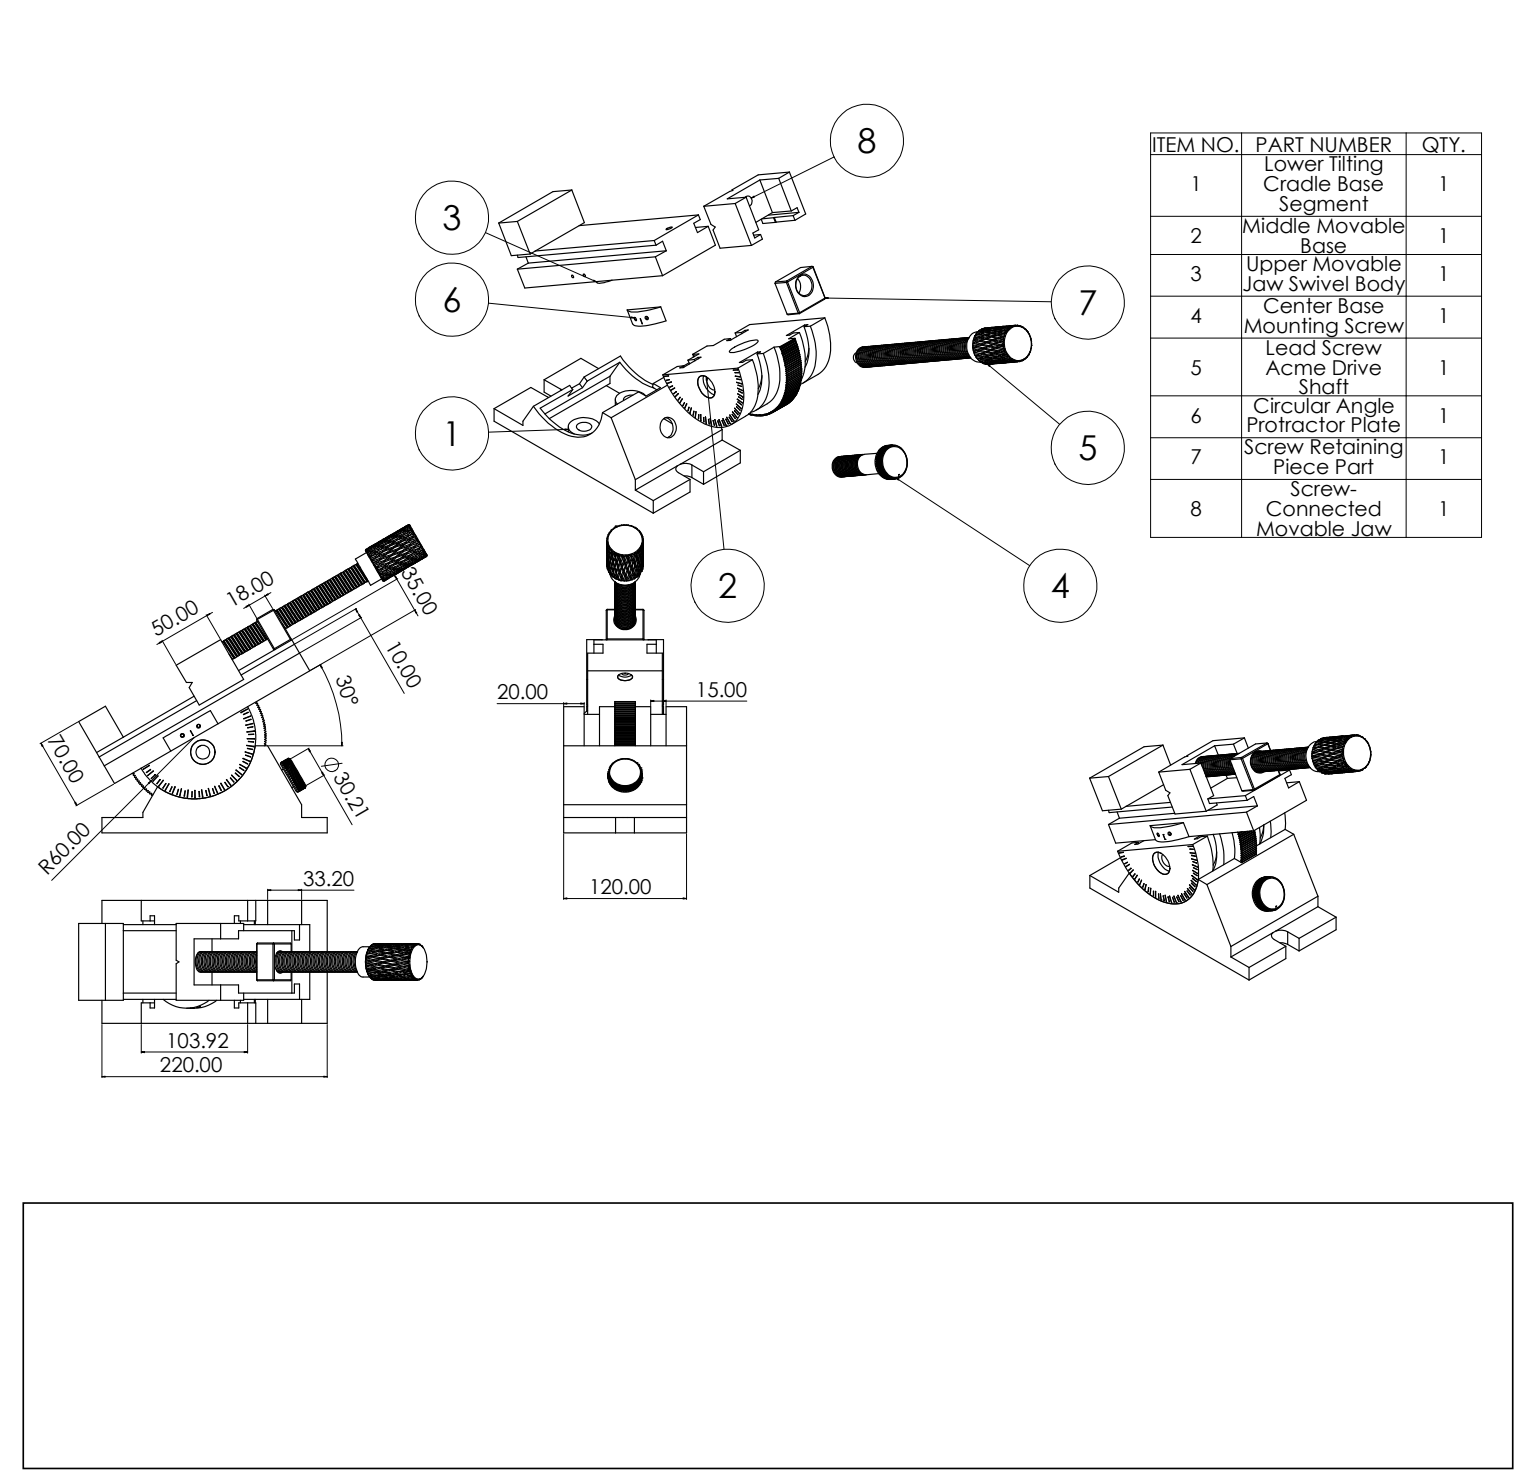
ISO-10303-21;
HEADER;
FILE_DESCRIPTION (('STEP AP214'),
    '1' );
FILE_NAME ('MAS-322',
    '2026-10-24T22:31:37',
    ( '' ),
    ( '' ),
    'SwSTEP 2.0',
    'SolidWorks 2025',
    '' );
FILE_SCHEMA (( 'AUTOMOTIVE_DESIGN' ));
ENDSEC;

DATA;
#1 = CARTESIAN_POINT ( 'NONE',  ( 23.65144817020273749, 15.78380873178787347, -6.180339887498949025 ) ) ;
#2 = EDGE_CURVE ( 'NONE', #71353, #27127, #17244, .T. ) ;
#3 = DIRECTION ( 'NONE',  ( 0.6270036013472524150, 0.3336146661356817478, 0.7039657224870777830 ) ) ;
#4 =( GEOMETRIC_REPRESENTATION_CONTEXT ( 3 ) GLOBAL_UNCERTAINTY_ASSIGNED_CONTEXT ( ( #48363 ) ) GLOBAL_UNIT_ASSIGNED_CONTEXT ( ( #53726, #45627, #22843 ) ) REPRESENTATION_CONTEXT ( 'NONE', 'WORKASPACE' ) );
#5 = CARTESIAN_POINT ( 'NONE',  ( 165.5065167046122099, 285.3186853228385758, 0.5240180121679646197 ) ) ;
#6 = CARTESIAN_POINT ( 'NONE',  ( 181.3318829485781976, 258.8378521386378566, -10.46588027007283017 ) ) ;
#7 = DIRECTION ( 'NONE',  ( -0.5866775868892348811, -0.8098206029990989707, 0.000000000000000000 ) ) ;
#8 = ORIENTED_EDGE ( 'NONE', *, *, #76052, .F. ) ;
#9 = CARTESIAN_POINT ( 'NONE',  ( 192.4853974341616549, 296.6629111496555424, 11.26379224701618398 ) ) ;
#10 = CARTESIAN_POINT ( 'NONE',  ( 33.33147356615550194, 41.01751292744059896, 6.180339887498949913 ) ) ;
#11 = CARTESIAN_POINT ( 'NONE',  ( 35.05240415091495976, 28.43677371833803846, -10.00000000000000355 ) ) ;
#12 = CARTESIAN_POINT ( 'NONE',  ( 201.3053499423511425, 281.9759013948520874, -16.75960365258566398 ) ) ;
#13 = CARTESIAN_POINT ( 'NONE',  ( 72.98662891910291250, 70.81012252529507123, 7.400885746516181030 ) ) ;
#14 = CARTESIAN_POINT ( 'NONE',  ( 67.19710446998851694, 67.37600790391256567, -7.293204404656055573 ) ) ;
#15 = CARTESIAN_POINT ( 'NONE',  ( 199.8044370756099966, 266.7412756917946695, 4.662294411209313871 ) ) ;
#16 = CARTESIAN_POINT ( 'NONE',  ( 202.7688273210276293, 274.1343011241658587, 13.26872680179261366 ) ) ;
#17 = CARTESIAN_POINT ( 'NONE',  ( 41.47569090598248920, 209.1868197944957899, -17.47570218321533631 ) ) ;
#18 = CARTESIAN_POINT ( 'NONE',  ( 80.56168512721397690, 49.66943426028002762, 14.25699872614796249 ) ) ;
#19 = CARTESIAN_POINT ( 'NONE',  ( 199.0151342380902406, 265.3454304162409585, 1.621217956766562551 ) ) ;
#20 = CARTESIAN_POINT ( 'NONE',  ( 154.6973317394036940, 271.0068791071395253, 14.01324914462427174 ) ) ;
#21 = VERTEX_POINT ( 'NONE', #91655 ) ;
#22 = CARTESIAN_POINT ( 'NONE',  ( 146.8195026170398023, 276.3481572557323034, 4.765869558735466249 ) ) ;
#23 = CARTESIAN_POINT ( 'NONE',  ( 202.2773826701151165, 280.2922913237452462, 16.62862787739668846 ) ) ;
#24 = CARTESIAN_POINT ( 'NONE',  ( 164.2578067403839555, 246.1441285162624126, -2.322300236470859591 ) ) ;
#27 = DIRECTION ( 'NONE',  ( 0.06115825522547173321, -0.9981280818701455670, 0.000000000000000000 ) ) ;
#26 = B_SPLINE_CURVE_WITH_KNOTS ( 'NONE', 3,
 ( #42002, #50106, #43488, #81061 ),
 .UNSPECIFIED., .F., .F.,
 ( 4, 4 ),
 ( 0.04462388129695979422, 0.04887120950165262795 ),
 .UNSPECIFIED. ) ;
#25 = CARTESIAN_POINT ( 'NONE',  ( 78.90549422596571105, 46.47045305960070039, 12.99985401326298984 ) ) ;
#28 = CARTESIAN_POINT ( 'NONE',  ( 21.21387930172907588, 35.18080186712593616, 3.090169943749475401 ) ) ;
#29 = CARTESIAN_POINT ( 'NONE',  ( 171.0277932295235814, 274.5471866711665712, 17.25980421070102366 ) ) ;
#30 = CARTESIAN_POINT ( 'NONE',  ( 30.34687108590969373, 93.06504152958497400, 45.00000000000000711 ) ) ;
#31 = CARTESIAN_POINT ( 'NONE',  ( -19.65312891409030271, 93.06504152958497400, -10.00000000000000888 ) ) ;
#32 = CARTESIAN_POINT ( 'NONE',  ( -22.42236680055709641, 157.8615022471902591, 0.000000000000000000 ) ) ;
#33 = CARTESIAN_POINT ( 'NONE',  ( 149.7543087857887656, 247.2677522451417929, -5.000000000000041744 ) ) ;
#34 = CARTESIAN_POINT ( 'NONE',  ( 82.20432729060253507, 208.2677522451417929, -5.000000000000041744 ) ) ;
#35 = VERTEX_POINT ( 'NONE', #22220 ) ;
#36 = VECTOR ( 'NONE', #79966, 1000.000000000000000 ) ;
#37 = CARTESIAN_POINT ( 'NONE',  ( 67.11298872355467893, 67.73948000908561085, -6.511686963657441929 ) ) ;
#38 = CARTESIAN_POINT ( 'NONE',  ( 73.03670947328784280, 70.42367050102286896, -8.076464510798354368 ) ) ;
#39 = DIRECTION ( 'NONE',  ( 0.000000000000000000, 0.000000000000000000, 1.000000000000000000 ) ) ;
#40 = CARTESIAN_POINT ( 'NONE',  ( 81.58428055322238492, 41.63658381244528073, 5.723166745212680873 ) ) ;
#41 = CARTESIAN_POINT ( 'NONE',  ( 20.25662117580333899, 176.3768266524159856, -9.188101187500093303 ) ) ;
#42 = FACE_OUTER_BOUND ( 'NONE', #88886, .T. ) ;
#43 = ADVANCED_FACE ( 'NONE', ( #53119 ), #78501, .F. ) ;
#44 = CARTESIAN_POINT ( 'NONE',  ( 181.8933809143826466, 275.6627081342313090, -16.43118812148207653 ) ) ;
#45 = CARTESIAN_POINT ( 'NONE',  ( 25.22600817569196963, 38.65659080271452552, -1.878358725466461243E-16 ) ) ;
#46 = CARTESIAN_POINT ( 'NONE',  ( 119.5854454918513170, 251.3967562850347122, -4.648177544792955347E-16 ) ) ;
#47 = CARTESIAN_POINT ( 'NONE',  ( 87.34642337659644795, 43.20430561321286689, -4.696387144280492735E-07 ) ) ;
#48 = DIRECTION ( 'NONE',  ( -0.8660254037844387076, -0.4999999999999998890, -0.000000000000000000 ) ) ;
#49 = CARTESIAN_POINT ( 'NONE',  ( 176.0471099249906217, 252.5555583919553726, -3.347364798285545895 ) ) ;
#50 = CARTESIAN_POINT ( 'NONE',  ( 190.7726985512088049, 261.9670508072832718, -0.9699378005772294475 ) ) ;
#51 = CARTESIAN_POINT ( 'NONE',  ( 182.4467602783141729, 295.3384606270356585, 1.016252470355397008 ) ) ;
#52 = CARTESIAN_POINT ( 'NONE',  ( 71.10837680816226225, 221.8615022471903160, 5.000000000000046185 ) ) ;
#53 = CARTESIAN_POINT ( 'NONE',  ( 45.00959873851216031, 26.39040679176986970, 1.333680081654574804E-15 ) ) ;
#54 = CARTESIAN_POINT ( 'NONE',  ( 82.57385212973971989, 41.04541115053230982, -1.138833187496899768 ) ) ;
#55 = CARTESIAN_POINT ( 'NONE',  ( 36.00728465925030974, 191.5958772461660544, -9.188101187500095079 ) ) ;
#56 = CARTESIAN_POINT ( 'NONE',  ( 66.42592059512334401, 67.89756533557547868, 6.603446877074300225 ) ) ;
#57 = ADVANCED_FACE ( 'NONE', ( #26227 ), #57103, .T. ) ;
#58 = DIRECTION ( 'NONE',  ( -0.5866775868892348811, -0.8098206029990989707, 0.000000000000000000 ) ) ;
#59 = CARTESIAN_POINT ( 'NONE',  ( 72.04657099559547362, 205.7365022471902023, -10.00000000000009237 ) ) ;
#60 = CARTESIAN_POINT ( 'NONE',  ( 198.6894790592683080, 286.5067226703918095, -17.06774375037124614 ) ) ;
#61 = CARTESIAN_POINT ( 'NONE',  ( 164.2600772519394923, 246.1401958748887182, -2.110785484364219311 ) ) ;
#62 = DIRECTION ( 'NONE',  ( 0.000000000000000000, -1.000000000000000000, 1.090355031989287297E-16 ) ) ;
#63 = CARTESIAN_POINT ( 'NONE',  ( 159.8708946529933996, 278.4983629143405324, -9.843749539283454197 ) ) ;
#64 = CARTESIAN_POINT ( 'NONE',  ( 160.1967185059513383, 280.0836358635930310, 9.265555704265979742 ) ) ;
#65 = CARTESIAN_POINT ( 'NONE',  ( 15.07770630580378501, 30.74646525600389424, 2.839279412974139660 ) ) ;
#66 = FACE_OUTER_BOUND ( 'NONE', #40596, .T. ) ;
#67 = CARTESIAN_POINT ( 'NONE',  ( 71.88182444303143370, 59.07920979518379312, 15.37605134340125090 ) ) ;
#68 = CARTESIAN_POINT ( 'NONE',  ( 188.9056787950111413, 270.0514309397178181, -14.11362088196558773 ) ) ;
#69 = EDGE_LOOP ( 'NONE', ( #91985, #84994, #72800, #59520 ) ) ;
#70 = CARTESIAN_POINT ( 'NONE',  ( 4.275827057391709651, 20.65586893147753500, -7.433330006724137462 ) ) ;
#71 = CARTESIAN_POINT ( 'NONE',  ( 75.23698744953621542, 53.54332355648684683, -16.05067780448434078 ) ) ;
#72 = CARTESIAN_POINT ( 'NONE',  ( 87.14941533941508567, 43.54552546780055877, 0.3078308432578384934 ) ) ;
#73 = CARTESIAN_POINT ( 'NONE',  ( -4.101579717973121930, 179.9860189848785694, -2.679491924311240503 ) ) ;
#74 = LINE ( 'NONE', #15241, #89935 ) ;
#75 = EDGE_LOOP ( 'NONE', ( #46929, #82112, #52955, #6832 ) ) ;
#76 = CARTESIAN_POINT ( 'NONE',  ( 47.43014843991451102, 113.9519901285712251, 10.00000000000000000 ) ) ;
#77 = CARTESIAN_POINT ( 'NONE',  ( 71.49780929996677514, 71.35361720523084728, -4.112299254006656746 ) ) ;
#78 = CARTESIAN_POINT ( 'NONE',  ( 76.99791550217098290, 63.80129665876799550, 14.94914524525639266 ) ) ;
#79 = CARTESIAN_POINT ( 'NONE',  ( 180.4501283053277803, 256.5846271277198412, -7.835696842545695873 ) ) ;
#80 = ORIENTED_EDGE ( 'NONE', *, *, #23057, .F. ) ;
#81 = ORIENTED_EDGE ( 'NONE', *, *, #67086, .T. ) ;
#82 = LINE ( 'NONE', #92802, #76218 ) ;
#83 = ORIENTED_EDGE ( 'NONE', *, *, #17750, .F. ) ;
#84 = CARTESIAN_POINT ( 'NONE',  ( 190.9907605556751093, 299.8412942717858414, 8.799173206188184437 ) ) ;
#85 = DIRECTION ( 'NONE',  ( 0.4999999999999992784, -0.8660254037844390407, 0.000000000000000000 ) ) ;
#86 = CARTESIAN_POINT ( 'NONE',  ( 80.05322980421331636, 57.68292478952277946, 16.60179730502024853 ) ) ;
#87 = CARTESIAN_POINT ( 'NONE',  ( 66.50947442187053582, 69.16636744153423422, -3.269992574601006119 ) ) ;
#88 = ORIENTED_EDGE ( 'NONE', *, *, #97854, .T. ) ;
#89 = CARTESIAN_POINT ( 'NONE',  ( 148.3280470635002928, 273.7352816289870248, 9.058704604771318003 ) ) ;
#90 = CARTESIAN_POINT ( 'NONE',  ( 196.4783028304046013, 290.3365922432724346, -16.37291435488387492 ) ) ;
#91 = CARTESIAN_POINT ( 'NONE',  ( 173.2337249902883798, 270.7486416191997023, 17.82094672905207133 ) ) ;
#92 = ORIENTED_EDGE ( 'NONE', *, *, #79784, .F. ) ;
#93 = LINE ( 'NONE', #62359, #20761 ) ;
#94 = CARTESIAN_POINT ( 'NONE',  ( 159.3297396961336290, 265.7340194281295567, 16.79158499271843041 ) ) ;
#95 = ORIENTED_EDGE ( 'NONE', *, *, #9124, .F. ) ;
#96 = ADVANCED_FACE ( 'NONE', ( #87601 ), #64731, .F. ) ;
#97 = CARTESIAN_POINT ( 'NONE',  ( 149.4491471355718772, 271.7934793437897270, 11.43912701239353780 ) ) ;
#98 = CARTESIAN_POINT ( 'NONE',  ( 78.41477381124543911, 47.32040575020751305, -14.22103711521623559 ) ) ;
#99 = ORIENTED_EDGE ( 'NONE', *, *, #21399, .F. ) ;
#100 = CARTESIAN_POINT ( 'NONE',  ( -11.19568923542803773, 72.02527638617826256, 14.65695210810445737 ) ) ;
#101 = CARTESIAN_POINT ( 'NONE',  ( 159.7595800023532320, 255.3516961917271999, 16.21405881663931936 ) ) ;
#102 = FACE_OUTER_BOUND ( 'NONE', #93953, .T. ) ;
#103 = CARTESIAN_POINT ( 'NONE',  ( 83.68415435101742617, 52.28560849428279766, 14.71934805883068975 ) ) ;
#104 = VERTEX_POINT ( 'NONE', #18635 ) ;
#105 = ORIENTED_EDGE ( 'NONE', *, *, #46073, .T. ) ;
#106 = CARTESIAN_POINT ( 'NONE',  ( 190.9402756120810523, 299.5005484933402613, 5.898581097966179243 ) ) ;
#107 = CARTESIAN_POINT ( 'NONE',  ( -32.94356256989595977, 94.88921800892812541, 10.61543114587583503 ) ) ;
#108 = CARTESIAN_POINT ( 'NONE',  ( 189.8480911035503880, 301.8204558191226283, -0.8992086515915015399 ) ) ;
#109 = CARTESIAN_POINT ( 'NONE',  ( 190.2389970918280540, 301.1433867864428748, 4.601241515604689525 ) ) ;
#110 = CARTESIAN_POINT ( 'NONE',  ( 173.6269293304046357, 276.7763204810394200, -15.65584202761720611 ) ) ;
#111 = CARTESIAN_POINT ( 'NONE',  ( 146.5086121934486982, 276.8866352649785654, -0.04230388357226919777 ) ) ;
#112 = EDGE_CURVE ( 'NONE', #27867, #86369, #27228, .T. ) ;
#113 = CARTESIAN_POINT ( 'NONE',  ( 192.8011239859581849, 296.7056528303708660, -11.79847971295421694 ) ) ;
#114 = CARTESIAN_POINT ( 'NONE',  ( 161.7445750920071816, 256.8061939151814386, 15.71254058960433397 ) ) ;
#115 = CARTESIAN_POINT ( 'NONE',  ( 70.01037705890988150, 67.69997893903554598, 9.246301564518420335 ) ) ;
#116 = DIRECTION ( 'NONE',  ( -0.8660254037844387076, -0.4999999999999998890, -0.000000000000000000 ) ) ;
#117 = LINE ( 'NONE', #62385, #16927 ) ;
#118 = CARTESIAN_POINT ( 'NONE',  ( 22.66956910419568061, 38.88013629349138256, -10.00000000000000000 ) ) ;
#119 = CARTESIAN_POINT ( 'NONE',  ( 78.58712697892576671, 47.46528512289431490, 14.24466080792137923 ) ) ;
#120 = CARTESIAN_POINT ( 'NONE',  ( 105.9391831106087380, 219.7202760586659736, -5.415160957724236172E-17 ) ) ;
#121 = VERTEX_POINT ( 'NONE', #65704 ) ;
#122 = CARTESIAN_POINT ( 'NONE',  ( 149.0943192338760070, 272.4080592974699471, -12.87526400066115606 ) ) ;
#123 = CARTESIAN_POINT ( 'NONE',  ( 70.63585127456710211, 66.25873673130102759, 11.15280021666221266 ) ) ;
#124 = CARTESIAN_POINT ( 'NONE',  ( 87.74659634842467426, 45.27479573043824246, -7.097702524348068920 ) ) ;
#125 = CARTESIAN_POINT ( 'NONE',  ( 79.09597600355056102, 46.01113921700726195, 13.22013416637107674 ) ) ;
#126 = CARTESIAN_POINT ( 'NONE',  ( 180.5399386764078997, 283.1336537301233420, -15.18944844307240238 ) ) ;
#127 = CARTESIAN_POINT ( 'NONE',  ( 80.54938030787035075, 54.28115242235315208, -16.20956398890630368 ) ) ;
#128 = AXIS2_PLACEMENT_3D ( 'NONE', #29113, #74733, #4299 ) ;
#129 = CARTESIAN_POINT ( 'NONE',  ( 69.87848390701969947, 64.97149032717396722, -11.85179110244203926 ) ) ;
#130 = VERTEX_POINT ( 'NONE', #94659 ) ;
#131 = CARTESIAN_POINT ( 'NONE',  ( 163.0056347026689707, 248.3129541054019569, -11.27842346302751508 ) ) ;
#132 = CARTESIAN_POINT ( 'NONE',  ( 72.22030775602182473, 71.51030902015637025, 5.034539909834746751 ) ) ;
#133 = CARTESIAN_POINT ( 'NONE',  ( 45.39824762976388683, 187.0177522451417929, 5.000000000000051514 ) ) ;
#134 = CARTESIAN_POINT ( 'NONE',  ( 124.5040820605901217, 248.8149278399160949, -9.188101187500095079 ) ) ;
#135 = CARTESIAN_POINT ( 'NONE',  ( 180.7770252323854834, 294.0936096853982349, -2.952313513407788026 ) ) ;
#136 = CARTESIAN_POINT ( 'NONE',  ( 67.15772368909350121, 67.74692886573922124, -6.548511843863573212 ) ) ;
#137 = CARTESIAN_POINT ( 'NONE',  ( 157.6673516573649181, 257.5591315650518141, 16.79781451397666103 ) ) ;
#138 = CARTESIAN_POINT ( 'NONE',  ( 175.3042518086594441, 253.4457403629180021, -3.880823026268251930 ) ) ;
#139 = CARTESIAN_POINT ( 'NONE',  ( 46.23738328933649200, 191.3768266524159856, -9.188101187500091527 ) ) ;
#140 = CARTESIAN_POINT ( 'NONE',  ( 85.75095722755503402, 48.73152497522561788, -11.95392408748539381 ) ) ;
#141 = ORIENTED_EDGE ( 'NONE', *, *, #32045, .F. ) ;
#142 = CARTESIAN_POINT ( 'NONE',  ( 70.62071346605948463, 62.04983420565448426, 13.98037766351442457 ) ) ;
#143 = CARTESIAN_POINT ( 'NONE',  ( -37.33262083840156009, 163.6868197944959888, -1.732050807568741524 ) ) ;
#144 = DIRECTION ( 'NONE',  ( 1.000000000000000000, 0.000000000000000000, 0.000000000000000000 ) ) ;
#145 = CARTESIAN_POINT ( 'NONE',  ( 146.8358616138309571, 276.3198226421291679, 4.054088818585255716 ) ) ;
#146 = CARTESIAN_POINT ( 'NONE',  ( 82.03168081927420019, 41.83908362533459524, -5.586039627916139949 ) ) ;
#147 = DIRECTION ( 'NONE',  ( -0.9979398670145497308, -0.06415622980648832963, 0.000000000000000000 ) ) ;
#148 = CARTESIAN_POINT ( 'NONE',  ( 17.25242200676963833, 170.7677522451417929, -5.000000000000041744 ) ) ;
#149 = CARTESIAN_POINT ( 'NONE',  ( 102.9889369814289921, 240.2677522451419065, -5.000000000000047962 ) ) ;
#150 = ORIENTED_EDGE ( 'NONE', *, *, #60128, .F. ) ;
#151 = CARTESIAN_POINT ( 'NONE',  ( 163.3854574543125580, 247.6550818016845597, 10.82482370245618775 ) ) ;
#152 = CARTESIAN_POINT ( 'NONE',  ( 163.3939361803663246, 247.6403962173759226, -10.78041711314006790 ) ) ;
#153 = EDGE_CURVE ( 'NONE', #73023, #47320, #41466, .T. ) ;
#154 = CARTESIAN_POINT ( 'NONE',  ( 29.56604717072103483, 194.0024278399160949, 9.188101187500095079 ) ) ;
#155 = CARTESIAN_POINT ( 'NONE',  ( 17.22757050757671493, 15.11029122506293554, -8.090169943749478065 ) ) ;
#156 = CARTESIAN_POINT ( 'NONE',  ( 195.4765535648738535, 273.5335777180424657, 14.55181105716135903 ) ) ;
#157 = DIRECTION ( 'NONE',  ( -1.000000000000000000, 0.000000000000000000, 0.000000000000000000 ) ) ;
#158 = DIRECTION ( 'NONE',  ( -0.4755282581475737680, 0.8236391035463299648, -0.3090169943749573878 ) ) ;
#160 = CARTESIAN_POINT ( 'NONE',  ( 69.07880331415105957, 204.5643266524160140, 9.188101187500095079 ) ) ;
#159 = CARTESIAN_POINT ( 'NONE',  ( 194.7274671941087831, 275.0520795863097305, -15.83285290351333785 ) ) ;
#161 = EDGE_CURVE ( 'NONE', #56410, #9864, #92298, .T. ) ;
#162 = CARTESIAN_POINT ( 'NONE',  ( 161.4396252346964218, 251.0253620690641299, 14.51972485405798885 ) ) ;
#163 = CARTESIAN_POINT ( 'NONE',  ( 72.59198933040177337, 57.21847231819964463, 16.35083922987430327 ) ) ;
#164 = CARTESIAN_POINT ( 'NONE',  ( -31.31952861460583648, 96.88699691338099740, 44.45098699770857564 ) ) ;
#165 = CARTESIAN_POINT ( 'NONE',  ( 66.48182541455327055, 68.83268692814938561, -4.376997617227660342 ) ) ;
#166 = VERTEX_POINT ( 'NONE', #35811 ) ;
#167 =( BOUNDED_CURVE ( )  B_SPLINE_CURVE ( 2, ( #94120, #92619, #24674, #32772, #7471, #38365, #3886, #40856, #18091 ),
 .UNSPECIFIED., .F., .T. ) 
 B_SPLINE_CURVE_WITH_KNOTS ( ( 3, 2, 2, 2, 3 ),
 ( 0.1330645161290322509, 0.1344086021505376261, 0.1370967741935483764, 0.1397849462365591267, 0.1411290322580645296 ),
 .UNSPECIFIED. ) 
 CURVE ( )  GEOMETRIC_REPRESENTATION_ITEM ( )  RATIONAL_B_SPLINE_CURVE ( ( 0.9330127018922194093, 0.9330127018922194093, 1.000000000000000000, 0.8660254037844387076, 1.000000000000000000, 0.8660254037844387076, 1.000000000000000000, 0.9330127018922187432, 0.9330127018922194093 ) ) 
 REPRESENTATION_ITEM ( '' )  );
#168 = CARTESIAN_POINT ( 'NONE',  ( 165.4887069070615269, 269.3414653546907402, 17.07898631664743405 ) ) ;
#169 = CARTESIAN_POINT ( 'NONE',  ( 29.10614472461701752, 187.6115022471902591, 10.00000000000009592 ) ) ;
#170 = CARTESIAN_POINT ( 'NONE',  ( 208.2175703429120688, 270.0035844679667889, 2.257951022351344150 ) ) ;
#171 = CARTESIAN_POINT ( 'NONE',  ( -1.394013918807642360, 163.8768266524159856, 9.188101187500098632 ) ) ;
#172 = CARTESIAN_POINT ( 'NONE',  ( 30.35763184873497877, 26.03085787977764198, 9.188101187500006262 ) ) ;
#174 = EDGE_CURVE ( 'NONE', #25263, #42575, #10857, .T. ) ;
#173 = CARTESIAN_POINT ( 'NONE',  ( 167.7163553651179768, 262.5077956943969753, -16.64284935447819791 ) ) ;
#175 = CARTESIAN_POINT ( 'NONE',  ( 185.3704253846254346, 260.3657602090070782, 6.355839938251095944 ) ) ;
#176 = CARTESIAN_POINT ( 'NONE',  ( 206.0627831668701901, 273.7357853363691902, 10.14454147593459687 ) ) ;
#177 = CARTESIAN_POINT ( 'NONE',  ( 68.73278530260755304, 67.96956153877513884, 8.699763636338595063 ) ) ;
#178 = CARTESIAN_POINT ( 'NONE',  ( 66.40112479374357690, 68.71345452083818373, 2.354737509933789941 ) ) ;
#179 = VERTEX_POINT ( 'NONE', #22103 ) ;
#180 = CARTESIAN_POINT ( 'NONE',  ( 43.35468487962021555, 120.5828561944265687, -10.00000000000000000 ) ) ;
#181 = CARTESIAN_POINT ( 'NONE',  ( 208.2813134324037492, 269.8931781983357041, -0.4511785827856357178 ) ) ;
#182 = DIRECTION ( 'NONE',  ( -0.8770933717188628131, -0.4803199113995136327, 0.000000000000000000 ) ) ;
#183 = CARTESIAN_POINT ( 'NONE',  ( 16.06339478488542127, 14.98920272979925272, 7.433330006724137462 ) ) ;
#184 = VERTEX_POINT ( 'NONE', #13527 ) ;
#185 = CARTESIAN_POINT ( 'NONE',  ( -77.58047734835668052, 56.02942318228900120, 10.00000000000000000 ) ) ;
#186 = EDGE_CURVE ( 'NONE', #58877, #48375, #99124, .T. ) ;
#187 = CARTESIAN_POINT ( 'NONE',  ( -37.40701240123932791, 25.35389310390295847, 177.5919119679930134 ) ) ;
#188 = CARTESIAN_POINT ( 'NONE',  ( 84.96478326871331888, 219.8615022471902591, -10.00000000000009592 ) ) ;
#189 = CARTESIAN_POINT ( 'NONE',  ( 173.0837253472800796, 264.8280141993791972, 17.07053884509587860 ) ) ;
#190 = CARTESIAN_POINT ( 'NONE',  ( 162.6541320028305506, 248.9217746405196294, -10.16950121496441817 ) ) ;
#191 = VECTOR ( 'NONE', #26487, 1000.000000000000000 ) ;
#192 = DIRECTION ( 'NONE',  ( -0.2575544297740129385, 0.9662637919863205083, 0.000000000000000000 ) ) ;
#193 = ORIENTED_EDGE ( 'NONE', *, *, #79471, .F. ) ;
#194 = ORIENTED_EDGE ( 'NONE', *, *, #7075, .T. ) ;
#195 = LINE ( 'NONE', #21507, #68091 ) ;
#196 = CARTESIAN_POINT ( 'NONE',  ( 72.70339454587075068, 70.80219159916109106, 7.145408444353458677 ) ) ;
#197 = ORIENTED_EDGE ( 'NONE', *, *, #54268, .F. ) ;
#198 = LINE ( 'NONE', #694, #6256 ) ;
#199 = DIRECTION ( 'NONE',  ( -0.1269555777209495084, -0.9919084036772447543, 0.000000000000000000 ) ) ;
#200 = ORIENTED_EDGE ( 'NONE', *, *, #33555, .T. ) ;
#201 = DIRECTION ( 'NONE',  ( -0.9956898167541090583, 0.09274582908232942291, 0.000000000000000000 ) ) ;
#202 = CARTESIAN_POINT ( 'NONE',  ( 171.2743479101317234, 254.4242377521371736, -11.94796457435898951 ) ) ;
#203 = CARTESIAN_POINT ( 'NONE',  ( 164.2712161151136172, 246.1209027979328710, 7.276091357954241445 ) ) ;
#204 = CARTESIAN_POINT ( 'NONE',  ( 69.57540738265171854, 62.56329180587877659, 13.35759117457639533 ) ) ;
#205 = ORIENTED_EDGE ( 'NONE', *, *, #96749, .F. ) ;
#206 = CARTESIAN_POINT ( 'NONE',  ( 155.6989589471585020, 260.9684877483775267, 17.28906573347438425 ) ) ;
#207 = CARTESIAN_POINT ( 'NONE',  ( 151.2455280670316711, 268.6820563007532314, 14.35914944935941229 ) ) ;
#208 = CARTESIAN_POINT ( 'NONE',  ( 81.41173721124711449, 42.57291668893481784, -7.675381966840256531 ) ) ;
#209 = ORIENTED_EDGE ( 'NONE', *, *, #18748, .T. ) ;
#210 = ADVANCED_FACE ( 'NONE', ( #82475 ), #75330, .F. ) ;
#211 = EDGE_CURVE ( 'NONE', #97533, #84233, #8682, .T. ) ;
#212 = ORIENTED_EDGE ( 'NONE', *, *, #13551, .F. ) ;
#213 = VERTEX_POINT ( 'NONE', #51000 ) ;
#214 = CARTESIAN_POINT ( 'NONE',  ( 159.9635946688021022, 268.7707599091479551, -17.14635356962945778 ) ) ;
#215 = ORIENTED_EDGE ( 'NONE', *, *, #48377, .F. ) ;
#216 = CARTESIAN_POINT ( 'NONE',  ( -34.42581292930597670, 25.91608375674935161, -10.00000000000000000 ) ) ;
#217 = ORIENTED_EDGE ( 'NONE', *, *, #97229, .F. ) ;
#218 = EDGE_CURVE ( 'NONE', #7931, #29087, #34574, .T. ) ;
#219 = CARTESIAN_POINT ( 'NONE',  ( 207.5792673731680793, 271.1091576421853233, 2.359198794924813214 ) ) ;
#220 = CARTESIAN_POINT ( 'NONE',  ( 90.04477061917849312, 44.76220097505219542, 0.000000000000000000 ) ) ;
#221 = CARTESIAN_POINT ( 'NONE',  ( 167.3703162778506055, 281.6204983129350694, 11.41617640160279024 ) ) ;
#222 = CARTESIAN_POINT ( 'NONE',  ( 194.9220242159064185, 293.0321458743159724, -14.92681063007793263 ) ) ;
#223 = EDGE_CURVE ( 'NONE', #61495, #4321, #98638, .T. ) ;
#224 = CARTESIAN_POINT ( 'NONE',  ( 82.66575685400569284, 54.08976349579732812, -15.88644314918171929 ) ) ;
#225 = ADVANCED_FACE ( 'NONE', ( #75832 ), #98127, .T. ) ;
#226 = CARTESIAN_POINT ( 'NONE',  ( -38.08094845355783065, 65.40755614729289391, -10.00000000000000000 ) ) ;
#227 = CARTESIAN_POINT ( 'NONE',  ( 11.61360469066603507, 28.74646525600389069, 2.839279412974139660 ) ) ;
#228 = CARTESIAN_POINT ( 'NONE',  ( 198.4408884114532725, 277.4403926908931908, -15.34803116808097023 ) ) ;
#229 = CARTESIAN_POINT ( 'NONE',  ( 85.68485941944550177, 48.66523437743575187, 11.91861461389294163 ) ) ;
#231 = EDGE_LOOP ( 'NONE', ( #23374, #30336, #91707, #91795 ) ) ;
#230 = LINE ( 'NONE', #68626, #5643 ) ;
#232 = EDGE_CURVE ( 'NONE', #38319, #90439, #71654, .T. ) ;
#233 = CARTESIAN_POINT ( 'NONE',  ( 147.2256490141643042, 275.6446910606013603, -4.110658582098289493 ) ) ;
#234 = CARTESIAN_POINT ( 'NONE',  ( 32.49301573174289359, 102.6727471919249552, 59.99999999999999289 ) ) ;
#235 = EDGE_CURVE ( 'NONE', #80145, #45676, #581, .T. ) ;
#236 = CARTESIAN_POINT ( 'NONE',  ( 206.3018347371251195, 273.3217358710584790, -9.309724106897926177 ) ) ;
#237 = PLANE ( 'NONE',  #70015 ) ;
#238 = CARTESIAN_POINT ( 'NONE',  ( 80.58987807051757102, 46.20205379198799989, -12.14270396900382742 ) ) ;
#239 = CARTESIAN_POINT ( 'NONE',  ( 171.8224262749942852, 254.8926688302297521, 11.02064826558146748 ) ) ;
#240 = CARTESIAN_POINT ( 'NONE',  ( 157.5687383428415274, 281.7222027203141579, 1.387399794590924440 ) ) ;
#241 = ORIENTED_EDGE ( 'NONE', *, *, #65257, .F. ) ;
#242 = CARTESIAN_POINT ( 'NONE',  ( 194.3044832453722677, 294.1017582110366106, -14.10778293554018603 ) ) ;
#243 = CARTESIAN_POINT ( 'NONE',  ( -5.171971415982786979, 24.31384663199769491, -10.00000000000000000 ) ) ;
#244 = CARTESIAN_POINT ( 'NONE',  ( 141.2767884429413243, 240.8262482093457777, 3.021315404115420679E-15 ) ) ;
#245 = CARTESIAN_POINT ( 'NONE',  ( -0.9341114727036189391, 170.2677522451418781, 10.00000000000009592 ) ) ;
#246 = CARTESIAN_POINT ( 'NONE',  ( 94.73480590126506229, 219.3768266524160140, 9.188101187500096856 ) ) ;
#247 = CARTESIAN_POINT ( 'NONE',  ( 195.8651621160345542, 269.3302623707359658, -10.80388373675355851 ) ) ;
#248 = B_SPLINE_CURVE_WITH_KNOTS ( 'NONE', 3,
 ( #65678, #27199, #81432, #4384, #59558, #20106, #51479, #97613, #89544, #13499, #59053, #74319, #21105, #43869, #50975, #81927, #67174, #28181, #12503, #36275, #83920, #90535, #6867, #75301, #21584, #82446, #82923, #43372, #90024, #4902, #51985, #5389, #13010, #98098, #74811, #52469, #20596, #35785, #67678, #29191, #68662, #60058, #44369, #28675, #66678, #13984 ),
 .UNSPECIFIED., .F., .F.,
 ( 4, 1, 1, 1, 2, 2, 1, 1, 1, 2, 2, 1, 1, 2, 2, 1, 1, 2, 2, 1, 1, 2, 2, 1, 2, 2, 1, 2, 2, 4 ),
 ( 0.000000000000000000, 0.06249999999999578115, 0.09374999999999281131, 0.1093749999999927697, 0.1171874999999917982, 0.1249999999999908268, 0.1874999999999810985, 0.2187499999999757694, 0.2343749999999731048, 0.2421874999999721889, 0.2499999999999712730, 0.3124999999999665823, 0.3437499999999636957, 0.3593749999999625855, 0.3749999999999614753, 0.4374999999999584777, 0.4687499999999559241, 0.4843749999999560907, 0.4999999999999562572, 0.5624999999999540368, 0.5937499999999539257, 0.6093749999999549249, 0.6249999999999558131, 0.6874999999999583666, 0.7187499999999606981, 0.7499999999999630296, 0.8124999999999696909, 0.8437499999999743538, 0.8749999999999790168, 1.000000000000000000 ),
 .UNSPECIFIED. ) ;
#249 = CARTESIAN_POINT ( 'NONE',  ( 19.31801425620939483, 115.5650415295850451, 45.00000000000000711 ) ) ;
#250 = CARTESIAN_POINT ( 'NONE',  ( 170.2105851965358738, 280.7371124046519526, -14.06690082814746390 ) ) ;
#251 = DIRECTION ( 'NONE',  ( -0.7299047266382377996, 0.6835488936653758563, 0.000000000000000000 ) ) ;
#253 = LINE ( 'NONE', #93489, #65775 ) ;
#252 = CARTESIAN_POINT ( 'NONE',  ( 17.27983239817682559, 168.5327760586659736, 1.948934522072303157E-15 ) ) ;
#254 = CARTESIAN_POINT ( 'NONE',  ( 200.4592688079413847, 283.4413569069752725, 18.39277739746426832 ) ) ;
#255 = ORIENTED_EDGE ( 'NONE', *, *, #28716, .T. ) ;
#256 = ORIENTED_EDGE ( 'NONE', *, *, #59561, .F. ) ;
#257 = CARTESIAN_POINT ( 'NONE',  ( 167.4700212936181458, 285.1112495945437786, 9.221858443278774686 ) ) ;
#258 = CARTESIAN_POINT ( 'NONE',  ( 84.80990162342361316, 46.15601649245774496, -9.987538208358218483 ) ) ;
#259 = CARTESIAN_POINT ( 'NONE',  ( 157.8159121039657293, 257.3018173235443555, -17.05074702406642118 ) ) ;
#260 = VECTOR ( 'NONE', #98642, 1000.000000000000000 ) ;
#261 = CARTESIAN_POINT ( 'NONE',  ( 201.9437967514558920, 280.8700790835527528, -16.67046097481324196 ) ) ;
#262 = CARTESIAN_POINT ( 'NONE',  ( 113.9506338607584723, 225.0494855054051868, -2.679491924311248496 ) ) ;
#263 = CARTESIAN_POINT ( 'NONE',  ( 74.05204724713870235, 68.33764315531155376, -11.67956189741113349 ) ) ;
#264 = CARTESIAN_POINT ( 'NONE',  ( 23.34166312890287998, 184.2833772461660544, -9.188101187500095079 ) ) ;
#265 = CARTESIAN_POINT ( 'NONE',  ( 130.0524911732904343, 236.7048013555409796, 4.594050593750051981 ) ) ;
#266 = CARTESIAN_POINT ( 'NONE',  ( 183.1279196651564973, 257.7771318069471249, -2.489900343309737529 ) ) ;
#267 = ORIENTED_EDGE ( 'NONE', *, *, #37270, .F. ) ;
#268 = CARTESIAN_POINT ( 'NONE',  ( 179.8888715531147682, 274.4711782159853328, -17.82026667163308531 ) ) ;
#269 = CARTESIAN_POINT ( 'NONE',  ( -8.863483026448420787, 159.5643266524160140, 9.188101187500095079 ) ) ;
#270 = DIRECTION ( 'NONE',  ( 0.000000000000000000, 0.000000000000000000, 1.000000000000000000 ) ) ;
#271 = CARTESIAN_POINT ( 'NONE',  ( 194.5047661587782386, 293.7548580291293092, 14.86680123054176583 ) ) ;
#272 = CARTESIAN_POINT ( 'NONE',  ( 177.2183068813167495, 256.3290312667157309, -10.31296860541032423 ) ) ;
#273 = CARTESIAN_POINT ( 'NONE',  ( 190.1462790299653420, 284.8797699240140560, 17.00550891877788473 ) ) ;
#274 = CARTESIAN_POINT ( 'NONE',  ( 147.6508870500795467, 274.9081571770856272, -8.950912509993816712 ) ) ;
#275 = CARTESIAN_POINT ( 'NONE',  ( 189.2224370172964143, 262.6230431603515854, 8.075317388220659254 ) ) ;
#276 = CARTESIAN_POINT ( 'NONE',  ( 167.7174649547847309, 278.2620246372183601, 14.62053864993239216 ) ) ;
#277 = DIRECTION ( 'NONE',  ( -0.8660254037844377084, -0.5000000000000015543, -0.000000000000000000 ) ) ;
#278 = CARTESIAN_POINT ( 'NONE',  ( 69.28790557221618940, 69.26308972205728764, 6.048929301421852145 ) ) ;
#279 = CARTESIAN_POINT ( 'NONE',  ( 148.3707431749605234, 273.6613297946520902, 8.912574527564540716 ) ) ;
#280 = FACE_OUTER_BOUND ( 'NONE', #77196, .T. ) ;
#281 = ORIENTED_EDGE ( 'NONE', *, *, #67790, .T. ) ;
#282 = CARTESIAN_POINT ( 'NONE',  ( 45.86253193465722688, 68.41350641406140198, -10.00000000000000000 ) ) ;
#283 = CARTESIAN_POINT ( 'NONE',  ( 184.9437015084479299, 269.6468049839930927, 15.52015019358652204 ) ) ;
#284 = CARTESIAN_POINT ( 'NONE',  ( 109.0781781035623226, 233.7833772461660544, -9.188101187500095079 ) ) ;
#285 = CARTESIAN_POINT ( 'NONE',  ( 17.19404571121151548, 18.43085787977762280, -9.188101187500008038 ) ) ;
#287 = EDGE_CURVE ( 'NONE', #95521, #97948, #4932, .T. ) ;
#286 = CARTESIAN_POINT ( 'NONE',  ( 190.9907605556751093, 299.8412942717858414, 8.799173206188184437 ) ) ;
#288 = CYLINDRICAL_SURFACE ( 'NONE', #48455, 17.82106496071139645 ) ;
#290 = CARTESIAN_POINT ( 'NONE',  ( 195.5685147139090816, 278.4936960503050045, 16.53693894814080423 ) ) ;
#289 = CARTESIAN_POINT ( 'NONE',  ( 48.58805178314242568, 84.67719436603331928, -10.00000000000000000 ) ) ;
#291 = CARTESIAN_POINT ( 'NONE',  ( 201.3138726815416817, 270.7303338844035352, -9.934698065831957692 ) ) ;
#292 = CARTESIAN_POINT ( 'NONE',  ( 163.2031704490160848, 279.2514240946757695, 12.88724473550253258 ) ) ;
#293 = CARTESIAN_POINT ( 'NONE',  ( 137.7719789713245291, 261.8967562850346553, -4.648177544792955347E-16 ) ) ;
#294 = CARTESIAN_POINT ( 'NONE',  ( 43.17480782474465428, 33.43085787977766898, -9.188101187500008038 ) ) ;
#295 = DIRECTION ( 'NONE',  ( -0.000000000000000000, 0.000000000000000000, -1.000000000000000000 ) ) ;
#296 = CARTESIAN_POINT ( 'NONE',  ( 81.30975366074838462, 56.24313983998633404, -16.44754541364716971 ) ) ;
#297 = ORIENTED_EDGE ( 'NONE', *, *, #4120, .T. ) ;
#298 = CARTESIAN_POINT ( 'NONE',  ( 163.8995163580303256, 256.4334289116373498, -14.90821826893867730 ) ) ;
#299 = CARTESIAN_POINT ( 'NONE',  ( 33.38390286057418166, 24.98920272979928470, 7.433330006724137462 ) ) ;
#300 = DIRECTION ( 'NONE',  ( 0.4145187862775202015, -0.7179675985244525771, -0.5591929034707450175 ) ) ;
#301 = CARTESIAN_POINT ( 'NONE',  ( 81.38004395914478550, 48.63429429711172247, 14.01118663915790030 ) ) ;
#302 = CARTESIAN_POINT ( 'NONE',  ( 149.5390997184345281, 271.6376768999995761, -11.52989534384373016 ) ) ;
#304 = ORIENTED_EDGE ( 'NONE', *, *, #16098, .T. ) ;
#303 = EDGE_CURVE ( 'NONE', #60481, #57725, #20128, .T. ) ;
#305 = B_SPLINE_SURFACE_WITH_KNOTS ( 'NONE', 3, 1, ( 
 ( #12840, #43700 ),
 ( #74643, #5218 ),
 ( #82762, #13328 ),
 ( #36596, #67500 ),
 ( #98432, #29023 ),
 ( #59894, #44684 ),
 ( #39075, #60879 ),
 ( #91339, #6708 ),
 ( #61389, #92343 ),
 ( #76606, #22402 ),
 ( #37586, #53297 ),
 ( #7698, #46696 ),
 ( #602, #22892 ),
 ( #14308, #91841 ),
 ( #8206, #99420 ),
 ( #45194, #69988 ),
 ( #69496, #23889 ),
 ( #99915, #7192 ),
 ( #68496, #84250 ),
 ( #92834, #15789 ),
 ( #38077, #54790 ),
 ( #14798, #21899 ),
 ( #68004, #53777 ),
 ( #38590, #77621 ),
 ( #31486, #84740 ),
 ( #76133, #45680 ),
 ( #62378, #29997 ),
 ( #68990, #93335 ),
 ( #109, #85769 ),
 ( #30501, #15281 ),
 ( #46176, #77096 ),
 ( #83745, #30994 ),
 ( #61879, #16297 ),
 ( #23385, #54275 ) ),
 .UNSPECIFIED., .T., .F., .F.,
 ( 4, 2, 2, 2, 2, 2, 2, 2, 2, 2, 2, 2, 2, 2, 2, 2, 4 ),
 ( 2, 2 ),
 ( 0.000000000000000000, 0.06250000000000000000, 0.1250000000000000000, 0.1875000000000000000, 0.2500000000000000000, 0.3125000000000000000, 0.3750000000000000000, 0.4375000000000000000, 0.5000000000000000000, 0.5625000000000000000, 0.6250000000000000000, 0.6875000000000000000, 0.7500000000000000000, 0.8125000000000000000, 0.8750000000000000000, 0.9375000000000000000, 1.000000000000000000 ),
 ( 0.000000000000000000, 1.000000000000000000 ),
 .UNSPECIFIED. ) ;
#306 = EDGE_CURVE ( 'NONE', #13446, #76018, #73820, .T. ) ;
#307 = CARTESIAN_POINT ( 'NONE',  ( 84.83590989842353736, 50.19589791021755332, -13.76099895038702847 ) ) ;
#308 = CARTESIAN_POINT ( 'NONE',  ( 75.63268008801900066, 65.14737934564519151, -14.41129995628930516 ) ) ;
#309 = CARTESIAN_POINT ( 'NONE',  ( 183.6798712561491982, 264.4388490002158960, -13.51192819117503596 ) ) ;
#310 = CARTESIAN_POINT ( 'NONE',  ( 73.99515186948657686, 54.97541550358009488, -16.60506967685200408 ) ) ;
#311 = CARTESIAN_POINT ( 'NONE',  ( 152.6845319923753834, 266.1896283897672220, 17.20844521882669653 ) ) ;
#312 = VERTEX_POINT ( 'NONE', #28205 ) ;
#313 = CARTESIAN_POINT ( 'NONE',  ( 73.43248428410468875, 69.89844921070914552, 9.717079046730820124 ) ) ;
#314 = CARTESIAN_POINT ( 'NONE',  ( 38.69312636016019269, 30.84335787977765619, 9.188101187500006262 ) ) ;
#315 = VERTEX_POINT ( 'NONE', #76800 ) ;
#316 = CARTESIAN_POINT ( 'NONE',  ( 167.5102911960937320, 249.8330499937025309, 6.951336391313942542 ) ) ;
#317 = CARTESIAN_POINT ( 'NONE',  ( -19.77952770554638207, 93.00072136042149396, 59.99999999999999289 ) ) ;
#318 = B_SPLINE_CURVE_WITH_KNOTS ( 'NONE', 3,
 ( #32597, #24493, #55372, #7801 ),
 .UNSPECIFIED., .F., .F.,
 ( 4, 4 ),
 ( 0.02854077651451781411, 0.03771323773808555463 ),
 .UNSPECIFIED. ) ;
#319 = ORIENTED_EDGE ( 'NONE', *, *, #9183, .T. ) ;
#320 = CARTESIAN_POINT ( 'NONE',  ( 86.52915347386752387, 47.38364953835303339, -10.30352551399626648 ) ) ;
#321 = CARTESIAN_POINT ( 'NONE',  ( 158.9773147466768819, 255.2902089383236159, 17.46634807813732237 ) ) ;
#322 = CARTESIAN_POINT ( 'NONE',  ( 192.9115332263593814, 296.5144184163711429, -13.56440505672942898 ) ) ;
#323 = CARTESIAN_POINT ( 'NONE',  ( 163.1062016187225936, 254.8584145212696228, 15.52417137768656019 ) ) ;
#324 = CARTESIAN_POINT ( 'NONE',  ( 41.44395331530407844, 35.87878583063845639, -9.188101187500006262 ) ) ;
#325 = CARTESIAN_POINT ( 'NONE',  ( 80.05943320740847469, 44.70013682444275815, 11.13689609985222617 ) ) ;
#326 = DIRECTION ( 'NONE',  ( 0.2091919045418403900, 0.9778746070300412541, 0.000000000000000000 ) ) ;
#327 = ORIENTED_EDGE ( 'NONE', *, *, #3828, .T. ) ;
#328 = CARTESIAN_POINT ( 'NONE',  ( 195.4130005142917241, 291.0508895501969846, 16.15472393341080348 ) ) ;
#329 = VERTEX_POINT ( 'NONE', #37789 ) ;
#330 = CARTESIAN_POINT ( 'NONE',  ( 81.35074466249913883, 55.80872010294902452, 16.38725056492407361 ) ) ;
#331 = ORIENTED_EDGE ( 'NONE', *, *, #16780, .F. ) ;
#332 = CARTESIAN_POINT ( 'NONE',  ( 171.7871149756895761, 270.4574563033415870, 16.48193621075655102 ) ) ;
#333 = ORIENTED_EDGE ( 'NONE', *, *, #33379, .F. ) ;
#334 = EDGE_CURVE ( 'NONE', #85237, #99635, #55991, .T. ) ;
#335 = DIRECTION ( 'NONE',  ( -0.5000000000000015543, 0.8660254037844378194, 0.000000000000000000 ) ) ;
#336 = CARTESIAN_POINT ( 'NONE',  ( 35.42939366167109938, 22.58380873178788306, 6.180339887498953466 ) ) ;
#337 = CARTESIAN_POINT ( 'NONE',  ( 48.83428215874786815, 87.09189275153327969, -10.00000000000000000 ) ) ;
#338 = CARTESIAN_POINT ( 'NONE',  ( 196.1025787785897307, 284.4507243824010629, -17.50425523595241017 ) ) ;
#339 = CARTESIAN_POINT ( 'NONE',  ( 82.56576626489119519, 41.03778865018932720, 1.100605105531167416 ) ) ;
#340 = CARTESIAN_POINT ( 'NONE',  ( 167.6634616256541790, 249.2278186638985744, -5.457181400944699057 ) ) ;
#341 = DIRECTION ( 'NONE',  ( -0.8660254037844387076, -0.4999999999999998890, -0.000000000000000000 ) ) ;
#342 = EDGE_CURVE ( 'NONE', #62365, #23265, #62078, .T. ) ;
#343 = CARTESIAN_POINT ( 'NONE',  ( 186.8073520874924611, 287.1005927419247996, -15.84640929283254174 ) ) ;
#344 = ADVANCED_FACE ( 'NONE', ( #31678 ), #99228, .T. ) ;
#345 = CARTESIAN_POINT ( 'NONE',  ( 119.1457234225564008, 239.5958772461660544, -9.188101187500095079 ) ) ;
#346 = VERTEX_POINT ( 'NONE', #7914 ) ;
#347 = CARTESIAN_POINT ( 'NONE',  ( 70.49910835669693654, 60.86989013130169468, -15.00567599565220434 ) ) ;
#348 = CARTESIAN_POINT ( 'NONE',  ( 41.71939737199939202, 29.80170272979930246, 7.433330006724137462 ) ) ;
#349 = CARTESIAN_POINT ( 'NONE',  ( 189.4928799553373437, 274.7536700704093846, 17.18705487055967396 ) ) ;
#350 = ORIENTED_EDGE ( 'NONE', *, *, #95990, .T. ) ;
#351 = EDGE_CURVE ( 'NONE', #45858, #78719, #48667, .T. ) ;
#352 = ORIENTED_EDGE ( 'NONE', *, *, #17619, .T. ) ;
#353 = DIRECTION ( 'NONE',  ( -0.000000000000000000, -0.000000000000000000, 1.000000000000000000 ) ) ;
#354 = CARTESIAN_POINT ( 'NONE',  ( -19.56589364647650697, 93.17686168307763239, 59.99999999999999289 ) ) ;
#355 = EDGE_CURVE ( 'NONE', #21265, #77716, #63095, .T. ) ;
#356 = CARTESIAN_POINT ( 'NONE',  ( 171.0928659016861673, 287.7346803495887002, -4.756451642342891972 ) ) ;
#357 = CARTESIAN_POINT ( 'NONE',  ( -54.25007008209492199, 32.21233689110872689, 10.00000000000000000 ) ) ;
#358 = CARTESIAN_POINT ( 'NONE',  ( 72.39980299547302423, 63.20348272691148139, 13.94953712136970836 ) ) ;
#359 = CARTESIAN_POINT ( 'NONE',  ( 153.1961624462112752, 265.3034584490234806, -16.19494717845262954 ) ) ;
#360 = CARTESIAN_POINT ( 'NONE',  ( 177.2362443690770135, 288.8424983797139021, -9.276591687040479428 ) ) ;
#361 = ORIENTED_EDGE ( 'NONE', *, *, #84758, .T. ) ;
#362 = LINE ( 'NONE', #55534, #72254 ) ;
#363 = CARTESIAN_POINT ( 'NONE',  ( 164.5340810747928515, 246.5053760637088658, 4.244836759601243514 ) ) ;
#364 = ORIENTED_EDGE ( 'NONE', *, *, #82612, .F. ) ;
#365 = CARTESIAN_POINT ( 'NONE',  ( 147.9791529310278122, 274.3395839928920168, -7.789432462804474433 ) ) ;
#366 = LINE ( 'NONE', #79411, #99707 ) ;
#367 = ORIENTED_EDGE ( 'NONE', *, *, #49379, .F. ) ;
#368 = CARTESIAN_POINT ( 'NONE',  ( 188.2054311839045226, 266.2807901288332459, -11.82779421608511150 ) ) ;
#369 = CARTESIAN_POINT ( 'NONE',  ( 156.9836120038223726, 276.6206255467238293, 10.24398227673275841 ) ) ;
#370 = CARTESIAN_POINT ( 'NONE',  ( 195.6984238921373560, 265.3498530178097212, 4.338345965406653626 ) ) ;
#371 = CARTESIAN_POINT ( 'NONE',  ( 179.8888715531147682, 274.4711782159853328, -17.82026667163308531 ) ) ;
#372 = PLANE ( 'NONE',  #40302 ) ;
#374 = CARTESIAN_POINT ( 'NONE',  ( 70.01283242295177445, 62.80173547756309915, -13.36538303052352816 ) ) ;
#373 = CARTESIAN_POINT ( 'NONE',  ( 153.4529711877194131, 270.0553744293359841, 14.23171068006870854 ) ) ;
#375 = CARTESIAN_POINT ( 'NONE',  ( 200.7484899876179441, 282.9404111291507888, -16.88964748465601673 ) ) ;
#376 = ORIENTED_EDGE ( 'NONE', *, *, #23774, .F. ) ;
#377 = CARTESIAN_POINT ( 'NONE',  ( 147.4963928429778264, 275.1757489932608109, 4.929816573182678852 ) ) ;
#378 = CARTESIAN_POINT ( 'NONE',  ( 72.32867159652951727, 65.47220889536410482, 12.56686077310279082 ) ) ;
#379 = CARTESIAN_POINT ( 'NONE',  ( 187.3693387071396046, 263.1408467955632204, -9.037621127357647666 ) ) ;
#380 = DIRECTION ( 'NONE',  ( 0.000000000000000000, 1.000000000000000000, 0.000000000000000000 ) ) ;
#381 = CARTESIAN_POINT ( 'NONE',  ( 173.8665542827094725, 250.6399523573830095, -0.9454928766311748722 ) ) ;
#382 = B_SPLINE_CURVE_WITH_KNOTS ( 'NONE', 3,
 ( #16996, #47885, #78827, #78323 ),
 .UNSPECIFIED., .F., .F.,
 ( 4, 4 ),
 ( 0.003697259335896347244, 0.01166702794401381499 ),
 .UNSPECIFIED. ) ;
#383 = CARTESIAN_POINT ( 'NONE',  ( 184.7157775894015117, 297.3647472220100099, -4.497232409310948142 ) ) ;
#384 = CARTESIAN_POINT ( 'NONE',  ( 45.79324619304848909, 117.8999360398438512, 177.5919119679930134 ) ) ;
#385 = CARTESIAN_POINT ( 'NONE',  ( 23.13271821863878230, 13.75978393459164195, -1.583844403245362020 ) ) ;
#386 = CARTESIAN_POINT ( 'NONE',  ( 155.2419697281468416, 261.7600162942170527, 18.58580762350309357 ) ) ;
#387 = CARTESIAN_POINT ( 'NONE',  ( 191.1424450985878138, 283.3691956586972083, -16.58317466969614173 ) ) ;
#388 = CARTESIAN_POINT ( 'NONE',  ( 82.68215287466908592, 53.55713939286302150, -15.73562046651999502 ) ) ;
#389 = CARTESIAN_POINT ( 'NONE',  ( 84.82981389336303835, 207.5327760586659167, 1.948934522072303157E-15 ) ) ;
#390 = CARTESIAN_POINT ( 'NONE',  ( -59.85755863633952600, 35.44530052843370527, 10.00000000000000000 ) ) ;
#391 = DIRECTION ( 'NONE',  ( 0.000000000000000000, 0.000000000000000000, 1.000000000000000000 ) ) ;
#392 = DIRECTION ( 'NONE',  ( -1.000000000000000000, 0.000000000000000000, 0.000000000000000000 ) ) ;
#393 = EDGE_CURVE ( 'NONE', #90851, #29361, #37739, .T. ) ;
#394 = CARTESIAN_POINT ( 'NONE',  ( 202.8535267948003593, 279.2943804273081696, -15.36804658072946062 ) ) ;
#395 = DIRECTION ( 'NONE',  ( 0.4999999999999992784, -0.8660254037844390407, 0.000000000000000000 ) ) ;
#396 = CARTESIAN_POINT ( 'NONE',  ( 84.87359499838788679, 50.02211777990267194, -13.22747082306951327 ) ) ;
#397 = CARTESIAN_POINT ( 'NONE',  ( 48.76667776935668996, 187.4155109091896065, 2.679491924311254714 ) ) ;
#399 = CARTESIAN_POINT ( 'NONE',  ( 75.97293632993350343, 51.42040260576536781, 16.16535879681820731 ) ) ;
#398 = CARTESIAN_POINT ( 'NONE',  ( 73.56775416758397057, 69.23451306489744184, -10.00871374113025070 ) ) ;
#400 = FACE_OUTER_BOUND ( 'NONE', #98699, .T. ) ;
#401 = CARTESIAN_POINT ( 'NONE',  ( 166.1592670111344887, 249.7066296865716311, -9.087955240109561572 ) ) ;
#402 = CARTESIAN_POINT ( 'NONE',  ( 205.5338712131946863, 274.6518877128656868, -12.59077173197751343 ) ) ;
#403 = CARTESIAN_POINT ( 'NONE',  ( 195.8248271798537417, 291.4684452715354155, 17.35175160929494709 ) ) ;
#404 = CARTESIAN_POINT ( 'NONE',  ( 167.9211111253673323, 249.4040118433879627, 8.061254949035708606 ) ) ;
#405 = CARTESIAN_POINT ( 'NONE',  ( 207.5785076975260779, 271.1104734389944042, -6.824813054587777650 ) ) ;
#406 = CARTESIAN_POINT ( 'NONE',  ( 43.09804120061789945, 189.5643266524160140, 9.188101187500095079 ) ) ;
#407 = CARTESIAN_POINT ( 'NONE',  ( 56.16917826928300883, 212.4244531367911577, -4.594050593750046652 ) ) ;
#408 = CARTESIAN_POINT ( 'NONE',  ( 185.8626946602280441, 259.3471889805154547, 7.308832903665572367 ) ) ;
#410 = EDGE_CURVE ( 'NONE', #10093, #75363, #77822, .T. ) ;
#409 = CARTESIAN_POINT ( 'NONE',  ( 75.75493378409400691, 65.86437009324525604, -14.07593894684414693 ) ) ;
#411 = CARTESIAN_POINT ( 'NONE',  ( 163.8983913010820572, 258.1275895590765685, 15.54516205773220250 ) ) ;
#412 = CARTESIAN_POINT ( 'NONE',  ( -3.441976700948088386, 155.4865022471901455, 1.119607411625061291E-15 ) ) ;
#413 = CARTESIAN_POINT ( 'NONE',  ( 66.36268096397610350, 69.44190093015801324, 9.875986171954755521E-07 ) ) ;
#414 = DIRECTION ( 'NONE',  ( -0.2270762630343793331, 0.9738769792773321887, 0.000000000000000000 ) ) ;
#415 = CARTESIAN_POINT ( 'NONE',  ( 27.04628097738780212, 27.56628583063842086, 9.188101187500006262 ) ) ;
#416 = CARTESIAN_POINT ( 'NONE',  ( 132.8668134119921547, 247.5177522451418497, -10.00000000000009592 ) ) ;
#417 = CARTESIAN_POINT ( 'NONE',  ( 81.38192374540615504, 47.39962897157295885, -12.69884445555879360 ) ) ;
#418 = CARTESIAN_POINT ( 'NONE',  ( 11.61057445305848823, 22.10171378149917842, 9.188101187500008038 ) ) ;
#419 = CARTESIAN_POINT ( 'NONE',  ( 70.29673831216418023, 202.2048013555409796, 4.594050593750051981 ) ) ;
#420 = CARTESIAN_POINT ( 'NONE',  ( 77.30463285345523161, 63.36080703450485174, 15.53535672671000079 ) ) ;
#421 = CARTESIAN_POINT ( 'NONE',  ( 155.2193237801463113, 261.7992402267395846, -18.58295809893692407 ) ) ;
#422 = CARTESIAN_POINT ( 'NONE',  ( 159.6978881494930249, 254.0421391940632532, 15.34888828951022610 ) ) ;
#423 = CARTESIAN_POINT ( 'NONE',  ( 67.41248320326423027, 66.37693208286884783, -8.946798147498746800 ) ) ;
#424 = CARTESIAN_POINT ( 'NONE',  ( 153.3576077035983758, 276.7962943880863804, 7.310696788985877603 ) ) ;
#425 = EDGE_CURVE ( 'NONE', #74638, #6038, #70695, .T. ) ;
#426 = B_SPLINE_CURVE_WITH_KNOTS ( 'NONE', 3,
 ( #1225, #30627, #55888, #713 ),
 .UNSPECIFIED., .F., .F.,
 ( 4, 4 ),
 ( 0.04422796245080886507, 0.04887120950165270428 ),
 .UNSPECIFIED. ) ;
#427 = EDGE_CURVE ( 'NONE', #15755, #20151, #43801, .T. ) ;
#428 = CARTESIAN_POINT ( 'NONE',  ( 80.28226457095783530, 55.01127608260450330, -15.95866588083628557 ) ) ;
#429 = CARTESIAN_POINT ( 'NONE',  ( 113.4714528099510744, 242.9865022471902876, -10.00000000000009415 ) ) ;
#430 = CARTESIAN_POINT ( 'NONE',  ( 200.8828793852583203, 282.7076418644388696, 17.90302398138411633 ) ) ;
#431 = CARTESIAN_POINT ( 'NONE',  ( 164.4440639631384045, 245.8215215431751233, -2.910115319305802029 ) ) ;
#432 = ORIENTED_EDGE ( 'NONE', *, *, #46720, .F. ) ;
#433 = CARTESIAN_POINT ( 'NONE',  ( 32.24342178309110096, 47.97677246190463052, 10.00000000000000000 ) ) ;
#434 = CARTESIAN_POINT ( 'NONE',  ( 82.50452235219570696, 53.86480448276186905, 15.85105177732747173 ) ) ;
#435 = ORIENTED_EDGE ( 'NONE', *, *, #30362, .T. ) ;
#436 = CARTESIAN_POINT ( 'NONE',  ( 206.1405152101578437, 273.6011494880188479, -9.618815605734603480 ) ) ;
#437 = CARTESIAN_POINT ( 'NONE',  ( 190.3113039736807934, 278.6935773923744364, -16.50932879894303085 ) ) ;
#438 = CARTESIAN_POINT ( 'NONE',  ( -47.78078991586326651, 28.96484896693080913, -10.00000000000000000 ) ) ;
#439 = EDGE_LOOP ( 'NONE', ( #58462, #85908, #2245, #41062 ) ) ;
#440 = CARTESIAN_POINT ( 'NONE',  ( 173.3330552357551824, 251.5762317818503959, 0.1350323028907620126 ) ) ;
#441 = VERTEX_POINT ( 'NONE', #51248 ) ;
#442 = LINE ( 'NONE', #39415, #16658 ) ;
#443 = CARTESIAN_POINT ( 'NONE',  ( 147.8308140999695866, 274.5965143850199865, -7.866624397492971710 ) ) ;
#444 = CARTESIAN_POINT ( 'NONE',  ( 82.09009853944208146, 44.85671956714123354, 10.87987463625776741 ) ) ;
#446 = ORIENTED_EDGE ( 'NONE', *, *, #42908, .T. ) ;
#445 = VECTOR ( 'NONE', #6291, 1000.000000000000000 ) ;
#447 = CARTESIAN_POINT ( 'NONE',  ( 23.73796034364816521, 35.74646525600390845, 2.839279412974139660 ) ) ;
#448 = CARTESIAN_POINT ( 'NONE',  ( 79.97518497192163522, 44.56399469350409959, 11.74208085782137267 ) ) ;
#449 = DIRECTION ( 'NONE',  ( 0.8660254037844391517, 0.4999999999999990008, 0.000000000000000000 ) ) ;
#450 = CARTESIAN_POINT ( 'NONE',  ( 75.08013308270209052, 67.09339902234967212, -13.09435070823463043 ) ) ;
#451 = AXIS2_PLACEMENT_3D ( 'NONE', #67847, #36429, #6548 ) ;
#452 = ORIENTED_EDGE ( 'NONE', *, *, #76491, .T. ) ;
#453 = CARTESIAN_POINT ( 'NONE',  ( -13.11024591527723437, 27.99999999999999645, -17.00000000000016698 ) ) ;
#454 = CARTESIAN_POINT ( 'NONE',  ( 206.7680519836501958, 272.5142239127119979, -10.57935479673322021 ) ) ;
#455 = ORIENTED_EDGE ( 'NONE', *, *, #60528, .T. ) ;
#456 = CARTESIAN_POINT ( 'NONE',  ( 174.8047606067528363, 286.1344884131184472, 10.79450168243746688 ) ) ;
#457 = EDGE_CURVE ( 'NONE', #20349, #15680, #60827, .T. ) ;
#459 = FACE_OUTER_BOUND ( 'NONE', #67397, .T. ) ;
#458 = CARTESIAN_POINT ( 'NONE',  ( 162.5887743522035294, 284.9919049736276975, -2.844505511527740005 ) ) ;
#460 = CARTESIAN_POINT ( 'NONE',  ( 163.4218292706009095, 247.5920839679097014, -10.44611490715852042 ) ) ;
#461 = CARTESIAN_POINT ( 'NONE',  ( 204.9103773355753617, 275.7318107871104189, 13.62808820451859937 ) ) ;
#462 = CARTESIAN_POINT ( 'NONE',  ( 185.4002507578896086, 292.6011188852542091, -10.72436994641770269 ) ) ;
#463 = CARTESIAN_POINT ( 'NONE',  ( 164.3112807403088595, 265.7596940169248683, -17.57772941833111346 ) ) ;
#464 = CARTESIAN_POINT ( 'NONE',  ( 141.8249372320439647, 246.5643266524160140, 9.188101187500095079 ) ) ;
#465 = CARTESIAN_POINT ( 'NONE',  ( 165.2663344650013642, 263.6115507486170486, 17.68040007492823662 ) ) ;
#466 = VECTOR ( 'NONE', #65332, 1000.000000000000114 ) ;
#467 = CARTESIAN_POINT ( 'NONE',  ( 181.8478599454992661, 260.3285582005539709, 9.484317556428793594 ) ) ;
#468 = CARTESIAN_POINT ( 'NONE',  ( 71.08131351252005459, 211.8458772461660544, 9.188101187500095079 ) ) ;
#469 = VERTEX_POINT ( 'NONE', #18019 ) ;
#470 = CARTESIAN_POINT ( 'NONE',  ( 191.0900422946452011, 299.6693332556258724, 8.872191398975367349 ) ) ;
#471 = DIRECTION ( 'NONE',  ( 0.8660254037844373753, 0.5000000000000021094, 0.000000000000000000 ) ) ;
#472 = ORIENTED_EDGE ( 'NONE', *, *, #57842, .T. ) ;
#473 = CARTESIAN_POINT ( 'NONE',  ( 196.0559066898898379, 291.0682038195648715, -16.90522961251436485 ) ) ;
#474 = ORIENTED_EDGE ( 'NONE', *, *, #73314, .T. ) ;
#475 = CARTESIAN_POINT ( 'NONE',  ( 67.16327201103491973, 67.73731889023997610, 6.573435314091265802 ) ) ;
#476 = EDGE_CURVE ( 'NONE', #86658, #66772, #15991, .T. ) ;
#477 = DIRECTION ( 'NONE',  ( -0.000000000000000000, 0.000000000000000000, 1.000000000000000000 ) ) ;
#478 = CARTESIAN_POINT ( 'NONE',  ( -32.68486601307109396, 95.73265939123938040, 11.22505256784756611 ) ) ;
#479 = CARTESIAN_POINT ( 'NONE',  ( 81.11670802570714045, 56.15934143863493944, 16.10866441373284630 ) ) ;
#480 = CARTESIAN_POINT ( 'NONE',  ( 56.79295721098551297, 192.0494855054051868, -2.679491924311248496 ) ) ;
#481 = CARTESIAN_POINT ( 'NONE',  ( 162.4279131726858623, 249.3135971479585464, 10.85034575916916921 ) ) ;
#482 = CARTESIAN_POINT ( 'NONE',  ( 87.75264963113552596, 209.2202760586659167, -5.415160957724236172E-17 ) ) ;
#483 = VERTEX_POINT ( 'NONE', #71220 ) ;
#484 = ADVANCED_BREP_SHAPE_REPRESENTATION ( '', ( #42857, #68784 ), #81782 ) ;
#485 = ORIENTED_EDGE ( 'NONE', *, *, #51159, .T. ) ;
#486 = CARTESIAN_POINT ( 'NONE',  ( 82.41630873631589793, 41.31828431233920895, -3.367117793111288560 ) ) ;
#487 = CARTESIAN_POINT ( 'NONE',  ( 161.3271158790198001, 251.2202339894231216, -13.00083852162470244 ) ) ;
#488 = EDGE_LOOP ( 'NONE', ( #46553, #54812, #94039, #23503 ) ) ;
#489 = CARTESIAN_POINT ( 'NONE',  ( 76.44840390471171077, 51.64438224287277279, -16.15499642960158155 ) ) ;
#490 = CARTESIAN_POINT ( 'NONE',  ( 184.0117498620529659, 275.1892951444139612, 16.37277468287277671 ) ) ;
#491 = ADVANCED_FACE ( 'NONE', ( #88467 ), #10916, .T. ) ;
#492 = CARTESIAN_POINT ( 'NONE',  ( 206.4695239676918845, 273.0312896038346366, 10.41704154450801667 ) ) ;
#493 = CARTESIAN_POINT ( 'NONE',  ( 161.9109773315472012, 284.6651530195127293, 0.5383145704399616704 ) ) ;
#494 = CARTESIAN_POINT ( 'NONE',  ( -80.08603253397791377, 57.73992072201551906, 177.5919119679930134 ) ) ;
#495 = CARTESIAN_POINT ( 'NONE',  ( 162.8949375270381665, 261.5393056731645061, 17.17550692532979895 ) ) ;
#496 = ORIENTED_EDGE ( 'NONE', *, *, #84432, .T. ) ;
#497 = CARTESIAN_POINT ( 'NONE',  ( 82.82785115793576836, 43.65967190867092285, -8.128949345812960914 ) ) ;
#498 = CARTESIAN_POINT ( 'NONE',  ( -59.87889494062799400, 37.30571521936384016, 10.00000000000000000 ) ) ;
#499 = CARTESIAN_POINT ( 'NONE',  ( 152.9251141908703175, 265.7729277985770864, -16.20110192949203309 ) ) ;
#500 = CARTESIAN_POINT ( 'NONE',  ( 72.42095758685501039, 70.73706075180957953, 7.727740079816340035 ) ) ;
#501 = CARTESIAN_POINT ( 'NONE',  ( 69.17735699518412673, 67.42632015883337715, -8.956856073786124028 ) ) ;
#502 = ORIENTED_EDGE ( 'NONE', *, *, #85667, .F. ) ;
#503 = CARTESIAN_POINT ( 'NONE',  ( 195.7907645185857461, 265.4364973583962524, 4.438536951565118294 ) ) ;
#504 = CARTESIAN_POINT ( 'NONE',  ( 98.80083580102480312, 239.3967562850347122, -4.648177544792955347E-16 ) ) ;
#505 = DIRECTION ( 'NONE',  ( -0.8660254037844385966, -0.4999999999999999445, 5.782411586589351229E-17 ) ) ;
#506 = CARTESIAN_POINT ( 'NONE',  ( 187.8986993795193428, 266.2277010579576881, -11.94388868202539911 ) ) ;
#507 = CARTESIAN_POINT ( 'NONE',  ( 198.6368176188399275, 266.0031191539155770, 1.462458297540865537 ) ) ;
#508 = EDGE_CURVE ( 'NONE', #53392, #59506, #69113, .T. ) ;
#509 = FACE_OUTER_BOUND ( 'NONE', #80990, .T. ) ;
#510 = B_SPLINE_CURVE_WITH_KNOTS ( 'NONE', 3,
 ( #45409, #38802, #46912, #7929 ),
 .UNSPECIFIED., .F., .F.,
 ( 4, 4 ),
 ( 0.02277490244884483594, 0.03199231217593029308 ),
 .UNSPECIFIED. ) ;
#511 = VERTEX_POINT ( 'NONE', #55477 ) ;
#512 = DIRECTION ( 'NONE',  ( -1.000000000000000000, 0.000000000000000000, 5.984665299743594308E-16 ) ) ;
#513 = CARTESIAN_POINT ( 'NONE',  ( 202.5511585997265911, 279.8180975037686835, 17.12781264818056925 ) ) ;
#514 = DIRECTION ( 'NONE',  ( -0.8660254037844359321, -0.5000000000000051070, -0.000000000000000000 ) ) ;
#516 = FACE_BOUND ( 'NONE', #48775, .T. ) ;
#515 = CARTESIAN_POINT ( 'NONE',  ( -29.31672308591111431, 23.47304723416778316, -10.00000000000000000 ) ) ;
#517 = CARTESIAN_POINT ( 'NONE',  ( 176.1295626651131556, 285.2769818187388751, -12.16386616229632800 ) ) ;
#518 = CIRCLE ( 'NONE', #92746, 0.1418229129680845801 ) ;
#519 = CARTESIAN_POINT ( 'NONE',  ( 32.89180500207565672, 24.15404122711135670, 8.090169943749479842 ) ) ;
#520 = CARTESIAN_POINT ( 'NONE',  ( 168.9255865893414921, 272.9744073663551376, 15.96626197445653261 ) ) ;
#521 = FACE_OUTER_BOUND ( 'NONE', #76798, .T. ) ;
#522 = CARTESIAN_POINT ( 'NONE',  ( 176.3945350884862933, 261.0281843545697029, -14.71337765310037504 ) ) ;
#523 = CARTESIAN_POINT ( 'NONE',  ( 188.2324206269368858, 260.8148967101335529, 3.170919259758945952 ) ) ;
#524 = CARTESIAN_POINT ( 'NONE',  ( 12.40843950188935629, 165.7202760586659736, -5.415160957724236172E-17 ) ) ;
#525 = CARTESIAN_POINT ( 'NONE',  ( 48.98007068238331385, 88.97864505566217019, 10.00000000000000000 ) ) ;
#526 = VERTEX_POINT ( 'NONE', #86463 ) ;
#528 = CARTESIAN_POINT ( 'NONE',  ( -22.42236680055709641, 157.8615022471902591, 0.000000000000000000 ) ) ;
#527 = VECTOR ( 'NONE', #79353, 1000.000000000000000 ) ;
#529 = CARTESIAN_POINT ( 'NONE',  ( 13.40335115377346753, 31.23654200823201776, 1.583844403245363353 ) ) ;
#530 = CARTESIAN_POINT ( 'NONE',  ( 81.82787295522399518, 41.24789425966510947, 5.851439987416612531 ) ) ;
#531 = CARTESIAN_POINT ( 'NONE',  ( 25.61497981383703149, 185.5958772461660544, -9.188101187500095079 ) ) ;
#532 = CARTESIAN_POINT ( 'NONE',  ( 22.06360519161784595, 36.23654200823203553, 1.583844403245363353 ) ) ;
#533 = CARTESIAN_POINT ( 'NONE',  ( 30.89548221274965556, 26.03677371833803633, 10.00000000000000533 ) ) ;
#534 = CARTESIAN_POINT ( 'NONE',  ( 86.35121876318000034, 43.08468197994678661, 0.3078304325362931637 ) ) ;
#535 = CARTESIAN_POINT ( 'NONE',  ( 191.7247331938518187, 298.5700163710982338, -9.650650827884682315 ) ) ;
#536 = CARTESIAN_POINT ( 'NONE',  ( 142.5294721856450053, 241.5494855054051584, -2.679491924311248496 ) ) ;
#537 = B_SPLINE_SURFACE_WITH_KNOTS ( 'NONE', 3, 1, ( 
 ( #25794, #64786 ),
 ( #41970, #96714 ),
 ( #10586, #19203 ),
 ( #57158, #3497 ),
 ( #88139, #43459 ),
 ( #50560, #42940 ),
 ( #41459, #81030 ),
 ( #96214, #56670 ),
 ( #73879, #4472 ),
 ( #26777, #57658 ),
 ( #11593, #11095 ),
 ( #34855, #82013 ),
 ( #66275, #97210 ),
 ( #89625, #74400 ),
 ( #87655, #49084 ),
 ( #80017, #72402 ),
 ( #3009, #33901 ),
 ( #95732, #26284 ),
 ( #18685, #49568 ),
 ( #72907, #14572 ),
 ( #75892, #28768 ),
 ( #22162, #29274 ),
 ( #15043, #76853 ),
 ( #5967, #43950 ),
 ( #98186, #30258 ),
 ( #82527, #74889 ),
 ( #84500, #22668 ),
 ( #59650, #97693 ),
 ( #98692, #37349 ),
 ( #28262, #45448 ),
 ( #90621, #44952 ),
 ( #92116, #36356 ),
 ( #76381, #21185 ),
 ( #14066, #60636 ) ),
 .UNSPECIFIED., .T., .F., .F.,
 ( 4, 2, 2, 2, 2, 2, 2, 2, 2, 2, 2, 2, 2, 2, 2, 2, 4 ),
 ( 2, 2 ),
 ( 0.000000000000000000, 0.06250000000000000000, 0.1250000000000000000, 0.1875000000000000000, 0.2500000000000000000, 0.3125000000000000000, 0.3750000000000000000, 0.4375000000000000000, 0.5000000000000000000, 0.5625000000000000000, 0.6250000000000000000, 0.6875000000000000000, 0.7500000000000000000, 0.8125000000000000000, 0.8750000000000000000, 0.9375000000000000000, 1.000000000000000000 ),
 ( 0.000000000000000000, 1.000000000000000000 ),
 .UNSPECIFIED. ) ;
#538 = CARTESIAN_POINT ( 'NONE',  ( 87.18439463908147502, 46.15779724344488244, -8.329569831597547491 ) ) ;
#539 = CARTESIAN_POINT ( 'NONE',  ( 174.3697573357644899, 277.1653490889620457, -17.12727634137145571 ) ) ;
#540 = EDGE_CURVE ( 'NONE', #56147, #90103, #63596, .T. ) ;
#541 = EDGE_CURVE ( 'NONE', #2236, #46058, #2271, .T. ) ;
#542 = CARTESIAN_POINT ( 'NONE',  ( 183.0713581288837304, 295.8141884393991745, 1.453977782348063963 ) ) ;
#543 = CARTESIAN_POINT ( 'NONE',  ( 64.97403019802248991, 214.9865022471903160, 10.00000000000009237 ) ) ;
#544 = CARTESIAN_POINT ( 'NONE',  ( 72.32117545662791258, 66.44659970230358681, -11.84374507886356831 ) ) ;
#545 = CARTESIAN_POINT ( 'NONE',  ( 205.7559715084180425, 271.1536124878838336, 6.114938359024117531 ) ) ;
#546 = EDGE_CURVE ( 'NONE', #4549, #55003, #44142, .T. ) ;
#547 = CARTESIAN_POINT ( 'NONE',  ( 24.66750420662404508, 194.2369531367911293, -4.594050593750048428 ) ) ;
#548 = CARTESIAN_POINT ( 'NONE',  ( 66.29454943693275482, 69.24199052626691753, -2.144636311159408226 ) ) ;
#549 = EDGE_CURVE ( 'NONE', #7391, #22636, #70359, .T. ) ;
#550 = CARTESIAN_POINT ( 'NONE',  ( 73.72680694775513643, 201.8262482093457777, 3.021315404115420679E-15 ) ) ;
#551 = CARTESIAN_POINT ( 'NONE',  ( 198.8570476668614049, 286.2164853282868080, -17.01721544293231858 ) ) ;
#552 = LINE ( 'NONE', #17762, #100067 ) ;
#553 = PLANE ( 'NONE',  #11961 ) ;
#554 = CARTESIAN_POINT ( 'NONE',  ( 159.9770076892122006, 278.5918188642896212, -9.796288430209179054 ) ) ;
#555 = DIRECTION ( 'NONE',  ( -0.8660254037844384856, -0.5000000000000002220, 5.782411586589354927E-17 ) ) ;
#556 = SHAPE_DEFINITION_REPRESENTATION ( #17576, #88422 ) ;
#557 = CARTESIAN_POINT ( 'NONE',  ( 19.25324864145614612, 26.51421378149919761, -9.188101187500004485 ) ) ;
#558 = CARTESIAN_POINT ( 'NONE',  ( 190.5444288681022442, 300.6143634316900943, -1.000014190476072873 ) ) ;
#559 = CARTESIAN_POINT ( 'NONE',  ( 100.0535195437283988, 240.1199935810941213, 2.679491924311251605 ) ) ;
#560 = DIRECTION ( 'NONE',  ( -0.000000000000000000, -0.000000000000000000, -1.000000000000000000 ) ) ;
#561 = ORIENTED_EDGE ( 'NONE', *, *, #16214, .T. ) ;
#562 = CARTESIAN_POINT ( 'NONE',  ( 185.5148080131019412, 290.8628339942631555, 13.12244952321606206 ) ) ;
#563 = CARTESIAN_POINT ( 'NONE',  ( 7.601631632957885465, 27.49540643055185285, 3.479690158560446702E-15 ) ) ;
#564 = DIRECTION ( 'NONE',  ( -0.4996954135095461047, 0.8654978445076770832, -0.03489949670251103753 ) ) ;
#565 = CARTESIAN_POINT ( 'NONE',  ( -3.532187684056978583, 178.7677522451419350, -5.000000000000047962 ) ) ;
#566 = VERTEX_POINT ( 'NONE', #60825 ) ;
#567 = CARTESIAN_POINT ( 'NONE',  ( 174.1456200854750023, 291.7975269716956177, -2.042136877227955782 ) ) ;
#568 = CARTESIAN_POINT ( 'NONE',  ( 72.40022343535652283, 71.86297034063233014, -5.456689119915505870 ) ) ;
#569 = CARTESIAN_POINT ( 'NONE',  ( 150.8167050463783312, 269.4247995599803289, 14.38040671671637938 ) ) ;
#570 = CARTESIAN_POINT ( 'NONE',  ( 180.2008674086625888, 256.3788900776044102, -7.862092545524210330 ) ) ;
#571 = ORIENTED_EDGE ( 'NONE', *, *, #75290, .T. ) ;
#572 = ORIENTED_EDGE ( 'NONE', *, *, #79852, .F. ) ;
#574 = CARTESIAN_POINT ( 'NONE',  ( 83.55937078812219454, 42.48588548430609535, -5.103737020810437564 ) ) ;
#573 = CARTESIAN_POINT ( 'NONE',  ( 189.0587110057432483, 273.8589833282692325, -15.65961006902252883 ) ) ;
#575 = ORIENTED_EDGE ( 'NONE', *, *, #83693, .F. ) ;
#576 = CARTESIAN_POINT ( 'NONE',  ( 191.3375250863502970, 299.2406804863936145, 8.828791580707859410 ) ) ;
#577 = PLANE ( 'NONE',  #1141 ) ;
#578 = CARTESIAN_POINT ( 'NONE',  ( 72.73633344227268083, 57.02636325111804183, -16.39140812357083021 ) ) ;
#579 = CARTESIAN_POINT ( 'NONE',  ( 76.64464310018406934, 63.53199411942404851, 15.34601863127964627 ) ) ;
#580 = CARTESIAN_POINT ( 'NONE',  ( 190.5154909595809727, 300.6644853595138329, -0.04129855346138300298 ) ) ;
#581 = CIRCLE ( 'NONE', #62027, 70.00000000000001421 ) ;
#582 = ORIENTED_EDGE ( 'NONE', *, *, #61102, .F. ) ;
#583 = DIRECTION ( 'NONE',  ( -0.000000000000000000, -0.000000000000000000, -1.000000000000000000 ) ) ;
#584 = CARTESIAN_POINT ( 'NONE',  ( 161.8159150606452670, 267.0902596021308568, 16.49972241951906327 ) ) ;
#585 = ORIENTED_EDGE ( 'NONE', *, *, #42908, .F. ) ;
#586 = CARTESIAN_POINT ( 'NONE',  ( 26.72152145096863762, 27.37878583063842086, 9.188101187500006262 ) ) ;
#587 = CARTESIAN_POINT ( 'NONE',  ( 149.5593209768671841, 271.6026526530012575, 11.55487339793564949 ) ) ;
#588 = CARTESIAN_POINT ( 'NONE',  ( 78.31654463311403447, 47.36115395161638020, -14.27160036167827784 ) ) ;
#589 = ORIENTED_EDGE ( 'NONE', *, *, #57818, .F. ) ;
#590 = CARTESIAN_POINT ( 'NONE',  ( -8.413379660334708632, 72.70744834316617755, 14.99993878877685916 ) ) ;
#591 = LINE ( 'NONE', #85759, #53118 ) ;
#592 = CARTESIAN_POINT ( 'NONE',  ( 150.2494575935072874, 270.4073009688167986, 14.61449051812962985 ) ) ;
#593 = CARTESIAN_POINT ( 'NONE',  ( 83.35161352719694605, 52.40881748729520240, 14.85180384881482674 ) ) ;
#594 = ORIENTED_EDGE ( 'NONE', *, *, #77639, .T. ) ;
#595 = EDGE_LOOP ( 'NONE', ( #20192, #17699, #51168, #51804 ) ) ;
#596 = CARTESIAN_POINT ( 'NONE',  ( 86.83016860379825630, 46.47919197584165119, 9.056981041330921300 ) ) ;
#598 = AXIS2_PLACEMENT_3D ( 'NONE', #72578, #77279, #80192 ) ;
#597 = CARTESIAN_POINT ( 'NONE',  ( 81.64670023727850889, 42.65128533460878657, -7.584980231169042852 ) ) ;
#599 = DIRECTION ( 'NONE',  ( 0.8660254037844382635, 0.5000000000000005551, 0.000000000000000000 ) ) ;
#600 = CARTESIAN_POINT ( 'NONE',  ( 190.5444288681022442, 300.6143634316900943, -1.000014190476072873 ) ) ;
#601 = ORIENTED_EDGE ( 'NONE', *, *, #47729, .T. ) ;
#602 = CARTESIAN_POINT ( 'NONE',  ( 190.6023073677431512, 300.5141149296460981, 3.174888932019753973 ) ) ;
#603 = CARTESIAN_POINT ( 'NONE',  ( 132.5758265486178971, 258.8967562850347122, -4.648177544792955347E-16 ) ) ;
#604 = CARTESIAN_POINT ( 'NONE',  ( 191.0739205222354258, 299.6972569845476073, 8.800115285385583519 ) ) ;
#605 = CARTESIAN_POINT ( 'NONE',  ( 147.4323331177958494, 275.2867036919951147, -5.064030047414062707 ) ) ;
#606 = VECTOR ( 'NONE', #83343, 1000.000000000000114 ) ;
#607 = CARTESIAN_POINT ( 'NONE',  ( 163.5023530932012079, 257.7703811534142346, 15.52546879389397461 ) ) ;
#608 = ADVANCED_FACE ( 'NONE', ( #98877 ), #22352, .T. ) ;
#609 = CARTESIAN_POINT ( 'NONE',  ( 69.00186724958503248, 65.47144582019447512, 10.96851354096545883 ) ) ;
#610 = CARTESIAN_POINT ( 'NONE',  ( 205.7576124508049418, 274.2643565215761328, 10.88614016733041545 ) ) ;
#611 = CARTESIAN_POINT ( 'NONE',  ( 67.43691672556117567, 66.98928061623196584, 9.017019808546432813 ) ) ;
#612 = CARTESIAN_POINT ( 'NONE',  ( 70.21952773771840839, 65.49792867059230161, -11.57245437907510244 ) ) ;
#613 = CARTESIAN_POINT ( 'NONE',  ( 78.41127520731549794, 47.42400182521100049, 14.27580055608907017 ) ) ;
#614 = CARTESIAN_POINT ( 'NONE',  ( 115.2218061334819623, 228.1423013555409796, -4.594050593750043987 ) ) ;
#615 = ORIENTED_EDGE ( 'NONE', *, *, #63474, .T. ) ;
#616 = CARTESIAN_POINT ( 'NONE',  ( 190.0576675296552764, 301.4574588010404455, -4.282990501740621347 ) ) ;
#617 = CARTESIAN_POINT ( 'NONE',  ( 69.93192355902827728, 64.35613849418326993, 12.34049615428977198 ) ) ;
#618 = PLANE ( 'NONE',  #9162 ) ;
#619 = CARTESIAN_POINT ( 'NONE',  ( 203.1705638993064156, 278.7452560544191442, -15.08126533799095093 ) ) ;
#620 = B_SPLINE_CURVE_WITH_KNOTS ( 'NONE', 3,
 ( #66257, #11575, #42433, #82510, #73367, #65740, #96694, #4966, #27759, #58631, #27263, #89605, #41953, #96197, #74384, #34355, #51036, #26758, #35849, #58146, #19678, #72382, #66742, #59118, #90091, #95716, #64767, #20659, #51548, #2992, #33882 ),
 .UNSPECIFIED., .F., .F.,
 ( 4, 3, 3, 3, 3, 3, 3, 3, 3, 3, 4 ),
 ( 0.000000000000000000, 0.1333490885032305451, 0.3007194338854253246, 0.4699862290244986029, 0.5844252810809236198, 0.6686540514502520294, 0.7354980260655306079, 0.8028463152565280536, 0.8633854507756927310, 0.9437142632666988273, 1.000000000000000000 ),
 .UNSPECIFIED. ) ;
#621 = CARTESIAN_POINT ( 'NONE',  ( 192.6159067191336476, 296.6392389330721926, 11.36185169173896448 ) ) ;
#622 = CARTESIAN_POINT ( 'NONE',  ( 83.88626965845651284, 51.63168102053428754, -14.39363241527635751 ) ) ;
#623 = CARTESIAN_POINT ( 'NONE',  ( 198.6444633007815810, 284.5846922512318997, -17.80363864581810418 ) ) ;
#624 = ORIENTED_EDGE ( 'NONE', *, *, #90672, .T. ) ;
#625 = CARTESIAN_POINT ( 'NONE',  ( 162.9383752892161397, 248.4294508267893491, -11.25953730674605957 ) ) ;
#627 = ADVANCED_FACE ( 'NONE', ( #24842 ), #553, .F. ) ;
#626 = CARTESIAN_POINT ( 'NONE',  ( 72.54208641595317886, 71.58009272687419866, 5.313622202418648577 ) ) ;
#628 = CARTESIAN_POINT ( 'NONE',  ( 206.3009434829942279, 272.9081483067511158, 8.547891559723822752 ) ) ;
#629 = CARTESIAN_POINT ( 'NONE',  ( 124.8827946268633298, 255.1589784336661069, -6.496448406907676862E-16 ) ) ;
#630 = CARTESIAN_POINT ( 'NONE',  ( 190.2913651263166628, 294.6875229615724265, -12.30047797060472803 ) ) ;
#631 = DIRECTION ( 'NONE',  ( -0.2347357813929480952, 0.4065742997269687908, 0.8829475928589233247 ) ) ;
#632 = CARTESIAN_POINT ( 'NONE',  ( 196.2609093297512857, 290.7131288316392670, 16.03897268885959448 ) ) ;
#633 = CARTESIAN_POINT ( 'NONE',  ( 83.18659939620825128, 40.82302332894202124, -0.8845490628100145525 ) ) ;
#634 = B_SPLINE_CURVE_WITH_KNOTS ( 'NONE', 3,
 ( #30232, #48312, #32606, #86869, #60608, #52525 ),
 .UNSPECIFIED., .F., .F.,
 ( 4, 2, 4 ),
 ( 0.0003203576572402824438, 0.0005551992086451969666, 0.0007900407600501114895 ),
 .UNSPECIFIED. ) ;
#635 = CARTESIAN_POINT ( 'NONE',  ( 57.73936995728981714, 194.9548013555410080, -4.594050593750042211 ) ) ;
#636 = CARTESIAN_POINT ( 'NONE',  ( 85.65412827366334625, 48.89905674914069067, -12.59087409094112253 ) ) ;
#637 = ORIENTED_EDGE ( 'NONE', *, *, #87810, .T. ) ;
#638 = DIRECTION ( 'NONE',  ( -0.2347357813929480952, 0.4065742997269687908, 0.8829475928589233247 ) ) ;
#639 = PLANE ( 'NONE',  #90141 ) ;
#640 = CARTESIAN_POINT ( 'NONE',  ( 21.31191609055706593, 183.1115022471902591, 10.00000000000009592 ) ) ;
#641 = CARTESIAN_POINT ( 'NONE',  ( 174.4676371989123140, 262.1820789082375995, 14.34376349448554144 ) ) ;
#642 = DIRECTION ( 'NONE',  ( -0.000000000000000000, 0.000000000000000000, 1.000000000000000000 ) ) ;
#643 = CARTESIAN_POINT ( 'NONE',  ( 154.9528145190857344, 262.2608478075840708, -17.26679351315302213 ) ) ;
#644 = CARTESIAN_POINT ( 'NONE',  ( 178.2689201652922861, 261.3463682195790625, 12.89043557696258979 ) ) ;
#645 = CARTESIAN_POINT ( 'NONE',  ( 100.3908607700756619, 238.7677522451419065, -5.000000000000047962 ) ) ;
#646 = CARTESIAN_POINT ( 'NONE',  ( 45.03145032967896100, 28.12755873383629890, -6.180339887498949025 ) ) ;
#647 = ORIENTED_EDGE ( 'NONE', *, *, #96875, .T. ) ;
#648 = CARTESIAN_POINT ( 'NONE',  ( 202.6070187115982719, 279.7213449518906145, 15.56322169823762280 ) ) ;
#649 = CARTESIAN_POINT ( 'NONE',  ( 88.00349997577261263, 44.64923112938743088, 4.253506518527973235 ) ) ;
#650 = CARTESIAN_POINT ( 'NONE',  ( 29.48529115882250551, 178.6423013555409796, -4.594050593750043987 ) ) ;
#651 = CARTESIAN_POINT ( 'NONE',  ( 10.05297690690921897, 28.73705186507752529, -3.090169943749475845 ) ) ;
#652 = DIRECTION ( 'NONE',  ( 0.000000000000000000, 0.000000000000000000, 1.000000000000000000 ) ) ;
#653 = CARTESIAN_POINT ( 'NONE',  ( 71.82703346931063493, 59.57451500028311386, -15.72875088550162914 ) ) ;
#654 = DIRECTION ( 'NONE',  ( 0.3074612162317589825, -0.9515606131578205895, 0.000000000000000000 ) ) ;
#656 = CARTESIAN_POINT ( 'NONE',  ( 67.50895872190925218, 209.7833772461660544, -9.188101187500095079 ) ) ;
#655 = CARTESIAN_POINT ( 'NONE',  ( 174.4019427205360842, 268.6781143085732992, 17.66204038257215458 ) ) ;
#657 = CARTESIAN_POINT ( 'NONE',  ( 164.4817765375028102, 245.7562014482918755, -6.334578229142199035 ) ) ;
#658 = CARTESIAN_POINT ( 'NONE',  ( 73.05975105895772970, 57.25024586824646633, 15.90232548103993615 ) ) ;
#659 = CARTESIAN_POINT ( 'NONE',  ( 45.37789370152431445, 208.5530062829863027, -4.648177544792955347E-16 ) ) ;
#660 = CARTESIAN_POINT ( 'NONE',  ( 10.55946980724658069, 24.83478043621386888, -8.090169943749479842 ) ) ;
#661 = ORIENTED_EDGE ( 'NONE', *, *, #87113, .F. ) ;
#662 = AXIS2_PLACEMENT_3D ( 'NONE', #54067, #69781, #39856 ) ;
#663 = CARTESIAN_POINT ( 'NONE',  ( 164.0312634879877294, 268.4089602666911105, 16.55773273759760400 ) ) ;
#664 = CARTESIAN_POINT ( 'NONE',  ( 22.68312297988236992, 197.2365022471903444, 2.944929066748280225E-16 ) ) ;
#665 = CARTESIAN_POINT ( 'NONE',  ( 163.1008115941903895, 248.1481028935802442, 11.25332017433677834 ) ) ;
#666 = CARTESIAN_POINT ( 'NONE',  ( -4.614459115189767147, 158.9548013555409796, -4.594050593750042211 ) ) ;
#667 = CARTESIAN_POINT ( 'NONE',  ( 31.05045217176252237, 26.43085787977764767, -9.188101187500008038 ) ) ;
#669 = CARTESIAN_POINT ( 'NONE',  ( 170.1430290936755227, 263.5485301713791841, 15.83574950237116141 ) ) ;
#668 = CARTESIAN_POINT ( 'NONE',  ( 164.4039089034689027, 259.8557547647841943, -16.35869283172417710 ) ) ;
#670 = EDGE_CURVE ( 'NONE', #48310, #39764, #20859, .T. ) ;
#671 = CARTESIAN_POINT ( 'NONE',  ( 185.5569508314414406, 260.4628387231232409, 6.337775543338724837 ) ) ;
#672 = CARTESIAN_POINT ( 'NONE',  ( 206.0691053506789387, 273.7248349927971844, 11.70564474658248422 ) ) ;
#673 = VECTOR ( 'NONE', #77839, 1000.000000000000227 ) ;
#674 = CARTESIAN_POINT ( 'NONE',  ( 183.8314122675164981, 256.5947891462430448, -1.876126292579811894 ) ) ;
#675 = CARTESIAN_POINT ( 'NONE',  ( 66.15645594251088824, 68.58591844969842555, 2.277906049505277863 ) ) ;
#676 = ORIENTED_EDGE ( 'NONE', *, *, #27395, .T. ) ;
#677 = CARTESIAN_POINT ( 'NONE',  ( 135.2899281637556896, 260.4637435831425023, 2.679491924311251605 ) ) ;
#678 =( LENGTH_UNIT ( ) NAMED_UNIT ( * ) SI_UNIT ( .MILLI., .METRE. ) );
#679 = CARTESIAN_POINT ( 'NONE',  ( 181.7952694153465245, 287.8449457046345970, 13.56394578825295305 ) ) ;
#680 = CARTESIAN_POINT ( 'NONE',  ( 196.2127072044743272, 290.0836373517121274, 16.37479000986071398 ) ) ;
#681 = CARTESIAN_POINT ( 'NONE',  ( 12.59929316974766955, 12.98920272979924739, 7.433330006724137462 ) ) ;
#682 = ORIENTED_EDGE ( 'NONE', *, *, #27159, .T. ) ;
#683 = CARTESIAN_POINT ( 'NONE',  ( 160.3856437025401931, 252.8509116329982191, 16.19741910828728493 ) ) ;
#684 = CARTESIAN_POINT ( 'NONE',  ( 157.3029956111992362, 258.1902147490555421, -18.22269824972649843 ) ) ;
#685 = CARTESIAN_POINT ( 'NONE',  ( 28.31825578742223115, 28.30066082961423390, -10.00000000000000533 ) ) ;
#686 = CARTESIAN_POINT ( 'NONE',  ( 207.6477529416552557, 270.9905371579805546, 7.447146952410988341 ) ) ;
#687 = CARTESIAN_POINT ( 'NONE',  ( 185.2057911854575138, 276.7165103822673586, 17.80337911918299909 ) ) ;
#688 = CARTESIAN_POINT ( 'NONE',  ( 163.0056347026689707, 248.3129541054019569, -11.27842346302751508 ) ) ;
#689 = CARTESIAN_POINT ( 'NONE',  ( 153.0444155045374544, 265.5662918618958201, -16.15173036748435109 ) ) ;
#690 = VERTEX_POINT ( 'NONE', #63350 ) ;
#691 = CARTESIAN_POINT ( 'NONE',  ( 190.8932553518572206, 280.9403775647153338, 16.64665765453319679 ) ) ;
#692 = FACE_OUTER_BOUND ( 'NONE', #1772, .T. ) ;
#693 = ORIENTED_EDGE ( 'NONE', *, *, #11844, .T. ) ;
#694 = CARTESIAN_POINT ( 'NONE',  ( 48.58805178314242568, 84.67719436603331928, 10.00000000000000000 ) ) ;
#695 = DIRECTION ( 'NONE',  ( 0.000000000000000000, 0.000000000000000000, 1.000000000000000000 ) ) ;
#696 = ORIENTED_EDGE ( 'NONE', *, *, #30280, .F. ) ;
#697 = CARTESIAN_POINT ( 'NONE',  ( -74.97640825042664403, 52.25402898078436920, -10.00000000000000000 ) ) ;
#698 = CARTESIAN_POINT ( 'NONE',  ( 79.11723855630624769, 59.11194703662723526, -16.21433712332713739 ) ) ;
#699 = CARTESIAN_POINT ( 'NONE',  ( 149.7072529793668707, 271.3464269086063041, -11.98883662638834657 ) ) ;
#700 = CARTESIAN_POINT ( 'NONE',  ( 69.78994883848024244, 62.55969527080727488, 13.43020027970054819 ) ) ;
#701 = ORIENTED_EDGE ( 'NONE', *, *, #49835, .T. ) ;
#702 = CARTESIAN_POINT ( 'NONE',  ( 200.6129772034685175, 283.1751261563724142, 18.36811917402039640 ) ) ;
#703 = DIRECTION ( 'NONE',  ( 0.000000000000000000, 0.000000000000000000, 1.000000000000000000 ) ) ;
#704 = CARTESIAN_POINT ( 'NONE',  ( 151.2591548104722108, 274.8925958778597192, -8.633445779095369588 ) ) ;
#705 = VERTEX_POINT ( 'NONE', #23335 ) ;
#706 = ORIENTED_EDGE ( 'NONE', *, *, #49315, .T. ) ;
#707 = ORIENTED_EDGE ( 'NONE', *, *, #77798, .F. ) ;
#708 = CARTESIAN_POINT ( 'NONE',  ( 73.41033574890859370, 61.45318865418844467, 14.95304618059455670 ) ) ;
#709 = VERTEX_POINT ( 'NONE', #54730 ) ;
#710 = DIRECTION ( 'NONE',  ( -0.6141984594095433181, -0.7891516029629183082, 0.000000000000000000 ) ) ;
#711 = ORIENTED_EDGE ( 'NONE', *, *, #24354, .F. ) ;
#712 = CARTESIAN_POINT ( 'NONE',  ( 207.5215400641004351, 271.2091442744748520, 2.886080616848571534 ) ) ;
#713 = CARTESIAN_POINT ( 'NONE',  ( 198.7045056313791633, 284.4806958840320021, 17.79791830837532274 ) ) ;
#714 = CARTESIAN_POINT ( 'NONE',  ( -19.65312891409030271, 93.06504152958497400, -55.00000000000000000 ) ) ;
#715 = CARTESIAN_POINT ( 'NONE',  ( 148.3025927079438304, 273.7793698660844939, -8.046026357031887954 ) ) ;
#716 = CARTESIAN_POINT ( 'NONE',  ( 175.1828650004762267, 290.0278138422783627, 6.199890812727518075 ) ) ;
#717 = DIRECTION ( 'NONE',  ( 1.000000000000000000, -2.577303450022684150E-15, 0.000000000000000000 ) ) ;
#718 = CARTESIAN_POINT ( 'NONE',  ( 73.00396795756827828, 57.62093675928252878, -16.32480838619500219 ) ) ;
#719 = CARTESIAN_POINT ( 'NONE',  ( 15.13723537722347778, 17.24335787977762280, -9.188101187500008038 ) ) ;
#720 = EDGE_CURVE ( 'NONE', #17180, #93223, #32942, .T. ) ;
#721 = CARTESIAN_POINT ( 'NONE',  ( 198.3666213183647926, 277.3917214242281375, -15.34159264812408452 ) ) ;
#722 = CARTESIAN_POINT ( 'NONE',  ( 68.45344762042827824, 64.57392882346940155, 12.12708197196866600 ) ) ;
#724 = ORIENTED_EDGE ( 'NONE', *, *, #71091, .F. ) ;
#723 = CARTESIAN_POINT ( 'NONE',  ( 193.0512205562391159, 275.6825563886401369, -16.88465587640301280 ) ) ;
#725 = CARTESIAN_POINT ( 'NONE',  ( 191.1159732739488106, 299.6244194819818745, 5.816361631709846769 ) ) ;
#726 = CARTESIAN_POINT ( 'NONE',  ( -72.48190909937208914, 49.06123820388767598, -10.00000000000000000 ) ) ;
#727 = CARTESIAN_POINT ( 'NONE',  ( 159.4491226731523454, 254.4730136382542582, -15.39140229921534520 ) ) ;
#728 = DIRECTION ( 'NONE',  ( -0.000000000000000000, -0.000000000000000000, -1.000000000000000000 ) ) ;
#729 = CARTESIAN_POINT ( 'NONE',  ( 82.52967124556970191, 45.91001068904856197, -10.98309457076566886 ) ) ;
#730 = CIRCLE ( 'NONE', #57349, 1.449999999999993072 ) ;
#731 = ADVANCED_FACE ( 'NONE', ( #78063 ), #54223, .F. ) ;
#732 = CARTESIAN_POINT ( 'NONE',  ( 200.4116241316243645, 283.5238799070667142, 18.37703770054986663 ) ) ;
#733 = DIRECTION ( 'NONE',  ( -0.8660254037844377084, -0.5000000000000014433, -0.000000000000000000 ) ) ;
#734 = VERTEX_POINT ( 'NONE', #24355 ) ;
#735 = CARTESIAN_POINT ( 'NONE',  ( 193.8687075137383999, 294.8565439189318340, -14.51137100490168486 ) ) ;
#737 = EDGE_CURVE ( 'NONE', #53287, #48247, #79529, .T. ) ;
#736 = LINE ( 'NONE', #24036, #27376 ) ;
#738 = CARTESIAN_POINT ( 'NONE',  ( 15.88121511744428282, 166.6427522451417644, 1.119607411625061291E-15 ) ) ;
#739 = CARTESIAN_POINT ( 'NONE',  ( 85.91165145656357538, 232.6589784336661353, -6.496448406907676862E-16 ) ) ;
#740 = CARTESIAN_POINT ( 'NONE',  ( 82.39535249337586720, 40.37214158351728344, -0.8705103534316617209 ) ) ;
#741 = CYLINDRICAL_SURFACE ( 'NONE', #85952, 17.82106496071139645 ) ;
#742 = CARTESIAN_POINT ( 'NONE',  ( 166.9577072416738019, 278.1838835069849551, -13.42963054343457863 ) ) ;
#743 = CARTESIAN_POINT ( 'NONE',  ( 72.53309028193872621, 70.86290320417140265, 7.626211012637800657 ) ) ;
#745 = CARTESIAN_POINT ( 'NONE',  ( 75.62238463899576857, 65.35737373615053514, 14.30258955018443956 ) ) ;
#744 = CARTESIAN_POINT ( 'NONE',  ( 9.079046938504149011, 185.2369531367911293, -4.594050593750048428 ) ) ;
#746 = CARTESIAN_POINT ( 'NONE',  ( 161.4025183475459073, 251.0896330829197041, 14.50747140106038735 ) ) ;
#747 = ORIENTED_EDGE ( 'NONE', *, *, #72238, .F. ) ;
#749 = VERTEX_POINT ( 'NONE', #78569 ) ;
#748 = UNCERTAINTY_MEASURE_WITH_UNIT (LENGTH_MEASURE( 1.000000000000000082E-05 ), #95770, 'distance_accuracy_value', 'NONE');
#750 = CARTESIAN_POINT ( 'NONE',  ( -17.69472717286124208, 126.6729902121449811, 2.598076211353400389 ) ) ;
#751 = CARTESIAN_POINT ( 'NONE',  ( 197.6375537770108792, 265.0377995068387804, -2.979366280021975122 ) ) ;
#752 = CARTESIAN_POINT ( 'NONE',  ( 85.52120238093419857, 46.04363271907506316, -9.405378037663709279 ) ) ;
#753 = CARTESIAN_POINT ( 'NONE',  ( 202.6448056009234904, 279.6558961397194594, -17.13147024041661126 ) ) ;
#754 =( BOUNDED_CURVE ( )  B_SPLINE_CURVE ( 2, ( #51590, #82036, #12612, #50581, #74420, #81531, #96236, #65295, #83027 ),
 .UNSPECIFIED., .F., .T. ) 
 B_SPLINE_CURVE_WITH_KNOTS ( ( 3, 2, 2, 2, 3 ),
 ( 0.3266129032258064391, 0.3279569892473118142, 0.3306451612903225645, 0.3333333333333333148, 0.3346774193548386900 ),
 .UNSPECIFIED. ) 
 CURVE ( )  GEOMETRIC_REPRESENTATION_ITEM ( )  RATIONAL_B_SPLINE_CURVE ( ( 0.9330127018922194093, 0.9330127018922194093, 1.000000000000000000, 0.8660254037844387076, 1.000000000000000000, 0.8660254037844387076, 1.000000000000000000, 0.9330127018922194093, 0.9330127018922194093 ) ) 
 REPRESENTATION_ITEM ( '' )  );
#755 = CARTESIAN_POINT ( 'NONE',  ( 113.3812418268423414, 226.2677522451417929, -5.000000000000041744 ) ) ;
#756 = CARTESIAN_POINT ( 'NONE',  ( 74.45862791283336435, 68.29041308412308808, -11.43317454991487914 ) ) ;
#757 = CARTESIAN_POINT ( 'NONE',  ( 24.36989474801440636, 191.0024278399161233, 9.188101187500095079 ) ) ;
#758 = CARTESIAN_POINT ( 'NONE',  ( 197.6585140451727511, 276.4987611936116423, 15.20518655683599896 ) ) ;
#759 = VERTEX_POINT ( 'NONE', #25344 ) ;
#760 = CARTESIAN_POINT ( 'NONE',  ( -14.53296615039140960, 35.34728565592875071, 59.99999999999999289 ) ) ;
#761 = CARTESIAN_POINT ( 'NONE',  ( 182.6096789788834087, 260.7894769810658318, -10.76918927552311622 ) ) ;
#762 = CARTESIAN_POINT ( 'NONE',  ( 30.11635425815369871, 39.16126292948897714, -6.180339887498951690 ) ) ;
#763 = CARTESIAN_POINT ( 'NONE',  ( 80.25178558894602077, 57.14685393251872370, -16.23521980932009612 ) ) ;
#764 = LINE ( 'NONE', #54961, #11155 ) ;
#765 = CARTESIAN_POINT ( 'NONE',  ( 59.77787777531585789, 211.9865022471903160, 10.00000000000009415 ) ) ;
#766 = CARTESIAN_POINT ( 'NONE',  ( 186.1370921618058674, 283.3846817430978149, 17.26256540491417368 ) ) ;
#767 = CARTESIAN_POINT ( 'NONE',  ( 194.2389208611690492, 294.2153155915419802, -15.75132567904764791 ) ) ;
#768 = ADVANCED_FACE ( 'NONE', ( #79091 ), #73419, .T. ) ;
#769 = CARTESIAN_POINT ( 'NONE',  ( 192.5078993207126814, 265.1470235889372589, 7.748826881858292381 ) ) ;
#770 = CARTESIAN_POINT ( 'NONE',  ( 168.9579038699606315, 279.3139280689009070, 15.08363371378442608 ) ) ;
#771 = LINE ( 'NONE', #16967, #7881 ) ;
#772 = CARTESIAN_POINT ( 'NONE',  ( 146.8859094598974480, 276.2331372299326517, -0.7994986043261681496 ) ) ;
#773 = CARTESIAN_POINT ( 'NONE',  ( 148.3997536239841679, 273.6110822229926498, 8.713694244701960301 ) ) ;
#774 = DIRECTION ( 'NONE',  ( 0.000000000000000000, -0.5247752241694974007, 0.8512408378936325848 ) ) ;
#775 = ORIENTED_EDGE ( 'NONE', *, *, #59166, .F. ) ;
#776 = CARTESIAN_POINT ( 'NONE',  ( 188.7267243920021542, 295.1910411013678299, 11.79826141631466463 ) ) ;
#777 = CARTESIAN_POINT ( 'NONE',  ( 9.548404355818409073, 182.9865022471903160, -10.00000000000009592 ) ) ;
#778 = CARTESIAN_POINT ( 'NONE',  ( 115.8441751185107478, 231.5643266524159856, 9.188101187500095079 ) ) ;
#779 = CARTESIAN_POINT ( 'NONE',  ( 10.91775413003093931, 21.70171378149917985, -9.188101187500004485 ) ) ;
#780 = CARTESIAN_POINT ( 'NONE',  ( -13.83428154636143503, 169.4865022471903160, -10.00000000000009592 ) ) ;
#781 = EDGE_CURVE ( 'NONE', #55876, #18677, #11467, .T. ) ;
#782 = FACE_OUTER_BOUND ( 'NONE', #41307, .T. ) ;
#784 = CARTESIAN_POINT ( 'NONE',  ( 195.1938325246360364, 279.1028983798199761, 16.30285934901647238 ) ) ;
#783 = CARTESIAN_POINT ( 'NONE',  ( 66.10780414051450293, 68.63670250712272036, 1.777645618418523865 ) ) ;
#785 = CARTESIAN_POINT ( 'NONE',  ( 150.4341052900205682, 270.0874817769553147, -15.18648472748443368 ) ) ;
#786 = CARTESIAN_POINT ( 'NONE',  ( 190.4856830296963039, 261.1280128588217622, -4.649057565560686278 ) ) ;
#787 = CARTESIAN_POINT ( 'NONE',  ( 149.8050492866161392, 271.5723974896224604, -11.69608657949948061 ) ) ;
#788 = CARTESIAN_POINT ( 'NONE',  ( 113.8864233123832577, 229.8927522451418213, 10.00000000000009948 ) ) ;
#789 = CARTESIAN_POINT ( 'NONE',  ( 132.0211419364472363, 235.4824982072973683, 3.021315404115420679E-15 ) ) ;
#790 = CARTESIAN_POINT ( 'NONE',  ( 85.94615330653621754, 47.59945275330427705, 10.87303975713271420 ) ) ;
#791 = ORIENTED_EDGE ( 'NONE', *, *, #48139, .T. ) ;
#792 = CARTESIAN_POINT ( 'NONE',  ( 192.9767279769529864, 266.9258724154651645, 11.43531444180136347 ) ) ;
#793 = CARTESIAN_POINT ( 'NONE',  ( 178.9040352719350722, 280.8175526911114162, 16.40818605171233813 ) ) ;
#794 = CARTESIAN_POINT ( 'NONE',  ( 199.8193483442802005, 270.0841922650383822, 9.248294916842718649 ) ) ;
#795 = EDGE_CURVE ( 'NONE', #82833, #80375, #31434, .T. ) ;
#796 = ADVANCED_FACE ( 'NONE', ( #63846 ), #32453, .F. ) ;
#797 = ORIENTED_EDGE ( 'NONE', *, *, #34932, .T. ) ;
#798 = CARTESIAN_POINT ( 'NONE',  ( 84.41462708798377435, 43.37824213815624574, 7.154511429969321767 ) ) ;
#799 =( GEOMETRIC_REPRESENTATION_CONTEXT ( 3 ) GLOBAL_UNCERTAINTY_ASSIGNED_CONTEXT ( ( #748 ) ) GLOBAL_UNIT_ASSIGNED_CONTEXT ( ( #95770, #27323, #35406 ) ) REPRESENTATION_CONTEXT ( 'NONE', 'WORKASPACE' ) );
#800 = CARTESIAN_POINT ( 'NONE',  ( 182.6461938784695747, 263.4785373306806378, -13.90739657620127190 ) ) ;
#801 = CARTESIAN_POINT ( 'NONE',  ( 72.40747426417379984, 71.81324781307232286, -5.589457107701495175 ) ) ;
#802 = CARTESIAN_POINT ( 'NONE',  ( 39.77289032284285497, 58.49985355908045648, -10.00000000000000000 ) ) ;
#803 = ORIENTED_EDGE ( 'NONE', *, *, #92983, .T. ) ;
#804 = CARTESIAN_POINT ( 'NONE',  ( 187.3992198486085385, 278.8856332353482230, 17.56695100383910102 ) ) ;
#805 = B_SPLINE_SURFACE_WITH_KNOTS ( 'NONE', 3, 1, ( 
 ( #39651, #16380 ),
 ( #76687, #85852 ),
 ( #46781, #683 ),
 ( #77179, #92421 ),
 ( #60970, #69577 ),
 ( #53858, #21983 ),
 ( #84821, #76212 ),
 ( #60465, #22971 ),
 ( #6788, #91420 ),
 ( #99503, #8286 ),
 ( #39152, #100002 ),
 ( #47271, #15359 ),
 ( #30586, #31068 ),
 ( #84329, #70065 ),
 ( #62455, #93422 ),
 ( #23973, #61959 ),
 ( #61473, #54353 ),
 ( #52877, #83828 ),
 ( #45764, #91930 ),
 ( #15871, #22485 ),
 ( #14875, #95446 ),
 ( #94418, #33589 ),
 ( #55848, #40665 ),
 ( #9805, #47760 ),
 ( #16875, #40161 ),
 ( #71602, #71103 ),
 ( #86843, #78699 ),
 ( #17899, #79233 ),
 ( #2698, #1701 ),
 ( #87852, #56868 ),
 ( #72610, #17378 ),
 ( #24971, #25997 ),
 ( #64485, #2198 ),
 ( #33081, #63481 ) ),
 .UNSPECIFIED., .T., .F., .F.,
 ( 4, 2, 2, 2, 2, 2, 2, 2, 2, 2, 2, 2, 2, 2, 2, 2, 4 ),
 ( 2, 2 ),
 ( 0.000000000000000000, 0.06250000000000000000, 0.1250000000000000000, 0.1875000000000000000, 0.2500000000000000000, 0.3125000000000000000, 0.3750000000000000000, 0.4375000000000000000, 0.5000000000000000000, 0.5625000000000000000, 0.6250000000000000000, 0.6875000000000000000, 0.7500000000000000000, 0.8125000000000000000, 0.8750000000000000000, 0.9375000000000000000, 1.000000000000000000 ),
 ( 0.000000000000000000, 1.000000000000000000 ),
 .UNSPECIFIED. ) ;
#806 = CARTESIAN_POINT ( 'NONE',  ( 41.82943821127123840, 26.01110640527295814, 2.839279412974134775 ) ) ;
#807 = ORIENTED_EDGE ( 'NONE', *, *, #26966, .F. ) ;
#808 = B_SPLINE_CURVE_WITH_KNOTS ( 'NONE', 3,
 ( #93246, #8616, #85674, #37500, #16211, #70408, #16709, #68407, #29915, #60785, #91750, #22313, #53216, #84167, #2530, #71426, #19242, #65308, #78530, #33412, #95269, #18222, #32901, #2016, #17202, #49603, #70927, #56193, #64818, #94250, #49116, #80053, #3531, #94743, #1532, #48624, #10620, #55682, #86669, #41498, #42006, #32413, #63308, #72439, #3045, #48104, #26320, #34408, #79047, #57194 ),
 .UNSPECIFIED., .F., .F.,
 ( 4, 2, 2, 2, 2, 2, 2, 2, 2, 2, 2, 2, 2, 2, 2, 2, 2, 2, 2, 2, 2, 2, 2, 2, 4 ),
 ( 0.0001456936475078258835, 0.001156712366743216369, 0.001662221726360948787, 0.001788599066265381945, 0.001914976406169814887, 0.002041353746074247612, 0.002167731085978680770, 0.002420485765787583950, 0.002673240445596487564, 0.003178749805214391069, 0.004189768524450103969, 0.005200787243685817303, 0.005706296603303709532, 0.005959051283112655646, 0.006211805962921601761, 0.006274994632873879055, 0.006338183302826156350, 0.006401371972778433644, 0.006464560642730710939, 0.006717315322539938946, 0.007222824682158399297, 0.007475579361967629038, 0.007728334041776859648, 0.007981088721586090257, 0.008233843401395319131 ),
 .UNSPECIFIED. ) ;
#809 = CARTESIAN_POINT ( 'NONE',  ( 79.99999999999998579, 20.00000000000000000, 2.622423327744102917 ) ) ;
#810 = CARTESIAN_POINT ( 'NONE',  ( 147.8819534105757043, 274.5079385007862811, -9.338341377131436971 ) ) ;
#811 = CARTESIAN_POINT ( 'NONE',  ( 156.7854950622006527, 259.0865519928661911, 18.17819951099994213 ) ) ;
#813 = EDGE_LOOP ( 'NONE', ( #50961, #70079, #41428, #11684 ) ) ;
#812 = CIRCLE ( 'NONE', #62261, 70.00000000000001421 ) ;
#814 = CARTESIAN_POINT ( 'NONE',  ( 86.28449982416978514, 46.95005333036156969, -10.54182221192813884 ) ) ;
#815 = CARTESIAN_POINT ( 'NONE',  ( 205.9381235462180655, 273.9517021329910449, 12.32333910181129788 ) ) ;
#816 = B_SPLINE_CURVE_WITH_KNOTS ( 'NONE', 3,
 ( #20818, #38347, #96847, #7455, #100186, #69257, #36485, #58292, #57789, #43591, #88767, #82657, #28907, #43073, #13216, #19337 ),
 .UNSPECIFIED., .F., .F.,
 ( 4, 1, 2, 2, 2, 1, 2, 2, 4 ),
 ( 0.000000000000000000, 0.1249999999999972522, 0.1874999999999962530, 0.2499999999999952816, 0.4999999999999940048, 0.6249999999999944489, 0.6874999999999946709, 0.7499999999999947820, 1.000000000000000000 ),
 .UNSPECIFIED. ) ;
#817 = CARTESIAN_POINT ( 'NONE',  ( -22.42236680055709641, 157.8615022471902591, 0.000000000000000000 ) ) ;
#818 = B_SPLINE_CURVE_WITH_KNOTS ( 'NONE', 3,
 ( #71729, #81351, #33203, #2834, #64103, #49904, #57488, #95053, #56499, #27618, #95568, #64613, #80862, #4294, #35196, #25614, #18022, #66102, #26113, #40781, #56991, #58484, #89460, #87973, #20015, #49403, #19032, #80351, #10921, #3332, #34210, #42288, #51391, #53382, #51903, #75711, #21021, #58967, #98011, #29109, #45282, #82844, #89937, #83331, #99507, #66599, #13415, #74728, #12417, #5793, #44284, #52388, #6792, #43284 ),
 .UNSPECIFIED., .F., .F.,
 ( 4, 2, 2, 2, 2, 2, 2, 2, 2, 2, 2, 2, 2, 2, 2, 2, 2, 2, 2, 2, 2, 2, 2, 2, 2, 2, 4 ),
 ( 0.0007884837803721018784, 0.0009911425274972654638, 0.001092471901059910953, 0.001193801274622556009, 0.001295130648185201499, 0.001396460021747846555, 0.001599118768873064025, 0.002004436263123498315, 0.002409753757373932822, 0.003220388745874802703, 0.004031023734375672150, 0.004841658722876542899, 0.005246976217126939242, 0.005449634964252138281, 0.005550964337814701804, 0.005601629024595986168, 0.005652293711377270533, 0.005702958398158554897, 0.005753623084939839261, 0.005854952458502437479, 0.006057611205627632181, 0.006260269952752827750, 0.006462928699878023320, 0.006665587447003218889, 0.006868246194128413591, 0.007070904941253609161, 0.007273563688378803863 ),
 .UNSPECIFIED. ) ;
#819 = CARTESIAN_POINT ( 'NONE',  ( 18.33840876668534037, 32.36126292948895866, 6.180339887498949913 ) ) ;
#820 = CARTESIAN_POINT ( 'NONE',  ( 18.86034532297697908, 34.61239144260639478, -10.00000000000000000 ) ) ;
#821 = CARTESIAN_POINT ( 'NONE',  ( 121.6288370910339864, 229.4824982072973398, 3.021315404115420679E-15 ) ) ;
#822 = CARTESIAN_POINT ( 'NONE',  ( 81.63517289312954972, 55.69097578121159131, -16.34528168754146904 ) ) ;
#823 = ORIENTED_EDGE ( 'NONE', *, *, #34079, .T. ) ;
#824 = ORIENTED_EDGE ( 'NONE', *, *, #18196, .F. ) ;
#825 = CARTESIAN_POINT ( 'NONE',  ( 175.1988826894065312, 258.4881829066944192, 12.95490576022639928 ) ) ;
#826 = VERTEX_POINT ( 'NONE', #48664 ) ;
#827 = CARTESIAN_POINT ( 'NONE',  ( 77.13172709529845861, 49.47536214534034826, -14.94599358421776358 ) ) ;
#828 = ORIENTED_EDGE ( 'NONE', *, *, #42263, .F. ) ;
#829 = CARTESIAN_POINT ( 'NONE',  ( 169.4845393771928173, 269.1455624229661225, 17.04989631985375453 ) ) ;
#830 = LINE ( 'NONE', #47917, #18689 ) ;
#831 = DIRECTION ( 'NONE',  ( -0.8660254037844378194, -0.5000000000000014433, -0.000000000000000000 ) ) ;
#832 = CARTESIAN_POINT ( 'NONE',  ( 36.01802474176511026, 21.76426979415091978, 3.090169943749476733 ) ) ;
#833 = CARTESIAN_POINT ( 'NONE',  ( 71.17767548612019368, 71.91738291818995776, 3.016136621268855844 ) ) ;
#834 = CARTESIAN_POINT ( 'NONE',  ( 190.0226014859668453, 301.5181949703289774, 3.835066345245774500 ) ) ;
#835 = CARTESIAN_POINT ( 'NONE',  ( 195.0987748510856647, 262.8777892843546056, 0.5876111608821336096 ) ) ;
#836 = CARTESIAN_POINT ( 'NONE',  ( 171.4762298308916968, 250.4071321773194256, -5.778962900379556622 ) ) ;
#837 = CARTESIAN_POINT ( 'NONE',  ( 44.24123536260515976, 207.8967562850346837, -4.648177544792955347E-16 ) ) ;
#838 = CARTESIAN_POINT ( 'NONE',  ( 202.6998011068605194, 275.8073517492424571, -14.46034972092035531 ) ) ;
#839 = CARTESIAN_POINT ( 'NONE',  ( 127.4544149619371609, 235.2048013555409796, 4.594050593750051981 ) ) ;
#840 = CARTESIAN_POINT ( 'NONE',  ( 70.47294781783818962, 60.89548864084860469, -14.98891872237399348 ) ) ;
#841 = CARTESIAN_POINT ( 'NONE',  ( 42.37730965384162829, 25.26216523072498532, -2.296566073217252530E-15 ) ) ;
#842 = ORIENTED_EDGE ( 'NONE', *, *, #99346, .F. ) ;
#844 = ADVANCED_FACE ( 'NONE', ( #61833 ), #9674, .T. ) ;
#843 = VECTOR ( 'NONE', #25615, 1000.000000000000000 ) ;
#846 = ORIENTED_EDGE ( 'NONE', *, *, #5709, .T. ) ;
#845 = CARTESIAN_POINT ( 'NONE',  ( 20.28716687417668751, 35.21091486745861232, 7.012934429366973338E-14 ) ) ;
#847 = CARTESIAN_POINT ( 'NONE',  ( 203.6154480045567254, 276.2142138887539886, 13.33356564682453893 ) ) ;
#848 = CARTESIAN_POINT ( 'NONE',  ( 177.5663600863603904, 253.5925114390991553, 1.368723437027021594 ) ) ;
#849 = EDGE_CURVE ( 'NONE', #75378, #62754, #4045, .T. ) ;
#850 = CARTESIAN_POINT ( 'NONE',  ( 165.4781454232152953, 246.0304399151612245, -2.837517270351797016 ) ) ;
#851 = DIRECTION ( 'NONE',  ( -0.8660254037844359321, -0.5000000000000051070, -0.000000000000000000 ) ) ;
#852 = CARTESIAN_POINT ( 'NONE',  ( 71.63285926872011089, 60.29674625202430605, 14.96834098354499965 ) ) ;
#853 = CARTESIAN_POINT ( 'NONE',  ( 153.2283961777204695, 265.2476279883323400, -17.66880461074566000 ) ) ;
#854 = CARTESIAN_POINT ( 'NONE',  ( 174.2107584283791937, 288.2982359596526294, -10.05413864759180775 ) ) ;
#855 = CARTESIAN_POINT ( 'NONE',  ( 173.2798715285074991, 281.8114527337138497, 15.08241540710736750 ) ) ;
#856 = CARTESIAN_POINT ( 'NONE',  ( 76.73342198214220389, 54.11205231684652972, -16.50410611215824375 ) ) ;
#857 = ORIENTED_EDGE ( 'NONE', *, *, #39122, .T. ) ;
#859 = CARTESIAN_POINT ( 'NONE',  ( 194.9385458806846430, 293.0035295114944347, -15.70518692812489192 ) ) ;
#858 = B_SPLINE_CURVE_WITH_KNOTS ( 'NONE', 3,
 ( #9139, #88196, #40012, #86692 ),
 .UNSPECIFIED., .F., .F.,
 ( 4, 4 ),
 ( 0.01500120671162206987, 0.02374886763876108906 ),
 .UNSPECIFIED. ) ;
#860 = CARTESIAN_POINT ( 'NONE',  ( 152.7606255379852485, 273.9024957846719417, 12.20944343624798201 ) ) ;
#861 = VERTEX_POINT ( 'NONE', #26360 ) ;
#863 = EDGE_CURVE ( 'NONE', #22269, #42801, #98193, .T. ) ;
#862 = CARTESIAN_POINT ( 'NONE',  ( 190.7462944391682527, 267.5255109591399787, -12.03952247946680565 ) ) ;
#864 = CARTESIAN_POINT ( 'NONE',  ( 159.4675140783279801, 279.0638630585228270, 10.93816975955046544 ) ) ;
#865 = CARTESIAN_POINT ( 'NONE',  ( 194.1886218511698985, 264.4780071475063892, 4.425547236910387205 ) ) ;
#866 = CYLINDRICAL_SURFACE ( 'NONE', #55855, 10.00000000000001066 ) ;
#867 = CARTESIAN_POINT ( 'NONE',  ( 6.290725127440143893, 185.9860189848785126, -2.679491924311252493 ) ) ;
#869 = CARTESIAN_POINT ( 'NONE',  ( 160.8351940225509793, 281.7148115565385638, 6.356997412616704146 ) ) ;
#868 = CARTESIAN_POINT ( 'NONE',  ( 164.7214155129279902, 283.9927988242368428, -6.830869372685311802 ) ) ;
#870 = CARTESIAN_POINT ( 'NONE',  ( 200.6680263064462792, 283.0797783131037022, -17.21821073473145347 ) ) ;
#871 = ORIENTED_EDGE ( 'NONE', *, *, #19349, .T. ) ;
#872 = CARTESIAN_POINT ( 'NONE',  ( 204.7752845747214110, 272.8046689790122628, -9.561809439462201965 ) ) ;
#873 = CARTESIAN_POINT ( 'NONE',  ( 190.3857086002435324, 265.7052621535535195, -12.18680232436801170 ) ) ;
#874 = CARTESIAN_POINT ( 'NONE',  ( 188.8588437571793008, 263.8686956098205769, -9.115312588253704718 ) ) ;
#875 = CARTESIAN_POINT ( 'NONE',  ( 191.8098186646358272, 275.3759357196170185, -15.83273902380079257 ) ) ;
#876 = CARTESIAN_POINT ( 'NONE',  ( 33.29424590502123493, 178.4824982072973683, 3.021315404115420679E-15 ) ) ;
#877 = ADVANCED_FACE ( 'NONE', ( #35443 ), #33453, .F. ) ;
#878 = CARTESIAN_POINT ( 'NONE',  ( 184.9851449735395192, 296.8426758125457354, -4.344182660386399775 ) ) ;
#879 = EDGE_CURVE ( 'NONE', #47755, #61485, #20257, .T. ) ;
#880 = VECTOR ( 'NONE', #94818, 999.9999999999998863 ) ;
#881 = CARTESIAN_POINT ( 'NONE',  ( 153.1745822862813498, 265.3408363824576668, 16.18092354043443493 ) ) ;
#882 = FACE_OUTER_BOUND ( 'NONE', #77373, .T. ) ;
#883 = CARTESIAN_POINT ( 'NONE',  ( 73.85662887421025857, 68.53912330967601463, 10.89787362795912884 ) ) ;
#884 = CARTESIAN_POINT ( 'NONE',  ( 34.75566377745538205, 179.3262482093457493, 3.021315404115420679E-15 ) ) ;
#885 = CARTESIAN_POINT ( 'NONE',  ( -2.801305199957352166, 163.0643266524160140, -9.188101187500093303 ) ) ;
#886 = CARTESIAN_POINT ( 'NONE',  ( 88.99704050542813150, 228.3149278399160664, 9.188101187500093303 ) ) ;
#887 = DIRECTION ( 'NONE',  ( 0.6123724356958057946, 0.3535533905932591314, 0.7071067811865451302 ) ) ;
#888 = CARTESIAN_POINT ( 'NONE',  ( 147.2567621633200474, 275.5908015054806128, -3.647191014543873955 ) ) ;
#889 = CARTESIAN_POINT ( 'NONE',  ( 187.7710022618638277, 277.0665775429750397, -17.72351784843695555 ) ) ;
#890 = AXIS2_PLACEMENT_3D ( 'NONE', #4675, #42163, #35566 ) ;
#891 = DIRECTION ( 'NONE',  ( 0.5000000000000014433, -0.8660254037844379305, 0.000000000000000000 ) ) ;
#892 = CARTESIAN_POINT ( 'NONE',  ( 78.12422403393351544, 55.30668070268215075, 16.12263249026505108 ) ) ;
#893 =( NAMED_UNIT ( * ) PLANE_ANGLE_UNIT ( ) SI_UNIT ( $, .RADIAN. ) );
#894 = CARTESIAN_POINT ( 'NONE',  ( 158.3585752585947262, 263.3710999200782226, 17.79390465796247156 ) ) ;
#897 = CARTESIAN_POINT ( 'NONE',  ( 76.39060622948801438, 51.12702130622679420, 16.04935315526039474 ) ) ;
#896 = B_SPLINE_CURVE_WITH_KNOTS ( 'NONE', 3,
 ( #59007, #89974, #13454, #81389, #49945, #20554, #82879, #57531, #35237, #51432, #12964, #43825, #5343, #36224, #19070, #67128, #59512, #90490, #21063, #37224, #7320, #38712, #91978, #13933, #99050, #14437, #61996, #23008, #75749, #53903, #38199, #68619, #99542, #68122, #14914, #21539, #36721, #5831, #45318, #45802, #69118, #100045, #76726, #23501, #52422, #69618 ),
 .UNSPECIFIED., .F., .F.,
 ( 4, 1, 2, 2, 1, 2, 2, 1, 1, 2, 2, 1, 1, 2, 2, 1, 1, 2, 2, 1, 1, 1, 2, 2, 1, 1, 1, 2, 2, 4 ),
 ( 0.000000000000000000, 0.06249999999999382438, 0.09374999999999200639, 0.1249999999999902023, 0.1874999999999839295, 0.2187499999999821532, 0.2499999999999804046, 0.3124999999999763522, 0.3437499999999758526, 0.3593749999999756306, 0.3749999999999754086, 0.4374999999999745759, 0.4687499999999757971, 0.4843749999999780731, 0.4999999999999803491, 0.5624999999999793499, 0.5937499999999791278, 0.6093749999999773515, 0.6249999999999755751, 0.6874999999999715783, 0.7187499999999709122, 0.7343749999999705791, 0.7421874999999703570, 0.7499999999999701350, 0.8124999999999732436, 0.8437499999999734657, 0.8593749999999736877, 0.8671874999999749090, 0.8749999999999761302, 1.000000000000000000 ),
 .UNSPECIFIED. ) ;
#895 = DIRECTION ( 'NONE',  ( 1.000000000000000000, 0.000000000000000000, 0.000000000000000000 ) ) ;
#898 = CARTESIAN_POINT ( 'NONE',  ( 161.8357418099448353, 250.3392680350139869, 14.17480975207680061 ) ) ;
#899 = EDGE_CURVE ( 'NONE', #47394, #59009, #20762, .T. ) ;
#900 = CARTESIAN_POINT ( 'NONE',  ( 169.4976558230340231, 251.7484151835147657, -9.940267045083754027 ) ) ;
#901 = CARTESIAN_POINT ( 'NONE',  ( 161.8566033897550085, 252.0880471315855686, 14.23877116480228544 ) ) ;
#902 = CARTESIAN_POINT ( 'NONE',  ( 157.6335212189247557, 257.6177276032722716, 16.76495363836117036 ) ) ;
#903 = CARTESIAN_POINT ( 'NONE',  ( -22.42236680055709641, 157.8615022471902591, 0.000000000000000000 ) ) ;
#904 = CARTESIAN_POINT ( 'NONE',  ( 72.71381692756899895, 57.00322135356037023, -15.91178980316282043 ) ) ;
#905 = EDGE_CURVE ( 'NONE', #18632, #67404, #6039, .T. ) ;
#906 = CARTESIAN_POINT ( 'NONE',  ( 37.36027580478099708, 198.5024278399160664, 9.188101187500095079 ) ) ;
#907 = CARTESIAN_POINT ( 'NONE',  ( 78.84873917453550973, 207.1423013555409796, -4.594050593750043987 ) ) ;
#908 = CARTESIAN_POINT ( 'NONE',  ( 5.968649350820379063, 188.6868197944959604, -22.49999999999984368 ) ) ;
#909 = CARTESIAN_POINT ( 'NONE',  ( 88.13330906385691321, 44.06097395418934326, 0.5526411241947467579 ) ) ;
#910 = EDGE_CURVE ( 'NONE', #22139, #62627, #36935, .T. ) ;
#911 = CARTESIAN_POINT ( 'NONE',  ( 167.2464745708191458, 259.8228882802526982, 16.05418551386606651 ) ) ;
#912 = CARTESIAN_POINT ( 'NONE',  ( 147.5623555321158165, 249.8768266524159856, -9.188101187500091527 ) ) ;
#914 = CARTESIAN_POINT ( 'NONE',  ( 77.22785773251615637, 49.24952049019824329, 15.36076451811752719 ) ) ;
#913 = CARTESIAN_POINT ( 'NONE',  ( -54.24312371938221133, 45.66933727564025247, 59.99999999999999289 ) ) ;
#915 = CARTESIAN_POINT ( 'NONE',  ( -37.96271243472389756, 25.23297040071578223, -10.00000000000000000 ) ) ;
#917 = EDGE_CURVE ( 'NONE', #66866, #86172, #60293, .T. ) ;
#916 = VECTOR ( 'NONE', #19818, 1000.000000000000000 ) ;
#918 = CARTESIAN_POINT ( 'NONE',  ( 33.49394369984602804, 21.19860640527294038, 2.839279412974134775 ) ) ;
#919 = CARTESIAN_POINT ( 'NONE',  ( 150.7133245577828689, 269.6038598187387834, -14.58664962216439598 ) ) ;
#920 = CARTESIAN_POINT ( 'NONE',  ( 196.2630260332681189, 290.7094625936034049, -17.43112004684450866 ) ) ;
#921 = CARTESIAN_POINT ( 'NONE',  ( 17.79544559245429625, 15.98920272979925628, 7.433330006724137462 ) ) ;
#922 = CARTESIAN_POINT ( 'NONE',  ( 68.13167480270307408, 200.9548013555409796, -4.594050593750042211 ) ) ;
#923 = CARTESIAN_POINT ( 'NONE',  ( 76.72890798614155017, 63.86846200969244336, 14.87016573101661265 ) ) ;
#924 = CARTESIAN_POINT ( 'NONE',  ( 203.1044072055706806, 278.8598428092302584, -16.67109798570195878 ) ) ;
#925 = CARTESIAN_POINT ( 'NONE',  ( 198.5966822647444587, 286.6674514332866579, 17.25284514431582750 ) ) ;
#926 = PLANE ( 'NONE',  #45711 ) ;
#927 = CARTESIAN_POINT ( 'NONE',  ( 153.3890631498689743, 264.9693446294729711, 16.84838431772464773 ) ) ;
#928 = ADVANCED_FACE ( 'NONE', ( #98768 ), #28850, .T. ) ;
#929 = AXIS2_PLACEMENT_3D ( 'NONE', #31113, #92953, #30634 ) ;
#930 = CARTESIAN_POINT ( 'NONE',  ( 79.71580056254293822, 55.22957162338799009, -16.02820282535946106 ) ) ;
#931 = CARTESIAN_POINT ( 'NONE',  ( 103.0791479645378104, 236.9865022471902876, -10.00000000000009415 ) ) ;
#932 = CARTESIAN_POINT ( 'NONE',  ( 200.8769374536528858, 282.7179335918746688, 17.26928237494566787 ) ) ;
#933 = CARTESIAN_POINT ( 'NONE',  ( 164.4781197247689306, 245.7625352337404649, -1.511762618280499515 ) ) ;
#934 = VERTEX_POINT ( 'NONE', #51650 ) ;
#935 = CARTESIAN_POINT ( 'NONE',  ( 77.14514041473603356, 49.33218330559527942, 15.40661048312039583 ) ) ;
#936 = CARTESIAN_POINT ( 'NONE',  ( 184.6950506501621021, 271.1962962339267165, 16.22049766843658603 ) ) ;
#937 = ORIENTED_EDGE ( 'NONE', *, *, #80216, .F. ) ;
#938 = CARTESIAN_POINT ( 'NONE',  ( 206.6912923161529818, 272.6471755567893638, -9.325620632947922317 ) ) ;
#939 = CARTESIAN_POINT ( 'NONE',  ( 193.9232833982383113, 293.2909642926495621, 15.00674244883364139 ) ) ;
#940 = CARTESIAN_POINT ( 'NONE',  ( 70.23258906160542381, 68.89773635095485815, -7.744023681228862976 ) ) ;
#941 = VERTEX_POINT ( 'NONE', #98260 ) ;
#942 = DIRECTION ( 'NONE',  ( -0.000000000000000000, -0.000000000000000000, -1.000000000000000000 ) ) ;
#943 = ORIENTED_EDGE ( 'NONE', *, *, #73759, .T. ) ;
#944 = CARTESIAN_POINT ( 'NONE',  ( 79.57426776858704898, 46.24084366563779724, -13.18946159609117252 ) ) ;
#945 = CARTESIAN_POINT ( 'NONE',  ( 194.3011251241114508, 294.1075746476782342, -14.76047579547631905 ) ) ;
#946 = FACE_OUTER_BOUND ( 'NONE', #38925, .T. ) ;
#947 = VERTEX_POINT ( 'NONE', #91178 ) ;
#948 = CARTESIAN_POINT ( 'NONE',  ( 33.34238925418374322, 21.11110640527294180, -2.839279412974138328 ) ) ;
#949 = VECTOR ( 'NONE', #67160, 1000.000000000000000 ) ;
#950 = CARTESIAN_POINT ( 'NONE',  ( 80.01036472522686438, 44.36946922474368904, 11.55303063996890245 ) ) ;
#951 = CARTESIAN_POINT ( 'NONE',  ( 30.24280306353621128, 178.2677522451417929, -5.000000000000041744 ) ) ;
#952 = CARTESIAN_POINT ( 'NONE',  ( 75.00927956955034404, 66.36452684332685692, -13.11830550837433229 ) ) ;
#953 = ORIENTED_EDGE ( 'NONE', *, *, #83634, .T. ) ;
#954 = DIRECTION ( 'NONE',  ( -0.8845109580947964067, 0.1124011590738280275, 0.4527762631246092795 ) ) ;
#955 = CARTESIAN_POINT ( 'NONE',  ( 159.7132918459648181, 254.0154592091499239, -16.90058287995827158 ) ) ;
#956 = AXIS2_PLACEMENT_3D ( 'NONE', #84126, #36465, #99782 ) ;
#957 = ORIENTED_EDGE ( 'NONE', *, *, #62143, .T. ) ;
#958 = CARTESIAN_POINT ( 'NONE',  ( 174.8110114269580606, 286.1294775324029160, 11.21431686804888983 ) ) ;
#960 = CARTESIAN_POINT ( 'NONE',  ( 67.96729249982780630, 66.07064282809847100, -10.47701906205939792 ) ) ;
#959 = CARTESIAN_POINT ( 'NONE',  ( 163.2766929973646484, 283.7647176037089594, -3.009406773168611604 ) ) ;
#961 = CYLINDRICAL_SURFACE ( 'NONE', #15742, 70.00000000000002842 ) ;
#962 = CARTESIAN_POINT ( 'NONE',  ( 194.1493756275458793, 294.3704124857528655, 13.94613522129020744 ) ) ;
#963 = CARTESIAN_POINT ( 'NONE',  ( 32.41152252715882298, 42.21091486745863364, 7.012934429366973338E-14 ) ) ;
#964 = CARTESIAN_POINT ( 'NONE',  ( 157.1539462478114615, 258.4483758192793061, -17.96006278656275867 ) ) ;
#965 = CARTESIAN_POINT ( 'NONE',  ( 138.6852480475602931, 257.0024278399160949, 9.188101187500095079 ) ) ;
#966 = CARTESIAN_POINT ( 'NONE',  ( 206.3049127377101968, 270.5357785998967870, 2.445900227168405383 ) ) ;
#967 = CARTESIAN_POINT ( 'NONE',  ( 179.2020837305335306, 258.4857288146945962, 9.693322143454775386 ) ) ;
#968 = CARTESIAN_POINT ( 'NONE',  ( 80.33678646758374953, 223.3149278399160949, -9.188101187500095079 ) ) ;
#969 = EDGE_LOOP ( 'NONE', ( #9920, #90585, #63476, #91922 ) ) ;
#970 = CARTESIAN_POINT ( 'NONE',  ( 151.4327733764141612, 268.3577379114237829, 14.90862905801242100 ) ) ;
#971 = CARTESIAN_POINT ( 'NONE',  ( 77.91510949599519620, 62.18724900762369856, -15.97225761198294691 ) ) ;
#972 = EDGE_LOOP ( 'NONE', ( #1245, #99515, #43357, #14062, #15878 ) ) ;
#973 = CARTESIAN_POINT ( 'NONE',  ( 157.2072737763903945, 258.3560098303381096, -16.87862088075553402 ) ) ;
#974 = ORIENTED_EDGE ( 'NONE', *, *, #10004, .T. ) ;
#975 = ORIENTED_EDGE ( 'NONE', *, *, #37146, .F. ) ;
#976 = CARTESIAN_POINT ( 'NONE',  ( 79.89934654500854094, 44.60194503138297506, -11.13433824245048953 ) ) ;
#977 = CARTESIAN_POINT ( 'NONE',  ( 66.62422707585170656, 67.62317984664836956, 6.187721633850552294 ) ) ;
#978 = CARTESIAN_POINT ( 'NONE',  ( 146.6138605399200117, 276.7043397814778132, -0.5394499176159462950 ) ) ;
#979 = CARTESIAN_POINT ( 'NONE',  ( 149.3545991938273971, 273.9572411826421217, -10.14243178476390028 ) ) ;
#980 = CARTESIAN_POINT ( 'NONE',  ( 83.22635668477047943, 47.66699298699816723, -12.18745831367220944 ) ) ;
#981 = DIRECTION ( 'NONE',  ( -0.9999990636452668058, -0.001368469433204011270, 0.000000000000000000 ) ) ;
#982 = CARTESIAN_POINT ( 'NONE',  ( 90.35072584248885619, 210.7202760586659736, -5.415160957724236172E-17 ) ) ;
#983 = VERTEX_POINT ( 'NONE', #22234 ) ;
#984 = ORIENTED_EDGE ( 'NONE', *, *, #57106, .F. ) ;
#985 = CARTESIAN_POINT ( 'NONE',  ( 112.9278751967105450, 247.5530062829863311, -4.648177544792955347E-16 ) ) ;
#986 = CARTESIAN_POINT ( 'NONE',  ( 161.2518619042614034, 251.3505776971759360, -13.56582882383257349 ) ) ;
#987 = ORIENTED_EDGE ( 'NONE', *, *, #63428, .F. ) ;
#988 = LINE ( 'NONE', #76978, #61278 ) ;
#989 = EDGE_CURVE ( 'NONE', #100173, #64867, #53135, .T. ) ;
#990 = CARTESIAN_POINT ( 'NONE',  ( 183.6463619201787481, 275.7299020814296568, 17.02459170948687373 ) ) ;
#991 = VECTOR ( 'NONE', #68257, 1000.000000000000000 ) ;
#992 = CARTESIAN_POINT ( 'NONE',  ( -30.47963256238546492, 93.39033706315194650, 44.25085353260880794 ) ) ;
#993 = CARTESIAN_POINT ( 'NONE',  ( 155.8152618860606538, 260.7670451491295012, 0.000000000000000000 ) ) ;
#995 = B_SPLINE_CURVE_WITH_KNOTS ( 'NONE', 3,
 ( #93557, #16517, #56515, #15503, #64120, #95070, #66486, #75593, #82240, #36571, #12816, #89829, #28998, #37076, #6178, #35591, #2850, #41302, #36075, #18038, #21388, #28478, #5193, #20405, #10938, #51799, #26130, #74107, #58860, #10430, #27981 ),
 .UNSPECIFIED., .F., .F.,
 ( 4, 3, 3, 3, 3, 3, 3, 3, 3, 3, 4 ),
 ( 0.000000000000000000, 0.1333490885032329043, 0.3007194338854308202, 0.4699862290245099827, 0.5844252810809248411, 0.6686540514502534727, 0.7354980260655189506, 0.8028463152565233907, 0.8633854507756654195, 0.9437142632666670750, 1.000000000000000000 ),
 .UNSPECIFIED. ) ;
#994 = CARTESIAN_POINT ( 'NONE',  ( 88.25642124133898392, 44.32248799199468436, 4.097629997315074490 ) ) ;
#996 = EDGE_LOOP ( 'NONE', ( #34380, #44799, #80487, #3308 ) ) ;
#997 = CARTESIAN_POINT ( 'NONE',  ( 81.50097959531993297, 43.67013008731806423, -9.164372295790522926 ) ) ;
#998 = CARTESIAN_POINT ( 'NONE',  ( 185.2745384195171141, 260.2690603060960370, 6.274088207539249673 ) ) ;
#999 = CARTESIAN_POINT ( 'NONE',  ( 36.28012939083434674, 26.11029122506296929, -8.090169943749478065 ) ) ;
#1001 = EDGE_CURVE ( 'NONE', #40825, #22518, #21739, .T. ) ;
#1000 = CARTESIAN_POINT ( 'NONE',  ( 200.7694952279801157, 282.9040289856181403, -17.94628235092568502 ) ) ;
#1002 = VECTOR ( 'NONE', #51820, 1000.000000000000000 ) ;
#1003 = CARTESIAN_POINT ( 'NONE',  ( 72.48280754011683769, 70.60311863597819126, 7.264376673680512653 ) ) ;
#1004 = EDGE_CURVE ( 'NONE', #12032, #15116, #42515, .T. ) ;
#1005 = CARTESIAN_POINT ( 'NONE',  ( 50.33662733789741139, 94.26254718190894266, -10.00000000000000000 ) ) ;
#1006 = ORIENTED_EDGE ( 'NONE', *, *, #90756, .F. ) ;
#1007 = CARTESIAN_POINT ( 'NONE',  ( 186.6806167748573273, 293.5666024053780916, -12.22359308779079079 ) ) ;
#1008 = CARTESIAN_POINT ( 'NONE',  ( 200.8828793852583203, 282.7076418644388696, 17.90302398138411633 ) ) ;
#1009 = CARTESIAN_POINT ( 'NONE',  ( 87.56313949369642557, 43.39506783062379469, 1.585011492977574488 ) ) ;
#1010 = CARTESIAN_POINT ( 'NONE',  ( 169.7276834213985239, 251.0855122629868106, 6.971127372306837877 ) ) ;
#1011 = CARTESIAN_POINT ( 'NONE',  ( 83.81044542681900111, 52.09240911291835374, 14.60277729873947905 ) ) ;
#1012 = CARTESIAN_POINT ( 'NONE',  ( 156.9258225138436842, 272.6371026541438596, 14.45601229042061675 ) ) ;
#1013 = CARTESIAN_POINT ( 'NONE',  ( 162.7561251957091031, 248.7451172484279027, 11.07313294959361194 ) ) ;
#1014 = B_SPLINE_CURVE_WITH_KNOTS ( 'NONE', 3,
 ( #94462, #9852, #87416, #64532 ),
 .UNSPECIFIED., .F., .F.,
 ( 4, 4 ),
 ( 0.02269137219855666548, 0.03190570623119325794 ),
 .UNSPECIFIED. ) ;
#1015 = VECTOR ( 'NONE', #6214, 1000.000000000000227 ) ;
#1016 = CARTESIAN_POINT ( 'NONE',  ( 77.93017357788673394, 184.0458036431182052, -30.52142883766498116 ) ) ;
#1018 = FACE_BOUND ( 'NONE', #32836, .T. ) ;
#1017 = CARTESIAN_POINT ( 'NONE',  ( 194.4889937320412230, 293.7821766735966662, 14.99892588346621380 ) ) ;
#1019 = CARTESIAN_POINT ( 'NONE',  ( 200.1528453280087945, 282.4639923692292314, -16.67548112269998128 ) ) ;
#1020 = CARTESIAN_POINT ( 'NONE',  ( 25.82140064434168636, 39.00034080476291365, -1.878358725466461243E-16 ) ) ;
#1021 = CARTESIAN_POINT ( 'NONE',  ( 168.3381296007061678, 273.6507282997970947, 16.34367694402899573 ) ) ;
#1022 = DIRECTION ( 'NONE',  ( 0.2588190451025028094, 0.9659258262890731972, -2.513112717808992705E-15 ) ) ;
#1023 = LINE ( 'NONE', #92751, #45256 ) ;
#1024 = CONICAL_SURFACE ( 'NONE', #73855, 2.749999999999999112, 0.7853981633974463916 ) ;
#1025 = CARTESIAN_POINT ( 'NONE',  ( 188.8970709661001592, 261.1830301768237632, 2.866754512114129128 ) ) ;
#1026 = CARTESIAN_POINT ( 'NONE',  ( 194.9663593620817892, 265.9656423931795644, -7.350908074652497071 ) ) ;
#1027 = EDGE_CURVE ( 'NONE', #65437, #26008, #58647, .T. ) ;
#1028 = CARTESIAN_POINT ( 'NONE',  ( -6.184650803196579893, 176.4244531367911293, -4.594050593750046652 ) ) ;
#1029 = CARTESIAN_POINT ( 'NONE',  ( 154.6982851380984130, 273.6571292083216349, -13.42362762759460892 ) ) ;
#1030 = VERTEX_POINT ( 'NONE', #52623 ) ;
#1031 = CARTESIAN_POINT ( 'NONE',  ( 161.1018488054811542, 253.0685122771756994, -14.87691902254530696 ) ) ;
#1032 = ADVANCED_FACE ( 'NONE', ( #74961 ), #37422, .T. ) ;
#1033 = CARTESIAN_POINT ( 'NONE',  ( 19.02883662497902861, 11.39040679176981996, 1.333680081654574804E-15 ) ) ;
#1034 = CARTESIAN_POINT ( 'NONE',  ( 164.6063343576543048, 274.4739709976624908, 16.17759516952312637 ) ) ;
#1035 = CARTESIAN_POINT ( 'NONE',  ( 22.47598482088345406, 171.5327760586659451, 1.948934522072302763E-15 ) ) ;
#1036 = CARTESIAN_POINT ( 'NONE',  ( 71.24475614018626857, 200.3932355074535963, -2.679491924311248496 ) ) ;
#1037 = CARTESIAN_POINT ( 'NONE',  ( 35.42939366167109938, 22.58380873178788306, 6.180339887498953466 ) ) ;
#1038 = CARTESIAN_POINT ( 'NONE',  ( 129.9981042655041392, 235.8615022471901739, 5.000000000000051514 ) ) ;
#1039 = B_SPLINE_CURVE_WITH_KNOTS ( 'NONE', 3,
 ( #8432, #70727, #7943, #24129, #38316, #68726, #92091, #16026, #78345, #39300, #69722, #86490, #100153, #85996 ),
 .UNSPECIFIED., .F., .F.,
 ( 4, 2, 2, 2, 2, 2, 4 ),
 ( 0.000000000000000000, 0.0004397231552390210105, 0.0008794463104780420211, 0.001099307888097552418, 0.001319169465717063032, 0.001539031043336573645, 0.001758892620956084042 ),
 .UNSPECIFIED. ) ;
#1040 = CARTESIAN_POINT ( 'NONE',  ( 173.3440299427151388, 273.3511298303828312, -17.59202441768653102 ) ) ;
#1041 = CARTESIAN_POINT ( 'NONE',  ( 13.97105408662886461, 167.3262482093458061, -5.229199737892075682E-14 ) ) ;
#1042 = ADVANCED_FACE ( 'NONE', ( #29840 ), #14643, .F. ) ;
#1043 = DIRECTION ( 'NONE',  ( 0.8660254037844395958, 0.4999999999999985567, 0.000000000000000000 ) ) ;
#1044 = CARTESIAN_POINT ( 'NONE',  ( 150.3996455637841621, 270.1471677736116703, 15.13740740754872327 ) ) ;
#1045 = CARTESIAN_POINT ( 'NONE',  ( 64.10800479423805598, 214.4865022471902876, -10.00000000000009415 ) ) ;
#1046 = CARTESIAN_POINT ( 'NONE',  ( 73.36681650135379584, 66.22633458900254766, -12.49190051511774868 ) ) ;
#1047 = B_SPLINE_CURVE_WITH_KNOTS ( 'NONE', 3,
 ( #4963, #35344, #52530, #58627, #50535, #97673, #89601, #44432, #35845, #21165 ),
 .UNSPECIFIED., .F., .F.,
 ( 4, 2, 2, 2, 4 ),
 ( 0.000000000000000000, 0.2499999999999983347, 0.4999999999999988898, 0.7499999999999994449, 1.000000000000000000 ),
 .UNSPECIFIED. ) ;
#1048 = CARTESIAN_POINT ( 'NONE',  ( 80.00798602660123038, 150.6044130683315814, 4.041334437186263538E-16 ) ) ;
#1049 = CARTESIAN_POINT ( 'NONE',  ( 36.95476026646328194, 182.9548013555409796, -4.594050593750042211 ) ) ;
#1050 = CARTESIAN_POINT ( 'NONE',  ( 72.74024025722111730, 70.77703717069299216, -7.960999691682594914 ) ) ;
#1051 = LINE ( 'NONE', #62833, #74374 ) ;
#1052 = CARTESIAN_POINT ( 'NONE',  ( -4.696103426644111956, 79.65490786025929992, 13.63766756523351020 ) ) ;
#1053 = CARTESIAN_POINT ( 'NONE',  ( 199.1526122334580862, 285.7045524820243259, -17.32174362185583050 ) ) ;
#1054 = DIRECTION ( 'NONE',  ( -0.9954067278227237692, 0.09573633691163400961, 0.000000000000000000 ) ) ;
#1055 = DIRECTION ( 'NONE',  ( 3.817860598523670672E-18, 1.090355031989287297E-16, 1.000000000000000000 ) ) ;
#1056 = CARTESIAN_POINT ( 'NONE',  ( 202.2006020915977729, 279.2500615382859905, -15.85648173203151323 ) ) ;
#1057 = CARTESIAN_POINT ( 'NONE',  ( 163.9073938094922767, 282.0100812378155410, 10.03296392472801024 ) ) ;
#1058 = CARTESIAN_POINT ( 'NONE',  ( 17.99393647837114329, 33.49540643055186706, 3.479690158560446702E-15 ) ) ;
#1059 = CARTESIAN_POINT ( 'NONE',  ( 202.7599932440484451, 279.4563852894229967, 15.58249343055423353 ) ) ;
#1060 = CARTESIAN_POINT ( 'NONE',  ( 100.8238734719678860, 239.0177522451419350, 5.000000000000046185 ) ) ;
#1061 = VECTOR ( 'NONE', #41991, 1000.000000000000000 ) ;
#1062 = CARTESIAN_POINT ( 'NONE',  ( 175.2559942677915785, 257.1225370724986874, 11.81907156814548365 ) ) ;
#1063 = ORIENTED_EDGE ( 'NONE', *, *, #73652, .T. ) ;
#1064 = VECTOR ( 'NONE', #92848, 999.9999999999998863 ) ;
#1065 = CARTESIAN_POINT ( 'NONE',  ( 7.128892988474023085, 19.51421378149916563, -9.188101187500004485 ) ) ;
#1066 = CARTESIAN_POINT ( 'NONE',  ( 88.24246443646677562, 44.29974554292944333, 4.047255302186846926 ) ) ;
#1067 = CARTESIAN_POINT ( 'NONE',  ( 77.56650176279948994, 58.32259081542915879, -16.15928628467516859 ) ) ;
#1068 = CARTESIAN_POINT ( 'NONE',  ( 87.95476553115707929, 44.23128429206734324, 2.820676398910382243 ) ) ;
#1069 = ORIENTED_EDGE ( 'NONE', *, *, #50508, .F. ) ;
#1071 = CARTESIAN_POINT ( 'NONE',  ( 32.27361296988652128, 177.8932355074535678, -2.679491924311248496 ) ) ;
#1070 =( BOUNDED_CURVE ( )  B_SPLINE_CURVE ( 2, ( #26741, #78974, #33868, #55617, #95188, #32338, #25759, #50042, #86600 ),
 .UNSPECIFIED., .F., .T. ) 
 B_SPLINE_CURVE_WITH_KNOTS ( ( 3, 2, 2, 2, 3 ),
 ( 0.3588709677419354982, 0.3602150537634408733, 0.3629032258064516236, 0.3655913978494623739, 0.3669354838709677491 ),
 .UNSPECIFIED. ) 
 CURVE ( )  GEOMETRIC_REPRESENTATION_ITEM ( )  RATIONAL_B_SPLINE_CURVE ( ( 0.9330127018922194093, 0.9330127018922194093, 1.000000000000000000, 0.8660254037844387076, 1.000000000000000000, 0.8660254037844387076, 1.000000000000000000, 0.9330127018922194093, 0.9330127018922194093 ) ) 
 REPRESENTATION_ITEM ( '' )  );
#1072 = CARTESIAN_POINT ( 'NONE',  ( 72.37415438388894984, 71.90064624941815907, -5.324036893254605829 ) ) ;
#1073 = VECTOR ( 'NONE', #13467, 1000.000000000000000 ) ;
#1074 = CARTESIAN_POINT ( 'NONE',  ( 85.24521657786070250, 49.07911862026776362, 12.45208212324389763 ) ) ;
#1075 = CARTESIAN_POINT ( 'NONE',  ( 84.13220800937075694, 41.60931624182121169, 2.733980135768734332 ) ) ;
#1076 = ORIENTED_EDGE ( 'NONE', *, *, #83228, .T. ) ;
#1077 = VERTEX_POINT ( 'NONE', #76454 ) ;
#1079 = CARTESIAN_POINT ( 'NONE',  ( 84.04471568993460551, 42.57412079040409481, -4.602180766856474037 ) ) ;
#1078 = DIRECTION ( 'NONE',  ( 0.4999999999999998890, -0.8660254037844385966, 0.000000000000000000 ) ) ;
#1080 = ORIENTED_EDGE ( 'NONE', *, *, #21239, .T. ) ;
#1081 = CARTESIAN_POINT ( 'NONE',  ( 191.5766842709549280, 298.8264446275616137, 8.039910086100929831 ) ) ;
#1082 = CARTESIAN_POINT ( 'NONE',  ( 72.09683433654826956, 72.38845567423071259, -3.220643376046866901 ) ) ;
#1083 = CYLINDRICAL_SURFACE ( 'NONE', #77437, 17.82106496071139645 ) ;
#1084 = CARTESIAN_POINT ( 'NONE',  ( 77.31919379202844311, 63.29706486701976331, 15.55867855103717545 ) ) ;
#1085 = EDGE_CURVE ( 'NONE', #56387, #18338, #31160, .T. ) ;
#1086 = CARTESIAN_POINT ( 'NONE',  ( 147.6220714307702622, 274.9580672937808572, 8.392894244419288441 ) ) ;
#1087 = CARTESIAN_POINT ( 'NONE',  ( 148.9194629746633893, 272.7109192224475009, -12.27648025871169679 ) ) ;
#1088 = CARTESIAN_POINT ( 'NONE',  ( 180.5747241553744686, 287.0254358638467806, -13.54112932651550416 ) ) ;
#1089 = ORIENTED_EDGE ( 'NONE', *, *, #73411, .F. ) ;
#1090 = FACE_OUTER_BOUND ( 'NONE', #73993, .T. ) ;
#1091 = CIRCLE ( 'NONE', #54496, 70.00000000000001421 ) ;
#1092 = CARTESIAN_POINT ( 'NONE',  ( 161.9493756838661511, 266.9722091390776768, 16.54811282007660012 ) ) ;
#1093 = ORIENTED_EDGE ( 'NONE', *, *, #65996, .T. ) ;
#1094 = CARTESIAN_POINT ( 'NONE',  ( 23.19008890107777177, 36.49540643055188838, 3.479690158560446702E-15 ) ) ;
#1095 = CARTESIAN_POINT ( 'NONE',  ( 157.1289238671306805, 259.1523436189365270, 17.02785937198905941 ) ) ;
#1096 = DIRECTION ( 'NONE',  ( 0.000000000000000000, 0.000000000000000000, 1.000000000000000000 ) ) ;
#1097 = CARTESIAN_POINT ( 'NONE',  ( 58.68649846873780263, 198.5643266524160140, 9.188101187500095079 ) ) ;
#1098 = VERTEX_POINT ( 'NONE', #99752 ) ;
#1099 = CARTESIAN_POINT ( 'NONE',  ( 74.17419530692131957, 68.61376803465689989, 10.99684454571890591 ) ) ;
#1100 = CARTESIAN_POINT ( 'NONE',  ( 82.15463706511577868, 40.84277258114416043, 1.595534587534165549 ) ) ;
#1102 = CIRCLE ( 'NONE', #14042, 70.00000000000001421 ) ;
#1101 = DIRECTION ( 'NONE',  ( 1.000000000000000000, 1.070572202317114942E-14, 0.000000000000000000 ) ) ;
#1103 = VERTEX_POINT ( 'NONE', #60710 ) ;
#1104 = CARTESIAN_POINT ( 'NONE',  ( 86.89671376885311815, 46.48613028513706524, 9.014139361656079430 ) ) ;
#1105 = CARTESIAN_POINT ( 'NONE',  ( 85.23557152020472927, 43.11680246062262256, -4.179448767779550877 ) ) ;
#1106 = CARTESIAN_POINT ( 'NONE',  ( 190.1607982559816890, 301.2788311432216233, -4.972636536415983244 ) ) ;
#1107 = CARTESIAN_POINT ( 'NONE',  ( 147.6207754342248961, 274.9603120256437592, 8.795690793376332195 ) ) ;
#1108 = VERTEX_POINT ( 'NONE', #37915 ) ;
#1109 = CARTESIAN_POINT ( 'NONE',  ( 175.3538927705540686, 261.0322813687463395, -14.65776196239626650 ) ) ;
#1110 = CARTESIAN_POINT ( 'NONE',  ( 171.9695299662907360, 276.3046275190319534, -16.98996149290084645 ) ) ;
#1111 = CARTESIAN_POINT ( 'NONE',  ( 207.8792014703394671, 270.5896565469619759, -5.780233892547864905 ) ) ;
#1112 = CARTESIAN_POINT ( 'NONE',  ( 193.1169444172380167, 296.1586357973259283, -13.13373377033755318 ) ) ;
#1113 = CARTESIAN_POINT ( 'NONE',  ( 163.8566702472313921, 257.1696457478908542, 15.67296822151954849 ) ) ;
#1114 = CARTESIAN_POINT ( 'NONE',  ( 176.9230647991562364, 269.9553266851162334, 16.63264067541030755 ) ) ;
#1115 = CARTESIAN_POINT ( 'NONE',  ( 84.39378192592442929, 42.61420722820205498, -5.616381072414180942 ) ) ;
#1116 = CARTESIAN_POINT ( 'NONE',  ( 67.53167658288728603, 67.09922345405099975, 8.942594108729585045 ) ) ;
#1117 = CARTESIAN_POINT ( 'NONE',  ( 74.55495018319990663, 64.55344886072012400, -13.93350266944992555 ) ) ;
#1118 = CARTESIAN_POINT ( 'NONE',  ( 78.05253372616796526, 47.80071866568432171, 14.02011486286742858 ) ) ;
#1119 = CARTESIAN_POINT ( 'NONE',  ( 109.2403843188893831, 240.0024278399160949, -9.188101187500093303 ) ) ;
#1120 = ORIENTED_EDGE ( 'NONE', *, *, #15724, .F. ) ;
#1121 = CARTESIAN_POINT ( 'NONE',  ( 191.1000148935602567, 299.6520602076213891, -9.462302242170249400 ) ) ;
#1122 = DIRECTION ( 'NONE',  ( -1.000000000000000000, 0.000000000000000000, 0.000000000000000000 ) ) ;
#1123 = CARTESIAN_POINT ( 'NONE',  ( 155.6535436963908694, 261.0471492701456668, -17.87366571046205976 ) ) ;
#1124 = EDGE_CURVE ( 'NONE', #7185, #31220, #63203, .T. ) ;
#1125 = CARTESIAN_POINT ( 'NONE',  ( 192.3862142521138878, 296.3260726571497798, 12.05156688669263687 ) ) ;
#1126 = EDGE_CURVE ( 'NONE', #56387, #14902, #59211, .T. ) ;
#1127 = CYLINDRICAL_SURFACE ( 'NONE', #11083, 17.82106496071139645 ) ;
#1128 = CARTESIAN_POINT ( 'NONE',  ( 76.04961876167374157, 51.28812058955301723, -15.63847478383918421 ) ) ;
#1129 = ORIENTED_EDGE ( 'NONE', *, *, #70913, .F. ) ;
#1130 = PLANE ( 'NONE',  #21880 ) ;
#1131 = CARTESIAN_POINT ( 'NONE',  ( 71.96379157542388327, 72.26892066703038608, 0.6295764574549533865 ) ) ;
#1132 = CARTESIAN_POINT ( 'NONE',  ( 72.04811769650319775, 71.35602353065117143, 5.168332083721276504 ) ) ;
#1133 = CARTESIAN_POINT ( 'NONE',  ( 206.7044739906782809, 272.6243442267827959, -10.28926534613781030 ) ) ;
#1134 = CARTESIAN_POINT ( 'NONE',  ( 126.4254891512956220, 252.9869531367911009, 4.594050593750046652 ) ) ;
#1135 = CARTESIAN_POINT ( 'NONE',  ( 151.1126408083691501, 268.9122237844355254, -15.82705194100464396 ) ) ;
#1136 = CARTESIAN_POINT ( 'NONE',  ( 185.5783427554117395, 297.2518047243089541, 4.097492125301632093 ) ) ;
#1137 = B_SPLINE_CURVE_WITH_KNOTS ( 'NONE', 3,
 ( #78716, #23991, #63498, #54889, #85870, #16396, #88363, #18922, #65993, #11329 ),
 .UNSPECIFIED., .F., .F.,
 ( 4, 2, 2, 2, 4 ),
 ( 0.000000000000000000, 0.2500000000000000000, 0.5000000000000000000, 0.7500000000000000000, 1.000000000000000000 ),
 .UNSPECIFIED. ) ;
#1138 = CARTESIAN_POINT ( 'NONE',  ( 187.5093160991869752, 281.3588210269506931, -17.01637650260816059 ) ) ;
#1139 = CARTESIAN_POINT ( 'NONE',  ( 83.55337146356914957, 41.01436309113273637, -0.4425042433306793921 ) ) ;
#1140 = CARTESIAN_POINT ( 'NONE',  ( 46.39958950466356669, 197.5958772461660544, -9.188101187500095079 ) ) ;
#1142 = CARTESIAN_POINT ( 'NONE',  ( 78.56356803705116931, 59.62236819939711552, -16.48917668510493684 ) ) ;
#1141 = AXIS2_PLACEMENT_3D ( 'NONE', #13781, #6180, #37077 ) ;
#1143 = ORIENTED_EDGE ( 'NONE', *, *, #74016, .T. ) ;
#1144 = CARTESIAN_POINT ( 'NONE',  ( -19.70914744582199774, 92.93475084401866582, 59.99999999999999289 ) ) ;
#1145 = CARTESIAN_POINT ( 'NONE',  ( 161.9461893331167914, 280.9078031139047198, -10.53061385661272276 ) ) ;
#1146 = B_SPLINE_SURFACE_WITH_KNOTS ( 'NONE', 3, 1, ( 
 ( #89996, #5855 ),
 ( #51958, #82898 ),
 ( #84381, #98579 ),
 ( #52440, #59026 ),
 ( #83388, #20572 ),
 ( #13953, #22044 ),
 ( #44836, #83892 ),
 ( #37727, #15933 ),
 ( #92477, #45818 ),
 ( #23024, #38730 ),
 ( #92967, #93981 ),
 ( #47330, #76742 ),
 ( #1760, #77240 ),
 ( #242, #7335 ),
 ( #23521, #53917 ),
 ( #54412, #40216 ),
 ( #46838, #61534 ),
 ( #8344, #77761 ),
 ( #38217, #85387 ),
 ( #78256, #70122 ),
 ( #31123, #8836 ),
 ( #735, #25031 ),
 ( #24533, #55910 ),
 ( #39215, #32639 ),
 ( #69633, #100062 ),
 ( #7846, #31619 ),
 ( #86398, #69132 ),
 ( #63535, #84879 ),
 ( #62516, #93479 ),
 ( #62015, #15419 ),
 ( #55414, #1246 ),
 ( #94477, #24032 ),
 ( #54932, #30649 ),
 ( #85909, #16436 ) ),
 .UNSPECIFIED., .T., .F., .F.,
 ( 4, 2, 2, 2, 2, 2, 2, 2, 2, 2, 2, 2, 2, 2, 2, 2, 4 ),
 ( 2, 2 ),
 ( 0.000000000000000000, 0.06250000000000000000, 0.1250000000000000000, 0.1875000000000000000, 0.2500000000000000000, 0.3125000000000000000, 0.3750000000000000000, 0.4375000000000000000, 0.5000000000000000000, 0.5625000000000000000, 0.6250000000000000000, 0.6875000000000000000, 0.7500000000000000000, 0.8125000000000000000, 0.8750000000000000000, 0.9375000000000000000, 1.000000000000000000 ),
 ( 0.000000000000000000, 1.000000000000000000 ),
 .UNSPECIFIED. ) ;
#1147 = CARTESIAN_POINT ( 'NONE',  ( 67.71395807953069834, 69.70288697866548944, -0.3208651280214164792 ) ) ;
#1148 = CARTESIAN_POINT ( 'NONE',  ( 174.7088583562716053, 261.8961954955167357, 14.25351817334065530 ) ) ;
#1149 = CARTESIAN_POINT ( 'NONE',  ( 151.2840067701813780, 278.5577605986394474, -1.687242923209387735 ) ) ;
#1150 = CARTESIAN_POINT ( 'NONE',  ( -30.95603806669010183, 23.98360954755323604, 177.5919119679930134 ) ) ;
#1151 = CARTESIAN_POINT ( 'NONE',  ( 17.82181404068577635, 169.5494855054051868, -2.679491924311248496 ) ) ;
#1152 = VECTOR ( 'NONE', #12982, 1000.000000000000000 ) ;
#1153 = EDGE_CURVE ( 'NONE', #7407, #88206, #54605, .T. ) ;
#1154 = CARTESIAN_POINT ( 'NONE',  ( 119.0825757350898755, 232.8927522451418213, 10.00000000000009592 ) ) ;
#1155 = CARTESIAN_POINT ( 'NONE',  ( 194.6014564220333511, 293.2009624057436099, -14.62462923522720715 ) ) ;
#1156 = ORIENTED_EDGE ( 'NONE', *, *, #93985, .F. ) ;
#1157 = CARTESIAN_POINT ( 'NONE',  ( 147.6430623265936219, 274.9217099957185155, 8.258152514891218487 ) ) ;
#1158 = CYLINDRICAL_SURFACE ( 'NONE', #83638, 10.00000000000010658 ) ;
#1159 = CARTESIAN_POINT ( 'NONE',  ( 34.24843087963692767, 181.3923013555409796, 4.594050593750050204 ) ) ;
#1160 = CARTESIAN_POINT ( 'NONE',  ( 18.95962131514559346, 16.11029122506294087, -8.090169943749478065 ) ) ;
#1161 = CIRCLE ( 'NONE', #65869, 0.1418229129681522482 ) ;
#1162 = CARTESIAN_POINT ( 'NONE',  ( 49.07456115661583596, 91.13648234292965356, -10.00000000000000000 ) ) ;
#1163 = CARTESIAN_POINT ( 'NONE',  ( 72.12578029244804156, 72.07013754146423423, 2.921549647394216631 ) ) ;
#1165 = CARTESIAN_POINT ( 'NONE',  ( 55.05949644674294774, 214.8464784336661637, 1.353441290958777327E-15 ) ) ;
#1164 = CARTESIAN_POINT ( 'NONE',  ( 2.161320418471442739, 24.18080186712590418, 3.090169943749475401 ) ) ;
#1166 = CARTESIAN_POINT ( 'NONE',  ( 172.5743551997954910, 287.3686559151746565, 7.484598097167019404 ) ) ;
#1167 = CARTESIAN_POINT ( 'NONE',  ( 184.7346430054644770, 257.4289713573899689, 1.391138223594709178 ) ) ;
#1168 = CARTESIAN_POINT ( 'NONE',  ( 204.6470611188870521, 276.1878878528713130, -13.02652554726987866 ) ) ;
#1169 = CARTESIAN_POINT ( 'NONE',  ( 66.51865997380296847, 68.29495818825724029, -4.336921469600853563 ) ) ;
#1170 = ORIENTED_EDGE ( 'NONE', *, *, #72286, .F. ) ;
#1171 = CARTESIAN_POINT ( 'NONE',  ( 179.4155677608637802, 294.8372702107813552, 1.080509646882094721 ) ) ;
#1172 = CARTESIAN_POINT ( 'NONE',  ( 33.07542782529571923, 183.2365022471902023, -10.00000000000009059 ) ) ;
#1173 = DIRECTION ( 'NONE',  ( -0.8965230319888208843, 0.4429971254010250936, 0.000000000000000000 ) ) ;
#1174 = VECTOR ( 'NONE', #10627, 1000.000000000000000 ) ;
#1175 = CARTESIAN_POINT ( 'NONE',  ( 162.7644741734472120, 248.7306563947940958, 9.865755277559742353 ) ) ;
#1176 = CARTESIAN_POINT ( 'NONE',  ( -5.724140937729833567, 161.3768266524159856, -9.188101187500091527 ) ) ;
#1177 = CARTESIAN_POINT ( 'NONE',  ( 27.72828276626169952, 36.98502408145593989, -5.678558825948271327 ) ) ;
#1179 = CARTESIAN_POINT ( 'NONE',  ( 200.3640505997411481, 282.4509422428217249, 17.04400613106654561 ) ) ;
#1178 = DIRECTION ( 'NONE',  ( 0.000000000000000000, 0.000000000000000000, 1.000000000000000000 ) ) ;
#1180 = CARTESIAN_POINT ( 'NONE',  ( 185.7885272225882147, 259.4715261277827949, 7.392998191279108511 ) ) ;
#1181 = CARTESIAN_POINT ( 'NONE',  ( 164.3090168944849836, 246.0554299274959931, 2.641760039552302430 ) ) ;
#1182 = DIRECTION ( 'NONE',  ( 0.8660254037844382635, 0.5000000000000005551, 0.000000000000000000 ) ) ;
#1183 = CARTESIAN_POINT ( 'NONE',  ( 66.04647813311905225, 68.58207190585535784, 1.910909007557326511 ) ) ;
#1184 = ORIENTED_EDGE ( 'NONE', *, *, #47229, .T. ) ;
#1185 = CARTESIAN_POINT ( 'NONE',  ( 177.8941590232256829, 264.7610587325321490, 16.13327920565182438 ) ) ;
#1186 = EDGE_CURVE ( 'NONE', #36969, #71264, #84573, .T. ) ;
#1187 = CARTESIAN_POINT ( 'NONE',  ( 177.8185504528716194, 286.5248637125107507, 13.46785215458145935 ) ) ;
#1188 = CARTESIAN_POINT ( 'NONE',  ( 167.1765958872485669, 286.3533408718084843, 0.5009160953947644490 ) ) ;
#1189 = CARTESIAN_POINT ( 'NONE',  ( 8.675723883004064163, 25.98502408145591147, -5.678558825948271327 ) ) ;
#1190 = DIRECTION ( 'NONE',  ( -0.8660254037844387076, -0.4999999999999998890, -0.000000000000000000 ) ) ;
#1191 = CARTESIAN_POINT ( 'NONE',  ( 206.0930919633010774, 273.6832889610345774, -9.866500005465628220 ) ) ;
#1192 = CARTESIAN_POINT ( 'NONE',  ( 152.6656396574222754, 266.2223508737794759, 17.04346597795114349 ) ) ;
#1193 = DIRECTION ( 'NONE',  ( 0.4999999999999992784, -0.8660254037844390407, 0.000000000000000000 ) ) ;
#1194 = CARTESIAN_POINT ( 'NONE',  ( 191.3509382880371561, 298.5884961055737108, 8.308752174519279166 ) ) ;
#1195 = CARTESIAN_POINT ( 'NONE',  ( 162.6257765080958677, 248.9708877980734485, -10.42859054881151160 ) ) ;
#1196 = CARTESIAN_POINT ( 'NONE',  ( 155.2695601165254402, 261.7122283397445131, 16.98599069618989077 ) ) ;
#1197 = VERTEX_POINT ( 'NONE', #62209 ) ;
#1198 = ORIENTED_EDGE ( 'NONE', *, *, #96350, .T. ) ;
#1199 = FACE_OUTER_BOUND ( 'NONE', #92317, .T. ) ;
#1200 = CARTESIAN_POINT ( 'NONE',  ( 72.95595290250773246, 70.82077856083527934, 7.354924289292173789 ) ) ;
#1201 = ORIENTED_EDGE ( 'NONE', *, *, #26302, .F. ) ;
#1202 = CARTESIAN_POINT ( 'NONE',  ( 69.03881359575697729, 65.98136758018425496, 11.20795008971583684 ) ) ;
#1203 = CARTESIAN_POINT ( 'NONE',  ( 10.24016918245798990, 49.27098784156451217, 59.99999999999999289 ) ) ;
#1204 = ORIENTED_EDGE ( 'NONE', *, *, #57213, .F. ) ;
#1205 = FACE_OUTER_BOUND ( 'NONE', #66271, .T. ) ;
#1206 = CARTESIAN_POINT ( 'NONE',  ( 79.40841717930322829, 59.11818797871130471, -16.22797407547709625 ) ) ;
#1207 = CARTESIAN_POINT ( 'NONE',  ( 197.0226655822963551, 289.3937282992477549, -17.28982543158101493 ) ) ;
#1208 = AXIS2_PLACEMENT_3D ( 'NONE', #24560, #55440, #15445 ) ;
#1209 = CARTESIAN_POINT ( 'NONE',  ( 12.22230530498201873, 30.55466486950698624, -1.111400068045478839E-16 ) ) ;
#1210 = ORIENTED_EDGE ( 'NONE', *, *, #81477, .F. ) ;
#1211 = CARTESIAN_POINT ( 'NONE',  ( 203.1289230791707325, 278.8173800705629901, 16.48573034889792766 ) ) ;
#1212 = AXIS2_PLACEMENT_3D ( 'NONE', #50050, #11070, #88611 ) ;
#1213 = CARTESIAN_POINT ( 'NONE',  ( 179.7896684074626705, 294.5542936293851994, 4.419446707887151327 ) ) ;
#1214 = CARTESIAN_POINT ( 'NONE',  ( 151.1926529451685326, 268.7736386982768408, 14.30343427984827365 ) ) ;
#1215 = CARTESIAN_POINT ( 'NONE',  ( 170.8865616681041786, 262.8912071418242817, 16.88624067591380040 ) ) ;
#1216 = ORIENTED_EDGE ( 'NONE', *, *, #59052, .T. ) ;
#1217 = ORIENTED_EDGE ( 'NONE', *, *, #67248, .F. ) ;
#1218 = VERTEX_POINT ( 'NONE', #22738 ) ;
#1219 = CARTESIAN_POINT ( 'NONE',  ( 73.18653013103410387, 60.48222858781691258, 15.22147476568558844 ) ) ;
#1220 = ORIENTED_EDGE ( 'NONE', *, *, #11993, .T. ) ;
#1221 = CARTESIAN_POINT ( 'NONE',  ( 67.16256804578091533, 66.80979783321161847, 8.146902435796070208 ) ) ;
#1222 = ORIENTED_EDGE ( 'NONE', *, *, #62050, .F. ) ;
#1223 = CARTESIAN_POINT ( 'NONE',  ( 164.4989226152910646, 245.7265035704120351, -6.575810094723514965 ) ) ;
#1224 =( GEOMETRIC_REPRESENTATION_CONTEXT ( 3 ) GLOBAL_UNCERTAINTY_ASSIGNED_CONTEXT ( ( #85922 ) ) GLOBAL_UNIT_ASSIGNED_CONTEXT ( ( #100216, #893, #55077 ) ) REPRESENTATION_CONTEXT ( 'NONE', 'WORKASPACE' ) );
#1225 = CARTESIAN_POINT ( 'NONE',  ( 194.3413770922408617, 282.8930799310762723, 17.82077676852630077 ) ) ;
#1226 = CARTESIAN_POINT ( 'NONE',  ( 167.8168677204402286, 281.0867839191200233, 11.63333370205274164 ) ) ;
#1227 = CARTESIAN_POINT ( 'NONE',  ( 194.8708600166808651, 293.1207648669033006, -14.79199694356877970 ) ) ;
#1228 = FACE_OUTER_BOUND ( 'NONE', #56169, .T. ) ;
#1229 = DIRECTION ( 'NONE',  ( -0.9515606131578174809, -0.3074612162317687525, 0.000000000000000000 ) ) ;
#1230 = CARTESIAN_POINT ( 'NONE',  ( 77.13133243787581250, 56.32679435582689109, -16.61903968960224276 ) ) ;
#1231 = CARTESIAN_POINT ( 'NONE',  ( 17.52119783388727825, 25.51421378149919050, -9.188101187500004485 ) ) ;
#1232 = CARTESIAN_POINT ( 'NONE',  ( 198.5175125801355023, 277.4849542247185923, -15.35271413496788284 ) ) ;
#1233 = CARTESIAN_POINT ( 'NONE',  ( 191.2828038517077687, 298.6283140572585921, -8.265843987895989287 ) ) ;
#1235 = VERTEX_POINT ( 'NONE', #433 ) ;
#1234 = CARTESIAN_POINT ( 'NONE',  ( 159.3169041484411537, 254.7020228407560580, 16.67170756419672628 ) ) ;
#1236 = CARTESIAN_POINT ( 'NONE',  ( 147.4638118793037336, 275.2321808777038541, -3.319864518316978597 ) ) ;
#1237 = CARTESIAN_POINT ( 'NONE',  ( 168.5649949959667424, 256.9588418996493715, -14.86446260810648567 ) ) ;
#1238 = CARTESIAN_POINT ( 'NONE',  ( 206.7408728089182546, 272.5612996242556960, -10.63134519248043475 ) ) ;
#1239 = DIRECTION ( 'NONE',  ( 0.5000000000000004441, -0.8660254037844383745, -0.000000000000000000 ) ) ;
#1240 = ADVANCED_FACE ( 'NONE', ( #61718 ), #29070, .T. ) ;
#1241 = CARTESIAN_POINT ( 'NONE',  ( 81.94105283978521470, 45.99306238629856836, -11.35642118984577742 ) ) ;
#1242 = CARTESIAN_POINT ( 'NONE',  ( 200.4403816905005158, 283.4740703539914648, 16.81798557643505987 ) ) ;
#1243 = EDGE_CURVE ( 'NONE', #60091, #33639, #89459, .T. ) ;
#1244 = CARTESIAN_POINT ( 'NONE',  ( 115.1800009256237729, 225.7592609112380160, 2.679491924311254714 ) ) ;
#1245 = ORIENTED_EDGE ( 'NONE', *, *, #53442, .T. ) ;
#1246 = CARTESIAN_POINT ( 'NONE',  ( 155.2417138354696817, 261.7604595133352063, -18.54054473025617966 ) ) ;
#1247 = VECTOR ( 'NONE', #98615, 1000.000000000000000 ) ;
#1248 = CARTESIAN_POINT ( 'NONE',  ( 128.6323578686148892, 256.6199935810940929, 2.679491924311251605 ) ) ;
#1249 = EDGE_CURVE ( 'NONE', #55525, #87546, #43781, .T. ) ;
#1250 = CARTESIAN_POINT ( 'NONE',  ( 141.9699493749754140, 259.7505386000626686, -7.968025677899344572 ) ) ;
#1251 = EDGE_CURVE ( 'NONE', #65280, #58155, #20847, .T. ) ;
#1252 = CARTESIAN_POINT ( 'NONE',  ( 14.65434579541627969, 179.2677522451418497, 10.00000000000009592 ) ) ;
#1253 = CARTESIAN_POINT ( 'NONE',  ( 94.11243691623624841, 215.9548013555409796, -4.594050593750042211 ) ) ;
#1254 = CARTESIAN_POINT ( 'NONE',  ( 82.12570432893160444, 40.77989999240937635, -1.063904901471852460 ) ) ;
#1255 = CARTESIAN_POINT ( 'NONE',  ( 174.6020076113873358, 282.3130386525841686, -14.36087153468174904 ) ) ;
#1256 = B_SPLINE_CURVE_WITH_KNOTS ( 'NONE', 3,
 ( #89072, #19623, #50977, #66193 ),
 .UNSPECIFIED., .F., .F.,
 ( 4, 4 ),
 ( 0.03792759114226184475, 0.04649815087312540729 ),
 .UNSPECIFIED. ) ;
#1257 = DIRECTION ( 'NONE',  ( -0.9054088711727240613, 0.4245406647209821749, 0.000000000000000000 ) ) ;
#1259 = CARTESIAN_POINT ( 'NONE',  ( 75.59751354683669433, 65.29851079375914935, 14.32525510856802065 ) ) ;
#1258 = CARTESIAN_POINT ( 'NONE',  ( 6.480970727150832111, 183.7369531367911009, -4.594050593750048428 ) ) ;
#1260 = CARTESIAN_POINT ( 'NONE',  ( 200.6129772034685175, 283.1751261563724142, 18.36811917402039640 ) ) ;
#1261 = EDGE_LOOP ( 'NONE', ( #21247, #73872, #79004, #53676 ) ) ;
#1262 = ORIENTED_EDGE ( 'NONE', *, *, #86789, .T. ) ;
#1263 = CARTESIAN_POINT ( 'NONE',  ( 147.7840666256145425, 276.6774833857293174, 0.9737628777943441172 ) ) ;
#1264 = CARTESIAN_POINT ( 'NONE',  ( 189.0469464145041911, 261.1622915045712148, -6.157471025067191128 ) ) ;
#1265 = CYLINDRICAL_SURFACE ( 'NONE', #17844, 10.00000000000001066 ) ;
#1266 = CARTESIAN_POINT ( 'NONE',  ( 33.48063555417975579, 19.73415679381824006, -6.890680421881970419E-14 ) ) ;
#1267 = CARTESIAN_POINT ( 'NONE',  ( 207.7320178805681508, 270.8445860024863237, -5.379955943374661764 ) ) ;
#1268 = CARTESIAN_POINT ( 'NONE',  ( 86.26382137438992004, 230.6115022471902876, -5.000000000000047962 ) ) ;
#1269 = CARTESIAN_POINT ( 'NONE',  ( 74.16736989203016606, 68.80940149631990721, -11.31408104362165545 ) ) ;
#1270 = CARTESIAN_POINT ( 'NONE',  ( 30.10766014385131939, 182.0643266524160424, 9.188101187500095079 ) ) ;
#1271 = CARTESIAN_POINT ( 'NONE',  ( 82.63733999249467388, 228.5177522451419350, 5.000000000000046185 ) ) ;
#1272 = AXIS2_PLACEMENT_3D ( 'NONE', #72427, #95248, #88660 ) ;
#1273 = CARTESIAN_POINT ( 'NONE',  ( 199.5360113197090186, 277.4446805320934004, 15.14791943599612445 ) ) ;
#1274 = ORIENTED_EDGE ( 'NONE', *, *, #51563, .T. ) ;
#1275 = CARTESIAN_POINT ( 'NONE',  ( 194.9499559406243918, 279.5747724307917679, 17.51673600049429780 ) ) ;
#1276 = CARTESIAN_POINT ( 'NONE',  ( 182.5651185885155598, 260.5800487877630758, -10.89712475207159592 ) ) ;
#1277 = CIRCLE ( 'NONE', #57894, 0.1418229129681557177 ) ;
#1278 = CARTESIAN_POINT ( 'NONE',  ( 151.2671975087473015, 270.6445237267302559, 14.15418255155509542 ) ) ;
#1279 = CARTESIAN_POINT ( 'NONE',  ( 157.1606030646430554, 258.4368458743103361, 17.96998724893680688 ) ) ;
#1280 = VECTOR ( 'NONE', #33335, 1000.000000000000227 ) ;
#1281 = DIRECTION ( 'NONE',  ( 0.8599083858334037878, -0.5104483989331242144, 0.000000000000000000 ) ) ;
#1282 = LINE ( 'NONE', #32166, #20635 ) ;
#1283 = CARTESIAN_POINT ( 'NONE',  ( 186.5814202129567434, 282.6718092406691767, 16.17431581196632706 ) ) ;
#1284 = CARTESIAN_POINT ( 'NONE',  ( 194.7576540903134799, 293.3168432830895540, -14.62421624641040196 ) ) ;
#1285 = CARTESIAN_POINT ( 'NONE',  ( 190.1907070792632624, 262.6060493502955637, 8.341994654895554362 ) ) ;
#1286 = CARTESIAN_POINT ( 'NONE',  ( 163.7239493340838123, 247.0687966679708438, 6.286946239157660266 ) ) ;
#1287 = CARTESIAN_POINT ( 'NONE',  ( 26.96143514339544467, 174.8262482093457777, 3.021315404115420679E-15 ) ) ;
#1288 = CARTESIAN_POINT ( 'NONE',  ( 69.81840073347110831, 69.95620362085875854, 5.184656770469231013 ) ) ;
#1289 = CARTESIAN_POINT ( 'NONE',  ( 147.7978300115112233, 274.6536445020713018, 7.902890709649431855 ) ) ;
#1290 = VERTEX_POINT ( 'NONE', #69581 ) ;
#1291 = FACE_OUTER_BOUND ( 'NONE', #71938, .T. ) ;
#1292 = AXIS2_PLACEMENT_3D ( 'NONE', #79941, #10501, #47984 ) ;
#1293 = CARTESIAN_POINT ( 'NONE',  ( 162.0012282828890022, 251.8624688453083422, -14.05248242572528738 ) ) ;
#1294 = CARTESIAN_POINT ( 'NONE',  ( 105.1810637865323628, 231.5333772461660828, 9.188101187500095079 ) ) ;
#1295 = CARTESIAN_POINT ( 'NONE',  ( 15.78795072819010770, 21.06628583063840665, -9.188101187500006262 ) ) ;
#1296 = LINE ( 'NONE', #61575, #47588 ) ;
#1297 = PLANE ( 'NONE',  #6369 ) ;
#1298 = VECTOR ( 'NONE', #47765, 1000.000000000000114 ) ;
#1300 = DIRECTION ( 'NONE',  ( 0.9616534368410327716, -0.2742675106749429270, 0.000000000000000000 ) ) ;
#1299 = CARTESIAN_POINT ( 'NONE',  ( 196.2609093297512857, 290.7131288316392670, 16.03897268885959448 ) ) ;
#1301 = CARTESIAN_POINT ( 'NONE',  ( 191.1669730766547275, 299.5360852325191559, -7.933564783864602177 ) ) ;
#1302 = CARTESIAN_POINT ( 'NONE',  ( 190.2490083984490354, 261.0793145204391976, -4.628088261293119565 ) ) ;
#1303 = DIRECTION ( 'NONE',  ( 0.2925570654631164946, 0.000000000000000000, 0.9562480658530033706 ) ) ;
#1304 = EDGE_CURVE ( 'NONE', #56569, #52500, #99009, .T. ) ;
#1305 = CARTESIAN_POINT ( 'NONE',  ( 46.95533697774293103, 209.4637435831424455, 2.679491924311303119 ) ) ;
#1306 = CARTESIAN_POINT ( 'NONE',  ( 146.9700173529739970, 276.0874580858064746, -5.099093031535578469 ) ) ;
#1307 = CARTESIAN_POINT ( 'NONE',  ( 86.22318085410130095, 47.68456650864125379, 10.79712569785469967 ) ) ;
#1308 = ORIENTED_EDGE ( 'NONE', *, *, #3460, .T. ) ;
#1309 = CARTESIAN_POINT ( 'NONE',  ( -22.42236680055709641, 157.8615022471902591, 0.000000000000000000 ) ) ;
#1310 = CARTESIAN_POINT ( 'NONE',  ( 75.53059436383961156, 63.11701598167661587, -15.26357697694628612 ) ) ;
#1311 = CARTESIAN_POINT ( 'NONE',  ( 199.9158968934949598, 270.1292180026705410, 9.240553224730840398 ) ) ;
#1312 = ORIENTED_EDGE ( 'NONE', *, *, #9305, .T. ) ;
#1313 = CARTESIAN_POINT ( 'NONE',  ( 72.06470348997973474, 72.25603645428108734, 1.367373202405260946 ) ) ;
#1314 = CARTESIAN_POINT ( 'NONE',  ( 79.30914410335456921, 50.55166203070548647, 14.90691090266632557 ) ) ;
#1316 = EDGE_CURVE ( 'NONE', #35809, #20300, #83330, .T. ) ;
#1315 = CARTESIAN_POINT ( 'NONE',  ( 180.9962514683335257, 255.6518059654043782, 5.281628127585873855 ) ) ;
#1317 = CARTESIAN_POINT ( 'NONE',  ( 183.2138347319267950, 296.5967044714456620, -4.168135968712713968 ) ) ;
#1318 = FACE_OUTER_BOUND ( 'NONE', #30711, .T. ) ;
#1319 = AXIS2_PLACEMENT_3D ( 'NONE', #28738, #47412, #55498 ) ;
#1320 = ORIENTED_EDGE ( 'NONE', *, *, #44937, .T. ) ;
#1321 = CARTESIAN_POINT ( 'NONE',  ( -86.81108781737714253, 15.00000000000000000, -9.212605237762131694 ) ) ;
#1322 = CARTESIAN_POINT ( 'NONE',  ( 41.28156676870083430, 26.76004757982093452, 5.678558825948272215 ) ) ;
#1323 = CARTESIAN_POINT ( 'NONE',  ( 86.25352412292622262, 43.32776165798921397, 4.621746443381918645 ) ) ;
#1324 = ORIENTED_EDGE ( 'NONE', *, *, #63685, .T. ) ;
#1325 = CARTESIAN_POINT ( 'NONE',  ( 165.6005443753849420, 279.9182785130287243, 11.76136245517345991 ) ) ;
#1326 = ADVANCED_FACE ( 'NONE', ( #76214 ), #13894, .T. ) ;
#1327 = PLANE ( 'NONE',  #96927 ) ;
#1328 = CARTESIAN_POINT ( 'NONE',  ( 82.55913317860365908, 44.02162453438392475, -9.665417050538319899 ) ) ;
#1329 = ORIENTED_EDGE ( 'NONE', *, *, #21958, .F. ) ;
#1330 = CARTESIAN_POINT ( 'NONE',  ( 86.50330892798304205, 47.09883604031134752, -10.56546389670383235 ) ) ;
#1331 = CARTESIAN_POINT ( 'NONE',  ( 134.6192181478005523, 236.9824982072973967, 3.021315404115420679E-15 ) ) ;
#1332 = CARTESIAN_POINT ( 'NONE',  ( 163.7729086741176161, 246.9839966035275438, 6.099406794390714204 ) ) ;
#1333 = CARTESIAN_POINT ( 'NONE',  ( 38.19908180566553568, 96.33262850695970769, 59.99999999999999289 ) ) ;
#1334 = DIRECTION ( 'NONE',  ( -0.1344185706417126702, 0.9909246428798905715, 0.000000000000000000 ) ) ;
#1335 = FACE_OUTER_BOUND ( 'NONE', #59028, .T. ) ;
#1336 = ORIENTED_EDGE ( 'NONE', *, *, #16346, .T. ) ;
#1337 = ORIENTED_EDGE ( 'NONE', *, *, #6609, .F. ) ;
#1338 = CARTESIAN_POINT ( 'NONE',  ( 175.4214522509338678, 258.5208151414564668, 13.04691889165856011 ) ) ;
#1339 = ORIENTED_EDGE ( 'NONE', *, *, #72669, .F. ) ;
#1340 = DIRECTION ( 'NONE',  ( -0.8660254037844379305, -0.5000000000000014433, -0.000000000000000000 ) ) ;
#1341 = VERTEX_POINT ( 'NONE', #60468 ) ;
#1342 = CARTESIAN_POINT ( 'NONE',  ( 173.3891276806938322, 270.4835184475072651, 17.26558241125811222 ) ) ;
#1343 = CARTESIAN_POINT ( 'NONE',  ( 78.63827745602966957, 50.59572098740068924, 15.06237687010368909 ) ) ;
#1344 = ORIENTED_EDGE ( 'NONE', *, *, #90823, .F. ) ;
#1345 = CARTESIAN_POINT ( 'NONE',  ( 182.7854418666322545, 280.3108875730028444, -16.10961360330436065 ) ) ;
#1346 = CARTESIAN_POINT ( 'NONE',  ( 164.2877295051262934, 246.0923007674255416, -1.726861278304287373 ) ) ;
#1347 = CARTESIAN_POINT ( 'NONE',  ( 147.5830093564496224, 275.0257247911527543, -7.422490571551428218 ) ) ;
#1348 = CARTESIAN_POINT ( 'NONE',  ( 186.1630411436486554, 296.9614825196608194, -7.488375694256206749 ) ) ;
#1349 = CARTESIAN_POINT ( 'NONE',  ( 79.47185235748389687, 46.29617394947011633, 12.66262444679482257 ) ) ;
#1350 = AXIS2_PLACEMENT_3D ( 'NONE', #58082, #80942, #42854 ) ;
#1351 = CARTESIAN_POINT ( 'NONE',  ( 167.6436438581388870, 249.1749608028844705, -5.378307912567069415 ) ) ;
#1352 = CARTESIAN_POINT ( 'NONE',  ( 76.90746743093833970, 62.93938289886319382, -15.23233999435671215 ) ) ;
#1354 = CARTESIAN_POINT ( 'NONE',  ( 154.0314627544081816, 279.5640916383285912, 2.169601216685385303 ) ) ;
#1353 = VECTOR ( 'NONE', #63954, 1000.000000000000000 ) ;
#1355 = CARTESIAN_POINT ( 'NONE',  ( 129.5380282679697075, 245.5958772461660544, -9.188101187500095079 ) ) ;
#1356 = CARTESIAN_POINT ( 'NONE',  ( 186.6422722926715778, 262.8257398156653153, -9.173408779546029734 ) ) ;
#1357 = VECTOR ( 'NONE', #24801, 1000.000000000000114 ) ;
#1358 = ORIENTED_EDGE ( 'NONE', *, *, #76601, .F. ) ;
#1359 = AXIS2_PLACEMENT_3D ( 'NONE', #81029, #56669, #96213 ) ;
#1361 = VERTEX_POINT ( 'NONE', #15363 ) ;
#1360 = CARTESIAN_POINT ( 'NONE',  ( 82.07993970318088373, 43.40442941875307525, -9.247700843510214597 ) ) ;
#1362 = DIRECTION ( 'NONE',  ( -0.2588190451025239591, -0.9659258262890673130, -6.568581106066860352E-16 ) ) ;
#1363 = EDGE_CURVE ( 'NONE', #22179, #13198, #68582, .T. ) ;
#1364 = CARTESIAN_POINT ( 'NONE',  ( 180.8417871952999860, 256.1704575049583354, 0.9644184763862307941 ) ) ;
#1365 = CARTESIAN_POINT ( 'NONE',  ( 174.3162989310297633, 290.4431585964500755, -4.830845372109453528 ) ) ;
#1366 = CARTESIAN_POINT ( 'NONE',  ( 192.2537778369132582, 297.6536841698438138, 12.51786810291793550 ) ) ;
#1367 = CARTESIAN_POINT ( 'NONE',  ( 71.78650793969821109, 60.87908065824935022, 14.79100780097532919 ) ) ;
#1368 = DIRECTION ( 'NONE',  ( 0.9481851146622169990, 0.3177184104407523302, 0.000000000000000000 ) ) ;
#1369 = CARTESIAN_POINT ( 'NONE',  ( 79.51266829831004657, 58.44199966345352948, 16.61175003844716258 ) ) ;
#1370 = CARTESIAN_POINT ( 'NONE',  ( 153.6596595523362794, 266.9882342533689439, 16.60685250298524807 ) ) ;
#1371 = DIRECTION ( 'NONE',  ( -0.000000000000000000, 0.000000000000000000, 1.000000000000000000 ) ) ;
#1372 =( BOUNDED_CURVE ( )  B_SPLINE_CURVE ( 1, ( #51079, #12106 ),
 .UNSPECIFIED., .F., .T. ) 
 B_SPLINE_CURVE_WITH_KNOTS ( ( 2, 2 ),
 ( 0.000000000000000000, 0.0003750000000000086272 ),
 .UNSPECIFIED. ) 
 CURVE ( )  GEOMETRIC_REPRESENTATION_ITEM ( )  RATIONAL_B_SPLINE_CURVE ( ( 0.9368410486966849415, 0.9368410486966849415 ) ) 
 REPRESENTATION_ITEM ( '' )  );
#1373 = ORIENTED_EDGE ( 'NONE', *, *, #91745, .T. ) ;
#1374 = CARTESIAN_POINT ( 'NONE',  ( 194.5252985417586729, 293.7192948986070178, -14.54632727629426370 ) ) ;
#1375 = CARTESIAN_POINT ( 'NONE',  ( 65.78143134570771622, 69.10410598619917266, -0.2546738380904993160 ) ) ;
#1376 = VERTEX_POINT ( 'NONE', #59470 ) ;
#1377 = EDGE_CURVE ( 'NONE', #70239, #29279, #92426, .T. ) ;
#1378 = CARTESIAN_POINT ( 'NONE',  ( 191.0752600067845037, 266.8597520346529564, -12.80755884565359892 ) ) ;
#1379 = EDGE_CURVE ( 'NONE', #37194, #36369, #53381, .T. ) ;
#1380 = VECTOR ( 'NONE', #44212, 1000.000000000000000 ) ;
#1381 = CARTESIAN_POINT ( 'NONE',  ( 160.2722201351343472, 278.9910888498445729, 10.57498524561427367 ) ) ;
#1382 = CARTESIAN_POINT ( 'NONE',  ( 151.9042993347139827, 267.5410309945612539, -16.88973072590943403 ) ) ;
#1383 = CARTESIAN_POINT ( 'NONE',  ( 190.7862358025146534, 300.1955415356651429, 3.573119809004446257 ) ) ;
#1384 = CARTESIAN_POINT ( 'NONE',  ( 204.7544901219449969, 272.8412540040631029, -10.83433605784845355 ) ) ;
#1386 = CARTESIAN_POINT ( 'NONE',  ( 160.8742158466989736, 281.6452003631559364, 6.228587064600521472 ) ) ;
#1385 = CARTESIAN_POINT ( 'NONE',  ( 152.9741103202414081, 270.0357790464439063, 14.04803099111643760 ) ) ;
#1387 = CARTESIAN_POINT ( 'NONE',  ( 152.6621968174709991, 266.2283140474973493, -17.02835521334403168 ) ) ;
#1388 = ORIENTED_EDGE ( 'NONE', *, *, #48703, .F. ) ;
#1389 = CARTESIAN_POINT ( 'NONE',  ( 190.2648877593310317, 301.0985428348857340, -4.426259207433023590 ) ) ;
#1390 = B_SPLINE_SURFACE_WITH_KNOTS ( 'NONE', 3, 1, ( 
 ( #13898, #71857 ),
 ( #79977, #98016 ),
 ( #41420, #36683 ),
 ( #67592, #59475 ),
 ( #80483, #34336 ),
 ( #2970, #2454 ),
 ( #33336, #96176 ),
 ( #70074, #45771 ),
 ( #83837, #37190 ),
 ( #100010, #91940 ),
 ( #22493, #6299 ),
 ( #39161, #84828 ),
 ( #30595, #22978 ),
 ( #14881, #61481 ),
 ( #7286, #689 ),
 ( #77710, #99510 ),
 ( #85334, #61964 ),
 ( #6795, #30094 ),
 ( #31571, #23982 ),
 ( #76219, #62463 ),
 ( #46265, #84336 ),
 ( #8296, #15367 ),
 ( #68092, #93429 ),
 ( #99013, #76693 ),
 ( #92431, #29600 ),
 ( #60472, #69085 ),
 ( #46790, #54879 ),
 ( #91429, #37676 ),
 ( #92917, #85860 ),
 ( #15877, #68587 ),
 ( #45285, #44778 ),
 ( #53867, #54361 ),
 ( #77186, #75714 ),
 ( #21992, #69583 ) ),
 .UNSPECIFIED., .T., .F., .F.,
 ( 4, 2, 2, 2, 2, 2, 2, 2, 2, 2, 2, 2, 2, 2, 2, 2, 4 ),
 ( 2, 2 ),
 ( 0.000000000000000000, 0.06250000000000000000, 0.1250000000000000000, 0.1875000000000000000, 0.2500000000000000000, 0.3125000000000000000, 0.3750000000000000000, 0.4375000000000000000, 0.5000000000000000000, 0.5625000000000000000, 0.6250000000000000000, 0.6875000000000000000, 0.7500000000000000000, 0.8125000000000000000, 0.8750000000000000000, 0.9375000000000000000, 1.000000000000000000 ),
 ( 0.000000000000000000, 1.000000000000000000 ),
 .UNSPECIFIED. ) ;
#1391 = CARTESIAN_POINT ( 'NONE',  ( 73.54766422090952460, 64.98954179014701538, 13.85985167941228546 ) ) ;
#1392 = CARTESIAN_POINT ( 'NONE',  ( 128.5366863930700276, 235.0177522451417929, 5.000000000000051514 ) ) ;
#1393 = CARTESIAN_POINT ( 'NONE',  ( 196.0587100571994483, 289.0633482449420626, -17.27351923437598913 ) ) ;
#1394 = CARTESIAN_POINT ( 'NONE',  ( 199.1713105229414964, 278.4797133870983430, -16.65774537300400837 ) ) ;
#1395 = CARTESIAN_POINT ( 'NONE',  ( 74.07459009150333884, 68.62600853808264389, 11.43350474783683879 ) ) ;
#1396 = CARTESIAN_POINT ( 'NONE',  ( 193.9204722154232741, 294.7668848255750049, 15.43855698596013859 ) ) ;
#1397 = CARTESIAN_POINT ( 'NONE',  ( 68.42167172887349125, 70.09380820080993146, 1.014016391010813978 ) ) ;
#1398 = AXIS2_PLACEMENT_3D ( 'NONE', #5621, #66429, #99340 ) ;
#1399 = CARTESIAN_POINT ( 'NONE',  ( -12.00317221093202136, 170.0024278399160949, 9.188101187500095079 ) ) ;
#1400 = CARTESIAN_POINT ( 'NONE',  ( 84.42325706775034178, 228.7369531367911293, -4.594050593750048428 ) ) ;
#1401 = CARTESIAN_POINT ( 'NONE',  ( 66.81833236730544456, 68.44078315879002616, 5.955615777142785561 ) ) ;
#1402 = CARTESIAN_POINT ( 'NONE',  ( 146.7944005049231180, 276.3916353892955726, -4.243051111306586520 ) ) ;
#1403 = CARTESIAN_POINT ( 'NONE',  ( 182.7907705717913416, 294.2845485110142363, -8.010541978009545261 ) ) ;
#1404 = B_SPLINE_CURVE_WITH_KNOTS ( 'NONE', 3,
 ( #51844, #89875, #97463, #67524, #6224, #81777, #42715, #73650, #37120, #43720, #4230, #51321, #82288, #13349 ),
 .UNSPECIFIED., .F., .F.,
 ( 4, 2, 2, 2, 2, 2, 4 ),
 ( 8.079268757097385768E-15, 0.0005064305305122302706, 0.001012861061016381284, 0.001266076326268456790, 0.001519291591520532296, 0.001772506856772607803, 0.002025722122024683526 ),
 .UNSPECIFIED. ) ;
#1405 = CARTESIAN_POINT ( 'NONE',  ( 78.11592650351285272, 47.71665711652420327, 14.50685932715414239 ) ) ;
#1406 = VECTOR ( 'NONE', #11738, 1000.000000000000000 ) ;
#1407 = CARTESIAN_POINT ( 'NONE',  ( 78.06834474603437002, 54.98730760881699098, 16.09275306223789315 ) ) ;
#1408 = SURFACE_STYLE_FILL_AREA ( #85550 ) ;
#1409 = CARTESIAN_POINT ( 'NONE',  ( 77.85473067527519220, 62.02510648819682615, 15.65027994488795215 ) ) ;
#1411 = CARTESIAN_POINT ( 'NONE',  ( 76.06974868155622005, 51.35906999481754553, 15.65069530268658404 ) ) ;
#1410 = CARTESIAN_POINT ( 'NONE',  ( 67.05596152584389813, 66.86776152947172136, 8.884023177476819910 ) ) ;
#1412 = CARTESIAN_POINT ( 'NONE',  ( 161.9966032734278940, 250.0606478072812706, 13.86476480043075199 ) ) ;
#1413 = CARTESIAN_POINT ( 'NONE',  ( 192.1779685593947420, 266.1842805242176269, 11.64530923862864142 ) ) ;
#1414 = CARTESIAN_POINT ( 'NONE',  ( 161.5601416284384584, 251.9944088100220085, 13.91020052908825733 ) ) ;
#1415 = LINE ( 'NONE', #87069, #9047 ) ;
#1416 = CARTESIAN_POINT ( 'NONE',  ( 71.65180518398884146, 72.09936778357817388, 3.358463432740978138 ) ) ;
#1417 = CARTESIAN_POINT ( 'NONE',  ( 161.2133744761260061, 251.4172398781588811, -14.30368667312104058 ) ) ;
#1418 = CARTESIAN_POINT ( 'NONE',  ( 39.09232661234986494, 199.5024278399160664, -9.188101187500093303 ) ) ;
#1419 = CARTESIAN_POINT ( 'NONE',  ( 75.81765026128996965, 205.3923013555409796, 4.594050593750050204 ) ) ;
#1420 = LINE ( 'NONE', #1917, #15890 ) ;
#1421 = CARTESIAN_POINT ( 'NONE',  ( 88.37445845132181432, 44.20200228399612286, 0.05334810252746784165 ) ) ;
#1422 = AXIS2_PLACEMENT_3D ( 'NONE', #52734, #21363, #76084 ) ;
#1423 = CARTESIAN_POINT ( 'NONE',  ( 96.31878499345593525, 237.9637435831424739, 2.679491924311251605 ) ) ;
#1425 = CARTESIAN_POINT ( 'NONE',  ( 77.48284268753138804, 49.21606489196949497, 15.29539255787453911 ) ) ;
#1424 = CARTESIAN_POINT ( 'NONE',  ( 198.2912749888956512, 286.5204237852628353, -17.12625248512345166 ) ) ;
#1426 = AXIS2_PLACEMENT_3D ( 'NONE', #48202, #77624, #47685 ) ;
#1427 = CARTESIAN_POINT ( 'NONE',  ( 196.5306890327151734, 269.6898905632888273, -10.81324570519863748 ) ) ;
#1428 = EDGE_CURVE ( 'NONE', #28142, #18551, #60972, .T. ) ;
#1429 = CARTESIAN_POINT ( 'NONE',  ( 29.91980124543643171, 22.98920272979927759, 7.433330006724137462 ) ) ;
#1430 = CARTESIAN_POINT ( 'NONE',  ( 198.4522155198218059, 286.9176751754968109, -17.57438352224490075 ) ) ;
#1431 = CARTESIAN_POINT ( 'NONE',  ( 81.84538571332693380, 47.30605694451114829, -12.45174469400575035 ) ) ;
#1432 = CARTESIAN_POINT ( 'NONE',  ( 8.584303441219292452, 23.14336893147753571, 7.433330006724141015 ) ) ;
#1433 = CARTESIAN_POINT ( 'NONE',  ( 65.88516108981343677, 208.8458772461660544, 9.188101187500095079 ) ) ;
#1434 = PLANE ( 'NONE',  #38359 ) ;
#1435 = CARTESIAN_POINT ( 'NONE',  ( 203.2369479875374623, 278.6302754407888074, -16.66242713208754367 ) ) ;
#1436 = VECTOR ( 'NONE', #17514, 1000.000000000000000 ) ;
#1437 = CARTESIAN_POINT ( 'NONE',  ( 197.8822014719394531, 287.9049684674569676, 17.88172308374019792 ) ) ;
#1438 = DIRECTION ( 'NONE',  ( 1.000000000000000000, 0.000000000000000000, 0.000000000000000000 ) ) ;
#1439 = CARTESIAN_POINT ( 'NONE',  ( 153.8601318185219782, 264.1534297615118021, 16.57777867432794139 ) ) ;
#1440 = ADVANCED_FACE ( 'NONE', ( #52883 ), #76689, .T. ) ;
#1441 = CARTESIAN_POINT ( 'NONE',  ( 76.78612666066324266, 56.27578982940967478, -16.16415727311750672 ) ) ;
#1442 = AXIS2_PLACEMENT_3D ( 'NONE', #13783, #67983, #44661 ) ;
#1443 = CARTESIAN_POINT ( 'NONE',  ( 104.4503548538631890, 231.1115022471902307, 10.00000000000009592 ) ) ;
#1444 = CARTESIAN_POINT ( 'NONE',  ( 200.9111546617170916, 282.6586676490145464, 17.66063511622358106 ) ) ;
#1445 = CARTESIAN_POINT ( 'NONE',  ( 207.4826643481121664, 271.2764789897469768, 7.783310782367018454 ) ) ;
#1446 = ORIENTED_EDGE ( 'NONE', *, *, #13820, .F. ) ;
#1447 = CARTESIAN_POINT ( 'NONE',  ( 77.68170011982932976, 49.37347120871703510, 15.31094863473072998 ) ) ;
#1448 = CARTESIAN_POINT ( 'NONE',  ( 185.8974605661406940, 271.6370272364711127, 16.87882237039100275 ) ) ;
#1449 = ORIENTED_EDGE ( 'NONE', *, *, #86391, .F. ) ;
#1450 = CARTESIAN_POINT ( 'NONE',  ( 159.8732321751776624, 253.7384344327741132, -15.51998349828054202 ) ) ;
#1451 = CARTESIAN_POINT ( 'NONE',  ( 189.2360998237118963, 278.0599140720760829, -16.51445267049493282 ) ) ;
#1452 = EDGE_CURVE ( 'NONE', #483, #4766, #99437, .T. ) ;
#1453 = CARTESIAN_POINT ( 'NONE',  ( 72.78091084507063613, 68.76417989200491832, -9.950453267798913259 ) ) ;
#1454 = ORIENTED_EDGE ( 'NONE', *, *, #94923, .T. ) ;
#1455 = CARTESIAN_POINT ( 'NONE',  ( -42.18579364100346396, 26.51648975995176372, -10.00000000000000000 ) ) ;
#1456 = VERTEX_POINT ( 'NONE', #82843 ) ;
#1457 = CARTESIAN_POINT ( 'NONE',  ( 72.44040225518423881, 71.75621485965102408, 5.770394931239938963 ) ) ;
#1458 = CARTESIAN_POINT ( 'NONE',  ( 162.7595241543376972, 265.1439861438755088, -17.82152945942356226 ) ) ;
#1459 = VECTOR ( 'NONE', #70154, 1000.000000000000227 ) ;
#1460 = EDGE_LOOP ( 'NONE', ( #77178, #31949, #62735, #10441 ) ) ;
#1461 = CARTESIAN_POINT ( 'NONE',  ( 28.30082151474694285, 24.84335787977763843, 9.188101187500006262 ) ) ;
#1462 = CARTESIAN_POINT ( 'NONE',  ( -27.42236680055714260, 166.5217562850347406, 1.224646799147364892E-15 ) ) ;
#1463 = CARTESIAN_POINT ( 'NONE',  ( 75.25625879159228759, 66.47192257091543865, -13.14164885170834829 ) ) ;
#1464 = CARTESIAN_POINT ( 'NONE',  ( 83.51651814802133345, 48.25154606481438435, -12.48491116408185242 ) ) ;
#1465 = ORIENTED_EDGE ( 'NONE', *, *, #2974, .T. ) ;
#1466 = DIRECTION ( 'NONE',  ( -0.000000000000000000, 0.000000000000000000, -1.000000000000000000 ) ) ;
#1467 = ADVANCED_FACE ( 'NONE', ( #100006 ), #21020, .T. ) ;
#1468 = LINE ( 'NONE', #48042, #82103 ) ;
#1469 = EDGE_LOOP ( 'NONE', ( #89103, #33769, #36814, #35601 ) ) ;
#1470 = CARTESIAN_POINT ( 'NONE',  ( 171.2347629857892457, 284.6507891007374269, 10.77592557674535279 ) ) ;
#1472 = CARTESIAN_POINT ( 'NONE',  ( 67.95004079286472631, 65.25863045202757462, -10.56757888573983273 ) ) ;
#1471 = CARTESIAN_POINT ( 'NONE',  ( 68.17803913764699075, 65.49435412443665427, 10.45721739836550945 ) ) ;
#1473 = CARTESIAN_POINT ( 'NONE',  ( -19.65312891409030271, 93.06504152958497400, 10.00000000000000888 ) ) ;
#1474 = CARTESIAN_POINT ( 'NONE',  ( 155.5204415533959548, 261.2776889444089647, 17.19127227448963424 ) ) ;
#1475 = CARTESIAN_POINT ( 'NONE',  ( 185.3860032077430162, 292.5766161388369255, -10.74141587811191911 ) ) ;
#1476 = CARTESIAN_POINT ( 'NONE',  ( 157.1269483542914998, 258.4951375425532092, -17.15328932028234377 ) ) ;
#1477 = CARTESIAN_POINT ( 'NONE',  ( 134.1114646098825176, 257.4244531367911577, -4.594050593750046652 ) ) ;
#1478 = CARTESIAN_POINT ( 'NONE',  ( 205.3498812800093276, 270.0116018477241369, 2.442032521302731851 ) ) ;
#1479 = DIRECTION ( 'NONE',  ( -0.4805540241036398430, -0.8769651246872923744, 0.000000000000000000 ) ) ;
#1480 = CARTESIAN_POINT ( 'NONE',  ( 93.67942421434402434, 215.7048013555409796, 4.594050593750051981 ) ) ;
#1481 = ORIENTED_EDGE ( 'NONE', *, *, #81998, .F. ) ;
#1482 = CARTESIAN_POINT ( 'NONE',  ( 151.4281781455628675, 268.3656970847310390, 15.24742929158552585 ) ) ;
#1483 = CARTESIAN_POINT ( 'NONE',  ( 78.14988184308933228, 61.89697373328141339, -16.07278474554906467 ) ) ;
#1484 = ORIENTED_EDGE ( 'NONE', *, *, #28389, .T. ) ;
#1485 = CARTESIAN_POINT ( 'NONE',  ( 182.7264905230827878, 296.4309396610331078, 3.745374670362856762 ) ) ;
#1486 = ORIENTED_EDGE ( 'NONE', *, *, #95684, .F. ) ;
#1487 = ORIENTED_EDGE ( 'NONE', *, *, #98535, .T. ) ;
#1488 = EDGE_CURVE ( 'NONE', #43189, #82089, #98518, .T. ) ;
#1489 = CARTESIAN_POINT ( 'NONE',  ( 80.02629435240551459, 44.46182459010558574, -11.62687173039730304 ) ) ;
#1490 = CARTESIAN_POINT ( 'NONE',  ( 146.6834825911944620, 276.5837508513432681, 0.6716460511724984261 ) ) ;
#1491 = CARTESIAN_POINT ( 'NONE',  ( 81.20643963274024202, 55.68550677472633481, 16.38154045842715334 ) ) ;
#1492 = CARTESIAN_POINT ( 'NONE',  ( 171.9695299662907360, 276.3046275190319534, -16.98996149290084645 ) ) ;
#1493 = CARTESIAN_POINT ( 'NONE',  ( 207.5603179267596374, 271.1419790461399089, 2.162348062361596490 ) ) ;
#1494 = CARTESIAN_POINT ( 'NONE',  ( 81.04025856027610075, 229.8464784336661353, 1.353441290958777327E-15 ) ) ;
#1495 = ORIENTED_EDGE ( 'NONE', *, *, #73193, .T. ) ;
#1496 = EDGE_CURVE ( 'NONE', #63991, #3825, #52387, .T. ) ;
#1497 = EDGE_LOOP ( 'NONE', ( #50090, #79860, #594, #87888 ) ) ;
#1498 = CARTESIAN_POINT ( 'NONE',  ( 162.9111474110223412, 248.4766108952035211, -9.702990628959184960 ) ) ;
#1499 = VECTOR ( 'NONE', #42114, 1000.000000000000000 ) ;
#1500 = EDGE_LOOP ( 'NONE', ( #32127, #61385, #61163, #87761 ) ) ;
#1501 = AXIS2_PLACEMENT_3D ( 'NONE', #64077, #39737, #47853 ) ;
#1502 = ADVANCED_FACE ( 'NONE', ( #1704 ), #40670, .T. ) ;
#1503 = CARTESIAN_POINT ( 'NONE',  ( 75.81625539762656274, 65.12695345013474935, -14.47344923651660054 ) ) ;
#1504 = CARTESIAN_POINT ( 'NONE',  ( 19.15050853525752927, 34.55466486950700045, 7.012934429366973338E-14 ) ) ;
#1505 = CARTESIAN_POINT ( 'NONE',  ( 162.2205785505892948, 283.9195354534895728, 0.5141653453796740658 ) ) ;
#1506 = CARTESIAN_POINT ( 'NONE',  ( 186.2214199329484074, 263.1771180729978710, -12.06840420414929937 ) ) ;
#1507 = CARTESIAN_POINT ( 'NONE',  ( 87.82600437409995209, 44.28008912978396694, 4.743525404917309451 ) ) ;
#1508 = ORIENTED_EDGE ( 'NONE', *, *, #88243, .F. ) ;
#1509 = CARTESIAN_POINT ( 'NONE',  ( 84.86869520348948015, 43.75225087683188718, -6.313702690781472171 ) ) ;
#1510 = EDGE_CURVE ( 'NONE', #25763, #18263, #85329, .T. ) ;
#1511 = CARTESIAN_POINT ( 'NONE',  ( 185.1628174925895678, 260.2253205732822039, 6.313110411375027375 ) ) ;
#1512 = CARTESIAN_POINT ( 'NONE',  ( 206.3423291502491566, 273.2515974901050413, -10.76717883871977577 ) ) ;
#1513 = EDGE_CURVE ( 'NONE', #39405, #4020, #94422, .T. ) ;
#1514 = CARTESIAN_POINT ( 'NONE',  ( 199.3359313799735162, 277.8054090533971134, 16.38672730308284997 ) ) ;
#1515 = CARTESIAN_POINT ( 'NONE',  ( 174.6702674810315159, 283.6871151125846495, 13.51636394462591895 ) ) ;
#1516 = CARTESIAN_POINT ( 'NONE',  ( -22.42236680055709641, 157.8615022471902591, 0.000000000000000000 ) ) ;
#1517 = CARTESIAN_POINT ( 'NONE',  ( -4.164184202058353712, 36.47075635815506445, 59.99999999999999289 ) ) ;
#1518 = ORIENTED_EDGE ( 'NONE', *, *, #11686, .T. ) ;
#1519 = CARTESIAN_POINT ( 'NONE',  ( -2.408111037970082968, 180.9637435831425307, 2.679491924311264039 ) ) ;
#1520 = VECTOR ( 'NONE', #88040, 1000.000000000000114 ) ;
#1521 = CARTESIAN_POINT ( 'NONE',  ( 161.1884843536000744, 251.4603508349806873, 13.21272898143761942 ) ) ;
#1522 = DIRECTION ( 'NONE',  ( 0.8660254037844377084, 0.5000000000000015543, 0.000000000000000000 ) ) ;
#1523 = CARTESIAN_POINT ( 'NONE',  ( 171.6205452999947738, 251.3949250676056977, 7.279205862586061393 ) ) ;
#1524 = CARTESIAN_POINT ( 'NONE',  ( 198.8472845770790229, 265.6353728642903889, 1.646580097172975155 ) ) ;
#1525 = CARTESIAN_POINT ( 'NONE',  ( 177.2779740990669666, 290.8998969752722701, -6.149525471840052937 ) ) ;
#1526 = CARTESIAN_POINT ( 'NONE',  ( 153.4465587549918837, 270.2984085571182504, 14.02096340496593108 ) ) ;
#1527 = ORIENTED_EDGE ( 'NONE', *, *, #76895, .F. ) ;
#1528 = FACE_OUTER_BOUND ( 'NONE', #61023, .T. ) ;
#1529 = B_SPLINE_CURVE_WITH_KNOTS ( 'NONE', 3,
 ( #96845, #49698, #64407, #3141, #26909, #50685, #4601, #80651, #87781, #27413, #66398, #72019, #97325, #19817, #11229, #48719, #3621, #18317, #42095, #89268, #79650, #80149, #10715, #10216 ),
 .UNSPECIFIED., .F., .F.,
 ( 4, 2, 2, 2, 2, 2, 2, 2, 2, 2, 2, 4 ),
 ( 0.0002170125375182288085, 0.0007842342920218860289, 0.001067845169273751692, 0.001138747888586716644, 0.001174199248243124093, 0.001209650607899531542, 0.001245101967555938991, 0.001280553327212346441, 0.001351456046525128813, 0.001918677801027586635, 0.002202288678278833435, 0.002485899555530080886 ),
 .UNSPECIFIED. ) ;
#1530 = VECTOR ( 'NONE', #96037, 1000.000000000000000 ) ;
#1531 = CARTESIAN_POINT ( 'NONE',  ( 76.21540257404608099, 63.22959166649816609, -14.98001016604830937 ) ) ;
#1533 = CARTESIAN_POINT ( 'NONE',  ( 73.83419370605903964, 55.14121766272175051, 16.60004764102358976 ) ) ;
#1532 = CARTESIAN_POINT ( 'NONE',  ( 180.6402368737672646, 266.9317641007265252, -14.80827112732728779 ) ) ;
#1534 = LINE ( 'NONE', #95271, #4496 ) ;
#1535 = CARTESIAN_POINT ( 'NONE',  ( 34.63914548426571827, 22.12755873383627758, -6.180339887498949025 ) ) ;
#1536 = CARTESIAN_POINT ( 'NONE',  ( 170.0966408101324703, 273.6447761240920613, 15.99755975640291084 ) ) ;
#1537 = CARTESIAN_POINT ( 'NONE',  ( 163.3213225887255078, 283.7535443778070317, -3.395488904438747735 ) ) ;
#1538 = CARTESIAN_POINT ( 'NONE',  ( -19.65312891409030271, 93.06504152958497400, -20.00000000000000355 ) ) ;
#1539 = CARTESIAN_POINT ( 'NONE',  ( 188.8136734414513001, 259.8025127425751180, 3.692511016432421744 ) ) ;
#1540 = CARTESIAN_POINT ( 'NONE',  ( 194.8451752635450021, 266.1831273802821443, -7.490151361129687935 ) ) ;
#1541 = CARTESIAN_POINT ( 'NONE',  ( 2.557053438076354990, 172.2833772461660828, -9.188101187500095079 ) ) ;
#1542 = DIRECTION ( 'NONE',  ( 0.7467472232290855993, 0.000000000000000000, 0.6651079495838628786 ) ) ;
#1543 = VERTEX_POINT ( 'NONE', #85856 ) ;
#1544 = CARTESIAN_POINT ( 'NONE',  ( 160.2740869459746023, 254.0686150970925610, -15.36085255641610914 ) ) ;
#1545 = LINE ( 'NONE', #8630, #17652 ) ;
#1546 = CARTESIAN_POINT ( 'NONE',  ( 81.38228331512368641, 42.18052851754683275, 8.075145019496558163 ) ) ;
#1547 = CARTESIAN_POINT ( 'NONE',  ( 198.7501991201633018, 286.4015524398827779, -18.58948563601804693 ) ) ;
#1548 = CARTESIAN_POINT ( 'NONE',  ( 24.58674819472551931, 178.8768266524160140, 9.188101187500096856 ) ) ;
#1549 = FACE_OUTER_BOUND ( 'NONE', #81417, .T. ) ;
#1550 = CARTESIAN_POINT ( 'NONE',  ( 32.81602777569660390, 24.11029122506295863, -8.090169943749478065 ) ) ;
#1551 = CARTESIAN_POINT ( 'NONE',  ( 180.8890834033174713, 294.3766012452771861, 6.559837412958372305 ) ) ;
#1552 = CARTESIAN_POINT ( 'NONE',  ( 191.8000917695741805, 298.4394914891611847, -9.452573400474340914 ) ) ;
#1553 = CARTESIAN_POINT ( 'NONE',  ( 12.29081813446918758, 171.2365022471902023, -10.00000000000009237 ) ) ;
#1554 = CARTESIAN_POINT ( 'NONE',  ( 81.86130692232174511, 42.15755783746833885, 7.590521390274829194 ) ) ;
#1555 = CARTESIAN_POINT ( 'NONE',  ( 87.17901322616850734, 46.26306768054848817, -8.477718022526687491 ) ) ;
#1556 = CARTESIAN_POINT ( 'NONE',  ( 187.5517675740670427, 259.2187753813501558, -0.7877570970383018789 ) ) ;
#1557 = CARTESIAN_POINT ( 'NONE',  ( 192.9518127100452034, 296.0217619941561793, -12.12386602825073645 ) ) ;
#1558 = CARTESIAN_POINT ( 'NONE',  ( 63.31414817410230000, 217.3615022471903160, 5.000000000000046185 ) ) ;
#1559 = CARTESIAN_POINT ( 'NONE',  ( 72.05627613218693739, 66.49406252133579187, -11.67341081358113009 ) ) ;
#1560 = CARTESIAN_POINT ( 'NONE',  ( 185.5756359364698085, 277.7569889279997142, -17.43085986457148806 ) ) ;
#1561 = CYLINDRICAL_SURFACE ( 'NONE', #75770, 10.00000000000010658 ) ;
#1562 = CARTESIAN_POINT ( 'NONE',  ( 29.86365662933068066, 197.2369531367911293, -4.594050593750048428 ) ) ;
#1563 = CARTESIAN_POINT ( 'NONE',  ( 159.2077906806335932, 254.8910129107889588, 16.14624949541834553 ) ) ;
#1564 = CARTESIAN_POINT ( 'NONE',  ( 77.21724311172287969, 49.67724645580758391, -14.99754053603360759 ) ) ;
#1565 = CARTESIAN_POINT ( 'NONE',  ( 198.7829547491859330, 286.3448180261817129, -18.59838968157616179 ) ) ;
#1566 = EDGE_CURVE ( 'NONE', #78218, #96180, #31528, .T. ) ;
#1568 = FACE_OUTER_BOUND ( 'NONE', #50419, .T. ) ;
#1567 = AXIS2_PLACEMENT_3D ( 'NONE', #41270, #32183, #47869 ) ;
#1569 = ORIENTED_EDGE ( 'NONE', *, *, #56933, .F. ) ;
#1570 = CARTESIAN_POINT ( 'NONE',  ( 89.31526421587503251, 210.8262482093457777, 3.021315404115420679E-15 ) ) ;
#1571 = LINE ( 'NONE', #30084, #19936 ) ;
#1572 = CARTESIAN_POINT ( 'NONE',  ( 162.8121824534329107, 280.4967882457603423, -9.952098035278266863 ) ) ;
#1573 = CARTESIAN_POINT ( 'NONE',  ( 205.7045377653668936, 269.1581673421392793, -1.349048711920618926 ) ) ;
#1574 = CARTESIAN_POINT ( 'NONE',  ( 23.25741983583088413, 25.37878583063841376, 9.188101187500006262 ) ) ;
#1575 = CARTESIAN_POINT ( 'NONE',  ( 203.0337691736598629, 278.9821914694464340, 16.08167820133810011 ) ) ;
#1576 = CARTESIAN_POINT ( 'NONE',  ( 149.6191398986701415, 271.4990432411842676, -11.66821883946526839 ) ) ;
#1577 = CARTESIAN_POINT ( 'NONE',  ( 186.1808859727878485, 268.2690591356716823, -14.28216311553996754 ) ) ;
#1578 = VERTEX_POINT ( 'NONE', #33085 ) ;
#1579 = CIRCLE ( 'NONE', #89003, 70.00000000000001421 ) ;
#1580 = CARTESIAN_POINT ( 'NONE',  ( 12.27453364332850505, 12.80170272979924739, 7.433330006724137462 ) ) ;
#1581 = CARTESIAN_POINT ( 'NONE',  ( 75.89814051312130516, 58.95594745416783411, -15.95455651496020444 ) ) ;
#1582 = CARTESIAN_POINT ( 'NONE',  ( 71.79363655647949827, 72.51690322118082577, -1.318798153274830076 ) ) ;
#1583 = EDGE_CURVE ( 'NONE', #75006, #51318, #47275, .T. ) ;
#1584 = ORIENTED_EDGE ( 'NONE', *, *, #68260, .F. ) ;
#1585 = CARTESIAN_POINT ( 'NONE',  ( 32.15758756610207314, 177.8262482093457777, 3.021315404115420679E-15 ) ) ;
#1586 = CARTESIAN_POINT ( 'NONE',  ( -22.42236680055709641, 157.8615022471902591, 0.000000000000000000 ) ) ;
#1587 = DIRECTION ( 'NONE',  ( 0.5000000000000003331, -0.8660254037844384856, 0.000000000000000000 ) ) ;
#1588 = ADVANCED_FACE ( 'NONE', ( #86345 ), #63107, .F. ) ;
#1589 = CARTESIAN_POINT ( 'NONE',  ( 180.8238942241078178, 257.6885452376805574, -7.457973117650044337 ) ) ;
#1590 = CARTESIAN_POINT ( 'NONE',  ( 190.0607312434325138, 301.4521522931182176, 3.538147641957853473 ) ) ;
#1591 = VERTEX_POINT ( 'NONE', #34580 ) ;
#1592 = VERTEX_POINT ( 'NONE', #42660 ) ;
#1594 = CARTESIAN_POINT ( 'NONE',  ( -167.0327448629461742, 42.61639673982678289, 21.50000000000000000 ) ) ;
#1593 = CARTESIAN_POINT ( 'NONE',  ( 189.6631063493766760, 274.4263583876541475, -15.75412945656347041 ) ) ;
#1595 = ORIENTED_EDGE ( 'NONE', *, *, #6391, .T. ) ;
#1596 = CARTESIAN_POINT ( 'NONE',  ( 200.6737073311291795, 283.0699384897140476, -17.61533935526990291 ) ) ;
#1597 = CARTESIAN_POINT ( 'NONE',  ( 71.80779569229208903, 72.11915028389421423, -3.640749997624285417 ) ) ;
#1598 = CARTESIAN_POINT ( 'NONE',  ( 72.95919681002737889, 57.42441093631072846, -15.86686462681733900 ) ) ;
#1599 = FACE_OUTER_BOUND ( 'NONE', #7023, .T. ) ;
#1600 = CARTESIAN_POINT ( 'NONE',  ( 204.6470611188870521, 276.1878878528713130, -13.02652554726987866 ) ) ;
#1601 = B_SPLINE_CURVE_WITH_KNOTS ( 'NONE', 3,
 ( #2491, #88138, #64277, #3972, #56156, #87151, #33373, #49083, #10585, #17683, #48583, #1984, #65270, #18684, #19202, #72906, #86633, #80016 ),
 .UNSPECIFIED., .F., .F.,
 ( 4, 2, 2, 1, 2, 2, 2, 2, 1, 4 ),
 ( 0.000000000000000000, 0.1185760491640068387, 0.1482200614550078510, 0.1778640737460088217, 0.2371520983280109851, 0.2964401229100130930, 0.3557281474920152564, 0.3853721597830173096, 0.4150161720740193072, 0.4743041966560226363 ),
 .UNSPECIFIED. ) ;
#1602 = CARTESIAN_POINT ( 'NONE',  ( 100.2557178503908517, 222.5643266524160140, 9.188101187500095079 ) ) ;
#1603 = AXIS2_PLACEMENT_3D ( 'NONE', #71225, #8410, #94542 ) ;
#1604 = CARTESIAN_POINT ( 'NONE',  ( 182.1881639437997933, 287.6810548547900908, -13.22834577702405490 ) ) ;
#1605 = ORIENTED_EDGE ( 'NONE', *, *, #70139, .T. ) ;
#1606 = CARTESIAN_POINT ( 'NONE',  ( 164.4578252119609090, 245.7976863610386999, -6.211333091911165560 ) ) ;
#1607 = ORIENTED_EDGE ( 'NONE', *, *, #96781, .F. ) ;
#1608 = CARTESIAN_POINT ( 'NONE',  ( 21.45803809350889679, 35.49540643055188127, 3.479690158560446702E-15 ) ) ;
#1609 = FACE_OUTER_BOUND ( 'NONE', #99954, .T. ) ;
#1610 = CARTESIAN_POINT ( 'NONE',  ( 78.58598452914725385, 47.91960314448038361, -14.47352538085859486 ) ) ;
#1612 = VECTOR ( 'NONE', #92271, 1000.000000000000114 ) ;
#1611 = CARTESIAN_POINT ( 'NONE',  ( 63.88265089144443465, 201.5643266524160140, 9.188101187500095079 ) ) ;
#1613 = CARTESIAN_POINT ( 'NONE',  ( 73.93840856004327122, 68.59252082510937498, 10.89217114877860659 ) ) ;
#1614 = CARTESIAN_POINT ( 'NONE',  ( 150.6431064791187850, 269.7254810985950257, 15.11064854015152470 ) ) ;
#1615 = DIRECTION ( 'NONE',  ( 0.000000000000000000, 0.000000000000000000, 1.000000000000000000 ) ) ;
#1616 = CARTESIAN_POINT ( 'NONE',  ( 176.5838317420758870, 273.2463210208075566, 17.06958482087071260 ) ) ;
#1617 = EDGE_LOOP ( 'NONE', ( #74533, #9087, #40422 ) ) ;
#1618 = ADVANCED_FACE ( 'NONE', ( #89819 ), #64994, .T. ) ;
#1619 = CARTESIAN_POINT ( 'NONE',  ( 183.1426684129219780, 267.5694331394444703, -16.03671021927237206 ) ) ;
#1620 = CARTESIAN_POINT ( 'NONE',  ( 146.9376205018946848, 276.1435710778808925, 5.066564108429441937 ) ) ;
#1621 = CARTESIAN_POINT ( 'NONE',  ( 20.94141239725287917, 35.71947554534623492, -10.00000000000000000 ) ) ;
#1622 = EDGE_LOOP ( 'NONE', ( #48162, #99884, #64854, #38345 ) ) ;
#1623 = CARTESIAN_POINT ( 'NONE',  ( 175.2696475750532841, 261.2817613914389767, -14.26110703076659902 ) ) ;
#1624 = LINE ( 'NONE', #53298, #100278 ) ;
#1625 = CARTESIAN_POINT ( 'NONE',  ( 146.5068495316331791, 276.8896882847997176, 0.02371565180376856638 ) ) ;
#1626 = CARTESIAN_POINT ( 'NONE',  ( 192.9523350703175311, 296.4437475495926719, -13.35611922184540923 ) ) ;
#1627 = EDGE_CURVE ( 'NONE', #8540, #35319, #15977, .T. ) ;
#1628 = EDGE_CURVE ( 'NONE', #64662, #76974, #18907, .T. ) ;
#1629 = CARTESIAN_POINT ( 'NONE',  ( 149.1903793729515257, 272.2416782560088677, 12.95958987445043675 ) ) ;
#1630 = CARTESIAN_POINT ( 'NONE',  ( 179.7358607235859438, 270.8417515334642189, 16.28888456289437414 ) ) ;
#1631 = CARTESIAN_POINT ( 'NONE',  ( 205.7829192689729325, 274.2205238267313234, 11.21202327925415254 ) ) ;
#1632 = CARTESIAN_POINT ( 'NONE',  ( 75.85858666007513307, 65.60472725796547877, 13.84649109559921420 ) ) ;
#1633 = CARTESIAN_POINT ( 'NONE',  ( 72.92312356590035449, 64.99263871788808444, -13.11958098651873250 ) ) ;
#1634 = CARTESIAN_POINT ( 'NONE',  ( 208.3135187673106543, 269.8373969220020285, 2.829653198597726682 ) ) ;
#1635 = CARTESIAN_POINT ( 'NONE',  ( 104.4229444624559733, 243.3464784336661353, 1.353441290958777327E-15 ) ) ;
#1636 = ORIENTED_EDGE ( 'NONE', *, *, #79163, .F. ) ;
#1637 = CARTESIAN_POINT ( 'NONE',  ( 147.2229325088103735, 275.6493961858936927, -0.4918294119671829390 ) ) ;
#1638 = EDGE_CURVE ( 'NONE', #76591, #63991, #42174, .T. ) ;
#1639 = EDGE_CURVE ( 'NONE', #18415, #51452, #44648, .T. ) ;
#1640 = LINE ( 'NONE', #9219, #16588 ) ;
#1641 = CARTESIAN_POINT ( 'NONE',  ( 192.1146148663661393, 296.2687097199236632, 12.34145616421383984 ) ) ;
#1642 = CARTESIAN_POINT ( 'NONE',  ( 83.70956241415673560, 51.66838590121233210, -14.83800726304596118 ) ) ;
#1643 = CARTESIAN_POINT ( 'NONE',  ( 178.0719526903251619, 255.3558746966477315, 4.708485374109758759 ) ) ;
#1644 = VERTEX_POINT ( 'NONE', #91305 ) ;
#1645 = CARTESIAN_POINT ( 'NONE',  ( 162.6396274730868186, 248.9468972229755082, -10.26162218571527518 ) ) ;
#1646 = CARTESIAN_POINT ( 'NONE',  ( 157.9704523343261258, 276.0272599195727707, -12.71455051359169808 ) ) ;
#1647 = CARTESIAN_POINT ( 'NONE',  ( 182.2170977436522605, 260.5581375984304486, 9.500862743582350944 ) ) ;
#1648 = CARTESIAN_POINT ( 'NONE',  ( 74.66818547213321722, 67.01009517369644186, 12.98877810528427013 ) ) ;
#1649 = CARTESIAN_POINT ( 'NONE',  ( 119.6866422041566551, 252.1589784336661069, -6.496448406907676862E-16 ) ) ;
#1650 = CARTESIAN_POINT ( 'NONE',  ( 151.0013883899287066, 269.1049186256390726, -14.25461351222133466 ) ) ;
#1651 = PLANE ( 'NONE',  #2903 ) ;
#1652 = CARTESIAN_POINT ( 'NONE',  ( 189.9224218318563260, 282.6927222767778858, -16.57155747260814849 ) ) ;
#1653 = PLANE ( 'NONE',  #7779 ) ;
#1654 = CARTESIAN_POINT ( 'NONE',  ( 45.88512659934279014, 206.4869531367911009, 4.594050593750046652 ) ) ;
#1655 = CARTESIAN_POINT ( 'NONE',  ( 85.67021663899103601, 48.38166113680176750, -11.71697781433778651 ) ) ;
#1656 = CARTESIAN_POINT ( 'NONE',  ( 88.06181012395556706, 44.63806904432505007, -4.156701318329214523 ) ) ;
#1657 = CARTESIAN_POINT ( 'NONE',  ( 80.12748291632911446, 44.63541364795098332, -11.72772784125804080 ) ) ;
#1658 = CARTESIAN_POINT ( 'NONE',  ( 172.6568878728820948, 261.0847548073755320, 14.48626931307794763 ) ) ;
#1659 = CARTESIAN_POINT ( 'NONE',  ( 82.28509353309422636, 41.51255840690875232, -5.852911540032354587 ) ) ;
#1660 = CARTESIAN_POINT ( 'NONE',  ( 178.8759581903709943, 291.7429665371036549, -6.258367371696258452 ) ) ;
#1661 = CARTESIAN_POINT ( 'NONE',  ( 92.14326550588401687, 235.5530062829863027, -4.648177544792955347E-16 ) ) ;
#1662 = CARTESIAN_POINT ( 'NONE',  ( 154.5654453936281811, 269.4902856693395279, -15.08148675096953717 ) ) ;
#1663 = CARTESIAN_POINT ( 'NONE',  ( 115.9793180381956148, 237.7677522451418497, 10.00000000000009592 ) ) ;
#1664 = B_SPLINE_SURFACE_WITH_KNOTS ( 'NONE', 3, 1, ( 
 ( #78285, #14961 ),
 ( #70666, #32165 ),
 ( #63069, #94012 ),
 ( #47849, #40254 ),
 ( #71194, #1787 ),
 ( #53463, #45849 ),
 ( #7365, #38250 ),
 ( #65072, #96021 ),
 ( #95019, #26584 ),
 ( #79818, #3783 ),
 ( #80833, #33689 ),
 ( #4263, #10887 ),
 ( #57457, #65567 ),
 ( #49373, #88951 ),
 ( #80316, #64074 ),
 ( #35162, #72709 ),
 ( #64583, #19506 ),
 ( #18488, #73189 ),
 ( #34665, #3299 ),
 ( #95535, #66072 ),
 ( #88436, #48884 ),
 ( #17471, #41763 ),
 ( #81317, #25582 ),
 ( #50363, #2294 ),
 ( #11888, #34178 ),
 ( #18997, #25065 ),
 ( #9894, #26083 ),
 ( #55941, #2802 ),
 ( #49872, #33174 ),
 ( #72195, #11401 ),
 ( #56468, #86939 ) ),
 .UNSPECIFIED., .F., .F., .F.,
 ( 4, 3, 3, 3, 3, 3, 3, 3, 3, 3, 4 ),
 ( 2, 2 ),
 ( 0.000000000000000000, 0.1122669598086777770, 0.2243161639709639332, 0.3396355846219138996, 0.4553962076585105212, 0.5677860799922255230, 0.6749047109689485513, 0.7773884377078289498, 0.8775581155834147884, 0.9782364162377931160, 1.000000000000000000 ),
 ( 0.000000000000000000, 1.000000000000000000 ),
 .UNSPECIFIED. ) ;
#1665 = CARTESIAN_POINT ( 'NONE',  ( 78.86766380650875874, 52.46362257666628182, -15.56641557883455818 ) ) ;
#1666 = ORIENTED_EDGE ( 'NONE', *, *, #83634, .F. ) ;
#1667 = EDGE_CURVE ( 'NONE', #92124, #12322, #84217, .T. ) ;
#1668 = CARTESIAN_POINT ( 'NONE',  ( 202.8499463704053198, 279.3005819042728604, 17.04674939340617001 ) ) ;
#1669 = CARTESIAN_POINT ( 'NONE',  ( 87.74913801566610516, 44.74219947183942026, 5.012341453613225362 ) ) ;
#1670 = CARTESIAN_POINT ( 'NONE',  ( 21.77181853666109745, 189.5024278399160949, 9.188101187500095079 ) ) ;
#1671 = CARTESIAN_POINT ( 'NONE',  ( 20.42956747364522485, 12.76426979415089313, 3.090169943749476733 ) ) ;
#1672 = CARTESIAN_POINT ( 'NONE',  ( 82.54166851694979812, 206.9155109091895781, 2.679491924311254714 ) ) ;
#1673 = DIRECTION ( 'NONE',  ( 0.4140345431502788220, 0.9102611697080897901, 0.000000000000000000 ) ) ;
#1674 = LINE ( 'NONE', #94391, #78214 ) ;
#1676 = CARTESIAN_POINT ( 'NONE',  ( 60.19284827774804114, 198.8927522451417929, -10.00000000000009059 ) ) ;
#1675 = CARTESIAN_POINT ( 'NONE',  ( 12.36470590445056317, 8.108019796199268825, 3.090169943749476733 ) ) ;
#1677 = CARTESIAN_POINT ( 'NONE',  ( 173.6627686280932039, 288.1531483176477764, 7.554607035878428967 ) ) ;
#1678 = CARTESIAN_POINT ( 'NONE',  ( 163.1218343930725894, 256.2508100442478849, -16.13596270478102923 ) ) ;
#1679 = FACE_OUTER_BOUND ( 'NONE', #67932, .T. ) ;
#1680 = CARTESIAN_POINT ( 'NONE',  ( 66.76293781782166548, 68.40909042380869209, -4.422493503458938768 ) ) ;
#1681 =( BOUNDED_CURVE ( )  B_SPLINE_CURVE ( 2, ( #41156, #50264, #34092, #96411, #26979, #96917, #48791, #34568, #56365 ),
 .UNSPECIFIED., .F., .T. ) 
 B_SPLINE_CURVE_WITH_KNOTS ( ( 3, 2, 2, 2, 3 ),
 ( 0.5201612903225806273, 0.5215053763440860024, 0.5241935483870967527, 0.5268817204301075030, 0.5282258064516128782 ),
 .UNSPECIFIED. ) 
 CURVE ( )  GEOMETRIC_REPRESENTATION_ITEM ( )  RATIONAL_B_SPLINE_CURVE ( ( 0.9330127018922194093, 0.9330127018922194093, 1.000000000000000000, 0.8660254037844387076, 1.000000000000000000, 0.8660254037844387076, 1.000000000000000000, 0.9330127018922194093, 0.9330127018922194093 ) ) 
 REPRESENTATION_ITEM ( '' )  );
#1682 = ORIENTED_EDGE ( 'NONE', *, *, #28240, .T. ) ;
#1683 = CARTESIAN_POINT ( 'NONE',  ( 30.33301404664501888, 174.9865022471901739, 1.119607411625061291E-15 ) ) ;
#1684 = CARTESIAN_POINT ( 'NONE',  ( 141.5809337175232940, 261.7369531367911009, -4.594050593750048428 ) ) ;
#1685 = CARTESIAN_POINT ( 'NONE',  ( 162.8996025780091941, 248.4966071325470125, 11.23567065566008516 ) ) ;
#1686 = CARTESIAN_POINT ( 'NONE',  ( 150.1064787036151245, 245.2202760586659736, -5.415160957724236172E-17 ) ) ;
#1687 = CARTESIAN_POINT ( 'NONE',  ( 41.60632629512001301, 26.94754757982092741, 5.678558825948272215 ) ) ;
#1689 = CARTESIAN_POINT ( 'NONE',  ( 170.5027933921127214, 263.5424279318320941, 15.79580204150556710 ) ) ;
#1688 = DIRECTION ( 'NONE',  ( 0.000000000000000000, 0.000000000000000000, 1.000000000000000000 ) ) ;
#1690 = CARTESIAN_POINT ( 'NONE',  ( 190.5297895243285211, 290.4239949136141377, -15.76409704461241290 ) ) ;
#1691 = CARTESIAN_POINT ( 'NONE',  ( 31.79857739925353499, 98.44139654353648439, 59.99999999999999289 ) ) ;
#1692 = EDGE_CURVE ( 'NONE', #25829, #86364, #82436, .T. ) ;
#1693 = CARTESIAN_POINT ( 'NONE',  ( 183.4288420069315180, 257.9430297361450926, -2.297013850620948983 ) ) ;
#1694 = CARTESIAN_POINT ( 'NONE',  ( 66.05284405871212527, 69.03255062257417762, 2.566972579851455993 ) ) ;
#1695 = EDGE_LOOP ( 'NONE', ( #50576, #69212, #82002, #45259 ) ) ;
#1696 = CARTESIAN_POINT ( 'NONE',  ( -0.2492734796364602656, 27.10516647459198225, -10.00000000000000000 ) ) ;
#1697 = SHAPE_REPRESENTATION_RELATIONSHIP ( 'NONE' , 'NONE' ,  #46310, #3033 ) ;
#1698 = CARTESIAN_POINT ( 'NONE',  ( 150.3237008197049249, 246.0494855054051868, -2.679491924311248496 ) ) ;
#1699 = CARTESIAN_POINT ( 'NONE',  ( 153.3157916388551882, 277.7051378986778900, -5.233164379718747483 ) ) ;
#1700 = CARTESIAN_POINT ( 'NONE',  ( 11.45782370926791849, 18.56628583063839244, 9.188101187500006262 ) ) ;
#1701 = CARTESIAN_POINT ( 'NONE',  ( 160.6498352449959555, 252.3933184585345657, 15.68867965355669192 ) ) ;
#1702 = CARTESIAN_POINT ( 'NONE',  ( 206.8106726053982811, 272.4404028303941914, -10.47827087991598560 ) ) ;
#1703 = EDGE_CURVE ( 'NONE', #82896, #73620, #37671, .T. ) ;
#1704 = FACE_OUTER_BOUND ( 'NONE', #98531, .T. ) ;
#1705 = CARTESIAN_POINT ( 'NONE',  ( 82.29453827371126806, 224.9865022471902876, -10.00000000000009592 ) ) ;
#1706 = CARTESIAN_POINT ( 'NONE',  ( 93.72070878210261924, 236.4637435831425023, 2.679491924311251605 ) ) ;
#1707 = EDGE_CURVE ( 'NONE', #24773, #78854, #42513, .T. ) ;
#1708 = CARTESIAN_POINT ( 'NONE',  ( 207.6555576926778883, 270.9770189326688410, -1.235081510489080436 ) ) ;
#1709 = CARTESIAN_POINT ( 'NONE',  ( 193.7275870247597425, 295.1009717758319084, 14.48058678254265885 ) ) ;
#1710 = ORIENTED_EDGE ( 'NONE', *, *, #10635, .F. ) ;
#1711 = ORIENTED_EDGE ( 'NONE', *, *, #9867, .F. ) ;
#1712 = CARTESIAN_POINT ( 'NONE',  ( 155.8328110275561187, 276.9913226184394830, -10.28370083813354263 ) ) ;
#1713 = CARTESIAN_POINT ( 'NONE',  ( 86.11363163537949106, 47.05074959952599301, 10.74854466831323840 ) ) ;
#1714 = ORIENTED_EDGE ( 'NONE', *, *, #95099, .F. ) ;
#1715 = CARTESIAN_POINT ( 'NONE',  ( 20.44744908501035496, 27.50829794293880681, -10.00000000000000355 ) ) ;
#1716 = CARTESIAN_POINT ( 'NONE',  ( 27.76992210170819675, 43.29297894285233639, -10.00000000000000000 ) ) ;
#1717 = VERTEX_POINT ( 'NONE', #76574 ) ;
#1718 = CARTESIAN_POINT ( 'NONE',  ( 146.5310397537613483, 276.8477895910274356, -0.2793038414862049068 ) ) ;
#1719 = CARTESIAN_POINT ( 'NONE',  ( 78.96380797632822635, 59.43460744216078950, -16.52597720501997358 ) ) ;
#1720 = B_SPLINE_CURVE_WITH_KNOTS ( 'NONE', 3,
 ( #31253, #17055, #62140, #71282 ),
 .UNSPECIFIED., .F., .F.,
 ( 4, 4 ),
 ( 0.003189740795969862874, 0.006687314450048887672 ),
 .UNSPECIFIED. ) ;
#1721 = B_SPLINE_CURVE_WITH_KNOTS ( 'NONE', 3,
 ( #38117, #44236, #53821, #52839, #69035, #99962, #61432, #36639, #92385, #67045, #68046, #83788, #22933, #5748, #98475, #29068, #47724, #8251, #8743, #38630, #54316, #33037, #78659, #39613, #85286, #48242, #16835, #94380, #2158, #92873, #77664, #24444, #63937, #15831, #46736, #39116, #47237, #9247, #24934, #69541, #644, #56328, #32026, #23426, #61923, #62935 ),
 .UNSPECIFIED., .F., .F.,
 ( 4, 2, 2, 2, 2, 2, 2, 2, 2, 2, 2, 2, 2, 2, 2, 2, 2, 2, 2, 2, 2, 2, 4 ),
 ( 0.0004469933677433058803, 0.001460477987537453677, 0.001967220297434580430, 0.002093905874908885429, 0.002220591452383190428, 0.002347277029857495426, 0.002473962607331800859, 0.002727333762280489352, 0.002980704917229178279, 0.003487447227126506261, 0.004500931846921240286, 0.005514416466715974310, 0.006021158776613377318, 0.006274529931562079256, 0.006527901086510781194, 0.006591243875247919382, 0.006654586663985056702, 0.006717929452722194890, 0.006781272241459332210, 0.007034643396407847665, 0.007541385706304846483, 0.008048128016201843565, 0.008554870326098843250 ),
 .UNSPECIFIED. ) ;
#1722 = B_SPLINE_CURVE_WITH_KNOTS ( 'NONE', 3,
 ( #93645, #23686, #24210, #69304 ),
 .UNSPECIFIED., .F., .F.,
 ( 4, 4 ),
 ( 0.008780835828182721042, 0.01389840247672927999 ),
 .UNSPECIFIED. ) ;
#1723 = CARTESIAN_POINT ( 'NONE',  ( 149.3253462891332219, 272.0079086998416074, -12.99539319630191336 ) ) ;
#1724 = CARTESIAN_POINT ( 'NONE',  ( 20.43632886220093070, 13.92755873383625698, 6.180339887498953466 ) ) ;
#1725 = VERTEX_POINT ( 'NONE', #61355 ) ;
#1726 = CARTESIAN_POINT ( 'NONE',  ( 200.6129772034685175, 283.1751261563724142, 18.36811917402039640 ) ) ;
#1727 = CARTESIAN_POINT ( 'NONE',  ( 6.396987757676594555, 15.64441083166260427, 0.000000000000000000 ) ) ;
#1728 = CARTESIAN_POINT ( 'NONE',  ( 150.6431064791187850, 269.7254810985950257, 15.11064854015152470 ) ) ;
#1729 = CARTESIAN_POINT ( 'NONE',  ( 34.97582608256301739, 32.14441083166263979, 10.00000000000000533 ) ) ;
#1730 = ORIENTED_EDGE ( 'NONE', *, *, #38874, .F. ) ;
#1731 = CARTESIAN_POINT ( 'NONE',  ( 3.854092266844447501, 28.45370138451379560, 10.00000000000000000 ) ) ;
#1732 = CARTESIAN_POINT ( 'NONE',  ( 163.4216610345155800, 247.5923753613567442, 10.58669027323842826 ) ) ;
#1733 = VERTEX_POINT ( 'NONE', #59861 ) ;
#1734 = VERTEX_POINT ( 'NONE', #21866 ) ;
#1735 = CARTESIAN_POINT ( 'NONE',  ( 73.34097623508702668, 61.15009553395870512, 15.04177895589568337 ) ) ;
#1736 = ORIENTED_EDGE ( 'NONE', *, *, #93576, .T. ) ;
#1737 = DIRECTION ( 'NONE',  ( -0.000000000000000000, -0.000000000000000000, -1.000000000000000000 ) ) ;
#1738 = ORIENTED_EDGE ( 'NONE', *, *, #62645, .F. ) ;
#1739 = ADVANCED_FACE ( 'NONE', ( #30463 ), #38042, .T. ) ;
#1740 = CARTESIAN_POINT ( 'NONE',  ( 82.34639549499804900, 46.43828254362050956, 11.54952222346724966 ) ) ;
#1741 = CARTESIAN_POINT ( 'NONE',  ( 71.58674681710026277, 69.69452789951117211, 7.786173541551400845 ) ) ;
#1742 = CARTESIAN_POINT ( 'NONE',  ( 147.8505793332463725, 274.5622799967613332, -9.317516487097901035 ) ) ;
#1743 = CARTESIAN_POINT ( 'NONE',  ( 174.9090629387510205, 290.7237071972734270, 6.492599126899565753 ) ) ;
#1744 = CARTESIAN_POINT ( 'NONE',  ( -9.181706736895311138, 177.0530062829863027, -4.648177544792955347E-16 ) ) ;
#1745 = ORIENTED_EDGE ( 'NONE', *, *, #19548, .F. ) ;
#1746 = CARTESIAN_POINT ( 'NONE',  ( 162.0192538899617318, 268.0510789565263394, -17.53028463913764057 ) ) ;
#1747 = CARTESIAN_POINT ( 'NONE',  ( 22.57541804695699028, 15.96004757982090183, -5.678558825948276656 ) ) ;
#1748 = CARTESIAN_POINT ( 'NONE',  ( 206.0627831668701901, 273.7357853363691902, 10.14454147593459687 ) ) ;
#1749 = CARTESIAN_POINT ( 'NONE',  ( 164.4494343874829099, 245.8122196953522121, 2.922779519406129456 ) ) ;
#1751 = ORIENTED_EDGE ( 'NONE', *, *, #46900, .F. ) ;
#1750 = CARTESIAN_POINT ( 'NONE',  ( 194.7576052748250390, 276.3294723641358246, -16.78574826228364714 ) ) ;
#1752 = CARTESIAN_POINT ( 'NONE',  ( 159.5180972751518595, 279.0588588540967976, -11.03979334413982016 ) ) ;
#1753 = CYLINDRICAL_SURFACE ( 'NONE', #31801, 10.00000000000010658 ) ;
#1754 = ADVANCED_FACE ( 'NONE', ( #98395 ), #22860, .F. ) ;
#1755 = CARTESIAN_POINT ( 'NONE',  ( 206.4484807199597753, 273.0677375780628608, -9.220527398138528952 ) ) ;
#1756 = LINE ( 'NONE', #79786, #92698 ) ;
#1757 = CARTESIAN_POINT ( 'NONE',  ( 200.8828793852583203, 282.7076418644388696, 17.90302398138411633 ) ) ;
#1758 = LINE ( 'NONE', #32637, #38511 ) ;
#1759 = VERTEX_POINT ( 'NONE', #6673 ) ;
#1760 = CARTESIAN_POINT ( 'NONE',  ( 194.4041250891751247, 293.9291734750100886, -14.17881196554796119 ) ) ;
#1761 = CARTESIAN_POINT ( 'NONE',  ( 125.9182562534771677, 255.0530062829863311, -4.648177544792955347E-16 ) ) ;
#1762 = FACE_OUTER_BOUND ( 'NONE', #78352, .T. ) ;
#1763 = CARTESIAN_POINT ( 'NONE',  ( 22.01556172758404628, 173.5177522451417929, 5.000000000000051514 ) ) ;
#1764 = CARTESIAN_POINT ( 'NONE',  ( 88.48327179163739231, 212.7048013555409796, 4.594050593750051981 ) ) ;
#1765 = CARTESIAN_POINT ( 'NONE',  ( 82.46956611399556891, 40.45592067260756863, -1.389944151191353505 ) ) ;
#1766 = DIRECTION ( 'NONE',  ( -0.9182972510888883777, 0.3958915996110437541, 0.000000000000000000 ) ) ;
#1767 = CARTESIAN_POINT ( 'NONE',  ( 208.1583869480885483, 270.1060931147653719, 3.025867354224990979 ) ) ;
#1768 = EDGE_CURVE ( 'NONE', #70878, #65992, #27919, .T. ) ;
#1770 = CARTESIAN_POINT ( 'NONE',  ( 75.94843506473843320, 65.47918399976401815, 14.33637728062728556 ) ) ;
#1769 = CARTESIAN_POINT ( 'NONE',  ( 6.400214715252306341, 168.3768266524160140, 9.188101187500098632 ) ) ;
#1771 = CARTESIAN_POINT ( 'NONE',  ( 161.8289209813647176, 250.3510820566641257, 13.28523796267037937 ) ) ;
#1772 = EDGE_LOOP ( 'NONE', ( #89350, #83464, #66589, #34713 ) ) ;
#1774 = EDGE_LOOP ( 'NONE', ( #22497, #18781, #42916, #60250, #80866, #21666, #96508 ) ) ;
#1773 = UNCERTAINTY_MEASURE_WITH_UNIT (LENGTH_MEASURE( 1.000000000000000082E-05 ), #86839, 'distance_accuracy_value', 'NONE');
#1775 = CARTESIAN_POINT ( 'NONE',  ( 200.7721129302025247, 267.7114073205713112, -2.857155443757144031 ) ) ;
#1776 = CARTESIAN_POINT ( 'NONE',  ( 69.34433977682154193, 70.64122323216504640, 0.8389772499948148221 ) ) ;
#1777 = CARTESIAN_POINT ( 'NONE',  ( 26.33642183074452703, 30.90829794293881960, 10.00000000000000355 ) ) ;
#1778 = CARTESIAN_POINT ( 'NONE',  ( 82.35975313173908319, 41.41624149291901347, 5.521678208619407613 ) ) ;
#1779 = CARTESIAN_POINT ( 'NONE',  ( 82.23066470189330346, 42.55849650999721945, 6.877359557377351607 ) ) ;
#1780 = DIRECTION ( 'NONE',  ( 0.000000000000000000, 0.000000000000000000, -1.000000000000000000 ) ) ;
#1781 = CARTESIAN_POINT ( 'NONE',  ( 43.58535403812915376, 183.7202760586659451, -5.415160957724236172E-17 ) ) ;
#1782 = CARTESIAN_POINT ( 'NONE',  ( 200.0154776055639445, 276.6224788825257974, 15.58692471366793519 ) ) ;
#1783 = ORIENTED_EDGE ( 'NONE', *, *, #22842, .T. ) ;
#1784 = CARTESIAN_POINT ( 'NONE',  ( 150.0080822439343535, 271.6737539543675553, -11.69383360110748526 ) ) ;
#1785 = CARTESIAN_POINT ( 'NONE',  ( 173.8805019302338621, 250.6242863632701585, 0.4030408839048176262 ) ) ;
#1786 = CARTESIAN_POINT ( 'NONE',  ( -15.08856125979659346, 174.3464784336661353, 1.353441290958777327E-15 ) ) ;
#1787 = CARTESIAN_POINT ( 'NONE',  ( 68.78537064792701017, 63.83817091373786212, -12.21312428423394536 ) ) ;
#1788 = CARTESIAN_POINT ( 'NONE',  ( 191.3843761966370209, 282.8631020262318430, -17.76976768207862278 ) ) ;
#1789 = DIRECTION ( 'NONE',  ( -0.5803476755362181327, -0.8143688203140567738, 0.000000000000000000 ) ) ;
#1790 = CARTESIAN_POINT ( 'NONE',  ( 148.4083960970861256, 273.5961130204771052, -8.574185186226726429 ) ) ;
#1791 = CARTESIAN_POINT ( 'NONE',  ( 186.0715527847238207, 298.7753624933060337, 1.084710433360843940 ) ) ;
#1792 = CARTESIAN_POINT ( 'NONE',  ( 204.4325665793906524, 276.5594032932251594, 13.33817701435311598 ) ) ;
#1793 = CARTESIAN_POINT ( 'NONE',  ( 147.2937583206075942, 275.5267222813735088, 0.1877253132609109920 ) ) ;
#1794 = CARTESIAN_POINT ( 'NONE',  ( 147.9748066657072627, 274.3471119452502762, 9.387104374042873900 ) ) ;
#1795 = ORIENTED_EDGE ( 'NONE', *, *, #38607, .F. ) ;
#1796 = CARTESIAN_POINT ( 'NONE',  ( 161.4297170363470570, 251.4317974835881273, -13.07316258580638291 ) ) ;
#1797 = CARTESIAN_POINT ( 'NONE',  ( 105.5326262849960131, 240.9244531367911293, -4.594050593750046652 ) ) ;
#1798 = CARTESIAN_POINT ( 'NONE',  ( 11.52878981408637848, 24.84336893147754921, -7.433330006724137462 ) ) ;
#1799 = CARTESIAN_POINT ( 'NONE',  ( 151.3883635558152321, 268.4346579770563608, 15.44343517165679103 ) ) ;
#1800 = DIRECTION ( 'NONE',  ( -0.8660254037844377084, -0.5000000000000014433, -0.000000000000000000 ) ) ;
#1802 = DIRECTION ( 'NONE',  ( -0.2197389712097134185, -0.9755587037855265597, 0.000000000000000000 ) ) ;
#1801 = CARTESIAN_POINT ( 'NONE',  ( 157.2744851780909414, 258.2395962677452985, 18.17792129701959070 ) ) ;
#1803 = CARTESIAN_POINT ( 'NONE',  ( -17.42236680055705023, 149.2012482093457777, 0.000000000000000000 ) ) ;
#1804 = CARTESIAN_POINT ( 'NONE',  ( 26.98754258172029452, 23.78052372038641238, -10.00000000000000355 ) ) ;
#1805 = CARTESIAN_POINT ( 'NONE',  ( 149.4965729687386045, 271.7113353911534546, -11.48413836595348059 ) ) ;
#1806 = CARTESIAN_POINT ( 'NONE',  ( 91.91334042722833431, 212.3262482093457493, 3.021315404115420679E-15 ) ) ;
#1807 = CARTESIAN_POINT ( 'NONE',  ( 172.9595584307079434, 290.0517967578398384, -1.801039841358881066 ) ) ;
#1808 = CARTESIAN_POINT ( 'NONE',  ( 86.36553431312867701, 47.62854645161011291, 10.65446341473505321 ) ) ;
#1809 = ORIENTED_EDGE ( 'NONE', *, *, #66514, .F. ) ;
#1810 = LINE ( 'NONE', #17499, #37592 ) ;
#1811 = CARTESIAN_POINT ( 'NONE',  ( 16.82306525903893046, 33.21091486745860522, -1.111400068045478839E-16 ) ) ;
#1812 = CARTESIAN_POINT ( 'NONE',  ( 199.9590217945695372, 270.1275301915071054, 9.211081333144562677 ) ) ;
#1813 = VERTEX_POINT ( 'NONE', #37550 ) ;
#1814 = CARTESIAN_POINT ( 'NONE',  ( 72.10789540236547168, 72.29255521243572957, 1.270859788509655974 ) ) ;
#1815 = ADVANCED_FACE ( 'NONE', ( #67970 ), #60345, .F. ) ;
#1816 = CARTESIAN_POINT ( 'NONE',  ( 79.38695290519767411, 50.85501981317847964, 15.00243835328062936 ) ) ;
#1817 = CARTESIAN_POINT ( 'NONE',  ( 83.90589546250612329, 51.88876590914236431, -14.49782437550669734 ) ) ;
#1818 = EDGE_CURVE ( 'NONE', #2161, #41560, #5184, .T. ) ;
#1819 = CARTESIAN_POINT ( 'NONE',  ( 71.35865581505748878, 223.5530062829863027, -4.648177544792955347E-16 ) ) ;
#1820 = CARTESIAN_POINT ( 'NONE',  ( 192.8325075361489382, 296.6512949269187516, 11.74553025762331515 ) ) ;
#1821 = ORIENTED_EDGE ( 'NONE', *, *, #26693, .F. ) ;
#1822 = LINE ( 'NONE', #8908, #48804 ) ;
#1823 = ADVANCED_FACE ( 'NONE', ( #29965 ), #60842, .T. ) ;
#1824 = CARTESIAN_POINT ( 'NONE',  ( 37.26657704017246431, 36.91421378149922816, 9.188101187500008038 ) ) ;
#1825 = CARTESIAN_POINT ( 'NONE',  ( 193.9412999261856783, 289.2827323037661245, -16.07620684846729375 ) ) ;
#1826 = ORIENTED_EDGE ( 'NONE', *, *, #7528, .F. ) ;
#1827 = CARTESIAN_POINT ( 'NONE',  ( 164.0147331130573320, 279.8062665722855513, 12.46059690269307829 ) ) ;
#1828 = ADVANCED_FACE ( 'NONE', ( #24857 ), #62342, .F. ) ;
#1829 = CARTESIAN_POINT ( 'NONE',  ( 147.9500839974939197, 274.3899328626944225, -9.375093207164509224 ) ) ;
#1830 = CARTESIAN_POINT ( 'NONE',  ( 160.2740869459746023, 254.0686150970925610, -15.36085255641610914 ) ) ;
#1831 = ORIENTED_EDGE ( 'NONE', *, *, #24685, .F. ) ;
#1832 = CARTESIAN_POINT ( 'NONE',  ( 86.52979389935374854, 47.15173288509246419, -10.60481917042622868 ) ) ;
#1833 = CARTESIAN_POINT ( 'NONE',  ( 188.6020111787380529, 293.7306159932854825, 12.99143650644070824 ) ) ;
#1834 = CARTESIAN_POINT ( 'NONE',  ( 163.7707306762541748, 246.9877690064858484, 7.021959502997312086 ) ) ;
#1835 = DIRECTION ( 'NONE',  ( 0.000000000000000000, 0.000000000000000000, 1.000000000000000000 ) ) ;
#1836 = CARTESIAN_POINT ( 'NONE',  ( 6.965316927136144365, 15.97253583063838711, -10.00000000000000533 ) ) ;
#1837 = CARTESIAN_POINT ( 'NONE',  ( 80.51741848527098000, 44.46186292381598548, 11.37106337338451922 ) ) ;
#1838 = CARTESIAN_POINT ( 'NONE',  ( 203.3205561747472814, 278.4854618126124706, -15.14439614831292147 ) ) ;
#1839 = ORIENTED_EDGE ( 'NONE', *, *, #94634, .T. ) ;
#1840 = ORIENTED_EDGE ( 'NONE', *, *, #7938, .F. ) ;
#1841 = CARTESIAN_POINT ( 'NONE',  ( 159.5606259118165724, 264.0648208006689401, -17.79391822139266566 ) ) ;
#1842 = ORIENTED_EDGE ( 'NONE', *, *, #75121, .F. ) ;
#1843 = CARTESIAN_POINT ( 'NONE',  ( 77.33513981957392502, 49.70526746924971206, -15.49639835079455352 ) ) ;
#1844 = ORIENTED_EDGE ( 'NONE', *, *, #76284, .F. ) ;
#1845 = FACE_OUTER_BOUND ( 'NONE', #48421, .T. ) ;
#1846 = CARTESIAN_POINT ( 'NONE',  ( 203.3684377202211522, 278.4025285431072803, -16.56116267537666076 ) ) ;
#1847 = EDGE_LOOP ( 'NONE', ( #71468, #74257, #26944, #16905, #19567 ) ) ;
#1848 = CARTESIAN_POINT ( 'NONE',  ( 185.9803440489478987, 282.4389606638047212, -17.18315826590863082 ) ) ;
#1849 = CARTESIAN_POINT ( 'NONE',  ( 25.52770680675560655, 38.23654200823203553, 1.583844403245397769 ) ) ;
#1850 = CARTESIAN_POINT ( 'NONE',  ( 147.3086308153996242, 275.5009623647583226, -7.272174762944374038 ) ) ;
#1851 = CARTESIAN_POINT ( 'NONE',  ( -8.669243101527598583, 25.19333184544593252, -10.00000000000000000 ) ) ;
#1852 = CARTESIAN_POINT ( 'NONE',  ( 192.5076277540105423, 297.2140032159341558, -13.10094381206144298 ) ) ;
#1853 = CARTESIAN_POINT ( 'NONE',  ( 153.2283961777204695, 265.2476279883323400, -17.66880461074566000 ) ) ;
#1854 = LINE ( 'NONE', #84976, #51747 ) ;
#1855 = CARTESIAN_POINT ( 'NONE',  ( 154.7533266961937102, 279.6344470633707715, 2.131676877324898189 ) ) ;
#1856 = CARTESIAN_POINT ( 'NONE',  ( 127.8874276638293850, 235.4548013555409796, -4.594050593750042211 ) ) ;
#1857 = CARTESIAN_POINT ( 'NONE',  ( 70.59331980588027022, 60.81386183084845243, -15.05063277410530276 ) ) ;
#1858 = ORIENTED_EDGE ( 'NONE', *, *, #37574, .T. ) ;
#1860 = VERTEX_POINT ( 'NONE', #15750 ) ;
#1859 = CARTESIAN_POINT ( 'NONE',  ( 138.9086373102437051, 262.5530062829863027, -4.648177544792955347E-16 ) ) ;
#1861 = CARTESIAN_POINT ( 'NONE',  ( 203.6309649086862237, 276.2215947889915810, 13.33342147041682502 ) ) ;
#1862 = CARTESIAN_POINT ( 'NONE',  ( 180.7207050551674001, 256.2221533644915894, 1.285094096768985006 ) ) ;
#1863 = CARTESIAN_POINT ( 'NONE',  ( 174.1986536150437246, 290.1369587316962679, -4.770100445387263299 ) ) ;
#1864 = CARTESIAN_POINT ( 'NONE',  ( 192.5140213078438762, 297.2029292558541442, 12.60096557781599103 ) ) ;
#1865 = CARTESIAN_POINT ( 'NONE',  ( 174.8696466734779449, 292.3029143586743430, -1.153856708368909967 ) ) ;
#1866 = CARTESIAN_POINT ( 'NONE',  ( -31.49789205211705934, 23.81092751074078606, -10.00000000000000000 ) ) ;
#1867 = CARTESIAN_POINT ( 'NONE',  ( 174.1678698021581226, 287.3101935015571939, -9.481082537716513770 ) ) ;
#1868 = CARTESIAN_POINT ( 'NONE',  ( 174.4948782939823104, 282.3355020129680497, 14.83901814079321824 ) ) ;
#1869 = AXIS2_PLACEMENT_3D ( 'NONE', #180, #45756, #59965 ) ;
#1870 = CARTESIAN_POINT ( 'NONE',  ( 22.87549206224920084, 39.05096577487528720, -10.00000000000000000 ) ) ;
#1871 = ORIENTED_EDGE ( 'NONE', *, *, #27551, .T. ) ;
#1872 = CARTESIAN_POINT ( 'NONE',  ( 194.1972774922283236, 294.2874440223457100, -15.09915398317898649 ) ) ;
#1873 = B_SPLINE_CURVE_WITH_KNOTS ( 'NONE', 3,
 ( #86795, #64439, #19844, #89292, #50714, #49728, #72047, #96369 ),
 .UNSPECIFIED., .F., .F.,
 ( 4, 2, 2, 4 ),
 ( 0.001444873917495229261, 0.001841091017814789352, 0.002237308118134349443, 0.003029742318773326077 ),
 .UNSPECIFIED. ) ;
#1874 = CARTESIAN_POINT ( 'NONE',  ( 152.1754162881449872, 273.0523641828442010, 11.78941638112353907 ) ) ;
#1875 = ORIENTED_EDGE ( 'NONE', *, *, #26762, .F. ) ;
#1876 = PLANE ( 'NONE',  #87255 ) ;
#1877 = CARTESIAN_POINT ( 'NONE',  ( 191.0428398434177097, 283.3979691902844138, -16.57323166652324886 ) ) ;
#1878 = CARTESIAN_POINT ( 'NONE',  ( 152.5148928264552524, 266.4834520440945198, -16.24327773663125640 ) ) ;
#1879 = DIRECTION ( 'NONE',  ( -0.9606745773021557744, 0.2776767122488390527, 0.000000000000000000 ) ) ;
#1880 = EDGE_CURVE ( 'NONE', #50442, #29620, #8170, .T. ) ;
#1881 = CARTESIAN_POINT ( 'NONE',  ( 162.8037981520209314, 248.6625452659484381, 9.809699077002424161 ) ) ;
#1883 = CARTESIAN_POINT ( 'NONE',  ( 160.9007617730179902, 281.5835503259689290, 5.800644519205480520 ) ) ;
#1882 = CARTESIAN_POINT ( 'NONE',  ( 163.8036614586782207, 284.0923275947843081, -7.069034562687269485 ) ) ;
#1884 = CARTESIAN_POINT ( 'NONE',  ( 152.6692142062575499, 266.2161595735824449, -16.77985299603479419 ) ) ;
#1885 = EDGE_LOOP ( 'NONE', ( #41574, #54395, #87632, #40774 ) ) ;
#1886 = CARTESIAN_POINT ( 'NONE',  ( 164.4644309026115252, 280.9914584399565456, -11.74015880431011105 ) ) ;
#1887 = CARTESIAN_POINT ( 'NONE',  ( 187.0781841533855641, 262.9812258568358629, -9.029666229471835948 ) ) ;
#1888 = LINE ( 'NONE', #72303, #26415 ) ;
#1889 = CARTESIAN_POINT ( 'NONE',  ( 173.8376058068382122, 250.6904955415916731, -0.9792276279091526314 ) ) ;
#1890 = CARTESIAN_POINT ( 'NONE',  ( 198.6346039733307975, 275.4709485704699432, 15.56980991080272680 ) ) ;
#1891 = B_SPLINE_CURVE_WITH_KNOTS ( 'NONE', 3,
 ( #60396, #97942, #91352, #83761, #37601, #14322, #5232, #68512, #74655, #22417, #59399, #53308, #84263, #20442, #51311, #82281, #45693, #36112, #76621, #38090, #13342, #75143, #69002, #12853, #67016, #28516, #5721, #123, #32000, #8717, #17311, #16810, #92847, #8220, #77635, #85258, #39089, #23904, #617, #32522, #63415, #70002, #24416, #69509, #15804, #94354 ),
 .UNSPECIFIED., .F., .F.,
 ( 4, 1, 2, 2, 1, 2, 2, 1, 1, 2, 2, 1, 1, 2, 2, 1, 1, 2, 2, 1, 1, 1, 2, 2, 1, 1, 1, 2, 2, 4 ),
 ( 0.000000000000000000, 0.06249999999998623323, 0.09374999999997925271, 0.1249999999999722722, 0.1874999999999620859, 0.2187499999999555633, 0.2499999999999490408, 0.3124999999999369393, 0.3437499999999324984, 0.3593749999999296674, 0.3749999999999268363, 0.4374999999999081846, 0.4687499999998982481, 0.4843749999998948064, 0.4999999999998913092, 0.5624999999998865352, 0.5937499999998842037, 0.6093749999998808731, 0.6249999999998775424, 0.6874999999998750999, 0.7187499999998721023, 0.7343749999998727684, 0.7421874999998735456, 0.7499999999998744338, 0.8124999999998896438, 0.8437499999998965272, 0.8593749999999006350, 0.8671874999999048539, 0.8749999999999091838, 1.000000000000000000 ),
 .UNSPECIFIED. ) ;
#1892 = CARTESIAN_POINT ( 'NONE',  ( 192.1396999271463812, 297.8512729055811974, 12.32430960859512403 ) ) ;
#1893 = CARTESIAN_POINT ( 'NONE',  ( 73.05912352472130067, 69.60491006942920933, 9.219028434792550186 ) ) ;
#1894 = CARTESIAN_POINT ( 'NONE',  ( 74.40909250051804236, 68.25437571282814986, 11.42766049309473786 ) ) ;
#1895 = CARTESIAN_POINT ( 'NONE',  ( 193.0126352936363503, 264.4189281174865869, 8.906082567666748773 ) ) ;
#1896 = CARTESIAN_POINT ( 'NONE',  ( 67.16990927169524639, 66.79708245693809943, -9.067759095298582039 ) ) ;
#1897 = CARTESIAN_POINT ( 'NONE',  ( 80.71549903385694336, 229.6589784336661637, -6.496448406907675876E-16 ) ) ;
#1898 = CARTESIAN_POINT ( 'NONE',  ( 67.12017456359353673, 66.69520300484214204, 8.276391925158705476 ) ) ;
#1899 = CARTESIAN_POINT ( 'NONE',  ( 87.97374987192618789, 44.76517282144749288, -4.661398658539860129 ) ) ;
#1900 = CARTESIAN_POINT ( 'NONE',  ( 76.48640248419295062, 51.58918322513654431, 15.64831315713033355 ) ) ;
#1901 = EDGE_CURVE ( 'NONE', #82781, #91972, #39535, .T. ) ;
#1902 = CARTESIAN_POINT ( 'NONE',  ( 202.9547455376043672, 279.1190644220934018, -15.19669173352461478 ) ) ;
#1903 = FACE_OUTER_BOUND ( 'NONE', #32599, .T. ) ;
#1904 = DIRECTION ( 'NONE',  ( -0.8660254037844387076, -0.4999999999999998890, -0.000000000000000000 ) ) ;
#1905 = CARTESIAN_POINT ( 'NONE',  ( 78.28914660356475963, 61.64131563665610969, 15.78308208647086985 ) ) ;
#1907 = DIRECTION ( 'NONE',  ( 1.000000000000000000, 0.000000000000000000, 0.000000000000000000 ) ) ;
#1906 = LINE ( 'NONE', #2413, #45145 ) ;
#1908 = CARTESIAN_POINT ( 'NONE',  ( 207.7802404240296141, 270.7610621071412424, 4.972114562312238029 ) ) ;
#1909 = CARTESIAN_POINT ( 'NONE',  ( 169.2351887702091915, 252.1965608303764554, -9.016775029077457759 ) ) ;
#1910 = CARTESIAN_POINT ( 'NONE',  ( 205.5937218600166432, 274.5482233517041095, -12.97537981636971338 ) ) ;
#1911 = CARTESIAN_POINT ( 'NONE',  ( 77.74985625145598078, 55.20120347894719970, -16.12416396296487520 ) ) ;
#1912 = CARTESIAN_POINT ( 'NONE',  ( -14.49388456338638598, 173.9860189848785410, -2.679491924311249385 ) ) ;
#1913 = CARTESIAN_POINT ( 'NONE',  ( 207.3874697692679945, 271.4413608369101780, -6.809237722377445401 ) ) ;
#1914 = CARTESIAN_POINT ( 'NONE',  ( 43.96406660440233338, 190.0643266524159571, -9.188101187500093303 ) ) ;
#1915 = CARTESIAN_POINT ( 'NONE',  ( 76.98305832116996328, 63.37377475765585899, -15.46912589935254623 ) ) ;
#1916 = CARTESIAN_POINT ( 'NONE',  ( 68.80799682758592439, 210.5333772461660544, 9.188101187500095079 ) ) ;
#1917 = CARTESIAN_POINT ( 'NONE',  ( -86.81108781737714253, -8.000000000000000000, 9.212605237762131694 ) ) ;
#1918 = CARTESIAN_POINT ( 'NONE',  ( 88.06041215430452951, 44.01892986890200632, 0.5558169716948772043 ) ) ;
#1919 = CARTESIAN_POINT ( 'NONE',  ( -19.65312891409030271, 93.06504152958497400, -10.00000000000000888 ) ) ;
#1921 = DIRECTION ( 'NONE',  ( 1.000000000000000000, -1.199437374818249260E-13, 0.000000000000000000 ) ) ;
#1920 = CARTESIAN_POINT ( 'NONE',  ( 82.34202771369412233, 42.93952482416137428, -8.411501796766556183 ) ) ;
#1922 = CARTESIAN_POINT ( 'NONE',  ( 175.2780979910569954, 269.4248474843194572, -16.41417513093275105 ) ) ;
#1923 = CARTESIAN_POINT ( 'NONE',  ( 27.11724708220625857, 33.84336893147757763, -7.433330006724137462 ) ) ;
#1924 = CARTESIAN_POINT ( 'NONE',  ( 80.93147017124917397, 45.39363699920941286, 11.98508622504169985 ) ) ;
#1925 = CARTESIAN_POINT ( 'NONE',  ( 149.2765980486851731, 272.0923431290771646, -11.40617906909507973 ) ) ;
#1926 = EDGE_LOOP ( 'NONE', ( #76923, #39186, #42296, #5688 ) ) ;
#1927 = CARTESIAN_POINT ( 'NONE',  ( 24.28581821943125263, 16.94754757982090254, 5.678558825948272215 ) ) ;
#1928 = CARTESIAN_POINT ( 'NONE',  ( 60.41820218054165537, 211.8149278399160949, 9.188101187500093303 ) ) ;
#1929 = CARTESIAN_POINT ( 'NONE',  ( 76.59052817429427762, 63.78587366202882691, 14.87114199683171734 ) ) ;
#1930 = CARTESIAN_POINT ( 'NONE',  ( 82.56047309644807797, 54.07683023134062239, -15.52634518316282630 ) ) ;
#1931 = CARTESIAN_POINT ( 'NONE',  ( 172.8484988039289476, 290.2287427593016673, -0.3445454264097566610 ) ) ;
#1932 = DIRECTION ( 'NONE',  ( 0.000000000000000000, 0.000000000000000000, 1.000000000000000000 ) ) ;
#1933 = CARTESIAN_POINT ( 'NONE',  ( 201.6381078894957852, 281.3995477237756404, 17.82831317141172889 ) ) ;
#1934 = CARTESIAN_POINT ( 'NONE',  ( 121.3378502276597288, 240.8615022471902591, -10.00000000000009592 ) ) ;
#1935 = DIRECTION ( 'NONE',  ( 0.4242989612870596283, -0.9055221650797523614, 0.000000000000000000 ) ) ;
#1936 = CARTESIAN_POINT ( 'NONE',  ( 206.9377610035629118, 272.2202792677204002, 7.440532334334675646 ) ) ;
#1937 = ORIENTED_EDGE ( 'NONE', *, *, #70332, .F. ) ;
#1938 = CARTESIAN_POINT ( 'NONE',  ( 149.1542970168542865, 273.4448608269726719, -9.883886189052034865 ) ) ;
#1939 = CARTESIAN_POINT ( 'NONE',  ( 82.31027433114240921, 53.67166805628563964, 15.82896004337745310 ) ) ;
#1940 = EDGE_LOOP ( 'NONE', ( #364, #62575, #82433, #97940 ) ) ;
#1941 = CARTESIAN_POINT ( 'NONE',  ( 162.8996025780091941, 248.4966071325470125, 11.23567065566008516 ) ) ;
#1942 = CARTESIAN_POINT ( 'NONE',  ( 37.35373998880870516, 180.8262482093457493, 3.021315404115420679E-15 ) ) ;
#1943 = CARTESIAN_POINT ( 'NONE',  ( -53.68831936616819434, 31.89637462494507147, -10.00000000000000000 ) ) ;
#1944 = EDGE_CURVE ( 'NONE', #21068, #20148, #50964, .T. ) ;
#1945 = ORIENTED_EDGE ( 'NONE', *, *, #26582, .F. ) ;
#1946 = CARTESIAN_POINT ( 'NONE',  ( 176.5495440887839038, 253.2411848376090973, -0.2568067590575703329 ) ) ;
#1947 = ORIENTED_EDGE ( 'NONE', *, *, #8996, .F. ) ;
#1948 = CARTESIAN_POINT ( 'NONE',  ( 72.49874796052694137, 71.64632196231394801, 6.095118657294443132 ) ) ;
#1949 = CARTESIAN_POINT ( 'NONE',  ( 169.5363729319136610, 249.7081694927524040, 3.427481716433138814 ) ) ;
#1950 = CARTESIAN_POINT ( 'NONE',  ( 161.1582366080876625, 264.6096096715138515, -17.81198817937834633 ) ) ;
#1951 = VERTEX_POINT ( 'NONE', #77056 ) ;
#1952 = CARTESIAN_POINT ( 'NONE',  ( 30.11465696128792757, 23.10170272979928541, -7.433330006724141015 ) ) ;
#1953 = CARTESIAN_POINT ( 'NONE',  ( 84.68046352546232924, 50.54697168049320055, -14.01127729920333742 ) ) ;
#1954 = DIRECTION ( 'NONE',  ( -0.8660254037844387076, -0.4999999999999998890, -0.000000000000000000 ) ) ;
#1955 = ORIENTED_EDGE ( 'NONE', *, *, #57301, .T. ) ;
#1956 = DIRECTION ( 'NONE',  ( -0.1269555777209495362, -0.9919084036772447543, 0.000000000000000000 ) ) ;
#1957 = CARTESIAN_POINT ( 'NONE',  ( 86.60116260073726835, 209.2592609112380160, 2.679491924311254714 ) ) ;
#1958 = EDGE_LOOP ( 'NONE', ( #58734, #50426 ) ) ;
#1959 = VERTEX_POINT ( 'NONE', #54744 ) ;
#1960 = CARTESIAN_POINT ( 'NONE',  ( 180.8890834033174713, 294.3766012452771861, 6.559837412958372305 ) ) ;
#1961 =( BOUNDED_CURVE ( )  B_SPLINE_CURVE ( 2, ( #31273, #15561, #30791, #76407, #8487, #15070, #23662, #38367, #37374 ),
 .UNSPECIFIED., .F., .T. ) 
 B_SPLINE_CURVE_WITH_KNOTS ( ( 3, 2, 2, 2, 3 ),
 ( 0.2782258064516128782, 0.2795698924731182533, 0.2822580645161290591, 0.2849462365591398094, 0.2862903225806451846 ),
 .UNSPECIFIED. ) 
 CURVE ( )  GEOMETRIC_REPRESENTATION_ITEM ( )  RATIONAL_B_SPLINE_CURVE ( ( 0.9330127018922194093, 0.9330127018922194093, 1.000000000000000000, 0.8660254037844387076, 1.000000000000000000, 0.8660254037844387076, 1.000000000000000000, 0.9330127018922194093, 0.9330127018922194093 ) ) 
 REPRESENTATION_ITEM ( '' )  );
#1963 = CARTESIAN_POINT ( 'NONE',  ( 148.0346525705264469, 274.2434557974783615, -9.381294579651672905 ) ) ;
#1962 = CARTESIAN_POINT ( 'NONE',  ( 68.11204775988159099, 65.46590518901473388, 10.44757278393263888 ) ) ;
#1964 = CARTESIAN_POINT ( 'NONE',  ( 208.2124092825819162, 270.0125236866795149, -2.339659020816897694 ) ) ;
#1965 = CARTESIAN_POINT ( 'NONE',  ( 155.0303156110108489, 262.1266119787277944, 17.11986653161320859 ) ) ;
#1966 = CARTESIAN_POINT ( 'NONE',  ( 38.51650576605270970, 30.43677371833804202, -10.00000000000000355 ) ) ;
#1967 = CARTESIAN_POINT ( 'NONE',  ( 205.2660270307054304, 275.1158074454486382, -13.97598661256119179 ) ) ;
#1968 = CARTESIAN_POINT ( 'NONE',  ( 208.0280121190496629, 270.3319089426888127, -3.803189352412944757 ) ) ;
#1969 = CARTESIAN_POINT ( 'NONE',  ( 206.4633727170604232, 270.6208656945399866, 2.462764060182144554 ) ) ;
#1970 = CARTESIAN_POINT ( 'NONE',  ( 79.31323107047896315, 59.76145823410249136, 16.51491591541846304 ) ) ;
#1971 = CARTESIAN_POINT ( 'NONE',  ( 91.08134800299070832, 214.2048013555409796, 4.594050593750051981 ) ) ;
#1972 = VERTEX_POINT ( 'NONE', #93296 ) ;
#1973 = CARTESIAN_POINT ( 'NONE',  ( 151.0036289208911171, 269.1010379121764799, 14.24595189915657478 ) ) ;
#1974 = LINE ( 'NONE', #48575, #80408 ) ;
#1975 = CARTESIAN_POINT ( 'NONE',  ( 46.85966550219794158, 197.8615022471903728, 4.537668576076727938E-14 ) ) ;
#1976 = ORIENTED_EDGE ( 'NONE', *, *, #55649, .F. ) ;
#1977 = VECTOR ( 'NONE', #48677, 1000.000000000000114 ) ;
#1978 = CARTESIAN_POINT ( 'NONE',  ( 195.3813422720796780, 292.2365836641902774, -16.04365517931749707 ) ) ;
#1979 = ORIENTED_EDGE ( 'NONE', *, *, #89670, .F. ) ;
#1980 = CARTESIAN_POINT ( 'NONE',  ( 80.04850862667662170, 44.86057290276260545, -11.28600205406214663 ) ) ;
#1981 = LINE ( 'NONE', #93203, #78611 ) ;
#1983 = B_SPLINE_SURFACE_WITH_KNOTS ( 'NONE', 3, 1, ( 
 ( #70286, #13727 ),
 ( #31288, #62175 ),
 ( #54570, #898 ),
 ( #44604, #16095 ),
 ( #77913, #75538 ),
 ( #13252, #6123 ),
 ( #28421, #51216 ),
 ( #75048, #44109 ),
 ( #46999, #20345 ),
 ( #37020, #5137 ),
 ( #67419, #89772 ),
 ( #59300, #8502 ),
 ( #90280, #98348 ),
 ( #28938, #21332 ),
 ( #91260, #59815 ),
 ( #33818, #70804 ),
 ( #18611, #24691 ),
 ( #10499, #63194 ),
 ( #25711, #56072 ),
 ( #55573, #56590 ),
 ( #47981, #93633 ),
 ( #79444, #64195 ),
 ( #1908, #88062 ),
 ( #25190, #10009 ),
 ( #95146, #32293 ),
 ( #87065, #57083 ),
 ( #2928, #86557 ),
 ( #41890, #94633 ),
 ( #32789, #49489 ),
 ( #87579, #17089 ),
 ( #55081, #1412 ),
 ( #18104, #17597 ),
 ( #64705, #33293 ),
 ( #80446, #8995 ) ),
 .UNSPECIFIED., .T., .F., .F.,
 ( 4, 2, 2, 2, 2, 2, 2, 2, 2, 2, 2, 2, 2, 2, 2, 2, 4 ),
 ( 2, 2 ),
 ( 0.000000000000000000, 0.06250000000000000000, 0.1250000000000000000, 0.1875000000000000000, 0.2500000000000000000, 0.3125000000000000000, 0.3750000000000000000, 0.4375000000000000000, 0.5000000000000000000, 0.5625000000000000000, 0.6250000000000000000, 0.6875000000000000000, 0.7500000000000000000, 0.8125000000000000000, 0.8750000000000000000, 0.9375000000000000000, 1.000000000000000000 ),
 ( 0.000000000000000000, 1.000000000000000000 ),
 .UNSPECIFIED. ) ;
#1982 = CARTESIAN_POINT ( 'NONE',  ( -13.11024591527723437, 4.999999999999999112, -17.00000000000016698 ) ) ;
#1984 = CARTESIAN_POINT ( 'NONE',  ( 84.65630082135325551, 42.18976564707919152, -0.8137823442531888496 ) ) ;
#1985 = CARTESIAN_POINT ( 'NONE',  ( 81.63649175858802209, 48.05684571567061880, -13.06511883598228430 ) ) ;
#1986 = CARTESIAN_POINT ( 'NONE',  ( 162.6859166034911652, 248.8667220972772611, 10.26171246773997758 ) ) ;
#1987 = CARTESIAN_POINT ( 'NONE',  ( 75.46539357129627490, 220.5024278399160664, -9.188101187500093303 ) ) ;
#1988 = ORIENTED_EDGE ( 'NONE', *, *, #92550, .F. ) ;
#1989 = VERTEX_POINT ( 'NONE', #86721 ) ;
#1990 = CARTESIAN_POINT ( 'NONE',  ( 200.7664336291577172, 282.9093318303307569, -18.32876612325386034 ) ) ;
#1991 = ORIENTED_EDGE ( 'NONE', *, *, #49837, .F. ) ;
#1992 = CARTESIAN_POINT ( 'NONE',  ( 75.86452061248199641, 65.14283366293828692, -14.47928019947265277 ) ) ;
#1993 = EDGE_CURVE ( 'NONE', #19180, #39829, #83364, .T. ) ;
#1994 = CARTESIAN_POINT ( 'NONE',  ( 165.4345553874274799, 285.6554192157983039, 1.183051567514476599 ) ) ;
#1995 = LINE ( 'NONE', #24779, #44472 ) ;
#1996 = CARTESIAN_POINT ( 'NONE',  ( 88.05221915382541908, 44.76013711945522289, 4.532355379009165297 ) ) ;
#1997 = VERTEX_POINT ( 'NONE', #7665 ) ;
#1998 = CARTESIAN_POINT ( 'NONE',  ( 188.6991936886695953, 294.9304948621235667, 11.61111646670225106 ) ) ;
#1999 = CARTESIAN_POINT ( 'NONE',  ( 156.7504469567443550, 274.0276245742728634, 13.42060143992435428 ) ) ;
#2000 = CARTESIAN_POINT ( 'NONE',  ( 159.9531724557437826, 253.5999738052623229, -15.71074128491364874 ) ) ;
#2001 = CARTESIAN_POINT ( 'NONE',  ( 155.6583371091562640, 262.5339888893300895, -17.25629704915573015 ) ) ;
#2002 = CARTESIAN_POINT ( 'NONE',  ( 175.2754180912867241, 284.4784848018189223, 14.01285901753186458 ) ) ;
#2003 = FACE_OUTER_BOUND ( 'NONE', #31225, .T. ) ;
#2004 = CARTESIAN_POINT ( 'NONE',  ( 195.4167945326838378, 279.6122101856814197, -17.17760159917481744 ) ) ;
#2005 = VERTEX_POINT ( 'NONE', #16260 ) ;
#2006 = DIRECTION ( 'NONE',  ( -0.3213938048432640748, 0.5566703992264119272, -0.7660444431189857850 ) ) ;
#2007 = CARTESIAN_POINT ( 'NONE',  ( 161.1089126327036354, 251.5981730984191529, 13.95161017039218976 ) ) ;
#2008 = DIRECTION ( 'NONE',  ( 0.6361630342459738685, -0.7715546603183444097, 0.000000000000000000 ) ) ;
#2009 = CARTESIAN_POINT ( 'NONE',  ( 170.9817807944941137, 251.5856905545531959, 7.058976180640677001 ) ) ;
#2010 = CARTESIAN_POINT ( 'NONE',  ( 83.37579341631962393, 51.76272850660085822, 14.96038908820327507 ) ) ;
#2011 = CARTESIAN_POINT ( 'NONE',  ( 202.4721870783228894, 268.0718720055712083, 5.348787301547115902 ) ) ;
#2012 = EDGE_CURVE ( 'NONE', #64801, #80515, #62589, .T. ) ;
#2013 = CARTESIAN_POINT ( 'NONE',  ( 153.2026299055073650, 270.4964049230587761, 13.90442887244355497 ) ) ;
#2014 = ORIENTED_EDGE ( 'NONE', *, *, #42285, .T. ) ;
#2015 = CARTESIAN_POINT ( 'NONE',  ( 76.47821338308438044, 63.12304481703771586, -15.07910235800729204 ) ) ;
#2017 = CARTESIAN_POINT ( 'NONE',  ( 73.70322323093775196, 55.31382080484373631, 16.11694223268900927 ) ) ;
#2016 = CARTESIAN_POINT ( 'NONE',  ( 179.8355924322922590, 266.3652243622770470, -14.78567419157851504 ) ) ;
#2018 = CARTESIAN_POINT ( 'NONE',  ( 185.0402102251197789, 257.2940728988994579, 2.699890041601303192 ) ) ;
#2019 = CARTESIAN_POINT ( 'NONE',  ( 31.51172446742527100, 30.14441083166263269, 10.00000000000000533 ) ) ;
#2021 = EDGE_CURVE ( 'NONE', #87939, #4112, #98188, .T. ) ;
#2020 = DIRECTION ( 'NONE',  ( -0.8660254037844387076, -0.4999999999999998890, -0.000000000000000000 ) ) ;
#2022 = CARTESIAN_POINT ( 'NONE',  ( 172.3175038124396110, 275.1038600624426067, 16.61276981194052738 ) ) ;
#2023 = CARTESIAN_POINT ( 'NONE',  ( 183.7733247487505253, 274.9862421907877206, 16.36274383044956693 ) ) ;
#2024 = CARTESIAN_POINT ( 'NONE',  ( 41.10966550219799842, 207.8207943907112281, 18.47570218321542868 ) ) ;
#2025 = CARTESIAN_POINT ( 'NONE',  ( 192.1810643495398665, 262.2731238949148178, 2.987946743577344133 ) ) ;
#2026 = CARTESIAN_POINT ( 'NONE',  ( 207.8792014703394671, 270.5896565469619759, -5.780233892547864905 ) ) ;
#2027 = CARTESIAN_POINT ( 'NONE',  ( -9.892408837089961438, 177.3464784336661637, 1.353441290958777327E-15 ) ) ;
#2028 = CARTESIAN_POINT ( 'NONE',  ( 82.19827357919754718, 47.83406103887718075, 12.71279386660662958 ) ) ;
#2029 = ORIENTED_EDGE ( 'NONE', *, *, #232, .F. ) ;
#2030 = CARTESIAN_POINT ( 'NONE',  ( 174.9122443831272165, 255.2793860169833522, 8.300717241462230334 ) ) ;
#2031 = CARTESIAN_POINT ( 'NONE',  ( 26.65225264301594166, 37.16126292948896293, -6.180339887498951690 ) ) ;
#2032 = CARTESIAN_POINT ( 'NONE',  ( 208.3117541397001844, 269.8404533466799080, 2.895672523916592578 ) ) ;
#2033 = CARTESIAN_POINT ( 'NONE',  ( 81.97703060113059337, 41.73519428853659718, 5.412281464924958208 ) ) ;
#2034 = CARTESIAN_POINT ( 'NONE',  ( 15.38488118375084390, 185.8149278399160949, -9.188101187500095079 ) ) ;
#2035 = VECTOR ( 'NONE', #52050, 1000.000000000000114 ) ;
#2036 = FACE_OUTER_BOUND ( 'NONE', #13697, .T. ) ;
#2037 = CARTESIAN_POINT ( 'NONE',  ( 37.82368544302515545, 30.03677371833804699, 10.00000000000000533 ) ) ;
#2038 = B_SPLINE_CURVE_WITH_KNOTS ( 'NONE', 3,
 ( #95873, #2133, #9746, #48219, #25414, #86781, #56306, #87795, #86278, #18337, #16814, #93865, #10230, #17835, #24422, #33016, #49231, #47701, #9222, #64422, #25937, #63915, #40099, #26430, #48735, #80165, #40605, #79668, #10732, #57310, #42109, #41606, #71040, #95385, #32527, #32004, #88280, #18833, #80669, #1643, #94360, #24914, #55788, #17315, #44087, #28921, #52193, #5119, #19353, #35999, #90764, #51199 ),
 .UNSPECIFIED., .F., .F.,
 ( 4, 2, 2, 2, 2, 2, 2, 2, 2, 2, 2, 2, 2, 2, 2, 2, 2, 2, 2, 2, 2, 2, 2, 2, 2, 4 ),
 ( 0.0004155875641910399465, 0.0008752706911513232803, 0.001105112254631483758, 0.001334953818111644236, 0.001449874599851724150, 0.001564795381591804063, 0.001679716163331883977, 0.001794636945071964324, 0.002024478508552008792, 0.002254320072032053261, 0.003173686325952355166, 0.004093052579872656638, 0.005012418833792958543, 0.005472101960753063959, 0.005701943524233080672, 0.005816864305973089462, 0.005874324696843134623, 0.005931785087713179784, 0.005989245478583224945, 0.006046705869453270106, 0.006161626651193358693, 0.006391468214673476020, 0.006851151341633709806, 0.007310834468593942724, 0.007540676032074041836, 0.007770517595554140081 ),
 .UNSPECIFIED. ) ;
#2039 = CARTESIAN_POINT ( 'NONE',  ( 199.5313597256959781, 267.4056706038007292, -6.663851089317214260 ) ) ;
#2040 = CARTESIAN_POINT ( 'NONE',  ( 173.5268431453002620, 273.0267676714563549, -16.40558794790413444 ) ) ;
#2041 = CARTESIAN_POINT ( 'NONE',  ( 81.22934400301913627, 56.18010474871477555, 16.10233499384894174 ) ) ;
#2042 = CARTESIAN_POINT ( 'NONE',  ( 84.99999999999998579, 14.99999999999999467, 59.99999999999999289 ) ) ;
#2043 = EDGE_CURVE ( 'NONE', #50852, #69710, #86222, .T. ) ;
#2044 = ADVANCED_FACE ( 'NONE', ( #94305 ), #46909, .F. ) ;
#2045 = CARTESIAN_POINT ( 'NONE',  ( 186.8369214609370488, 295.7978260411641713, -8.160117540320300122 ) ) ;
#2046 = AXIS2_PLACEMENT_3D ( 'NONE', #13651, #66837, #83081 ) ;
#2047 = CARTESIAN_POINT ( 'NONE',  ( 84.02300986820688422, 51.73893231647485180, 14.78971152351953045 ) ) ;
#2048 = EDGE_CURVE ( 'NONE', #72912, #83865, #78409, .T. ) ;
#2049 = CARTESIAN_POINT ( 'NONE',  ( 182.6352093130429068, 296.5685661505265784, 1.834901431546525297 ) ) ;
#2050 = CARTESIAN_POINT ( 'NONE',  ( 85.83080867249778123, 210.3615022471902023, 5.000000000000051514 ) ) ;
#2051 = CARTESIAN_POINT ( 'NONE',  ( 71.79182426994934474, 66.53813379304610010, -11.50093241856152559 ) ) ;
#2052 = CARTESIAN_POINT ( 'NONE',  ( 161.8935460472482930, 280.0887632390822546, 11.41936692958946509 ) ) ;
#2053 = CARTESIAN_POINT ( 'NONE',  ( 170.2529524909020324, 288.7139002527517277, 5.426736320396455149 ) ) ;
#2054 = CARTESIAN_POINT ( 'NONE',  ( 47.96943409690536697, 192.3768266524160140, 9.188101187500098632 ) ) ;
#2055 = CARTESIAN_POINT ( 'NONE',  ( 67.31503155234506153, 66.65634768321555725, -8.484550801122479058 ) ) ;
#2056 = CARTESIAN_POINT ( 'NONE',  ( 203.7093853360854894, 270.4153380413875993, -6.448685755690142685 ) ) ;
#2057 = CARTESIAN_POINT ( 'NONE',  ( 147.5498377207569263, 275.0831797495432056, 4.097967709737811326 ) ) ;
#2058 = CARTESIAN_POINT ( 'NONE',  ( 67.28733722124985661, 66.41312804726935326, -8.801120809818232971 ) ) ;
#2059 = EDGE_CURVE ( 'NONE', #67256, #32333, #54564, .T. ) ;
#2060 = ORIENTED_EDGE ( 'NONE', *, *, #27585, .T. ) ;
#2062 = DIRECTION ( 'NONE',  ( 0.9974094913373514615, 0.07193265315672570104, 0.000000000000000000 ) ) ;
#2061 = AXIS2_PLACEMENT_3D ( 'NONE', #98573, #23019, #29156 ) ;
#2063 = LINE ( 'NONE', #94289, #52221 ) ;
#2064 = CARTESIAN_POINT ( 'NONE',  ( 147.1674053649995528, 275.7455720201731424, 6.878590988502374159 ) ) ;
#2065 = CARTESIAN_POINT ( 'NONE',  ( -13.11024591527734628, 4.999999999999999112, 32.50000000000000000 ) ) ;
#2066 = CARTESIAN_POINT ( 'NONE',  ( 32.62131273085646654, 21.76004757982090965, 5.678558825948272215 ) ) ;
#2067 = CARTESIAN_POINT ( 'NONE',  ( 162.8996025780091941, 248.4966071325470125, 11.23567065566008516 ) ) ;
#2068 = CARTESIAN_POINT ( 'NONE',  ( 149.1486417047969155, 272.3139700178423368, -11.47583619705022606 ) ) ;
#2069 = CARTESIAN_POINT ( 'NONE',  ( 188.9913214560809536, 269.9620198908939415, -15.45701251956971944 ) ) ;
#2070 = ORIENTED_EDGE ( 'NONE', *, *, #10876, .T. ) ;
#2071 = B_SPLINE_CURVE_WITH_KNOTS ( 'NONE', 3,
 ( #43014, #33970, #96281, #50142, #11662, #66341, #42524, #73458, #4041, #65826, #73952, #27841, #48660, #3080, #98762, #14639, #67332, #66832, #59725, #91667, #36424, #84088, #45519, #97760, #35930, #82090, #14138, #98256, #6543, #6034, #28330, #75450, #68821, #36929, #60210, #37418, #59207, #90691, #76450, #68324, #20757, #99250, #60706, #90182, #29345, #7027, #28845, #51645 ),
 .UNSPECIFIED., .F., .F.,
 ( 4, 2, 2, 2, 2, 2, 2, 2, 2, 2, 2, 2, 2, 2, 2, 2, 2, 2, 2, 2, 2, 2, 2, 4 ),
 ( 0.0007362855887611816693, 0.0009426974782739958644, 0.001149109367786810059, 0.001252315312543195690, 0.001355521257299581537, 0.001561933146812410911, 0.001974756925838208003, 0.002387580704864005095, 0.003213228262915446623, 0.004038875820966888151, 0.004864523379018329680, 0.005277347158044092511, 0.005483759047556896297, 0.005586964992313334620, 0.005638567964691484392, 0.005690170937069634165, 0.005793376881825774115, 0.005896582826581914065, 0.006102994716094055187, 0.006515818495118457995, 0.006722230384630654629, 0.006928642274142851262, 0.007135054163655047896, 0.007341466053167244529 ),
 .UNSPECIFIED. ) ;
#2072 = CARTESIAN_POINT ( 'NONE',  ( 14.66449673273962162, 9.262165230724928477, -2.296566073217252530E-15 ) ) ;
#2073 = ADVANCED_FACE ( 'NONE', ( #1903 ), #56585, .F. ) ;
#2074 = CARTESIAN_POINT ( 'NONE',  ( 198.4226516368227067, 264.7884397865803408, 0.06761542484275395726 ) ) ;
#2075 = CARTESIAN_POINT ( 'NONE',  ( 73.31883174054932795, 59.80927123552942959, -15.43389514559521558 ) ) ;
#2076 = CARTESIAN_POINT ( 'NONE',  ( 71.47791206682282450, 72.34364865201936823, -1.216664393387151488 ) ) ;
#2077 = ADVANCED_FACE ( 'NONE', ( #39367 ), #10005, .T. ) ;
#2078 = ORIENTED_EDGE ( 'NONE', *, *, #27213, .T. ) ;
#2079 = FACE_OUTER_BOUND ( 'NONE', #90824, .T. ) ;
#2080 = CARTESIAN_POINT ( 'NONE',  ( 150.6487462746963502, 269.7157126861102370, 15.18501655901553704 ) ) ;
#2081 = CARTESIAN_POINT ( 'NONE',  ( -19.65312891409030271, 93.06504152958497400, -10.00000000000000888 ) ) ;
#2082 = CARTESIAN_POINT ( 'NONE',  ( 190.0896302098338424, 301.4020978150248311, 3.433521196325825642 ) ) ;
#2083 = ORIENTED_EDGE ( 'NONE', *, *, #56810, .T. ) ;
#2085 = CARTESIAN_POINT ( 'NONE',  ( 183.4553195968295256, 297.0403188216897661, -2.838562726794640056 ) ) ;
#2084 = CARTESIAN_POINT ( 'NONE',  ( 186.2533614392526715, 272.0223876180238562, -16.20928411658415769 ) ) ;
#2086 = ORIENTED_EDGE ( 'NONE', *, *, #49860, .T. ) ;
#2087 = CARTESIAN_POINT ( 'NONE',  ( 152.7295469705997277, 266.1116601603806657, -17.40211458100010589 ) ) ;
#2088 = CARTESIAN_POINT ( 'NONE',  ( 175.3074307085254020, 254.5436327766159650, 9.407465564047683415 ) ) ;
#2089 = CARTESIAN_POINT ( 'NONE',  ( 73.12133584826474930, 57.41764960941905827, -15.88333458976553381 ) ) ;
#2090 = LINE ( 'NONE', #85219, #22466 ) ;
#2091 = B_SPLINE_CURVE_WITH_KNOTS ( 'NONE', 3,
 ( #32829, #40909, #48543, #9556, #85594, #39411, #85070, #62718, #93166, #100255, #79483, #10046, #93675, #31816, #31327, #94672, #30837, #16135, #47033, #71352, #61723, #94176, #77950, #940, #24239, #24727, #48025, #15617, #54112, #25229, #78969, #92670, #55117, #46515, #77453, #47526, #9036, #39908, #70841, #1453, #40419, #86594, #56116, #19162, #75216, #43788 ),
 .UNSPECIFIED., .F., .F.,
 ( 4, 1, 1, 1, 2, 2, 1, 1, 1, 2, 2, 1, 1, 2, 2, 1, 1, 2, 2, 1, 1, 2, 2, 1, 2, 2, 1, 2, 2, 4 ),
 ( 0.000000000000000000, 0.06250000000000756339, 0.09375000000001003364, 0.1093750000000108941, 0.1171875000000097977, 0.1250000000000086875, 0.1875000000000000278, 0.2187499999999972800, 0.2343749999999944489, 0.2421874999999930334, 0.2499999999999916178, 0.3124999999999925060, 0.3437499999999928946, 0.3593749999999915623, 0.3749999999999902300, 0.4374999999999908962, 0.4687499999999912292, 0.4843749999999913958, 0.4999999999999915623, 0.5624999999999952260, 0.5937499999999971134, 0.6093749999999963363, 0.6249999999999955591, 0.6874999999999895639, 0.7187499999999882316, 0.7499999999999868994, 0.8124999999999877875, 0.8437499999999895639, 0.8749999999999913403, 1.000000000000000000 ),
 .UNSPECIFIED. ) ;
#2092 = CARTESIAN_POINT ( 'NONE',  ( 157.4211152037729562, 257.9856256133486454, -16.71526195140576831 ) ) ;
#2093 = CARTESIAN_POINT ( 'NONE',  ( 98.52366704282199805, 221.5643266524159856, -9.188101187500093303 ) ) ;
#2094 = B_SPLINE_CURVE_WITH_KNOTS ( 'NONE', 3,
 ( #88328, #34559, #34083, #88831, #89322, #81699 ),
 .UNSPECIFIED., .F., .F.,
 ( 4, 2, 4 ),
 ( 0.001541644710436317414, 0.001826678494032424977, 0.002111712277628532541 ),
 .UNSPECIFIED. ) ;
#2095 = CARTESIAN_POINT ( 'NONE',  ( 184.0096797657860179, 289.1861371066262905, -13.00318607164890494 ) ) ;
#2096 = VERTEX_POINT ( 'NONE', #31283 ) ;
#2097 = DIRECTION ( 'NONE',  ( -0.6544109481086123337, -0.7561390817803210762, 0.000000000000000000 ) ) ;
#2098 = ORIENTED_EDGE ( 'NONE', *, *, #49119, .T. ) ;
#2099 = CARTESIAN_POINT ( 'NONE',  ( 31.23567208480136514, 20.96004757982091604, -5.678558825948276656 ) ) ;
#2100 = CARTESIAN_POINT ( 'NONE',  ( 159.4574711498080433, 254.4585536525209477, 16.86100557095418395 ) ) ;
#2101 = CARTESIAN_POINT ( 'NONE',  ( 71.07376813403469384, 70.69339414025402846, -6.375625711488249969 ) ) ;
#2102 = CARTESIAN_POINT ( 'NONE',  ( 65.42534541587671981, 199.3923013555409796, 4.594050593750050204 ) ) ;
#2103 = CARTESIAN_POINT ( 'NONE',  ( 73.83553503644242255, 68.51229284434135991, 10.91127707145445314 ) ) ;
#2104 = CARTESIAN_POINT ( 'NONE',  ( 150.7226148805041817, 269.5877685077668957, 15.52819754351937576 ) ) ;
#2105 = CARTESIAN_POINT ( 'NONE',  ( 150.4319008355389542, 270.0913000041206260, 13.83804576328048697 ) ) ;
#2106 = CARTESIAN_POINT ( 'NONE',  ( 172.6732692711807147, 271.7370492138056761, 16.73332340419656461 ) ) ;
#2107 = EDGE_LOOP ( 'NONE', ( #36555, #33108, #78838, #5603, #26273, #97174, #217, #80248, #20760, #70554, #64523, #79355, #35597, #90155, #96285, #63008, #99410, #19525, #46811, #50604 ) ) ;
#2108 = CARTESIAN_POINT ( 'NONE',  ( 76.22354811720457235, 58.03663319312042290, -16.07154475767281099 ) ) ;
#2109 = CARTESIAN_POINT ( 'NONE',  ( 83.55665905661119552, 42.82685997504432862, -5.889658287066807496 ) ) ;
#2110 = CARTESIAN_POINT ( 'NONE',  ( 177.1723795352289130, 288.8195398279596589, 11.30650638855078327 ) ) ;
#2111 = DIRECTION ( 'NONE',  ( -0.8660254037844359321, -0.5000000000000051070, -0.000000000000000000 ) ) ;
#2112 = VERTEX_POINT ( 'NONE', #86063 ) ;
#2113 = CARTESIAN_POINT ( 'NONE',  ( 172.1042385749445032, 259.7490272540697447, -13.86291087914393039 ) ) ;
#2114 = CARTESIAN_POINT ( 'NONE',  ( 174.0496840832364569, 277.6969804377837931, -15.67051255850419444 ) ) ;
#2115 = DIRECTION ( 'NONE',  ( -0.7511915808658273797, -0.6600842437418872333, 0.000000000000000000 ) ) ;
#2116 = CARTESIAN_POINT ( 'NONE',  ( 193.0142717932987182, 296.3364699985351081, -13.30037542329744937 ) ) ;
#2117 = CARTESIAN_POINT ( 'NONE',  ( 190.4841013044967042, 300.7188538369516095, 4.682298117523464143 ) ) ;
#2118 = AXIS2_PLACEMENT_3D ( 'NONE', #61696, #17102, #69309 ) ;
#2119 = CARTESIAN_POINT ( 'NONE',  ( 177.3509020185674103, 269.5276210205321945, 16.09886373478537180 ) ) ;
#2120 = ADVANCED_FACE ( 'NONE', ( #62170 ), #8990, .T. ) ;
#2121 = CARTESIAN_POINT ( 'NONE',  ( -22.42236680055709641, 157.8615022471902591, 0.000000000000000000 ) ) ;
#2122 = CARTESIAN_POINT ( 'NONE',  ( 67.25018235246020026, 66.88641011210830811, 9.010392920173572406 ) ) ;
#2123 = CARTESIAN_POINT ( 'NONE',  ( 73.65118521283083908, 64.80899555395295408, -13.49371764281556807 ) ) ;
#2124 = DIRECTION ( 'NONE',  ( -0.2033683215378938036, 0.3522442655536374700, -0.9135454576426059736 ) ) ;
#2125 = CARTESIAN_POINT ( 'NONE',  ( 102.9345500736427113, 239.4244531367911293, -4.594050593750046652 ) ) ;
#2126 = VERTEX_POINT ( 'NONE', #95140 ) ;
#2127 = CARTESIAN_POINT ( 'NONE',  ( 191.0862225170008628, 299.6759493045793192, -9.402218231374108726 ) ) ;
#2128 = CARTESIAN_POINT ( 'NONE',  ( 31.50071699975810091, 85.35483982831681260, 59.99999999999999289 ) ) ;
#2129 = EDGE_CURVE ( 'NONE', #25226, #26753, #87573, .T. ) ;
#2130 = CARTESIAN_POINT ( 'NONE',  ( 155.3513572141771704, 261.5705516107003064, -17.00592413546589299 ) ) ;
#2131 = CARTESIAN_POINT ( 'NONE',  ( 164.0741338217690668, 246.4622593432776796, 7.359073626423302983 ) ) ;
#2132 = CARTESIAN_POINT ( 'NONE',  ( 83.52018940653934465, 51.62319858702418429, -14.86581989589152819 ) ) ;
#2133 = CARTESIAN_POINT ( 'NONE',  ( 175.7490893856983689, 252.6561874605901608, 5.270972134136622245 ) ) ;
#2134 = ORIENTED_EDGE ( 'NONE', *, *, #91860, .T. ) ;
#2135 = CARTESIAN_POINT ( 'NONE',  ( 80.34072333937859867, 58.10214405650913250, -16.60604606379114401 ) ) ;
#2136 = B_SPLINE_CURVE_WITH_KNOTS ( 'NONE', 3,
 ( #3952, #18667, #96194, #40927, #95713, #57137 ),
 .UNSPECIFIED., .F., .F.,
 ( 4, 2, 4 ),
 ( 0.0007689256722880135090, 0.001136985650662513314, 0.001505045629037013010 ),
 .UNSPECIFIED. ) ;
#2137 = CARTESIAN_POINT ( 'NONE',  ( 71.76701767287354983, 72.15843607843383722, 0.5844455542204934906 ) ) ;
#2138 = CARTESIAN_POINT ( 'NONE',  ( 181.9589692923136113, 260.5425098207756491, 9.737347583194500444 ) ) ;
#2139 = CARTESIAN_POINT ( 'NONE',  ( 206.5266458972945429, 272.9323515195362120, -9.802257691457246125 ) ) ;
#2140 = CARTESIAN_POINT ( 'NONE',  ( 146.0739611433025686, 245.9548013555409796, -4.594050593750042211 ) ) ;
#2141 = EDGE_CURVE ( 'NONE', #77129, #80395, #48652, .T. ) ;
#2142 = CARTESIAN_POINT ( 'NONE',  ( 150.8247211172754589, 269.4109153179094278, -14.37608026040300402 ) ) ;
#2143 = CIRCLE ( 'NONE', #15053, 17.82106496071138224 ) ;
#2144 = CARTESIAN_POINT ( 'NONE',  ( 189.1275178940386752, 299.7030702647930411, 4.939670191479129890 ) ) ;
#2145 = DIRECTION ( 'NONE',  ( -0.000000000000000000, -0.000000000000000000, -1.000000000000000000 ) ) ;
#2146 = CARTESIAN_POINT ( 'NONE',  ( 62.50250967810423930, 197.7048013555409796, 4.594050593750051981 ) ) ;
#2147 = CARTESIAN_POINT ( 'NONE',  ( 85.47443485840854294, 48.29312219740740630, -11.73648896724759716 ) ) ;
#2148 = CARTESIAN_POINT ( 'NONE',  ( 205.2414727015710412, 275.1583367910551488, -12.71338796362297963 ) ) ;
#2149 = LINE ( 'NONE', #78150, #15677 ) ;
#2150 = EDGE_CURVE ( 'NONE', #39162, #45893, #11517, .T. ) ;
#2151 = B_SPLINE_CURVE_WITH_KNOTS ( 'NONE', 3,
 ( #21256, #60218, #75459, #36940, #91182, #21743, #52627, #45034, #32339, #56638, #79489, #62724, #71864, #86601, #31823, #86109 ),
 .UNSPECIFIED., .F., .F.,
 ( 4, 2, 2, 2, 2, 2, 2, 4 ),
 ( 0.0005595848447356708590, 0.0008683227071104232054, 0.001177060569485175552, 0.001485798431859928007, 0.001794536294234680245, 0.002103274156609432483, 0.002412012018984184721, 0.003029487743733707845 ),
 .UNSPECIFIED. ) ;
#2152 = CARTESIAN_POINT ( 'NONE',  ( 69.93729631481735964, 70.68432073330353660, -3.157426850868849666 ) ) ;
#2153 = ADVANCED_FACE ( 'NONE', ( #3897 ), #88553, .T. ) ;
#2154 = CARTESIAN_POINT ( 'NONE',  ( 174.3956825652301461, 262.1553256887494854, 14.35235884442154308 ) ) ;
#2155 = CARTESIAN_POINT ( 'NONE',  ( 155.1820006974310218, 279.5632244157534387, -1.579113261361717369 ) ) ;
#2156 = CARTESIAN_POINT ( 'NONE',  ( 178.8091420268403908, 291.8339325867452771, -6.888020678422202003 ) ) ;
#2157 = CARTESIAN_POINT ( 'NONE',  ( 155.6569868912636991, 261.0411854816857158, -17.75433477650897984 ) ) ;
#2158 = CARTESIAN_POINT ( 'NONE',  ( 178.6208630460672282, 261.2445556773918156, 12.21686540733617754 ) ) ;
#2159 = CARTESIAN_POINT ( 'NONE',  ( 128.9696990949622659, 235.2677522451417929, -5.000000000000041744 ) ) ;
#2160 = DIRECTION ( 'NONE',  ( 0.5000000000000014433, -0.8660254037844378194, 0.000000000000000000 ) ) ;
#2161 = VERTEX_POINT ( 'NONE', #19119 ) ;
#2162 = CARTESIAN_POINT ( 'NONE',  ( 189.9457600613112902, 301.6512882219586800, 0.04117870562599101891 ) ) ;
#2163 = CARTESIAN_POINT ( 'NONE',  ( -15.79203335248894469, 167.8149278399160949, -9.188101187500095079 ) ) ;
#2164 = CARTESIAN_POINT ( 'NONE',  ( 46.56214281575564939, 191.5643266524159856, -9.188101187500093303 ) ) ;
#2165 = CARTESIAN_POINT ( 'NONE',  ( 13.94779419600527959, 26.79103043416548147, 8.090169943749478065 ) ) ;
#2166 = CARTESIAN_POINT ( 'NONE',  ( 32.38751264475774860, 201.0530062829863027, -4.648177544792955347E-16 ) ) ;
#2167 = CARTESIAN_POINT ( 'NONE',  ( 79.57660877456937953, 50.05937193655102391, -15.15852024261339537 ) ) ;
#2168 = CARTESIAN_POINT ( 'NONE',  ( 190.4976253092930278, 300.6954295735222900, -5.764807383508308902 ) ) ;
#2169 = CARTESIAN_POINT ( 'NONE',  ( 71.88679598306705998, 71.95097395942667617, 2.841373724777338960 ) ) ;
#2170 = ADVANCED_FACE ( 'NONE', ( #58089 ), #90025, .T. ) ;
#2172 = CARTESIAN_POINT ( 'NONE',  ( 64.52297529667023923, 201.3927522451418213, 10.00000000000009592 ) ) ;
#2171 = CARTESIAN_POINT ( 'NONE',  ( 198.0787076940555949, 277.7817408258703722, -16.06897465026475658 ) ) ;
#2173 = CARTESIAN_POINT ( 'NONE',  ( -132.5954152546898115, 108.6868197944956478, 37.50000000000002132 ) ) ;
#2174 = CARTESIAN_POINT ( 'NONE',  ( 184.5677135434892193, 257.8300269524731334, 1.356526893385950006 ) ) ;
#2175 = CARTESIAN_POINT ( 'NONE',  ( 157.8159121039657293, 257.3018173235443555, -17.05074702406642118 ) ) ;
#2176 = DIRECTION ( 'NONE',  ( 0.000000000000000000, -1.000000000000000000, 0.000000000000000000 ) ) ;
#2177 = ORIENTED_EDGE ( 'NONE', *, *, #46472, .F. ) ;
#2178 = EDGE_CURVE ( 'NONE', #53490, #54109, #93351, .T. ) ;
#2179 = CARTESIAN_POINT ( 'NONE',  ( 34.80747863286459420, 184.2365022471902023, 10.00000000000009592 ) ) ;
#2180 = DIRECTION ( 'NONE',  ( 1.000000000000000000, 0.000000000000000000, 0.000000000000000000 ) ) ;
#2181 = CARTESIAN_POINT ( 'NONE',  ( 202.4323889586180201, 280.0238125565655878, 15.69595176008160919 ) ) ;
#2182 = CARTESIAN_POINT ( 'NONE',  ( 142.3387059458346755, 262.1744531367911009, 4.594050593750047540 ) ) ;
#2183 = CARTESIAN_POINT ( 'NONE',  ( 34.65648599653719231, 40.98502408145595410, -5.678558825948271327 ) ) ;
#2185 = CARTESIAN_POINT ( 'NONE',  ( 170.3204754281883879, 263.6398627415188116, 15.82658840592242022 ) ) ;
#2184 = CARTESIAN_POINT ( 'NONE',  ( 164.3186433446439878, 252.3970802647851315, 13.58250517929732659 ) ) ;
#2186 = FACE_OUTER_BOUND ( 'NONE', #78731, .T. ) ;
#2187 = CARTESIAN_POINT ( 'NONE',  ( 21.78279761992806129, 35.68290643055188838, 3.479690158560446702E-15 ) ) ;
#2188 = CARTESIAN_POINT ( 'NONE',  ( 205.8379285891498682, 274.1252448892948905, 10.44730901608240181 ) ) ;
#2189 = CARTESIAN_POINT ( 'NONE',  ( 185.7240582157602091, 259.0518005378353337, -2.331041323071082250 ) ) ;
#2190 = EDGE_CURVE ( 'NONE', #32767, #65750, #49994, .T. ) ;
#2191 = LINE ( 'NONE', #94910, #43241 ) ;
#2192 = VERTEX_POINT ( 'NONE', #42862 ) ;
#2193 = CARTESIAN_POINT ( 'NONE',  ( 188.1018771210319471, 260.4230313274653099, 6.875771660441075461 ) ) ;
#2194 = CARTESIAN_POINT ( 'NONE',  ( 195.2495212664957194, 275.1290853193528392, -16.26662379558266380 ) ) ;
#2195 = CARTESIAN_POINT ( 'NONE',  ( 10.59299460361177125, 21.51421378149917274, -9.188101187500004485 ) ) ;
#2196 = CARTESIAN_POINT ( 'NONE',  ( 166.1085421714060431, 285.6684600996341032, 0.4957535612788783186 ) ) ;
#2197 = CARTESIAN_POINT ( 'NONE',  ( 23.27484393518965788, 15.29860640527292226, -2.839279412974138328 ) ) ;
#2198 = CARTESIAN_POINT ( 'NONE',  ( 160.4797372417389454, 252.6879368424417294, 16.11078530976836731 ) ) ;
#2199 = CLOSED_SHELL ( 'NONE', ( #75150, #7233, #84553, #37271, #22213, #44129, #61711, #25953, #74022, #4386, #1042, #68700, #27934, #56439, #64130, #11572, #38638, #98679, #79121, #731, #36244, #12582, #9749, #91004, #12653, #26400, #28305, #79766, #19607, #61517, #59063, #68707, #71578, #39382 ) ) ;
#2200 = EDGE_CURVE ( 'NONE', #39565, #54118, #11015, .T. ) ;
#2201 = CARTESIAN_POINT ( 'NONE',  ( 152.9031728309432765, 274.9703759552688780, 10.73379579711528820 ) ) ;
#2202 = CARTESIAN_POINT ( 'NONE',  ( 159.9770824720811220, 253.5585604421560788, -16.42166711341322483 ) ) ;
#2203 = VERTEX_POINT ( 'NONE', #35786 ) ;
#2204 = CARTESIAN_POINT ( 'NONE',  ( 32.31170220804710880, 20.78380873178788946, -6.180339887498949025 ) ) ;
#2205 = CARTESIAN_POINT ( 'NONE',  ( 207.6209998424140792, 271.0368748851258260, 6.610167240481342965 ) ) ;
#2206 = DIRECTION ( 'NONE',  ( 0.2033683215378999376, -0.3522442655536480172, -0.9135454576426004225 ) ) ;
#2207 = CARTESIAN_POINT ( 'NONE',  ( 162.7738416911812180, 248.7144313781379310, -11.09964294874192525 ) ) ;
#2208 = CARTESIAN_POINT ( 'NONE',  ( 154.8596847415876994, 262.4221533139083817, 17.65401077761399762 ) ) ;
#2209 = ORIENTED_EDGE ( 'NONE', *, *, #23725, .T. ) ;
#2210 = ORIENTED_EDGE ( 'NONE', *, *, #40001, .T. ) ;
#2211 = CARTESIAN_POINT ( 'NONE',  ( 156.0423484674798829, 277.4799991307274922, -10.51687751763815726 ) ) ;
#2212 = VECTOR ( 'NONE', #60192, 1000.000000000000114 ) ;
#2213 = CARTESIAN_POINT ( 'NONE',  ( 86.43056390414663781, 47.56170780119803254, 10.54448901942590311 ) ) ;
#2214 = ORIENTED_EDGE ( 'NONE', *, *, #3427, .F. ) ;
#2215 = CARTESIAN_POINT ( 'NONE',  ( 77.75543676104368274, 57.50219656113497280, 16.18064258310643311 ) ) ;
#2216 = CARTESIAN_POINT ( 'NONE',  ( 155.3895351254020625, 262.3183883289777896, -17.15772230249129393 ) ) ;
#2217 = ORIENTED_EDGE ( 'NONE', *, *, #99968, .F. ) ;
#2218 = CARTESIAN_POINT ( 'NONE',  ( 38.67678797688638070, 22.73415679381825072, -6.890680421881970419E-14 ) ) ;
#2219 = CARTESIAN_POINT ( 'NONE',  ( 79.44952676368946243, 59.15621205895340040, -16.22681862362401262 ) ) ;
#2220 = AXIS2_PLACEMENT_3D ( 'NONE', #6260, #68551, #76187 ) ;
#2221 = CARTESIAN_POINT ( 'NONE',  ( 21.35627990119762032, 12.73415679381821519, 1.333680081654574804E-15 ) ) ;
#2222 = ORIENTED_EDGE ( 'NONE', *, *, #85455, .T. ) ;
#2223 = CARTESIAN_POINT ( 'NONE',  ( 200.4775477985258760, 283.4096967665721536, 16.80647240730505487 ) ) ;
#2224 = CARTESIAN_POINT ( 'NONE',  ( 166.1020561509257902, 274.0512672971645429, -15.22686407272243336 ) ) ;
#2225 = CARTESIAN_POINT ( 'NONE',  ( 164.2059258710715994, 246.2339888178522926, 7.329631442356459914 ) ) ;
#2226 = CARTESIAN_POINT ( 'NONE',  ( 151.4086371529806740, 275.0624268371906282, -8.516296556100446224 ) ) ;
#2227 = PRODUCT_DEFINITION_SHAPE ( 'NONE', 'NONE',  #80010 ) ;
#2228 = EDGE_LOOP ( 'NONE', ( #75387, #38719, #43530, #51865 ) ) ;
#2229 = CARTESIAN_POINT ( 'NONE',  ( 170.9015845831005436, 255.7403565480592533, -11.60269983186427467 ) ) ;
#2230 = CARTESIAN_POINT ( 'NONE',  ( 40.33962347462181697, 28.45404122711136452, -8.090169943749478065 ) ) ;
#2231 = EDGE_LOOP ( 'NONE', ( #47227, #68601, #60703, #89435 ) ) ;
#2232 = ORIENTED_EDGE ( 'NONE', *, *, #97469, .T. ) ;
#2233 = CARTESIAN_POINT ( 'NONE',  ( 74.06167665414214696, 64.39312597440692798, 13.88171286573246910 ) ) ;
#2234 = ORIENTED_EDGE ( 'NONE', *, *, #80199, .F. ) ;
#2235 = CARTESIAN_POINT ( 'NONE',  ( 160.9377252177449975, 270.8987565486240783, 15.95750095843152039 ) ) ;
#2236 = VERTEX_POINT ( 'NONE', #79936 ) ;
#2237 = CARTESIAN_POINT ( 'NONE',  ( 84.42663183290279960, 49.91580812419739743, -13.73522929182741059 ) ) ;
#2238 = CARTESIAN_POINT ( 'NONE',  ( 168.5704745160775246, 272.7448807985149415, 15.97903247022720485 ) ) ;
#2239 = DIRECTION ( 'NONE',  ( 0.000000000000000000, 0.000000000000000000, 1.000000000000000000 ) ) ;
#2240 = DIRECTION ( 'NONE',  ( -0.8660254037844387076, -0.4999999999999998890, -0.000000000000000000 ) ) ;
#2241 = CARTESIAN_POINT ( 'NONE',  ( 73.13476967714908028, 57.39438153525127007, 15.88807208273858684 ) ) ;
#2242 = DIRECTION ( 'NONE',  ( -0.2938926261462390666, 0.5090369604551334692, 0.8090169943749425663 ) ) ;
#2243 = CARTESIAN_POINT ( 'NONE',  ( 174.5780023577881082, 290.2779860773731002, 6.405149012862879410 ) ) ;
#2244 = LINE ( 'NONE', #33123, #75801 ) ;
#2245 = ORIENTED_EDGE ( 'NONE', *, *, #94471, .F. ) ;
#2246 = CARTESIAN_POINT ( 'NONE',  ( 157.9225728654248257, 276.1116997103654285, -12.95724163227552239 ) ) ;
#2247 = CARTESIAN_POINT ( 'NONE',  ( 22.22900788544320605, 15.76004757982089544, 5.678558825948272215 ) ) ;
#2248 = DIRECTION ( 'NONE',  ( 1.000000000000000000, 0.000000000000000000, 0.000000000000000000 ) ) ;
#2250 = VERTEX_POINT ( 'NONE', #35286 ) ;
#2249 = CARTESIAN_POINT ( 'NONE',  ( 197.9952413503812352, 287.7091776547143809, 17.17611241386010690 ) ) ;
#2251 = ORIENTED_EDGE ( 'NONE', *, *, #23354, .F. ) ;
#2252 = FACE_OUTER_BOUND ( 'NONE', #24255, .T. ) ;
#2253 = DIRECTION ( 'NONE',  ( 0.000000000000000000, 0.000000000000000000, 1.000000000000000000 ) ) ;
#2254 = CARTESIAN_POINT ( 'NONE',  ( 159.3995226465659982, 254.5589234043588078, -16.81133486613867234 ) ) ;
#2255 = DIRECTION ( 'NONE',  ( -0.4527707594502665689, -0.8916269620120450545, 0.000000000000000000 ) ) ;
#2256 = CARTESIAN_POINT ( 'NONE',  ( 200.5621507313343557, 283.2631601884785368, 16.81037192529623425 ) ) ;
#2257 = DIRECTION ( 'NONE',  ( 0.5000000000000013323, -0.8660254037844378194, 0.000000000000000000 ) ) ;
#2258 = ORIENTED_EDGE ( 'NONE', *, *, #93815, .T. ) ;
#2259 = CARTESIAN_POINT ( 'NONE',  ( 153.0051671234592163, 269.7671913317512917, 15.26340949627251042 ) ) ;
#2260 = CARTESIAN_POINT ( 'NONE',  ( 7.095368192108828076, 22.83478043621386178, -8.090169943749479842 ) ) ;
#2261 = FACE_OUTER_BOUND ( 'NONE', #27980, .T. ) ;
#2262 = DIRECTION ( 'NONE',  ( -1.000000000000000000, 0.000000000000000000, 0.000000000000000000 ) ) ;
#2263 = CARTESIAN_POINT ( 'NONE',  ( 6.860117161356284576, 184.7677522451419065, -5.000000000000047962 ) ) ;
#2264 = CARTESIAN_POINT ( 'NONE',  ( 90.72909131299699936, 229.3149278399160949, -9.188101187500095079 ) ) ;
#2265 = EDGE_CURVE ( 'NONE', #61940, #28329, #66575, .T. ) ;
#2266 = CARTESIAN_POINT ( 'NONE',  ( 82.18753490691527475, 40.78579184768809540, -0.6546124752527298085 ) ) ;
#2267 = CARTESIAN_POINT ( 'NONE',  ( 28.41076618884173044, 115.4572390722850912, 59.99999999999999289 ) ) ;
#2268 = FACE_OUTER_BOUND ( 'NONE', #2590, .T. ) ;
#2270 = CARTESIAN_POINT ( 'NONE',  ( 75.76889645089327985, 65.47676480558789081, 14.28475327549652540 ) ) ;
#2269 = CARTESIAN_POINT ( 'NONE',  ( 4.992576338337581632, 179.8149278399160949, -9.188101187500095079 ) ) ;
#2271 = CIRCLE ( 'NONE', #89654, 17.82106496071138935 ) ;
#2272 = CARTESIAN_POINT ( 'NONE',  ( 200.1103929410127762, 284.0456276340304953, 17.67835211026828901 ) ) ;
#2273 = ORIENTED_EDGE ( 'NONE', *, *, #12991, .T. ) ;
#2274 = ORIENTED_EDGE ( 'NONE', *, *, #36758, .F. ) ;
#2275 = CARTESIAN_POINT ( 'NONE',  ( 200.8494367518017611, 267.7546157101949689, -2.866440153229757648 ) ) ;
#2276 = EDGE_CURVE ( 'NONE', #36092, #45167, #84729, .T. ) ;
#2277 =( BOUNDED_CURVE ( )  B_SPLINE_CURVE ( 2, ( #72348, #57102, #10529, #63216, #41404, #17110, #97508, #32315, #25213 ),
 .UNSPECIFIED., .F., .T. ) 
 B_SPLINE_CURVE_WITH_KNOTS ( ( 3, 2, 2, 2, 3 ),
 ( 0.6653225806451612545, 0.6666666666666666297, 0.6693548387096773800, 0.6720430107526881303, 0.6733870967741935054 ),
 .UNSPECIFIED. ) 
 CURVE ( )  GEOMETRIC_REPRESENTATION_ITEM ( )  RATIONAL_B_SPLINE_CURVE ( ( 0.9330127018922194093, 0.9330127018922194093, 1.000000000000000000, 0.8660254037844387076, 1.000000000000000000, 0.8660254037844387076, 1.000000000000000000, 0.9330127018922194093, 0.9330127018922194093 ) ) 
 REPRESENTATION_ITEM ( '' )  );
#2278 = CARTESIAN_POINT ( 'NONE',  ( 79.73293522532485156, 47.11546486241463327, -13.12060147480491601 ) ) ;
#2279 = EDGE_CURVE ( 'NONE', #8428, #64780, #93724, .T. ) ;
#2280 = LINE ( 'NONE', #79315, #64508 ) ;
#2281 = AXIS2_PLACEMENT_3D ( 'NONE', #51796, #83720, #82735 ) ;
#2282 = CARTESIAN_POINT ( 'NONE',  ( 49.74924850768368145, 83.93760989710258968, -10.00000000000000000 ) ) ;
#2283 = CARTESIAN_POINT ( 'NONE',  ( 185.8590724889926378, 286.6100872548933012, 15.79318560268085037 ) ) ;
#2284 = CARTESIAN_POINT ( 'NONE',  ( 174.9671601572613326, 281.6994072225486434, -15.63500919100072473 ) ) ;
#2285 = CARTESIAN_POINT ( 'NONE',  ( 32.16412338207434374, 195.5024278399160949, 9.188101187500095079 ) ) ;
#2286 = CARTESIAN_POINT ( 'NONE',  ( 73.18322933451453594, 226.3927522451419350, 2.944929066748280225E-16 ) ) ;
#2287 = CIRCLE ( 'NONE', #37664, 0.5000000000000004441 ) ;
#2288 = CARTESIAN_POINT ( 'NONE',  ( 93.02964483790795214, 234.5177522451419350, 5.000000000000046185 ) ) ;
#2289 = ORIENTED_EDGE ( 'NONE', *, *, #38391, .T. ) ;
#2290 = CARTESIAN_POINT ( 'NONE',  ( 82.56263159380813477, 44.11904566611071488, 8.977829394507185867 ) ) ;
#2291 = VECTOR ( 'NONE', #19767, 1000.000000000000114 ) ;
#2292 = CARTESIAN_POINT ( 'NONE',  ( 175.5827251679224617, 251.6158941198623040, 0.7410290085531462401 ) ) ;
#2293 = CARTESIAN_POINT ( 'NONE',  ( -5.399381411310668177, 161.5643266524160140, -9.188101187500093303 ) ) ;
#2294 = CARTESIAN_POINT ( 'NONE',  ( 68.97555762870663898, 64.32427639738035907, -11.91833701315977301 ) ) ;
#2295 = DIRECTION ( 'NONE',  ( -0.4330127018922184656, -0.2499999999999943934, -0.8660254037844407060 ) ) ;
#2296 = CARTESIAN_POINT ( 'NONE',  ( 186.7612184996281144, 282.7283756238621777, 16.18745214556588863 ) ) ;
#2297 = CARTESIAN_POINT ( 'NONE',  ( 194.3541845315608612, 294.0156730581561533, -14.67567721756631016 ) ) ;
#2298 = CARTESIAN_POINT ( 'NONE',  ( 73.52959106948154044, 67.84374563276222148, -11.86275638489837014 ) ) ;
#2299 = CARTESIAN_POINT ( 'NONE',  ( 204.7610021263893429, 275.9905362388115577, 13.36619428527026976 ) ) ;
#2300 = CARTESIAN_POINT ( 'NONE',  ( 147.2784190576484491, 275.5532906641692534, 0.2793038414862047958 ) ) ;
#2301 = CARTESIAN_POINT ( 'NONE',  ( 148.3280470635002928, 273.7352816289870248, 9.058704604771318003 ) ) ;
#2302 = ORIENTED_EDGE ( 'NONE', *, *, #92503, .F. ) ;
#2303 = EDGE_CURVE ( 'NONE', #30511, #19593, #61709, .T. ) ;
#2304 = CARTESIAN_POINT ( 'NONE',  ( 8.321535033790441460, 185.6115022471903160, -5.000000000000047962 ) ) ;
#2305 = CARTESIAN_POINT ( 'NONE',  ( 108.0499464844507997, 227.0643266524160424, 9.188101187500095079 ) ) ;
#2306 = CARTESIAN_POINT ( 'NONE',  ( 18.92609651878039756, 19.43085787977762280, -9.188101187500008038 ) ) ;
#2307 = CARTESIAN_POINT ( 'NONE',  ( 75.25521838011508180, 66.92519264401985879, 13.27308740013157262 ) ) ;
#2308 = CARTESIAN_POINT ( 'NONE',  ( 40.63510790894943625, 194.2677522451418781, 10.00000000000009592 ) ) ;
#2310 = CARTESIAN_POINT ( 'NONE',  ( 162.1227137712282342, 251.8422180177273901, -14.11218862277787345 ) ) ;
#2309 = CARTESIAN_POINT ( 'NONE',  ( 195.9713281756800427, 291.2146981034049418, 17.52210387885178022 ) ) ;
#2311 = EDGE_CURVE ( 'NONE', #56696, #93369, #14094, .T. ) ;
#2312 = CARTESIAN_POINT ( 'NONE',  ( 150.8963010474469684, 269.2869352420495943, -15.14557988994318016 ) ) ;
#2313 = DIRECTION ( 'NONE',  ( 0.4999999999999998890, -0.8660254037844385966, 0.000000000000000000 ) ) ;
#2314 = CARTESIAN_POINT ( 'NONE',  ( 149.1939152435731728, 272.2355539484436235, -11.44223522189843933 ) ) ;
#2315 = CARTESIAN_POINT ( 'NONE',  ( -10.80656490723494123, 24.88181024604956804, -10.00000000000000000 ) ) ;
#2316 = CARTESIAN_POINT ( 'NONE',  ( 204.0100964097678968, 276.7670827000571876, 13.67351780134896266 ) ) ;
#2317 = DIRECTION ( 'NONE',  ( 0.000000000000000000, 0.000000000000000000, 1.000000000000000000 ) ) ;
#2318 = ORIENTED_EDGE ( 'NONE', *, *, #21665, .T. ) ;
#2319 = CARTESIAN_POINT ( 'NONE',  ( 189.3522642941718743, 265.7560121150649479, 10.75527977382243527 ) ) ;
#2320 = CARTESIAN_POINT ( 'NONE',  ( 177.7074169911321349, 279.7993272485674652, 15.60716354588072718 ) ) ;
#2321 = CARTESIAN_POINT ( 'NONE',  ( 165.7666411575162329, 269.9458407505568402, -16.28142105735056333 ) ) ;
#2322 = EDGE_CURVE ( 'NONE', #76205, #22170, #43600, .T. ) ;
#2323 = CARTESIAN_POINT ( 'NONE',  ( 79.86762560990425186, 52.96440835099240019, 15.56858714322070014 ) ) ;
#2324 = LINE ( 'NONE', #48409, #843 ) ;
#2325 = DIRECTION ( 'NONE',  ( -0.000000000000000000, 0.000000000000000000, 1.000000000000000000 ) ) ;
#2326 = CARTESIAN_POINT ( 'NONE',  ( 75.01736285511192648, 53.01766956676284792, -16.01582039744900143 ) ) ;
#2327 = CARTESIAN_POINT ( 'NONE',  ( 152.8134625983922490, 265.9663140294953791, 17.57333028169644251 ) ) ;
#2328 = CARTESIAN_POINT ( 'NONE',  ( -22.42236680055709641, 157.8615022471902591, 0.000000000000000000 ) ) ;
#2329 = CARTESIAN_POINT ( 'NONE',  ( 35.68911091587340678, 42.64646525600393545, -2.839279412974133887 ) ) ;
#2330 = CARTESIAN_POINT ( 'NONE',  ( 187.4322965893034905, 284.5321960278562301, 17.17379807122665625 ) ) ;
#2331 = VERTEX_POINT ( 'NONE', #7882 ) ;
#2332 = CARTESIAN_POINT ( 'NONE',  ( 167.8081459420055523, 280.8398059720881861, 11.95526808680748942 ) ) ;
#2333 = CARTESIAN_POINT ( 'NONE',  ( 148.3625667886952044, 273.6754917110858401, -8.960758510948144462 ) ) ;
#2334 = CARTESIAN_POINT ( 'NONE',  ( 87.51038571601205263, 44.12602541333317419, -4.835627537363936135 ) ) ;
#2335 = EDGE_LOOP ( 'NONE', ( #36448, #29872, #78999, #49639 ) ) ;
#2336 = CARTESIAN_POINT ( 'NONE',  ( 78.82690945070837074, 60.06733921958858247, 16.11100571342160492 ) ) ;
#2337 = CARTESIAN_POINT ( 'NONE',  ( 188.6646623341742668, 293.7383209822070285, 12.96511213459449863 ) ) ;
#2338 = CARTESIAN_POINT ( 'NONE',  ( 28.28448313147312021, 16.73415679381822230, 1.333680081654574804E-15 ) ) ;
#2339 = CARTESIAN_POINT ( 'NONE',  ( 76.06280709947594687, 52.62385153157702433, -15.89955354223746298 ) ) ;
#2340 = CARTESIAN_POINT ( 'NONE',  ( 202.8535267948003593, 279.2943804273081696, -15.36804658072946062 ) ) ;
#2341 = ORIENTED_EDGE ( 'NONE', *, *, #58740, .T. ) ;
#2342 = B_SPLINE_CURVE_WITH_KNOTS ( 'NONE', 3,
 ( #81861, #2853, #33743, #87507, #18040, #57012, #87991, #18539, #89958, #45304 ),
 .UNSPECIFIED., .F., .F.,
 ( 4, 2, 2, 2, 4 ),
 ( 0.001222343323482912199, 0.001313399527160096208, 0.001404455730837280217, 0.001586568138191648235, 0.001950792952900384488 ),
 .UNSPECIFIED. ) ;
#2343 = VERTEX_POINT ( 'NONE', #85938 ) ;
#2344 = DIRECTION ( 'NONE',  ( 0.8263106059122495850, 0.5632146860273895550, 0.000000000000000000 ) ) ;
#2345 = ORIENTED_EDGE ( 'NONE', *, *, #52749, .T. ) ;
#2346 = CARTESIAN_POINT ( 'NONE',  ( 81.19301662773271744, 55.65398007790845014, 16.37810844063417548 ) ) ;
#2347 = CIRCLE ( 'NONE', #75171, 7.499999999999996447 ) ;
#2349 = ORIENTED_EDGE ( 'NONE', *, *, #73320, .F. ) ;
#2348 = ADVANCED_FACE ( 'NONE', ( #8376 ), #70664, .T. ) ;
#2350 = CARTESIAN_POINT ( 'NONE',  ( 88.32078559155080200, 44.16791947909882765, 0.3596700509409204716 ) ) ;
#2351 = CARTESIAN_POINT ( 'NONE',  ( 78.95994887262315842, 51.98449323110317266, 15.44357915373326406 ) ) ;
#2352 = ORIENTED_EDGE ( 'NONE', *, *, #58095, .T. ) ;
#2353 = CARTESIAN_POINT ( 'NONE',  ( 185.7214944442812907, 282.3173832595768431, -17.29588648652288185 ) ) ;
#2354 = CARTESIAN_POINT ( 'NONE',  ( 164.5379227956242687, 245.6589532765702870, -2.440899697315300987 ) ) ;
#2355 = CARTESIAN_POINT ( 'NONE',  ( 147.1970330202780701, 275.6942554159216456, -7.017118315561711839 ) ) ;
#2356 = CARTESIAN_POINT ( 'NONE',  ( -107.5954152546897262, 65.38554960527366688, -21.50000000000000000 ) ) ;
#2357 = CARTESIAN_POINT ( 'NONE',  ( 192.9523350703175311, 296.4437475495926719, -13.35611922184540923 ) ) ;
#2360 = ADVANCED_FACE ( 'NONE', ( #38759 ), #24562, .T. ) ;
#2359 = CARTESIAN_POINT ( 'NONE',  ( 152.9251141908703175, 265.7729277985770864, -16.20110192949203309 ) ) ;
#2358 = B_SPLINE_CURVE_WITH_KNOTS ( 'NONE', 3,
 ( #3094, #55728, #86717, #79100 ),
 .UNSPECIFIED., .F., .F.,
 ( 4, 4 ),
 ( 0.04814469201508995294, 0.04887120950165273203 ),
 .UNSPECIFIED. ) ;
#2361 = DIRECTION ( 'NONE',  ( -0.000000000000000000, 0.000000000000000000, -1.000000000000000000 ) ) ;
#2362 = VECTOR ( 'NONE', #18549, 1000.000000000000000 ) ;
#2363 = CARTESIAN_POINT ( 'NONE',  ( 157.7753659096992180, 281.3564795509028613, 2.871017466566028187 ) ) ;
#2364 = CARTESIAN_POINT ( 'NONE',  ( 120.1739550416679378, 246.3149278399160949, 9.188101187500093303 ) ) ;
#2365 = ORIENTED_EDGE ( 'NONE', *, *, #11432, .F. ) ;
#2366 = CARTESIAN_POINT ( 'NONE',  ( 70.67451223566608576, 61.02758652436570941, -14.45160611066157941 ) ) ;
#2367 = DIRECTION ( 'NONE',  ( 0.5000000000000048850, -0.8660254037844358210, 0.000000000000000000 ) ) ;
#2368 = CARTESIAN_POINT ( 'NONE',  ( 41.76871284172324295, 36.06628583063844928, -9.188101187500006262 ) ) ;
#2369 = ORIENTED_EDGE ( 'NONE', *, *, #47652, .F. ) ;
#2371 = ORIENTED_EDGE ( 'NONE', *, *, #69900, .T. ) ;
#2370 = CARTESIAN_POINT ( 'NONE',  ( 21.20711791317337003, 34.01751292744057054, 6.180339887498949913 ) ) ;
#2372 = CARTESIAN_POINT ( 'NONE',  ( 203.5267646298421482, 276.4525192296148930, 13.67989786268708308 ) ) ;
#2373 = CARTESIAN_POINT ( 'NONE',  ( 177.9747879117682317, 253.3556439134052027, 1.401624406440116877 ) ) ;
#2374 = CARTESIAN_POINT ( 'NONE',  ( 171.2053697672408816, 287.8281772831969647, -4.637733492338565355 ) ) ;
#2375 = CARTESIAN_POINT ( 'NONE',  ( 192.6815422931747435, 296.9127743979267962, 12.45400196617769595 ) ) ;
#2376 = PLANE ( 'NONE',  #7947 ) ;
#2377 = CARTESIAN_POINT ( 'NONE',  ( 76.87325692288003154, 51.52439226058535837, -16.07951750168037819 ) ) ;
#2378 = CARTESIAN_POINT ( 'NONE',  ( 173.5110880923138836, 287.6292713490308302, -9.896673617075110840 ) ) ;
#2379 = CARTESIAN_POINT ( 'NONE',  ( 174.4023533683497362, 281.7821760571821983, 14.15141610718057485 ) ) ;
#2380 = DIRECTION ( 'NONE',  ( 0.000000000000000000, 0.000000000000000000, 1.000000000000000000 ) ) ;
#2381 = VERTEX_POINT ( 'NONE', #54441 ) ;
#2382 = CARTESIAN_POINT ( 'NONE',  ( 194.3442947553755005, 294.0328026529847421, -15.97648891113594871 ) ) ;
#2383 = CARTESIAN_POINT ( 'NONE',  ( 5.488910272030937065, 180.6427522451419350, -10.00000000000009592 ) ) ;
#2384 = VERTEX_POINT ( 'NONE', #69662 ) ;
#2385 = CARTESIAN_POINT ( 'NONE',  ( 164.0628648187332885, 278.0734779406835173, 13.23368607355390481 ) ) ;
#2386 = CARTESIAN_POINT ( 'NONE',  ( 205.1070740870186455, 269.0972391188071242, -3.016557977693823389 ) ) ;
#2387 = CARTESIAN_POINT ( 'NONE',  ( 151.9037511824772082, 267.5419804220855440, -15.52605960223452186 ) ) ;
#2388 = CARTESIAN_POINT ( 'NONE',  ( 190.3572031550745294, 300.9386478791372497, 3.093832330100951378 ) ) ;
#2389 = CARTESIAN_POINT ( 'NONE',  ( 163.2835940097493790, 247.8315144631017404, 11.08416305054517359 ) ) ;
#2391 = CARTESIAN_POINT ( 'NONE',  ( 152.8134590189604580, 275.7618923605953114, -8.624218497726184651 ) ) ;
#2390 = CARTESIAN_POINT ( 'NONE',  ( 153.1733743200604181, 270.1408812147403751, 14.03834090807932888 ) ) ;
#2392 = CARTESIAN_POINT ( 'NONE',  ( 200.6583719735737645, 283.0965001081523269, -17.35266956530146132 ) ) ;
#2393 = ORIENTED_EDGE ( 'NONE', *, *, #31168, .T. ) ;
#2394 = CARTESIAN_POINT ( 'NONE',  ( 166.7135982584813405, 281.2722395198167646, -10.95386632010279193 ) ) ;
#2395 = CARTESIAN_POINT ( 'NONE',  ( 1.326623512302396168, 183.1199935810941213, 2.679491924311264039 ) ) ;
#2396 = CARTESIAN_POINT ( 'NONE',  ( 42.54989241151534429, 183.8262482093457493, 3.021315404115420679E-15 ) ) ;
#2397 = EDGE_CURVE ( 'NONE', #36600, #21409, #76285, .T. ) ;
#2398 = CARTESIAN_POINT ( 'NONE',  ( 74.17388174154397973, 65.32774866087831356, -13.41372763693923531 ) ) ;
#2399 = CARTESIAN_POINT ( 'NONE',  ( -105.0000000000000000, 10.00000000000000000, 54.99999999999999289 ) ) ;
#2400 = ADVANCED_FACE ( 'NONE', ( #8867 ), #55484, .T. ) ;
#2401 = CARTESIAN_POINT ( 'NONE',  ( 73.76584831522595209, 68.38082682530665579, 11.49424229391075514 ) ) ;
#2402 = PLANE ( 'NONE',  #90238 ) ;
#2403 = CARTESIAN_POINT ( 'NONE',  ( 67.38523018514564455, 69.28993244173518917, 2.473534599136319123 ) ) ;
#2404 = CARTESIAN_POINT ( 'NONE',  ( -9.134289513013563067, 165.5333772461660828, 9.188101187500095079 ) ) ;
#2405 = EDGE_CURVE ( 'NONE', #34725, #23455, #44181, .T. ) ;
#2406 = CARTESIAN_POINT ( 'NONE',  ( 85.91165145656356117, 232.6589784336661637, -6.496448406907675876E-16 ) ) ;
#2407 = CARTESIAN_POINT ( 'NONE',  ( 88.06692388374393943, 44.73466778012474521, -4.429792403987857341 ) ) ;
#2408 = CARTESIAN_POINT ( 'NONE',  ( 147.8927139526707606, 275.3200074130446637, 4.767002118840804492 ) ) ;
#2409 = ADVANCED_FACE ( 'NONE', ( #94401 ), #47256, .F. ) ;
#2410 = FACE_OUTER_BOUND ( 'NONE', #81383, .T. ) ;
#2411 = CARTESIAN_POINT ( 'NONE',  ( 77.71263964979601724, 53.15247193762592559, 15.85337299538524469 ) ) ;
#2412 = CARTESIAN_POINT ( 'NONE',  ( 164.1968994398425536, 284.1293336553245581, 5.791912491216440806 ) ) ;
#2414 = CARTESIAN_POINT ( 'NONE',  ( 76.47997935286269922, 51.56731111080835461, 15.64421333830926741 ) ) ;
#2413 = CARTESIAN_POINT ( 'NONE',  ( -110.0000000000000000, 0.000000000000000000, 59.99999999999999289 ) ) ;
#2415 = CARTESIAN_POINT ( 'NONE',  ( 177.8607531624229523, 289.9922794532071180, 9.730199643517920549 ) ) ;
#2416 = CARTESIAN_POINT ( 'NONE',  ( 70.96429761875693032, 61.15374941679502996, 14.99935025239129871 ) ) ;
#2417 = CARTESIAN_POINT ( 'NONE',  ( 164.6890007341313265, 245.3972786111733626, -5.485860350477558711 ) ) ;
#2418 = LINE ( 'NONE', #65685, #91587 ) ;
#2419 = CARTESIAN_POINT ( 'NONE',  ( 79.14484663501158934, 45.92919831353032833, -13.14721640033899241 ) ) ;
#2420 = CIRCLE ( 'NONE', #34724, 0.1418229129680828593 ) ;
#2421 = CARTESIAN_POINT ( 'NONE',  ( 207.2683629543511756, 271.6476598918739001, -6.694388351944108528 ) ) ;
#2422 = CARTESIAN_POINT ( 'NONE',  ( 73.65406247650449245, 69.69847601991219221, 9.512545074604176421 ) ) ;
#2423 = CARTESIAN_POINT ( 'NONE',  ( 51.37958267218910891, 188.2202760586659451, -5.415160957724236172E-17 ) ) ;
#2424 = EDGE_CURVE ( 'NONE', #77804, #11947, #65853, .T. ) ;
#2425 = CARTESIAN_POINT ( 'NONE',  ( 175.5502453897478574, 265.0413399349590691, -16.57660258381358531 ) ) ;
#2426 = CARTESIAN_POINT ( 'NONE',  ( 65.85835811776894388, 199.6423013555410080, -4.594050593750043987 ) ) ;
#2427 = CARTESIAN_POINT ( 'NONE',  ( 207.1158949475991164, 271.9117422260973740, -5.823035679195911918 ) ) ;
#2429 = CARTESIAN_POINT ( 'NONE',  ( 76.97945238447553606, 53.12258697838318966, -16.36430810493287424 ) ) ;
#2428 = AXIS2_PLACEMENT_3D ( 'NONE', #79203, #33564, #78168 ) ;
#2430 = CARTESIAN_POINT ( 'NONE',  ( 85.19480112191604348, 49.06367757593693568, -12.43476213627227089 ) ) ;
#2432 = CARTESIAN_POINT ( 'NONE',  ( 200.2066897919534938, 283.8788365955923609, 16.98287317603211477 ) ) ;
#2431 = CARTESIAN_POINT ( 'NONE',  ( 167.6502826215564994, 287.3877002845107995, 4.891367078714356609 ) ) ;
#2433 = CARTESIAN_POINT ( 'NONE',  ( 176.6519481562020246, 270.0898229012302068, -17.23250062992003606 ) ) ;
#2434 = CARTESIAN_POINT ( 'NONE',  ( 29.31840136419365450, 25.43085787977764056, -9.188101187500008038 ) ) ;
#2435 = CARTESIAN_POINT ( 'NONE',  ( -25.57896346879523364, 41.67372163389741502, 59.99999999999999289 ) ) ;
#2436 = CARTESIAN_POINT ( 'NONE',  ( 79.40534888915426848, 47.81769003582009958, -13.62930039999817033 ) ) ;
#2437 = VERTEX_POINT ( 'NONE', #70557 ) ;
#2438 = CARTESIAN_POINT ( 'NONE',  ( 13.26084062165525523, 25.84336893147755276, -7.433330006724137462 ) ) ;
#2439 = CARTESIAN_POINT ( 'NONE',  ( 73.67938972387338481, 213.3458772461660544, 9.188101187500095079 ) ) ;
#2440 = LINE ( 'NONE', #86577, #73966 ) ;
#2441 = CARTESIAN_POINT ( 'NONE',  ( 172.5631314460892156, 290.7196233979062754, -0.4289259863806654249 ) ) ;
#2442 = CARTESIAN_POINT ( 'NONE',  ( -31.55997627504339320, 93.43085135866357405, 11.06573829301134282 ) ) ;
#2443 = CARTESIAN_POINT ( 'NONE',  ( 153.7538396745889031, 264.3375331552495027, 18.11269671319490371 ) ) ;
#2444 = ORIENTED_EDGE ( 'NONE', *, *, #32642, .T. ) ;
#2445 = CARTESIAN_POINT ( 'NONE',  ( 86.50957498950597824, 47.24826369376732771, 10.71680696257866394 ) ) ;
#2446 = CARTESIAN_POINT ( 'NONE',  ( 189.7817514553160834, 286.5108602900515393, 16.56304429735581962 ) ) ;
#2447 = CARTESIAN_POINT ( 'NONE',  ( 124.8019518427975356, 232.8615022471901739, 5.000000000000051514 ) ) ;
#2448 = CARTESIAN_POINT ( 'NONE',  ( 75.21948224091696034, 53.29821691096760361, 16.02883939873531105 ) ) ;
#2449 = ORIENTED_EDGE ( 'NONE', *, *, #87057, .T. ) ;
#2450 = CARTESIAN_POINT ( 'NONE',  ( 82.12724052554919751, 54.15063765581061972, 15.62772812625948582 ) ) ;
#2451 = ORIENTED_EDGE ( 'NONE', *, *, #14087, .F. ) ;
#2452 = CARTESIAN_POINT ( 'NONE',  ( 202.9216520459657147, 279.1763840310111391, 15.75371595331685803 ) ) ;
#2453 = DIRECTION ( 'NONE',  ( 0.08592509128337570690, -0.9963016002636669866, 0.000000000000000000 ) ) ;
#2454 = CARTESIAN_POINT ( 'NONE',  ( 153.4361244163197000, 264.8878321249116539, -17.23169627811277493 ) ) ;
#2455 = EDGE_LOOP ( 'NONE', ( #48973, #51200, #92435, #11325 ) ) ;
#2456 = CARTESIAN_POINT ( 'NONE',  ( 173.3140550308864078, 251.6862458793178234, -0.2129259167810379494 ) ) ;
#2457 = ORIENTED_EDGE ( 'NONE', *, *, #68326, .T. ) ;
#2458 = CARTESIAN_POINT ( 'NONE',  ( 72.50318959249285911, 71.67715071215087619, 6.033079537162470807 ) ) ;
#2459 = CARTESIAN_POINT ( 'NONE',  ( 170.6745590487207096, 250.4173498944666107, 3.281460215579040884 ) ) ;
#2460 = CARTESIAN_POINT ( 'NONE',  ( 148.4682235075532901, 274.1715865626006803, 7.806811515100825716 ) ) ;
#2461 = EDGE_CURVE ( 'NONE', #55260, #55159, #55344, .T. ) ;
#2462 = ORIENTED_EDGE ( 'NONE', *, *, #78688, .F. ) ;
#2463 = VECTOR ( 'NONE', #73111, 1000.000000000000227 ) ;
#2464 = CARTESIAN_POINT ( 'NONE',  ( 28.76090768559789979, 38.64646525600391413, -2.839279412974133887 ) ) ;
#2465 = CARTESIAN_POINT ( 'NONE',  ( 80.08281979147555774, 44.31827980528016298, 11.46924030742146883 ) ) ;
#2466 = CARTESIAN_POINT ( 'NONE',  ( 74.95832312740790826, 66.37231070943815325, -13.09348500807924509 ) ) ;
#2467 = CARTESIAN_POINT ( 'NONE',  ( 82.43495555929192165, 48.51766243573657533, -13.06424617837711644 ) ) ;
#2468 = CARTESIAN_POINT ( 'NONE',  ( 168.1001124519679877, 276.8241359285356111, 15.41633075000079423 ) ) ;
#2469 = PLANE ( 'NONE',  #31919 ) ;
#2470 = EDGE_LOOP ( 'NONE', ( #75576, #27975, #83260, #5207 ) ) ;
#2471 = ORIENTED_EDGE ( 'NONE', *, *, #85259, .F. ) ;
#2472 = CARTESIAN_POINT ( 'NONE',  ( 183.1096229524326020, 295.7703253833122403, 0.8402911052648339707 ) ) ;
#2474 = CARTESIAN_POINT ( 'NONE',  ( 87.85430303351097336, 43.89859490532884223, 0.3596698246726173775 ) ) ;
#2473 = CARTESIAN_POINT ( 'NONE',  ( 67.63749347275029322, 65.82635250199255950, 10.53419884080181035 ) ) ;
#2475 = DIRECTION ( 'NONE',  ( 1.000000000000000000, 0.000000000000000000, 0.000000000000000000 ) ) ;
#2476 = CARTESIAN_POINT ( 'NONE',  ( 194.4459411895494725, 293.8567458645873103, 14.31012567920753042 ) ) ;
#2477 = CARTESIAN_POINT ( 'NONE',  ( 185.3991843159095367, 292.5114241635241115, -11.58673315860843189 ) ) ;
#2478 = CARTESIAN_POINT ( 'NONE',  ( 122.1835217032046330, 252.8967562850346553, -4.648177544792955347E-16 ) ) ;
#2479 = CARTESIAN_POINT ( 'NONE',  ( 206.7587669622944304, 270.1143081540075173, 3.338494309489741241 ) ) ;
#2480 = DIRECTION ( 'NONE',  ( 0.8660254037844380415, -0.5000000000000011102, 0.000000000000000000 ) ) ;
#2481 = CARTESIAN_POINT ( 'NONE',  ( 86.31820828217628616, 211.4548013555409796, -4.594050593750042211 ) ) ;
#2482 = ORIENTED_EDGE ( 'NONE', *, *, #56346, .F. ) ;
#2483 = CARTESIAN_POINT ( 'NONE',  ( 149.9428439900298144, 271.4018792907216380, 11.96959320080079259 ) ) ;
#2484 = CARTESIAN_POINT ( 'NONE',  ( 78.08890065365325484, 61.45839965263433413, -16.15943835942215756 ) ) ;
#2485 = ORIENTED_EDGE ( 'NONE', *, *, #31531, .F. ) ;
#2486 = CARTESIAN_POINT ( 'NONE',  ( 164.9747645813434644, 264.6250227286296877, -16.82035684215298232 ) ) ;
#2487 = ORIENTED_EDGE ( 'NONE', *, *, #17553, .T. ) ;
#2488 = CARTESIAN_POINT ( 'NONE',  ( 80.44297273222078104, 44.73620253183693762, -11.65665792485825669 ) ) ;
#2489 = DIRECTION ( 'NONE',  ( 0.8660254037844395958, 0.4999999999999985567, 0.000000000000000000 ) ) ;
#2490 = CARTESIAN_POINT ( 'NONE',  ( 147.0721334091522294, 275.9105878882373304, 0.7242168585908188572 ) ) ;
#2491 = CARTESIAN_POINT ( 'NONE',  ( 82.41630873631589793, 41.31828431233920895, -3.367117793111288560 ) ) ;
#2492 = CARTESIAN_POINT ( 'NONE',  ( 78.95335204094531889, 48.73056600144941086, -14.23687683951352412 ) ) ;
#2493 = CARTESIAN_POINT ( 'NONE',  ( 207.5573902749007971, 271.1470498879065190, 2.528158314636208548 ) ) ;
#2494 = CARTESIAN_POINT ( 'NONE',  ( 86.23641098298274699, 232.8464784336661353, 1.353441290958777327E-15 ) ) ;
#2495 = ORIENTED_EDGE ( 'NONE', *, *, #3717, .T. ) ;
#2496 = CIRCLE ( 'NONE', #12172, 17.82106496071138224 ) ;
#2497 = ORIENTED_EDGE ( 'NONE', *, *, #47982, .F. ) ;
#2498 = CARTESIAN_POINT ( 'NONE',  ( 5.968649350820482979, 188.6868197944959320, -37.49999999999994316 ) ) ;
#2499 = B_SPLINE_SURFACE_WITH_KNOTS ( 'NONE', 3, 1, ( 
 ( #45972, #76888 ),
 ( #63193, #69789 ),
 ( #8994, #39865 ),
 ( #399, #85030 ),
 ( #46479, #46998 ),
 ( #99712, #84538 ),
 ( #53584, #94134 ),
 ( #31287, #15083 ),
 ( #70802, #16094 ),
 ( #77409, #8014 ),
 ( #38886, #54569 ),
 ( #62174, #77912 ),
 ( #93126, #38381 ),
 ( #8501, #1411 ),
 ( #32292, #30804 ),
 ( #68788, #85553 ),
 ( #39371, #70285 ),
 ( #24690, #55572 ),
 ( #897, #7488 ),
 ( #86556, #62679 ),
 ( #93632, #24199 ),
 ( #69294, #55080 ),
 ( #61684, #17088 ),
 ( #76420, #61186 ),
 ( #6992, #92634 ),
 ( #30301, #23183 ),
 ( #54075, #37877 ),
 ( #56589, #2414 ),
 ( #17596, #33292 ),
 ( #63697, #95145 ),
 ( #25710, #95655 ) ),
 .UNSPECIFIED., .F., .F., .F.,
 ( 4, 3, 3, 3, 3, 3, 3, 3, 3, 3, 4 ),
 ( 2, 2 ),
 ( 0.000000000000000000, 0.1122669598086765003, 0.2243161639709622401, 0.3396355846219112906, 0.4553962076585172380, 0.5677860799922342938, 0.6749047109689697566, 0.7773884377078434937, 0.8775581155834070168, 0.9782364162377823469, 1.000000000000000000 ),
 ( 0.000000000000000000, 1.000000000000000000 ),
 .UNSPECIFIED. ) ;
#2500 = CARTESIAN_POINT ( 'NONE',  ( 208.3226489551340990, 269.8215829728092103, -1.240262689467544366 ) ) ;
#2501 = EDGE_LOOP ( 'NONE', ( #57636, #79002, #91081, #29969 ) ) ;
#2502 =( GEOMETRIC_REPRESENTATION_CONTEXT ( 3 ) GLOBAL_UNCERTAINTY_ASSIGNED_CONTEXT ( ( #47345 ) ) GLOBAL_UNIT_ASSIGNED_CONTEXT ( ( #60965, #8282, #62449 ) ) REPRESENTATION_CONTEXT ( 'NONE', 'WORKASPACE' ) );
#2503 = CARTESIAN_POINT ( 'NONE',  ( 47.78135487164287554, 106.4364430393875267, 10.00000000000000000 ) ) ;
#2504 = CARTESIAN_POINT ( 'NONE',  ( 71.61522850875250867, 69.38231080192815625, -8.322070056553526385 ) ) ;
#2505 = CARTESIAN_POINT ( 'NONE',  ( 87.76310869853918462, 45.07707962072153407, -6.704660406813174767 ) ) ;
#2506 = LINE ( 'NONE', #19217, #63935 ) ;
#2507 = CARTESIAN_POINT ( 'NONE',  ( 88.26308438319264837, 44.34169033064829080, 4.149168146237482091 ) ) ;
#2508 = VERTEX_POINT ( 'NONE', #48265 ) ;
#2509 = CARTESIAN_POINT ( 'NONE',  ( 157.0808507922293131, 258.5749808621497436, 16.84357500595720580 ) ) ;
#2510 = CARTESIAN_POINT ( 'NONE',  ( 157.5154073855773902, 274.2076768598925582, 13.14496121706235598 ) ) ;
#2511 = CARTESIAN_POINT ( 'NONE',  ( 159.8732321751776624, 253.7384344327741132, -15.51998349828054202 ) ) ;
#2512 = CARTESIAN_POINT ( 'NONE',  ( 191.4622417012445226, 271.4753688487222689, 14.17392657159957103 ) ) ;
#2513 = CARTESIAN_POINT ( 'NONE',  ( 177.7195682713364988, 285.0153326636437896, 13.03457619952185098 ) ) ;
#2514 = ADVANCED_FACE ( 'NONE', ( #86321 ), #71585, .T. ) ;
#2515 = CARTESIAN_POINT ( 'NONE',  ( 198.8010046576729337, 284.7357643445890290, -17.59468233100604806 ) ) ;
#2516 = DIRECTION ( 'NONE',  ( 1.000000000000000000, 1.830829162166278276E-15, -8.881784197001251337E-16 ) ) ;
#2517 = ORIENTED_EDGE ( 'NONE', *, *, #5755, .T. ) ;
#2518 = EDGE_CURVE ( 'NONE', #22379, #61940, #42592, .T. ) ;
#2519 = CARTESIAN_POINT ( 'NONE',  ( 0.02212491418958350761, 177.4865022471903160, 10.00000000000009415 ) ) ;
#2520 = FACE_OUTER_BOUND ( 'NONE', #32195, .T. ) ;
#2521 = CYLINDRICAL_SURFACE ( 'NONE', #94827, 10.00000000000001066 ) ;
#2522 = CARTESIAN_POINT ( 'NONE',  ( 187.6695521735992997, 265.9902340032063535, -11.83501235947671404 ) ) ;
#2523 = CARTESIAN_POINT ( 'NONE',  ( 77.95656630038031665, 61.79485276963480089, 16.07049939491896851 ) ) ;
#2524 = CARTESIAN_POINT ( 'NONE',  ( 178.7342092137616305, 291.7075392037597226, -6.124219736295335004 ) ) ;
#2525 = CARTESIAN_POINT ( 'NONE',  ( -19.65312891409030271, 93.06504152958497400, 10.00000000000000888 ) ) ;
#2526 = EDGE_CURVE ( 'NONE', #91993, #81911, #518, .T. ) ;
#2527 = ORIENTED_EDGE ( 'NONE', *, *, #11654, .T. ) ;
#2528 = AXIS2_PLACEMENT_3D ( 'NONE', #87175, #94239, #88163 ) ;
#2529 = CARTESIAN_POINT ( 'NONE',  ( 206.9878665138179770, 272.1334939782196329, 6.566295309274049252 ) ) ;
#2531 = CARTESIAN_POINT ( 'NONE',  ( 183.7457943646905676, 265.5583575750509908, 13.24080542652859904 ) ) ;
#2530 = CARTESIAN_POINT ( 'NONE',  ( 177.3863179211383567, 264.6869915026061335, -15.25279286059338624 ) ) ;
#2532 = CARTESIAN_POINT ( 'NONE',  ( 199.1563789199090877, 281.8025795620720260, -16.58559166199236756 ) ) ;
#2533 = CARTESIAN_POINT ( 'NONE',  ( 36.78662229117171734, 22.20801979619930933, -3.090169943749474069 ) ) ;
#2534 = DIRECTION ( 'NONE',  ( 1.000000000000000000, 0.000000000000000000, 0.000000000000000000 ) ) ;
#2535 = CARTESIAN_POINT ( 'NONE',  ( 168.5628821761766289, 273.2637907955208902, 15.98574214255321380 ) ) ;
#2536 = CARTESIAN_POINT ( 'NONE',  ( 180.9278271019973374, 273.2195462377731019, 17.49290913295951100 ) ) ;
#2537 = DIRECTION ( 'NONE',  ( -1.000000000000000000, 0.000000000000000000, 0.000000000000000000 ) ) ;
#2538 = VECTOR ( 'NONE', #67777, 999.9999999999998863 ) ;
#2539 = CARTESIAN_POINT ( 'NONE',  ( 178.3571982967953602, 292.6181790745828835, -7.174879954037646002 ) ) ;
#2540 = CARTESIAN_POINT ( 'NONE',  ( 190.8429499865819707, 278.0757709512191695, -17.64141544901220371 ) ) ;
#2541 = CARTESIAN_POINT ( 'NONE',  ( 2.042590532755589994, 181.1744531367911577, 4.594050593750047540 ) ) ;
#2542 = CARTESIAN_POINT ( 'NONE',  ( 81.86138060899043012, 46.81554957853204968, 12.09595161180856060 ) ) ;
#2543 = ORIENTED_EDGE ( 'NONE', *, *, #40393, .T. ) ;
#2544 = CARTESIAN_POINT ( 'NONE',  ( 177.7380108946867665, 256.6765468135970423, 8.337886873569251733 ) ) ;
#2545 = LINE ( 'NONE', #70423, #19259 ) ;
#2546 = CARTESIAN_POINT ( 'NONE',  ( 71.95319803722021845, 72.64445964553972601, -0.8526933041427806614 ) ) ;
#2547 = CARTESIAN_POINT ( 'NONE',  ( 26.64321143294854721, 192.3149278399161233, 9.188101187500093303 ) ) ;
#2548 = CARTESIAN_POINT ( 'NONE',  ( 181.6779114849496466, 276.3290641470016453, -17.56019397242378588 ) ) ;
#2549 = CARTESIAN_POINT ( 'NONE',  ( 29.86737195101774844, 39.01751292744058475, 6.180339887498949913 ) ) ;
#2550 = CARTESIAN_POINT ( 'NONE',  ( 179.5516160758070612, 292.2552566163012671, 6.096423350851510214 ) ) ;
#2551 = CARTESIAN_POINT ( 'NONE',  ( -48.71813016832984289, 30.75580926756359901, 10.00000000000000000 ) ) ;
#2553 = CARTESIAN_POINT ( 'NONE',  ( 196.3214660117057235, 290.6082415817560332, 16.86635188982479860 ) ) ;
#2552 = AXIS2_PLACEMENT_3D ( 'NONE', #64991, #65977, #19896 ) ;
#2554 = CARTESIAN_POINT ( 'NONE',  ( 73.34023794504622629, 66.76775327374055280, 12.61468185384920559 ) ) ;
#2555 = CARTESIAN_POINT ( 'NONE',  ( 81.55798275936130892, 41.98492694272253800, 7.594723423486053449 ) ) ;
#2556 = CARTESIAN_POINT ( 'NONE',  ( 186.8161249571872133, 295.8581466444864532, -7.749471023126312197 ) ) ;
#2557 = CARTESIAN_POINT ( 'NONE',  ( 83.61138909378800577, 52.00041238365412255, 15.00249647689079247 ) ) ;
#2559 =( BOUNDED_CURVE ( )  B_SPLINE_CURVE ( 2, ( #99215, #23184, #22201, #45486, #53095, #99713, #69295 ),
 .UNSPECIFIED., .F., .T. ) 
 B_SPLINE_CURVE_WITH_KNOTS ( ( 3, 2, 2, 3 ),
 ( 0.000000000000000000, 0.005000000000000000104, 0.01000000000000000021, 0.01250000000000000243 ),
 .UNSPECIFIED. ) 
 CURVE ( )  GEOMETRIC_REPRESENTATION_ITEM ( )  RATIONAL_B_SPLINE_CURVE ( ( 1.000000000000000000, 0.9510565162951535312, 1.000000000000000000, 0.9510565162951535312, 1.000000000000000000, 0.9755282581475768211, 0.9755282581475768211 ) ) 
 REPRESENTATION_ITEM ( '' )  );
#2558 = CARTESIAN_POINT ( 'NONE',  ( 91.96515528263753936, 217.2365022471902307, 10.00000000000009592 ) ) ;
#2560 = CARTESIAN_POINT ( 'NONE',  ( 70.52080361708803480, 66.70997956558090891, -10.64257139366791449 ) ) ;
#2561 = CARTESIAN_POINT ( 'NONE',  ( 28.94742091202107304, 40.21091486745862653, 7.012934429366973338E-14 ) ) ;
#2562 = CARTESIAN_POINT ( 'NONE',  ( 42.85403768609726427, 204.7369531367911293, -4.594050593750048428 ) ) ;
#2563 = FACE_OUTER_BOUND ( 'NONE', #81678, .T. ) ;
#2564 = ORIENTED_EDGE ( 'NONE', *, *, #90628, .T. ) ;
#2565 = CARTESIAN_POINT ( 'NONE',  ( -6.349302005936061200, 83.25572239057319734, 13.46179068210798668 ) ) ;
#2566 = CARTESIAN_POINT ( 'NONE',  ( 190.9380839614473473, 299.9325328093580652, -5.232187664503159752 ) ) ;
#2567 = DIRECTION ( 'NONE',  ( 0.5000000000000048850, -0.8660254037844358210, 0.000000000000000000 ) ) ;
#2568 = ORIENTED_EDGE ( 'NONE', *, *, #28791, .F. ) ;
#2569 = CARTESIAN_POINT ( 'NONE',  ( 167.6379738498630729, 285.0209819684473018, 7.709156655479272757 ) ) ;
#2570 = CARTESIAN_POINT ( 'NONE',  ( 82.80564809338142140, 40.64392876451550762, -1.326136484204851973 ) ) ;
#2571 = CARTESIAN_POINT ( 'NONE',  ( 66.06214068257196459, 68.71579393632853794, -0.4716098740908659659 ) ) ;
#2572 = CARTESIAN_POINT ( 'NONE',  ( 85.64506726322308339, 45.94279376922860791, -9.832067947323890778 ) ) ;
#2573 = CARTESIAN_POINT ( 'NONE',  ( 22.20737081713591010, 33.79752408145593279, -5.678558825948271327 ) ) ;
#2574 = CARTESIAN_POINT ( 'NONE',  ( 162.9466247808429102, 248.4151622881552441, 11.25765811906727443 ) ) ;
#2575 = CARTESIAN_POINT ( 'NONE',  ( 196.6288634187112052, 290.0758136547079289, -16.31544900032282186 ) ) ;
#2576 = EDGE_CURVE ( 'NONE', #60705, #8540, #71704, .T. ) ;
#2577 = CARTESIAN_POINT ( 'NONE',  ( 175.2796639585627361, 257.3526018093201060, 11.64661369289347448 ) ) ;
#2578 = ORIENTED_EDGE ( 'NONE', *, *, #9324, .T. ) ;
#2579 = CARTESIAN_POINT ( 'NONE',  ( 11.83670304002995444, 9.760047579820874120, 5.678558825948272215 ) ) ;
#2580 = CARTESIAN_POINT ( 'NONE',  ( 199.1041333440138317, 265.1832257255362038, 0.2027868546939186056 ) ) ;
#2581 = CARTESIAN_POINT ( 'NONE',  ( 24.47938433582656259, 173.3932355074535963, -2.679491924311248496 ) ) ;
#2582 = FACE_OUTER_BOUND ( 'NONE', #41311, .T. ) ;
#2583 = EDGE_LOOP ( 'NONE', ( #3319, #41235, #86461, #66975 ) ) ;
#2584 = CARTESIAN_POINT ( 'NONE',  ( 72.23967728755036433, 71.11445379834010794, -6.005443314427597379 ) ) ;
#2585 = CARTESIAN_POINT ( 'NONE',  ( 85.04377965201177858, 48.84687674572034410, 12.36303725827022149 ) ) ;
#2586 = CARTESIAN_POINT ( 'NONE',  ( 177.4968317130364994, 256.2040971538554004, -7.264605064380178057 ) ) ;
#2587 = LINE ( 'NONE', #33473, #33463 ) ;
#2588 = EDGE_CURVE ( 'NONE', #83357, #20667, #32841, .T. ) ;
#2589 = ORIENTED_EDGE ( 'NONE', *, *, #37624, .F. ) ;
#2590 = EDGE_LOOP ( 'NONE', ( #64056, #58020, #66053 ) ) ;
#2591 = CARTESIAN_POINT ( 'NONE',  ( 188.2427339305948522, 273.3740536669656649, -15.69085291912274549 ) ) ;
#2592 = ORIENTED_EDGE ( 'NONE', *, *, #72741, .T. ) ;
#2593 = CARTESIAN_POINT ( 'NONE',  ( 200.6583719735737645, 283.0965001081523269, -17.35266956530146132 ) ) ;
#2594 = DIRECTION ( 'NONE',  ( 0.000000000000000000, 0.000000000000000000, 1.000000000000000000 ) ) ;
#2595 = CARTESIAN_POINT ( 'NONE',  ( 72.74059857843660382, 57.24590185972273559, -15.87550358816797136 ) ) ;
#2596 = CARTESIAN_POINT ( 'NONE',  ( 76.69221233506321767, 63.60975152925200859, 15.32791472565302016 ) ) ;
#2597 = EDGE_CURVE ( 'NONE', #31958, #82127, #99240, .T. ) ;
#2598 = CARTESIAN_POINT ( 'NONE',  ( 157.8159121039657293, 257.3018173235443555, -17.05074702406642118 ) ) ;
#2599 = CARTESIAN_POINT ( 'NONE',  ( 110.1064097226738312, 240.5024278399161233, 9.188101187500095079 ) ) ;
#2600 = CARTESIAN_POINT ( 'NONE',  ( 181.9173911336421270, 287.5464557181833243, -13.25301832635643429 ) ) ;
#2601 = AXIS2_PLACEMENT_3D ( 'NONE', #65764, #58169, #89153 ) ;
#2602 = EDGE_LOOP ( 'NONE', ( #6268, #31875, #84211, #65507 ) ) ;
#2603 = CARTESIAN_POINT ( 'NONE',  ( 161.2652686759580831, 266.8029729739616869, 16.52606187695826989 ) ) ;
#2604 = EDGE_LOOP ( 'NONE', ( #91400, #73163, #28488, #84955 ) ) ;
#2605 = CARTESIAN_POINT ( 'NONE',  ( 29.48198420892518357, 37.99752408145594273, 5.678558825948277544 ) ) ;
#2606 = CARTESIAN_POINT ( 'NONE',  ( 197.8809552785519656, 287.9071269377202498, 17.61728046362068412 ) ) ;
#2607 = CARTESIAN_POINT ( 'NONE',  ( 78.53400660641976572, 48.00963154751628537, -13.98445158027483259 ) ) ;
#2608 = CARTESIAN_POINT ( 'NONE',  ( 69.56611615166229967, 198.7202760586659736, -5.415160957724236172E-17 ) ) ;
#2609 = CARTESIAN_POINT ( 'NONE',  ( 74.10605571268695257, 68.62492193873490010, 11.45106078344676526 ) ) ;
#2610 = CARTESIAN_POINT ( 'NONE',  ( 151.4327733764141612, 268.3577379114237829, 14.90862905801242100 ) ) ;
#2611 = CARTESIAN_POINT ( 'NONE',  ( 198.4383541551818553, 286.9416837633153250, 16.97133247567711578 ) ) ;
#2612 = AXIS2_PLACEMENT_3D ( 'NONE', #76038, #24793, #3035 ) ;
#2613 = CARTESIAN_POINT ( 'NONE',  ( -105.0000000000000000, 9.999999999999998224, 59.99999999999999289 ) ) ;
#2614 = ORIENTED_EDGE ( 'NONE', *, *, #33649, .F. ) ;
#2615 = DIRECTION ( 'NONE',  ( -0.4999999999999987788, 0.8660254037844392627, 0.000000000000000000 ) ) ;
#2616 = CARTESIAN_POINT ( 'NONE',  ( 84.43521566569499726, 42.96028256297638137, -5.024410855636625151 ) ) ;
#2617 = CARTESIAN_POINT ( 'NONE',  ( 177.7333452155622524, 288.3950663957488700, 10.76829023525657725 ) ) ;
#2618 = PLANE ( 'NONE',  #18949 ) ;
#2619 = VERTEX_POINT ( 'NONE', #58345 ) ;
#2620 = CARTESIAN_POINT ( 'NONE',  ( 175.4672344667806385, 261.1926118659519602, -14.53162499237264704 ) ) ;
#2621 = CARTESIAN_POINT ( 'NONE',  ( 67.32255408704899935, 69.10951546266757362, -3.098682020105078649 ) ) ;
#2622 = CARTESIAN_POINT ( 'NONE',  ( 207.8575108622103755, 270.6272257822888037, -6.381720258959569847 ) ) ;
#2623 = CARTESIAN_POINT ( 'NONE',  ( 82.02303788424785580, 52.21633268006980444, -15.43096719693068586 ) ) ;
#2624 = CARTESIAN_POINT ( 'NONE',  ( 149.0802055316563326, 272.4325049467973940, 12.84384348890831085 ) ) ;
#2625 = CARTESIAN_POINT ( 'NONE',  ( 186.7554075434758545, 282.3000898601083577, 17.53539547572453827 ) ) ;
#2626 = DIRECTION ( 'NONE',  ( 0.8660254037844395958, 0.4999999999999985567, 0.000000000000000000 ) ) ;
#2627 = CARTESIAN_POINT ( 'NONE',  ( 168.0509104211369333, 255.6975718937168267, 13.75861284036475851 ) ) ;
#2628 = CARTESIAN_POINT ( 'NONE',  ( 86.32721218574307898, 47.55264674982593931, -11.12316258729872054 ) ) ;
#2629 = CARTESIAN_POINT ( 'NONE',  ( 113.7598676209481994, 245.6744531367911293, 4.594050593750047540 ) ) ;
#2630 = ORIENTED_EDGE ( 'NONE', *, *, #20845, .T. ) ;
#2631 = VECTOR ( 'NONE', #64054, 1000.000000000000000 ) ;
#2632 = CARTESIAN_POINT ( 'NONE',  ( 87.33262174781505394, 44.32265804349968619, -4.467604021659223434 ) ) ;
#2633 = CARTESIAN_POINT ( 'NONE',  ( 84.59927265645079331, 42.67612751815072869, 3.880141412610480955 ) ) ;
#2634 = ADVANCED_FACE ( 'NONE', ( #20367 ), #27947, .T. ) ;
#2635 = DIRECTION ( 'NONE',  ( 0.6600842437418872333, -0.7511915808658273797, 0.000000000000000000 ) ) ;
#2636 = AXIS2_PLACEMENT_3D ( 'NONE', #93637, #31293, #8506 ) ;
#2637 = CARTESIAN_POINT ( 'NONE',  ( 183.2034608524758994, 284.9060971692327939, -14.93137950553607673 ) ) ;
#2638 = CARTESIAN_POINT ( 'NONE',  ( 83.80076462262509551, 51.77978008689729705, -14.86347872566931549 ) ) ;
#2639 = ORIENTED_EDGE ( 'NONE', *, *, #24673, .F. ) ;
#2640 = CARTESIAN_POINT ( 'NONE',  ( 80.47503692277169307, 57.63887959601478883, -16.59359448248663682 ) ) ;
#2641 = CARTESIAN_POINT ( 'NONE',  ( 157.6038783220860466, 274.4889219920046344, -12.58265736104147159 ) ) ;
#2643 = CARTESIAN_POINT ( 'NONE',  ( 185.0449151060633142, 261.9026404081322994, 9.668537895844421470 ) ) ;
#2642 = CARTESIAN_POINT ( 'NONE',  ( -0.04208563418565033909, 182.3297689869269504, -2.679491924311240503 ) ) ;
#2644 = CARTESIAN_POINT ( 'NONE',  ( 206.6093111437328957, 272.7891711126852101, -9.934261249647553527 ) ) ;
#2645 = CARTESIAN_POINT ( 'NONE',  ( 145.1264855360895751, 254.5958772461660544, -9.188101187500095079 ) ) ;
#2646 = EDGE_CURVE ( 'NONE', #86838, #32226, #4151, .T. ) ;
#2647 = CARTESIAN_POINT ( 'NONE',  ( -41.79694972978692391, 146.7012482093458914, -8.867527416774462878 ) ) ;
#2648 = DIRECTION ( 'NONE',  ( 0.8660254037844379305, 0.5000000000000014433, 0.000000000000000000 ) ) ;
#2649 = CARTESIAN_POINT ( 'NONE',  ( 56.95410056540389832, 209.8149278399160949, -9.188101187500095079 ) ) ;
#2650 = CARTESIAN_POINT ( 'NONE',  ( 85.51230132848702681, 48.33290926536287913, -12.21747540207229932 ) ) ;
#2651 = CARTESIAN_POINT ( 'NONE',  ( 176.6604108716779820, 252.5228158049957017, 3.079518071111189137 ) ) ;
#2652 = SURFACE_SIDE_STYLE ('',( #48752 ) ) ;
#2653 = CARTESIAN_POINT ( 'NONE',  ( 172.0910100529608258, 260.0785035667472584, 15.53398388876759206 ) ) ;
#2654 = CARTESIAN_POINT ( 'NONE',  ( 45.57373283677818421, 114.7827874512443032, 10.00000000000000000 ) ) ;
#2655 = DIRECTION ( 'NONE',  ( -0.000000000000000000, -0.000000000000000000, -1.000000000000000000 ) ) ;
#2656 = CARTESIAN_POINT ( 'NONE',  ( 203.2187760522547819, 278.6617501559703101, -15.08675642319914978 ) ) ;
#2657 = CARTESIAN_POINT ( 'NONE',  ( 193.0813327359068126, 289.3713108709676476, 16.53843723896193652 ) ) ;
#2658 = CARTESIAN_POINT ( 'NONE',  ( 125.0004159942835571, 229.6427522451417360, 1.119607411625061291E-15 ) ) ;
#2659 = CARTESIAN_POINT ( 'NONE',  ( 78.71885683147529278, 52.51053486998128506, -15.59668387851618476 ) ) ;
#2660 = ORIENTED_EDGE ( 'NONE', *, *, #81375, .T. ) ;
#2661 = LINE ( 'NONE', #95900, #33993 ) ;
#2662 = CARTESIAN_POINT ( 'NONE',  ( -16.46870247313679059, 170.4869531367911293, 4.594050593750046652 ) ) ;
#2663 = B_SPLINE_CURVE_WITH_KNOTS ( 'NONE', 3,
 ( #70677, #40263, #24575, #77805, #47862, #15979, #38772, #61571, #94023, #77285, #54453, #23067, #32175, #100107, #24079, #16971 ),
 .UNSPECIFIED., .F., .F.,
 ( 4, 2, 2, 2, 2, 2, 2, 4 ),
 ( 0.000000000000000000, 0.0003786681000628006294, 0.0007573362001256012587, 0.001136004300188401834, 0.001514672400251202517, 0.001893340500314003418, 0.002272008600376803668, 0.003029344800502417178 ),
 .UNSPECIFIED. ) ;
#2664 = AXIS2_PLACEMENT_3D ( 'NONE', #33143, #39707, #70636 ) ;
#2665 = CARTESIAN_POINT ( 'NONE',  ( 44.28847903505648986, 202.5024278399160949, -9.188101187500093303 ) ) ;
#2666 = CARTESIAN_POINT ( 'NONE',  ( 16.38795500122288473, 25.16454794089041513, -10.00000000000000355 ) ) ;
#2667 = CARTESIAN_POINT ( 'NONE',  ( 42.80017141841058503, 185.5177522451417929, 5.000000000000051514 ) ) ;
#2668 = DIRECTION ( 'NONE',  ( 0.000000000000000000, 0.000000000000000000, 1.000000000000000000 ) ) ;
#2670 = CIRCLE ( 'NONE', #59247, 10.00000000000011369 ) ;
#2669 = LINE ( 'NONE', #94886, #41900 ) ;
#2671 = CARTESIAN_POINT ( 'NONE',  ( 190.3791419447713906, 300.9006487807255326, -5.688668718458480988 ) ) ;
#2672 = DIRECTION ( 'NONE',  ( 0.3535533905932688459, -0.6123724356957851445, -0.7071067811865581199 ) ) ;
#2674 = CARTESIAN_POINT ( 'NONE',  ( 70.44081555586392085, 198.1427522451417644, 1.119607411625061291E-15 ) ) ;
#2673 = CARTESIAN_POINT ( 'NONE',  ( 1.874387969441054569, 24.58029201028039168, 1.583844403245364241 ) ) ;
#2675 = CARTESIAN_POINT ( 'NONE',  ( 119.5854454918513170, 251.3967562850347122, -4.648177544792955347E-16 ) ) ;
#2676 = CARTESIAN_POINT ( 'NONE',  ( 183.9856954830609936, 257.7508274558034032, 1.338685087526031658 ) ) ;
#2677 = CARTESIAN_POINT ( 'NONE',  ( 4.496589500409242213, 166.7365022471902023, -10.00000000000009237 ) ) ;
#2678 = DIRECTION ( 'NONE',  ( 0.000000000000000000, 0.000000000000000000, -1.000000000000000000 ) ) ;
#2679 = VECTOR ( 'NONE', #28253, 1000.000000000000114 ) ;
#2680 = CARTESIAN_POINT ( 'NONE',  ( 161.4046941692269002, 267.9362656474927462, 17.36169958451479189 ) ) ;
#2681 = CARTESIAN_POINT ( 'NONE',  ( 35.67350403664894998, 204.7365022471903160, 2.944929066748280225E-16 ) ) ;
#2682 = CARTESIAN_POINT ( 'NONE',  ( 184.9788321220551381, 294.4173266759285070, 9.914855298944029727 ) ) ;
#2683 = CARTESIAN_POINT ( 'NONE',  ( 163.0171530587457767, 248.2930037274571191, 9.677214176418313940 ) ) ;
#2684 = CARTESIAN_POINT ( 'NONE',  ( 0.6624493194153854292, 177.3149278399160664, 9.188101187500093303 ) ) ;
#2685 = CARTESIAN_POINT ( 'NONE',  ( 40.97001837269192492, 24.44966523072497822, -2.296566073217252530E-15 ) ) ;
#2687 = DIRECTION ( 'NONE',  ( -0.000000000000000000, -0.000000000000000000, -1.000000000000000000 ) ) ;
#2686 = CARTESIAN_POINT ( 'NONE',  ( 161.5266078408477597, 251.3399204103630211, 13.01505764280997468 ) ) ;
#2688 = CARTESIAN_POINT ( 'NONE',  ( 192.7507137768506880, 296.7929658737652971, 11.30364540927242345 ) ) ;
#2689 = CARTESIAN_POINT ( 'NONE',  ( 31.10096393961467598, 36.14336893147757479, 7.433330006724141015 ) ) ;
#2690 = CARTESIAN_POINT ( 'NONE',  ( 75.87151652897667020, 224.6115022471903160, -5.000000000000047962 ) ) ;
#2691 = FACE_OUTER_BOUND ( 'NONE', #94966, .T. ) ;
#2692 = CARTESIAN_POINT ( 'NONE',  ( 154.8838596469624349, 262.3802811495310152, 18.07457254681616021 ) ) ;
#2693 = CARTESIAN_POINT ( 'NONE',  ( 40.24855657362158468, 31.43677371833804912, -10.00000000000000355 ) ) ;
#2694 = FACE_OUTER_BOUND ( 'NONE', #12221, .T. ) ;
#2695 = CARTESIAN_POINT ( 'NONE',  ( 16.39654754030849659, 10.26216523072493203, -2.296566073217252530E-15 ) ) ;
#2696 = CARTESIAN_POINT ( 'NONE',  ( 153.3042509968460934, 277.6952823349280948, -5.244408299408142682 ) ) ;
#2697 = CARTESIAN_POINT ( 'NONE',  ( 23.10163885443276754, 15.19860640527292261, 2.839279412974134775 ) ) ;
#2698 = CARTESIAN_POINT ( 'NONE',  ( 207.2051200232459962, 271.7571998617677309, 9.213853433517439129 ) ) ;
#2699 = EDGE_CURVE ( 'NONE', #82304, #55615, #96400, .T. ) ;
#2700 = CIRCLE ( 'NONE', #77076, 70.00000000000001421 ) ;
#2701 = CARTESIAN_POINT ( 'NONE',  ( 193.9204722154232741, 294.7668848255750049, 15.43855698596013859 ) ) ;
#2702 = VECTOR ( 'NONE', #64696, 1000.000000000000227 ) ;
#2703 = CARTESIAN_POINT ( 'NONE',  ( -19.62743117869748843, 92.92556620904963438, 59.99999999999999289 ) ) ;
#2704 = CARTESIAN_POINT ( 'NONE',  ( 159.8732321751776624, 253.7384344327741132, -15.51998349828054202 ) ) ;
#2705 = ADVANCED_FACE ( 'NONE', ( #82206 ), #95915, .T. ) ;
#2706 = EDGE_LOOP ( 'NONE', ( #63491, #62939, #84124, #23159 ) ) ;
#2707 = CARTESIAN_POINT ( 'NONE',  ( 152.3854270389657586, 267.1361007204005205, 15.42493684955348066 ) ) ;
#2708 = CARTESIAN_POINT ( 'NONE',  ( 164.6460902696047128, 245.4716017159096566, -3.036414139157908476 ) ) ;
#2709 = AXIS2_PLACEMENT_3D ( 'NONE', #26703, #42381, #19128 ) ;
#2710 = CARTESIAN_POINT ( 'NONE',  ( 66.25740745690036704, 68.21673160025993354, 4.121950718744524345 ) ) ;
#2711 = CARTESIAN_POINT ( 'NONE',  ( 87.85893154554855755, 45.08040635541047436, 6.601944857759015406 ) ) ;
#2712 = CARTESIAN_POINT ( 'NONE',  ( 155.5888570658010508, 261.1591898008976500, 17.34682632352454945 ) ) ;
#2713 = VERTEX_POINT ( 'NONE', #64972 ) ;
#2714 = ORIENTED_EDGE ( 'NONE', *, *, #91500, .T. ) ;
#2715 = CARTESIAN_POINT ( 'NONE',  ( 159.5339686208487535, 278.3616057620046149, -9.790299535603285364 ) ) ;
#2716 = CARTESIAN_POINT ( 'NONE',  ( 86.54431918921495992, 47.23684621844409293, 10.68448168089783756 ) ) ;
#2717 = EDGE_LOOP ( 'NONE', ( #33273, #74366, #47400, #87529 ) ) ;
#2718 = CARTESIAN_POINT ( 'NONE',  ( 77.90008039292268904, 58.37449120656814472, 16.15501551646137202 ) ) ;
#2719 = CARTESIAN_POINT ( 'NONE',  ( 47.66616421796181413, 112.2513067263565034, -10.00000000000000000 ) ) ;
#2721 = ADVANCED_FACE ( 'NONE', ( #88327 ), #26969, .F. ) ;
#2720 = ORIENTED_EDGE ( 'NONE', *, *, #89108, .F. ) ;
#2722 = CARTESIAN_POINT ( 'NONE',  ( 28.14208253200458287, 39.18080186712595037, 3.090169943749475401 ) ) ;
#2723 = CARTESIAN_POINT ( 'NONE',  ( -19.65312891409030271, 93.06504152958497400, 59.99999999999999289 ) ) ;
#2724 = CARTESIAN_POINT ( 'NONE',  ( 198.2505066714982149, 285.2670451491296149, 0.000000000000000000 ) ) ;
#2725 = EDGE_CURVE ( 'NONE', #31346, #2508, #57850, .T. ) ;
#2726 = ORIENTED_EDGE ( 'NONE', *, *, #54440, .F. ) ;
#2727 = CARTESIAN_POINT ( 'NONE',  ( 161.7587802986029999, 250.4725692828850754, 14.33336164792646450 ) ) ;
#2728 = CARTESIAN_POINT ( 'NONE',  ( 169.5281517825888500, 276.4612764335079191, -15.85450656213009601 ) ) ;
#2729 = CARTESIAN_POINT ( 'NONE',  ( 191.1489696025915919, 299.5672681643093256, 8.892130899335590755 ) ) ;
#2730 = CARTESIAN_POINT ( 'NONE',  ( 151.0597526782644309, 274.7879323711273400, -8.642014759372267818 ) ) ;
#2731 = VERTEX_POINT ( 'NONE', #90801 ) ;
#2732 = CARTESIAN_POINT ( 'NONE',  ( 173.2764727202423387, 256.9869438812573321, -11.70977877276238921 ) ) ;
#2733 = EDGE_CURVE ( 'NONE', #23710, #48945, #91778, .T. ) ;
#2734 = VERTEX_POINT ( 'NONE', #83185 ) ;
#2735 = EDGE_CURVE ( 'NONE', #18050, #9815, #68433, .T. ) ;
#2736 = VERTEX_POINT ( 'NONE', #6653 ) ;
#2737 = PLANE ( 'NONE',  #87118 ) ;
#2738 = EDGE_LOOP ( 'NONE', ( #28327, #90071, #29281, #27735 ) ) ;
#2739 = LINE ( 'NONE', #56902, #44417 ) ;
#2740 = ORIENTED_EDGE ( 'NONE', *, *, #13889, .F. ) ;
#2741 = CARTESIAN_POINT ( 'NONE',  ( 82.28003896795380001, 40.62557011406286733, -3.142018250819523129 ) ) ;
#2742 = CARTESIAN_POINT ( 'NONE',  ( 147.9036042187065618, 274.4704382010785935, 6.970551717703401984 ) ) ;
#2743 = LINE ( 'NONE', #33118, #23751 ) ;
#2744 = CARTESIAN_POINT ( 'NONE',  ( 71.79993839105814857, 70.08644720081231583, 7.366185827508974882 ) ) ;
#2745 = CARTESIAN_POINT ( 'NONE',  ( 152.6845319923753834, 266.1896283897672220, 17.20844521882669653 ) ) ;
#2746 = CARTESIAN_POINT ( 'NONE',  ( 82.54140815357128247, 53.47864718817667296, -15.73643156343348615 ) ) ;
#2747 = CARTESIAN_POINT ( 'NONE',  ( 158.6106834916122068, 255.9252328997384609, -16.08117073480969239 ) ) ;
#2748 = EDGE_LOOP ( 'NONE', ( #90725, #47523, #57705, #11938 ) ) ;
#2749 = CARTESIAN_POINT ( 'NONE',  ( 174.3506819931331506, 286.9267872025895940, 11.76311152586403885 ) ) ;
#2750 = CARTESIAN_POINT ( 'NONE',  ( 25.69310950058096310, 17.76004757982090254, 5.678558825948272215 ) ) ;
#2751 = AXIS2_PLACEMENT_3D ( 'NONE', #2921, #42371, #87571 ) ;
#2752 = CARTESIAN_POINT ( 'NONE',  ( 164.6869624841032191, 245.4008089637804346, 1.435659848726088317 ) ) ;
#2754 = CARTESIAN_POINT ( 'NONE',  ( 206.2520115784021471, 273.4080321133600933, 11.69992874350409018 ) ) ;
#2753 = FACE_OUTER_BOUND ( 'NONE', #46864, .T. ) ;
#2756 = ORIENTED_EDGE ( 'NONE', *, *, #1186, .T. ) ;
#2755 = CARTESIAN_POINT ( 'NONE',  ( 198.2114954873088948, 287.3346145022089786, 18.52864136173620935 ) ) ;
#2757 = VECTOR ( 'NONE', #76466, 1000.000000000000227 ) ;
#2758 = ORIENTED_EDGE ( 'NONE', *, *, #49682, .F. ) ;
#2759 = CARTESIAN_POINT ( 'NONE',  ( 187.5021553793853002, 277.0230319745485872, 17.44130860609008948 ) ) ;
#2760 = ADVANCED_FACE ( 'NONE', ( #38018 ), #85181, .F. ) ;
#2761 = CARTESIAN_POINT ( 'NONE',  ( 171.5618304431668548, 259.5850279847709885, -13.97585501171604427 ) ) ;
#2762 = CARTESIAN_POINT ( 'NONE',  ( 164.4568492923521887, 247.7993767033852919, 8.703614106482779889 ) ) ;
#2763 = DIRECTION ( 'NONE',  ( 0.03487823687205911238, -0.06041087834082882468, 0.9975640502598247528 ) ) ;
#2764 = VECTOR ( 'NONE', #42700, 1000.000000000000227 ) ;
#2765 = CARTESIAN_POINT ( 'NONE',  ( 161.5875797534026219, 250.7690973254556468, 12.95526170413129030 ) ) ;
#2766 = CARTESIAN_POINT ( 'NONE',  ( 191.2423980897042100, 261.1760977627640159, -0.01336292133867102681 ) ) ;
#2767 = ORIENTED_EDGE ( 'NONE', *, *, #22716, .F. ) ;
#2769 = ADVANCED_FACE ( 'NONE', ( #45136 ), #22342, .T. ) ;
#2768 = CARTESIAN_POINT ( 'NONE',  ( 153.4232513496498598, 270.1086993216917449, 15.21047082690287588 ) ) ;
#2770 = CARTESIAN_POINT ( 'NONE',  ( 178.9714194486930694, 253.6239517424200187, 1.422777586239305059 ) ) ;
#2771 = CARTESIAN_POINT ( 'NONE',  ( 207.6477529416552557, 270.9905371579805546, 7.447146952410988341 ) ) ;
#2772 = CARTESIAN_POINT ( 'NONE',  ( 17.68543470866176648, 191.0177522451419065, 5.000000000000046185 ) ) ;
#2773 = CARTESIAN_POINT ( 'NONE',  ( 92.65049840370248546, 233.4869531367911293, 4.594050593750046652 ) ) ;
#2774 = CARTESIAN_POINT ( 'NONE',  ( 82.68332475418115735, 40.58172727773597899, -1.414306879930183003 ) ) ;
#2775 = ADVANCED_FACE ( 'NONE', ( #98370 ), #38529, .T. ) ;
#2776 = DIRECTION ( 'NONE',  ( 0.000000000000000000, 0.000000000000000000, 1.000000000000000000 ) ) ;
#2777 = CARTESIAN_POINT ( 'NONE',  ( 162.8493988834005677, 248.5835624823365322, 11.81438570587263470 ) ) ;
#2778 = CARTESIAN_POINT ( 'NONE',  ( 25.45277359850996390, 179.3768266524160140, -9.188101187500091527 ) ) ;
#2779 = EDGE_CURVE ( 'NONE', #38467, #31611, #6145, .T. ) ;
#2780 = CARTESIAN_POINT ( 'NONE',  ( 46.43574122514301195, 74.10519008736565638, -10.00000000000000000 ) ) ;
#2781 = VECTOR ( 'NONE', #47717, 1000.000000000000227 ) ;
#2782 = VERTEX_POINT ( 'NONE', #14741 ) ;
#2783 = CIRCLE ( 'NONE', #38311, 17.82106496071138224 ) ;
#2785 = VERTEX_POINT ( 'NONE', #99854 ) ;
#2784 = UNCERTAINTY_MEASURE_WITH_UNIT (LENGTH_MEASURE( 1.000000000000000082E-05 ), #94636, 'distance_accuracy_value', 'NONE');
#2786 = EDGE_CURVE ( 'NONE', #42053, #90329, #81164, .T. ) ;
#2787 = CARTESIAN_POINT ( 'NONE',  ( 188.1316680866631543, 261.3724935531064375, -5.915372741867520823 ) ) ;
#2788 = EDGE_CURVE ( 'NONE', #19489, #21672, #32129, .T. ) ;
#2789 = CARTESIAN_POINT ( 'NONE',  ( 68.71788151997813543, 70.18350386356217996, 1.720494083608670843 ) ) ;
#2790 = AXIS2_PLACEMENT_3D ( 'NONE', #51162, #80630, #11206 ) ;
#2791 = DIRECTION ( 'NONE',  ( -0.000000000000000000, -0.000000000000000000, 1.000000000000000000 ) ) ;
#2792 = CARTESIAN_POINT ( 'NONE',  ( -17.26243516413818924, 24.35187462261285063, -10.00000000000000000 ) ) ;
#2793 = CARTESIAN_POINT ( 'NONE',  ( 42.66591781529977823, 183.8932355074535963, -2.679491924311248496 ) ) ;
#2794 = CARTESIAN_POINT ( 'NONE',  ( 68.80540557632873799, 64.07494415132596544, 12.03686799599169888 ) ) ;
#2795 = CARTESIAN_POINT ( 'NONE',  ( 98.22579726061456995, 237.5177522451419350, 5.000000000000046185 ) ) ;
#2796 = CARTESIAN_POINT ( 'NONE',  ( 35.38456857845647363, 200.4244531367911293, -4.594050593750046652 ) ) ;
#2797 = CARTESIAN_POINT ( 'NONE',  ( 80.83312040127708542, 224.1427522451419065, -10.00000000000009415 ) ) ;
#2798 = ORIENTED_EDGE ( 'NONE', *, *, #60201, .T. ) ;
#2799 = CARTESIAN_POINT ( 'NONE',  ( 82.66344616542426138, 44.30278114141059831, 9.141997255372078968 ) ) ;
#2800 = CARTESIAN_POINT ( 'NONE',  ( 1.032487885271483163, 164.7365022471902307, 10.00000000000009948 ) ) ;
#2801 = CARTESIAN_POINT ( 'NONE',  ( -11.38080322590321281, 173.4244531367911293, -4.594050593750046652 ) ) ;
#2802 = CARTESIAN_POINT ( 'NONE',  ( 69.10645821515414866, 64.33862435200268237, -11.96736273993547961 ) ) ;
#2803 = CARTESIAN_POINT ( 'NONE',  ( 199.1944722252943905, 285.6320488493591938, -18.17555833707144686 ) ) ;
#2804 = LINE ( 'NONE', #8380, #56443 ) ;
#2805 = CARTESIAN_POINT ( 'NONE',  ( 147.5118896528469179, 275.1489077312122049, -3.975523961781759930 ) ) ;
#2806 = CARTESIAN_POINT ( 'NONE',  ( 72.70941816336303987, 68.00343649803248525, -11.28160401705123306 ) ) ;
#2807 = CARTESIAN_POINT ( 'NONE',  ( 163.9704062730716032, 246.6419207277664327, 7.317582738093436845 ) ) ;
#2808 = CARTESIAN_POINT ( 'NONE',  ( 191.0933613939813540, 299.6635844069401173, -8.689828987424775164 ) ) ;
#2809 = CARTESIAN_POINT ( 'NONE',  ( 207.1601050488701503, 271.8351680844880889, 6.320235450527015075 ) ) ;
#2810 = VERTEX_POINT ( 'NONE', #30937 ) ;
#2811 = CARTESIAN_POINT ( 'NONE',  ( 5.723458822437210713, 164.1115022471902023, -5.000000000000041744 ) ) ;
#2812 = CARTESIAN_POINT ( 'NONE',  ( 16.11576366785047654, 170.1115022471901739, -5.000000000000041744 ) ) ;
#2813 = CARTESIAN_POINT ( 'NONE',  ( 121.1210835531159091, 249.9244531367911293, -4.594050593750046652 ) ) ;
#2814 = CARTESIAN_POINT ( 'NONE',  ( 24.72364882272980324, 19.98920272979926693, 7.433330006724137462 ) ) ;
#2815 = CARTESIAN_POINT ( 'NONE',  ( -19.65312891409030271, 93.06504152958497400, 59.99999999999999289 ) ) ;
#2816 = CARTESIAN_POINT ( 'NONE',  ( 151.2076104553919151, 269.2233279204718883, 14.08327307015630225 ) ) ;
#2818 = CARTESIAN_POINT ( 'NONE',  ( 185.9608592076092464, 288.5956984647530703, 15.36535719480430018 ) ) ;
#2817 = CARTESIAN_POINT ( 'NONE',  ( 195.8248271798537417, 291.4684452715354155, 17.35175160929494709 ) ) ;
#2819 = CARTESIAN_POINT ( 'NONE',  ( 190.7790613819595080, 300.2079679965814876, -6.533365802463900529 ) ) ;
#2820 = VERTEX_POINT ( 'NONE', #28959 ) ;
#2821 = CARTESIAN_POINT ( 'NONE',  ( 193.4292346840946379, 262.9787757345689556, -5.315308200742018485 ) ) ;
#2822 = CARTESIAN_POINT ( 'NONE',  ( 149.6230451358742926, 271.4922791719315001, -12.72565967355361671 ) ) ;
#2823 = AXIS2_PLACEMENT_3D ( 'NONE', #62040, #46345, #46865 ) ;
#2824 = CARTESIAN_POINT ( 'NONE',  ( 96.20275958967147290, 237.8967562850346837, -4.648177544792955347E-16 ) ) ;
#2825 = CARTESIAN_POINT ( 'NONE',  ( 172.9948194558320438, 289.9929851553021081, -1.758069817448381977 ) ) ;
#2826 = CARTESIAN_POINT ( 'NONE',  ( 81.59257867409928622, 55.89534513097626700, -16.02158239418033503 ) ) ;
#2827 = VERTEX_POINT ( 'NONE', #59838 ) ;
#2828 = CARTESIAN_POINT ( 'NONE',  ( 189.1399679817465938, 265.6558378727139029, 10.77106915762913353 ) ) ;
#2829 = CARTESIAN_POINT ( 'NONE',  ( 175.2876851193108223, 279.0504642908932738, 15.49633333057976259 ) ) ;
#2830 = VECTOR ( 'NONE', #51929, 1000.000000000000114 ) ;
#2831 = CARTESIAN_POINT ( 'NONE',  ( 168.7163198393688788, 271.7405862636877600, -16.69663154779234304 ) ) ;
#2832 = CARTESIAN_POINT ( 'NONE',  ( 72.12312422658187927, 72.33562412997507352, 0.9419202200955228976 ) ) ;
#2833 = B_SPLINE_SURFACE_WITH_KNOTS ( 'NONE', 3, 1, ( 
 ( #98216, #43978 ),
 ( #4004, #81059 ),
 ( #74920, #66796 ),
 ( #88668, #51084 ),
 ( #27311, #58197 ),
 ( #5502, #19724 ),
 ( #81539, #11622 ),
 ( #73417, #65304 ),
 ( #90653, #28800 ),
 ( #67289, #21211 ),
 ( #5014, #82554 ),
 ( #58679, #34890 ),
 ( #73913, #97721 ),
 ( #82046, #44481 ),
 ( #89177, #13119 ),
 ( #89651, #50589 ),
 ( #83037, #96246 ),
 ( #26807, #59165 ),
 ( #20212, #13608 ),
 ( #35396, #43486 ),
 ( #12111, #66305 ),
 ( #97238, #75412 ),
 ( #57690, #19235 ),
 ( #27806, #74430 ),
 ( #30293, #92148 ),
 ( #30798, #92627 ),
 ( #100212, #44982 ),
 ( #8005, #6504 ),
 ( #77907, #53089 ),
 ( #61677, #16086 ),
 ( #99705, #84533 ),
 ( #60170, #61181 ),
 ( #15077, #14100 ),
 ( #37381, #22701 ) ),
 .UNSPECIFIED., .T., .F., .F.,
 ( 4, 2, 2, 2, 2, 2, 2, 2, 2, 2, 2, 2, 2, 2, 2, 2, 4 ),
 ( 2, 2 ),
 ( 0.000000000000000000, 0.06250000000000000000, 0.1250000000000000000, 0.1875000000000000000, 0.2500000000000000000, 0.3125000000000000000, 0.3750000000000000000, 0.4375000000000000000, 0.5000000000000000000, 0.5625000000000000000, 0.6250000000000000000, 0.6875000000000000000, 0.7500000000000000000, 0.8125000000000000000, 0.8750000000000000000, 0.9375000000000000000, 1.000000000000000000 ),
 ( 0.000000000000000000, 1.000000000000000000 ),
 .UNSPECIFIED. ) ;
#2834 = CARTESIAN_POINT ( 'NONE',  ( 200.2436573053165034, 272.2885561403415977, 12.78478541099706156 ) ) ;
#2835 = CARTESIAN_POINT ( 'NONE',  ( 83.60735424973495356, 51.47225398191811507, -14.39433507971101278 ) ) ;
#2836 = CARTESIAN_POINT ( 'NONE',  ( 71.25277716278617390, 71.82511101822419164, -0.9037114356811193350 ) ) ;
#2837 = CARTESIAN_POINT ( 'NONE',  ( 153.1973045377566507, 265.3014802884401320, 17.70608187426261892 ) ) ;
#2838 = VECTOR ( 'NONE', #15684, 1000.000000000000114 ) ;
#2839 = CARTESIAN_POINT ( 'NONE',  ( 197.9901163037401943, 272.1418500761980681, -13.83221381771805625 ) ) ;
#2840 = CARTESIAN_POINT ( 'NONE',  ( 14.09675671201943992, 9.108019796199272378, 3.090169943749476733 ) ) ;
#2841 = CARTESIAN_POINT ( 'NONE',  ( 191.8915949969537564, 288.0041433326085780, -15.85806419801627598 ) ) ;
#2842 = EDGE_LOOP ( 'NONE', ( #16526, #90745, #61506, #34235 ) ) ;
#2843 = CARTESIAN_POINT ( 'NONE',  ( 78.20977235749720080, 61.70939135586247204, 16.12143617465002166 ) ) ;
#2844 = CARTESIAN_POINT ( 'NONE',  ( 194.2223991963907963, 294.2439319543634610, -14.97294938100067441 ) ) ;
#2845 = CARTESIAN_POINT ( 'NONE',  ( 164.4429246715887416, 246.1956853373532681, -1.592092674508304384 ) ) ;
#2847 = EDGE_CURVE ( 'NONE', #31137, #38635, #21356, .T. ) ;
#2846 = VERTEX_POINT ( 'NONE', #29446 ) ;
#2848 = CARTESIAN_POINT ( 'NONE',  ( 79.12311323331778112, 59.82187722400571062, 16.49858871944914540 ) ) ;
#2849 = CARTESIAN_POINT ( 'NONE',  ( 188.2744984008364497, 292.9879626925077218, 12.47922449114265042 ) ) ;
#2850 = CARTESIAN_POINT ( 'NONE',  ( 88.28491662655248717, 43.90562524633402575, -2.137378875048265403 ) ) ;
#2851 = CARTESIAN_POINT ( 'NONE',  ( 58.97569090598251051, 178.8759306620404175, -18.47570218321542868 ) ) ;
#2852 = VECTOR ( 'NONE', #35001, 1000.000000000000114 ) ;
#2853 = CARTESIAN_POINT ( 'NONE',  ( 189.4220206103759381, 300.3593688522817615, 3.300941728658063568 ) ) ;
#2854 = CARTESIAN_POINT ( 'NONE',  ( 25.47966334272171807, 195.5177522451419350, 5.000000000000046185 ) ) ;
#2855 = ORIENTED_EDGE ( 'NONE', *, *, #29398, .F. ) ;
#2856 = ADVANCED_FACE ( 'NONE', ( #60323 ), #21845, .T. ) ;
#2857 = VERTEX_POINT ( 'NONE', #47130 ) ;
#2858 = CARTESIAN_POINT ( 'NONE',  ( 178.0571612022058048, 260.8998630075552683, 12.21430617061977486 ) ) ;
#2859 = ADVANCED_FACE ( 'NONE', ( #54721 ), #40018, .T. ) ;
#2860 = ORIENTED_EDGE ( 'NONE', *, *, #96342, .T. ) ;
#2861 = CARTESIAN_POINT ( 'NONE',  ( 192.8902927049463472, 294.0135136195178802, 14.17129879840491391 ) ) ;
#2862 = VERTEX_POINT ( 'NONE', #23828 ) ;
#2863 = DIRECTION ( 'NONE',  ( 0.000000000000000000, 0.000000000000000000, 1.000000000000000000 ) ) ;
#2864 = CARTESIAN_POINT ( 'NONE',  ( 203.5629025532486196, 278.0657055720176913, -15.85226727704602823 ) ) ;
#2866 = VERTEX_POINT ( 'NONE', #79082 ) ;
#2865 =( BOUNDED_CURVE ( )  B_SPLINE_CURVE ( 2, ( #96602, #72278, #11485, #89034, #19583, #42337, #73267, #20068, #10973 ),
 .UNSPECIFIED., .F., .T. ) 
 B_SPLINE_CURVE_WITH_KNOTS ( ( 3, 2, 2, 2, 3 ),
 ( 0.8508064516129032473, 0.8521505376344086224, 0.8548387096774193727, 0.8575268817204301230, 0.8588709677419354982 ),
 .UNSPECIFIED. ) 
 CURVE ( )  GEOMETRIC_REPRESENTATION_ITEM ( )  RATIONAL_B_SPLINE_CURVE ( ( 0.9330127018922194093, 0.9330127018922194093, 1.000000000000000000, 0.8660254037844387076, 1.000000000000000000, 0.8660254037844387076, 1.000000000000000000, 0.9330127018922194093, 0.9330127018922194093 ) ) 
 REPRESENTATION_ITEM ( '' )  );
#2867 = CIRCLE ( 'NONE', #61096, 70.00000000000001421 ) ;
#2868 = CARTESIAN_POINT ( 'NONE',  ( 82.15643586640744900, 40.65243239225524974, 3.555191510540661071 ) ) ;
#2869 = CARTESIAN_POINT ( 'NONE',  ( 190.6501024053443132, 300.4313314961713672, 3.138638463324308514 ) ) ;
#2870 = CARTESIAN_POINT ( 'NONE',  ( 162.0312816687286386, 277.4338305391307244, -12.97134983198379210 ) ) ;
#2871 = CARTESIAN_POINT ( 'NONE',  ( 192.6789561813392595, 296.9172536750198219, -11.84591848451790952 ) ) ;
#2872 = CARTESIAN_POINT ( 'NONE',  ( 153.3506059258413643, 265.0359544954067132, -16.39100908615009899 ) ) ;
#2873 = CARTESIAN_POINT ( 'NONE',  ( 87.00377149549910882, 43.01292419151745605, -0.4974700842552756685 ) ) ;
#2874 = B_SPLINE_CURVE_WITH_KNOTS ( 'NONE', 3,
 ( #32869, #26776, #57657, #73385, #17168, #48068, #26283, #57157, #79009, #94707, #71394, #63775, #74399, #50559, #12080, #51567, #5966, #20679, #97209, #44951, #13088, #89143 ),
 .UNSPECIFIED., .F., .F.,
 ( 4, 2, 2, 2, 2, 2, 2, 2, 2, 2, 4 ),
 ( 0.0002504268395162665534, 0.0009777574624113120373, 0.001705088085306357467, 0.001796004413168241940, 0.001841462577099220715, 0.001886920741030199706, 0.001977837068892119524, 0.002068753396754039343, 0.002432418708201630145, 0.002796084019649220515, 0.003159749331096811317 ),
 .UNSPECIFIED. ) ;
#2875 = CARTESIAN_POINT ( 'NONE',  ( 183.4283023828987211, 284.5394489297055429, -16.36380929643289406 ) ) ;
#2876 = CARTESIAN_POINT ( 'NONE',  ( 134.7341806906763395, 248.5958772461660544, -9.188101187500095079 ) ) ;
#2877 = CARTESIAN_POINT ( 'NONE',  ( 75.37843707191279918, 53.50823561223473490, 16.04097401286667335 ) ) ;
#2878 = ORIENTED_EDGE ( 'NONE', *, *, #11365, .F. ) ;
#2880 = ORIENTED_EDGE ( 'NONE', *, *, #13843, .F. ) ;
#2879 = CARTESIAN_POINT ( 'NONE',  ( 31.10880476808887352, 18.36477965099641096, 1.583844403245330712 ) ) ;
#2881 = CARTESIAN_POINT ( 'NONE',  ( 176.1016924857606796, 254.5150318770701290, -8.700168781860330824 ) ) ;
#2882 = CARTESIAN_POINT ( 'NONE',  ( -29.41917662106829212, 23.74964416229700248, -10.00000000000000000 ) ) ;
#2883 = CARTESIAN_POINT ( 'NONE',  ( 105.1336465626505969, 243.0530062829863027, -4.648177544792955347E-16 ) ) ;
#2884 = CARTESIAN_POINT ( 'NONE',  ( 192.0681310285980032, 297.9752338741087101, 12.08674140724503054 ) ) ;
#2885 = CARTESIAN_POINT ( 'NONE',  ( 155.2046175752080615, 277.9469667126091394, 7.179509265143448893 ) ) ;
#2886 = PLANE ( 'NONE',  #49661 ) ;
#2887 = DIRECTION ( 'NONE',  ( 0.4999999999999998890, -0.8660254037844385966, 0.000000000000000000 ) ) ;
#2888 =( BOUNDED_CURVE ( )  B_SPLINE_CURVE ( 2, ( #3403, #2395, #11000, #80426, #57564, #71798, #41873, #33275, #34277 ),
 .UNSPECIFIED., .F., .T. ) 
 B_SPLINE_CURVE_WITH_KNOTS ( ( 3, 2, 2, 2, 3 ),
 ( 0.1169354838709677491, 0.1182795698924731242, 0.1209677419354838745, 0.1236559139784946248, 0.1250000000000000000 ),
 .UNSPECIFIED. ) 
 CURVE ( )  GEOMETRIC_REPRESENTATION_ITEM ( )  RATIONAL_B_SPLINE_CURVE ( ( 0.9330127018922192983, 0.9330127018922196314, 1.000000000000000000, 0.8660254037844387076, 1.000000000000000000, 0.8660254037844387076, 1.000000000000000000, 0.9330127018922194093, 0.9330127018922194093 ) ) 
 REPRESENTATION_ITEM ( '' )  );
#2889 = CARTESIAN_POINT ( 'NONE',  ( 171.0049078633470856, 280.9014079933706967, 14.16035466535159415 ) ) ;
#2890 = CARTESIAN_POINT ( 'NONE',  ( 76.32868100360434482, 51.65245485454531860, -16.17077658888306857 ) ) ;
#2891 = CARTESIAN_POINT ( 'NONE',  ( 177.2243378689070710, 256.1247485821839405, -7.470792856032248075 ) ) ;
#2892 = ORIENTED_EDGE ( 'NONE', *, *, #90641, .T. ) ;
#2894 = EDGE_CURVE ( 'NONE', #39791, #63243, #19419, .T. ) ;
#2893 = CARTESIAN_POINT ( 'NONE',  ( 147.8163551302855296, 274.6215580551378821, -9.286329195885331345 ) ) ;
#2895 = CARTESIAN_POINT ( 'NONE',  ( 66.22186792372609432, 68.80901709827284662, 0.1133511356784482477 ) ) ;
#2896 = EDGE_LOOP ( 'NONE', ( #21191, #88784, #5315, #91705 ) ) ;
#2897 = VECTOR ( 'NONE', #73906, 1000.000000000000000 ) ;
#2898 = PLANE ( 'NONE',  #3113 ) ;
#2899 = EDGE_CURVE ( 'NONE', #63730, #72252, #75026, .T. ) ;
#2900 = CARTESIAN_POINT ( 'NONE',  ( 204.9603142014765353, 269.2154079871559702, -2.986001317163250235 ) ) ;
#2901 = CARTESIAN_POINT ( 'NONE',  ( 152.3236346572827813, 266.8147209104637909, -16.89516215687428158 ) ) ;
#2902 = CARTESIAN_POINT ( 'NONE',  ( 196.0997760050400416, 263.6366458471133569, -2.478146138921373254 ) ) ;
#2903 = AXIS2_PLACEMENT_3D ( 'NONE', #63430, #94368, #55797 ) ;
#2904 = CARTESIAN_POINT ( 'NONE',  ( 163.2919429874875448, 247.8170536094679903, 9.876785378511263147 ) ) ;
#2906 = CARTESIAN_POINT ( 'NONE',  ( 151.4835516929774712, 274.9458191638564131, -9.335966666621812848 ) ) ;
#2905 = DIRECTION ( 'NONE',  ( -0.7299047266382377996, 0.6835488936653758563, 0.000000000000000000 ) ) ;
#2907 = CARTESIAN_POINT ( 'NONE',  ( 199.9887875258707197, 267.3737047273518783, 6.263774817124060590 ) ) ;
#2908 = ORIENTED_EDGE ( 'NONE', *, *, #44734, .F. ) ;
#2909 = CARTESIAN_POINT ( 'NONE',  ( 70.01283242295176024, 62.80173547756309915, -13.36538303052352283 ) ) ;
#2910 = ADVANCED_FACE ( 'NONE', ( #3559 ), #18753, .T. ) ;
#2911 = CARTESIAN_POINT ( 'NONE',  ( 193.5554883805989164, 276.0937916413638504, -16.57716084711649174 ) ) ;
#2912 = CARTESIAN_POINT ( 'NONE',  ( 70.18173327330886480, 66.19638441240277871, -10.95949337109657762 ) ) ;
#2913 = CARTESIAN_POINT ( 'NONE',  ( 153.3127735718713609, 265.1014820546527631, 17.57722645152040641 ) ) ;
#2914 = VECTOR ( 'NONE', #16336, 1000.000000000000227 ) ;
#2915 = CARTESIAN_POINT ( 'NONE',  ( 80.62087421845698998, 43.38634220051089585, -9.432027624119850628 ) ) ;
#2916 = CARTESIAN_POINT ( 'NONE',  ( 69.27034135246833557, 70.64205536240437766, -0.1784889401922611085 ) ) ;
#2917 = CARTESIAN_POINT ( 'NONE',  ( -5.074968980656518802, 174.0024278399161233, -9.188101187500093303 ) ) ;
#2918 = CARTESIAN_POINT ( 'NONE',  ( 98.87557663705065636, 218.7048013555409796, 4.594050593750051981 ) ) ;
#2919 = CARTESIAN_POINT ( 'NONE',  ( 192.5076277540105423, 297.2140032159341558, -13.10094381206144298 ) ) ;
#2920 = CARTESIAN_POINT ( 'NONE',  ( 24.41136278775235269, 63.57149826474137200, 59.99999999999999289 ) ) ;
#2921 = CARTESIAN_POINT ( 'NONE',  ( 46.15481705937101964, 68.45315478587873770, -10.00000000000000000 ) ) ;
#2922 = VECTOR ( 'NONE', #78983, 1000.000000000000000 ) ;
#2923 = CARTESIAN_POINT ( 'NONE',  ( 194.4175321639488629, 282.9566666730594307, 17.82086732188745870 ) ) ;
#2924 = AXIS2_PLACEMENT_3D ( 'NONE', #33899, #94213, #54654 ) ;
#2925 = CARTESIAN_POINT ( 'NONE',  ( 160.9346792447446717, 281.6669817926451174, 5.574211404230215550 ) ) ;
#2927 = CARTESIAN_POINT ( 'NONE',  ( 163.4178923001155681, 247.5989030008181260, -10.38047187240561442 ) ) ;
#2926 = CARTESIAN_POINT ( 'NONE',  ( 81.59425157384957572, 59.39892931189028502, 0.4045084971874712831 ) ) ;
#2928 = CARTESIAN_POINT ( 'NONE',  ( 207.9683050836422069, 270.4353245615839114, 5.627704969255242773 ) ) ;
#2929 = CARTESIAN_POINT ( 'NONE',  ( -69.42519150082246426, 45.64199051378594163, -10.00000000000000000 ) ) ;
#2930 = CARTESIAN_POINT ( 'NONE',  ( -19.65312891409030271, 93.06504152958497400, -10.00000000000000888 ) ) ;
#2931 = CARTESIAN_POINT ( 'NONE',  ( 76.52674025845067263, 55.63219038539143924, -16.16525125865949164 ) ) ;
#2932 = CARTESIAN_POINT ( 'NONE',  ( 143.2591182574054187, 253.5177522451418497, -10.00000000000009592 ) ) ;
#2933 = CARTESIAN_POINT ( 'NONE',  ( 183.1207986101861138, 294.8225010653632694, -8.165837621905515320 ) ) ;
#2934 = CARTESIAN_POINT ( 'NONE',  ( 73.52963229642551823, 69.81563172817719476, 9.291775542480344541 ) ) ;
#2935 = CARTESIAN_POINT ( 'NONE',  ( 55.03304057046344866, 193.3923013555409796, 4.594050593750050204 ) ) ;
#2936 = CIRCLE ( 'NONE', #87075, 60.00000000000002132 ) ;
#2937 = CARTESIAN_POINT ( 'NONE',  ( 76.67567146729665239, 63.34086528488000312, -15.41964329106466103 ) ) ;
#2938 = EDGE_CURVE ( 'NONE', #92910, #45021, #93153, .T. ) ;
#2939 = CARTESIAN_POINT ( 'NONE',  ( 68.04987750350953490, 222.3464784336661637, 1.353441290958777327E-15 ) ) ;
#2940 = CARTESIAN_POINT ( 'NONE',  ( 207.3874697692679945, 271.4413608369101780, -6.809237722377445401 ) ) ;
#2942 = DIRECTION ( 'NONE',  ( 1.000000000000000000, 0.000000000000000000, 0.000000000000000000 ) ) ;
#2941 = B_SPLINE_CURVE_WITH_KNOTS ( 'NONE', 3,
 ( #40943, #58526, #64269, #10580, #35239, #74274, #18177, #5344, #90491, #95222, #97566, #82399, #35740, #56665, #4858, #75253, #42819, #66636, #4343, #10079, #50931, #29145, #28135, #36225, #80011, #59513, #89975, #20555, #81881, #51433, #67130, #21064, #51941, #82880, #13455, #5833, #67626, #60016, #48578, #79517, #2486, #99051, #83370, #37225, #60506, #13934, #52423, #68123, #21540, #44814 ),
 .UNSPECIFIED., .F., .F.,
 ( 4, 2, 2, 2, 2, 2, 2, 2, 2, 2, 2, 2, 2, 2, 2, 2, 2, 2, 2, 2, 2, 2, 2, 2, 4 ),
 ( 0.001883115646984252940, 0.002330946116002702642, 0.002554861350511887595, 0.002778776585021072547, 0.002890734202275699934, 0.003002691819530327322, 0.003114649436784954276, 0.003226607054039581229, 0.003450522288548780493, 0.003674437523057979757, 0.004570098461094487113, 0.005465759399130996204, 0.006361420337167503561, 0.006809250806185799740, 0.007257081275204095051, 0.007369038892458601442, 0.007425017701085824713, 0.007480996509713047984, 0.007592954126967495394, 0.007704911744221941937, 0.008152742213239631830, 0.008376657447748478078, 0.008600572682257322590, 0.008824487916766168838, 0.009048403151275013351 ),
 .UNSPECIFIED. ) ;
#2943 = CARTESIAN_POINT ( 'NONE',  ( 163.2522125179119996, 258.2236914498371334, 15.93854035083980669 ) ) ;
#2945 = DIRECTION ( 'NONE',  ( -0.8660254037844387076, -0.4999999999999998890, -0.000000000000000000 ) ) ;
#2944 = DIRECTION ( 'NONE',  ( 0.000000000000000000, 0.000000000000000000, 1.000000000000000000 ) ) ;
#2946 = CARTESIAN_POINT ( 'NONE',  ( 196.8489777528309048, 268.3839510415193104, -10.94460251732624023 ) ) ;
#2947 = CARTESIAN_POINT ( 'NONE',  ( 34.12723495145388597, 35.10171378149922816, 9.188101187500008038 ) ) ;
#2948 = CARTESIAN_POINT ( 'NONE',  ( 82.78961024920913303, 51.80492193425784819, 15.12833883139485636 ) ) ;
#2949 = CARTESIAN_POINT ( 'NONE',  ( 9.827979128326980174, 29.57595373812807082, -10.00000000000000000 ) ) ;
#2950 = VERTEX_POINT ( 'NONE', #27836 ) ;
#2951 = CARTESIAN_POINT ( 'NONE',  ( 11.39049277451480080, 29.68290643055186706, 3.479690158560446702E-15 ) ) ;
#2952 = CARTESIAN_POINT ( 'NONE',  ( 80.17458025225667484, 217.0958772461660544, -9.188101187500095079 ) ) ;
#2953 = LINE ( 'NONE', #20500, #70774 ) ;
#2954 = CARTESIAN_POINT ( 'NONE',  ( 169.1905967623088145, 288.2264484338115835, -1.107241701029636038 ) ) ;
#2955 = CARTESIAN_POINT ( 'NONE',  ( 147.1125781744767949, 275.8405354997948962, -5.216646253929903665 ) ) ;
#2956 = CARTESIAN_POINT ( 'NONE',  ( 201.9589676041426003, 280.8438023959050156, 17.68527200368066943 ) ) ;
#2957 = ORIENTED_EDGE ( 'NONE', *, *, #62836, .T. ) ;
#2958 = PLANE ( 'NONE',  #16225 ) ;
#2959 = CARTESIAN_POINT ( 'NONE',  ( 193.8272087209040251, 288.0738267443611562, 16.53761133020671181 ) ) ;
#2960 = CARTESIAN_POINT ( 'NONE',  ( 72.16246046514868340, 71.47350907076796034, 5.042997787714098124 ) ) ;
#2961 = CARTESIAN_POINT ( 'NONE',  ( 136.8541387121310038, 236.4865022471901455, 1.119607411625061291E-15 ) ) ;
#2962 = CARTESIAN_POINT ( 'NONE',  ( 21.88130812447325368, 171.8932355074535678, -2.679491924311248496 ) ) ;
#2963 = CARTESIAN_POINT ( 'NONE',  ( 74.72784533871833901, 53.57696346259629649, 16.08082742858022129 ) ) ;
#2964 = ORIENTED_EDGE ( 'NONE', *, *, #34297, .T. ) ;
#2965 = AXIS2_PLACEMENT_3D ( 'NONE', #13155, #7022, #6539 ) ;
#2966 = CARTESIAN_POINT ( 'NONE',  ( 188.3087462637927842, 273.2467909115973157, 15.60395914083236946 ) ) ;
#2967 = ORIENTED_EDGE ( 'NONE', *, *, #19789, .F. ) ;
#2968 = CARTESIAN_POINT ( 'NONE',  ( 202.6560281492536717, 279.6364581158209717, 17.15553667345918853 ) ) ;
#2969 = CARTESIAN_POINT ( 'NONE',  ( 2.487887237287232711, 134.7156766241960497, 22.50000000000002132 ) ) ;
#2970 = CARTESIAN_POINT ( 'NONE',  ( 201.3715986869907510, 281.8611552031986776, -17.89433714524984964 ) ) ;
#2971 = ORIENTED_EDGE ( 'NONE', *, *, #13120, .F. ) ;
#2972 = DIRECTION ( 'NONE',  ( 0.000000000000000000, 0.000000000000000000, 1.000000000000000000 ) ) ;
#2974 = EDGE_CURVE ( 'NONE', #88081, #4549, #42478, .T. ) ;
#2973 = VERTEX_POINT ( 'NONE', #81577 ) ;
#2975 = CARTESIAN_POINT ( 'NONE',  ( 72.09527832497458633, 71.67135281093830201, 5.495264124482682533 ) ) ;
#2976 = CARTESIAN_POINT ( 'NONE',  ( 170.3932416883117753, 250.2835119183525308, 3.409375801508330639 ) ) ;
#2977 = CARTESIAN_POINT ( 'NONE',  ( 201.4520623681621316, 281.7217880192456505, -17.56577389517433119 ) ) ;
#2978 = AXIS2_PLACEMENT_3D ( 'NONE', #44180, #4720, #5205 ) ;
#2979 = ORIENTED_EDGE ( 'NONE', *, *, #57729, .F. ) ;
#2980 = CARTESIAN_POINT ( 'NONE',  ( 27.02885687802902837, 37.64646525600391413, -2.839279412974133887 ) ) ;
#2981 = CARTESIAN_POINT ( 'NONE',  ( 79.78397074742090922, 49.18318286717641286, -14.22441051831706460 ) ) ;
#2983 = ADVANCED_FACE ( 'NONE', ( #20247 ), #43009, .T. ) ;
#2982 = CARTESIAN_POINT ( 'NONE',  ( 79.11275361910446691, 46.11146926033848814, 13.27945046499837112 ) ) ;
#2984 = CARTESIAN_POINT ( 'NONE',  ( 85.83080867249778123, 210.3615022471902023, 5.000000000000051514 ) ) ;
#2985 = EDGE_CURVE ( 'NONE', #25441, #81845, #6953, .T. ) ;
#2986 = ORIENTED_EDGE ( 'NONE', *, *, #68263, .F. ) ;
#2987 = ORIENTED_EDGE ( 'NONE', *, *, #235, .T. ) ;
#2988 = CARTESIAN_POINT ( 'NONE',  ( 183.2998219562535667, 295.8549255701772154, 1.009210091351407490 ) ) ;
#2989 = VECTOR ( 'NONE', #42260, 1000.000000000000000 ) ;
#2991 = CARTESIAN_POINT ( 'NONE',  ( 194.7576540903134799, 293.3168432830895540, -14.62421624641040196 ) ) ;
#2990 = CARTESIAN_POINT ( 'NONE',  ( 68.23738887302573630, 65.53295183940775814, 10.45289023565593389 ) ) ;
#2992 = CARTESIAN_POINT ( 'NONE',  ( 85.29796244568555608, 48.43343408700369679, 12.39349753750686034 ) ) ;
#2993 = CARTESIAN_POINT ( 'NONE',  ( 194.4889937320412230, 293.7821766735966662, 14.99892588346621380 ) ) ;
#2994 = CARTESIAN_POINT ( 'NONE',  ( -15.10528209597770299, 24.46087392797018722, -10.00000000000000000 ) ) ;
#2995 = CARTESIAN_POINT ( 'NONE',  ( 157.7847820078105201, 257.3557362317297361, -18.02899742403477035 ) ) ;
#2996 = CARTESIAN_POINT ( 'NONE',  ( 164.5591015285399408, 245.6222706351205147, 4.316513966039805084 ) ) ;
#2997 = CARTESIAN_POINT ( 'NONE',  ( 169.3663320018198988, 267.2185400183821002, 16.84669842072003476 ) ) ;
#2998 = AXIS2_PLACEMENT_3D ( 'NONE', #23502, #46822, #87414 ) ;
#2999 = CARTESIAN_POINT ( 'NONE',  ( 79.22635074364777097, 59.80166750096645245, 16.50638431802919470 ) ) ;
#3000 = CARTESIAN_POINT ( 'NONE',  ( 78.60473566001486745, 222.3149278399160664, 9.188101187500093303 ) ) ;
#3001 = ORIENTED_EDGE ( 'NONE', *, *, #87099, .F. ) ;
#3002 = CARTESIAN_POINT ( 'NONE',  ( 150.4606192027571581, 271.6476180253717416, 12.81392864905067874 ) ) ;
#3003 = CARTESIAN_POINT ( 'NONE',  ( 163.1660300598458377, 276.5360652196470710, -13.90274221281887534 ) ) ;
#3004 = ORIENTED_EDGE ( 'NONE', *, *, #31411, .F. ) ;
#3005 = ORIENTED_EDGE ( 'NONE', *, *, #44476, .T. ) ;
#3006 = CARTESIAN_POINT ( 'NONE',  ( 26.52232502553263416, 56.86189125829066882, 59.99999999999999289 ) ) ;
#3007 = CARTESIAN_POINT ( 'NONE',  ( 191.0604813119340690, 299.7205343796033503, -9.270812881586136811 ) ) ;
#3008 = CARTESIAN_POINT ( 'NONE',  ( 32.64838280634442214, 30.80066082961423746, 10.00000000000000533 ) ) ;
#3009 = CARTESIAN_POINT ( 'NONE',  ( 206.2041691044954348, 273.4908977089264113, -9.455375957961031474 ) ) ;
#3010 = DIRECTION ( 'NONE',  ( 0.9532659690011952014, -0.2314883312386644132, -0.1941575258509203872 ) ) ;
#3011 = CARTESIAN_POINT ( 'NONE',  ( 85.85769841670953895, 226.5024278399160664, -9.188101187500093303 ) ) ;
#3012 = ORIENTED_EDGE ( 'NONE', *, *, #97598, .T. ) ;
#3013 = VECTOR ( 'NONE', #54314, 1000.000000000000114 ) ;
#3014 = ORIENTED_EDGE ( 'NONE', *, *, #73824, .F. ) ;
#3015 = EDGE_CURVE ( 'NONE', #38318, #39540, #95797, .T. ) ;
#3016 = CARTESIAN_POINT ( 'NONE',  ( 207.9328781051891042, 270.4966858882232259, -0.8820402142964423042 ) ) ;
#3017 = ORIENTED_EDGE ( 'NONE', *, *, #70166, .T. ) ;
#3018 = CARTESIAN_POINT ( 'NONE',  ( 75.98901751930753790, 65.25029023645535631, -14.46192986472697584 ) ) ;
#3019 = AXIS2_PLACEMENT_3D ( 'NONE', #44601, #98345, #28936 ) ;
#3020 = CARTESIAN_POINT ( 'NONE',  ( 69.59202289449447676, 69.33098532997668428, -6.332424716581326329 ) ) ;
#3021 = CARTESIAN_POINT ( 'NONE',  ( -77.58047734835668052, 56.02942318228900120, -10.00000000000000000 ) ) ;
#3022 = CARTESIAN_POINT ( 'NONE',  ( -11.32641631811692662, 174.2677522451419350, -5.000000000000047962 ) ) ;
#3023 = CARTESIAN_POINT ( 'NONE',  ( 87.53579730927835101, 44.58748639555269477, 4.920146826978176513 ) ) ;
#3024 = VERTEX_POINT ( 'NONE', #35433 ) ;
#3025 = CARTESIAN_POINT ( 'NONE',  ( 156.6938127249734976, 259.2453504591003934, 17.44495368413245728 ) ) ;
#3026 = CARTESIAN_POINT ( 'NONE',  ( 160.7333616651760622, 275.5160038079451397, 13.07907024587930245 ) ) ;
#3027 = CARTESIAN_POINT ( 'NONE',  ( 191.2827847134780654, 298.6246597018299553, 8.274781095337747416 ) ) ;
#3028 = CARTESIAN_POINT ( 'NONE',  ( 152.2788729538580696, 278.4366366002627160, 5.141355727269526277 ) ) ;
#3029 = CARTESIAN_POINT ( 'NONE',  ( 174.8134674376002522, 283.6915436203280478, 13.42846482262391028 ) ) ;
#3030 = DIRECTION ( 'NONE',  ( -0.7696402260561132636, -0.6384778167143279060, 0.000000000000000000 ) ) ;
#3031 = LINE ( 'NONE', #62788, #30792 ) ;
#3032 = CARTESIAN_POINT ( 'NONE',  ( 81.13608137687064925, 42.60696278352305200, 7.988320930663086905 ) ) ;
#3033 = ADVANCED_BREP_SHAPE_REPRESENTATION ( '', ( #9388, #68784 ), #26785 ) ;
#3034 = CARTESIAN_POINT ( 'NONE',  ( 200.7079229450794173, 283.0106753079404029, 16.90512463913211505 ) ) ;
#3035 = DIRECTION ( 'NONE',  ( 0.000000000000000000, 0.000000000000000000, -1.000000000000000000 ) ) ;
#3036 = VECTOR ( 'NONE', #61789, 1000.000000000000000 ) ;
#3037 = CARTESIAN_POINT ( 'NONE',  ( 167.6339060968662977, 249.9402736688152515, 7.007630826504156474 ) ) ;
#3038 = CARTESIAN_POINT ( 'NONE',  ( 83.13802928724584262, 52.17454805837402176, 14.80588059101579645 ) ) ;
#3039 = CARTESIAN_POINT ( 'NONE',  ( 109.0771152426536190, 245.3297689869269220, -2.679491924311252493 ) ) ;
#3040 = CARTESIAN_POINT ( 'NONE',  ( 163.1454208480229511, 248.0708373994541773, -10.54743435624756742 ) ) ;
#3042 = ADVANCED_FACE ( 'NONE', ( #73947 ), #34440, .F. ) ;
#3041 = VECTOR ( 'NONE', #9744, 1000.000000000000114 ) ;
#3043 = AXIS2_PLACEMENT_3D ( 'NONE', #28874, #43561, #89241 ) ;
#3044 = CARTESIAN_POINT ( 'NONE',  ( 206.8986117509267899, 272.2880877623646825, 6.975890063856878598 ) ) ;
#3046 = CARTESIAN_POINT ( 'NONE',  ( 181.9612031435554229, 264.0215097815707281, 13.83388833630109183 ) ) ;
#3045 = CARTESIAN_POINT ( 'NONE',  ( 180.5523533409438812, 267.1348689491979371, -15.92591746638905015 ) ) ;
#3047 = CARTESIAN_POINT ( 'NONE',  ( 199.7141866094727334, 282.2205715192249613, -16.63415621045345105 ) ) ;
#3048 = CARTESIAN_POINT ( 'NONE',  ( 28.38430345058481308, 38.16126292948897714, -6.180339887498951690 ) ) ;
#3049 = CARTESIAN_POINT ( 'NONE',  ( 34.81516168915606357, 51.10768172523390973, 10.00000000000000000 ) ) ;
#3050 = DIRECTION ( 'NONE',  ( -0.8660254037844387076, -0.4999999999999998890, -0.000000000000000000 ) ) ;
#3051 = DIRECTION ( 'NONE',  ( -0.7891516029629184192, 0.6141984594095433181, 0.000000000000000000 ) ) ;
#3052 = CARTESIAN_POINT ( 'NONE',  ( 161.0804023394942988, 273.4036736971156074, -15.32506370326049705 ) ) ;
#3053 = CARTESIAN_POINT ( 'NONE',  ( 81.88482396345729342, 43.19773723414667188, -8.246544634686086894 ) ) ;
#3054 = VECTOR ( 'NONE', #46166, 1000.000000000000114 ) ;
#3055 = CARTESIAN_POINT ( 'NONE',  ( 9.052243966459650792, 176.0333772461660828, 9.188101187500095079 ) ) ;
#3056 = CARTESIAN_POINT ( 'NONE',  ( 81.05870138697780192, 44.81917051076717939, 10.73315104669606512 ) ) ;
#3057 = ORIENTED_EDGE ( 'NONE', *, *, #68950, .F. ) ;
#3058 = B_SPLINE_CURVE_WITH_KNOTS ( 'NONE', 3,
 ( #41803, #57000, #57501, #49914, #40292, #1827, #88480, #72750, #72237, #9931, #17513, #87982, #19042, #71235, #24609, #55490, #80871, #32710, #33214, #64623, #1325, #55985, #86476, #63610, #3343, #95578, #34219, #70711, #47893, #26123, #17004, #86982, #78835, #94549, #25104, #48418, #2332, #64112, #95064, #18031, #65605, #44292, #83339, #90955 ),
 .UNSPECIFIED., .F., .F.,
 ( 4, 2, 2, 2, 2, 2, 2, 2, 2, 2, 2, 2, 2, 2, 2, 2, 2, 2, 2, 2, 2, 4 ),
 ( 0.0002033711871256132782, 0.0006869211536439505947, 0.001170471120162287857, 0.001412246103421541544, 0.001654021086680795448, 0.001774908578310349216, 0.001895796069939902984, 0.002137571053198942216, 0.002621121019716995959, 0.003104670986235049703, 0.004071770919271142444, 0.005038870852307235186, 0.005522420818825281123, 0.005764195802084304959, 0.006005970785343327928, 0.006066414531158064588, 0.006126858276972801248, 0.006247745768602325743, 0.006489520751861375600, 0.006973070718379464905, 0.007456620684897553343, 0.007940170651415641781 ),
 .UNSPECIFIED. ) ;
#3059 = PLANE ( 'NONE',  #60521 ) ;
#3060 = CARTESIAN_POINT ( 'NONE',  ( 14.27891468289787191, 30.01751292744055633, 6.180339887498949913 ) ) ;
#3061 = CARTESIAN_POINT ( 'NONE',  ( 72.09830524877247626, 72.30916584571114925, -0.9965686167420374497 ) ) ;
#3062 = CARTESIAN_POINT ( 'NONE',  ( 39.11982377592438809, 184.2048013555409796, 4.594050593750051981 ) ) ;
#3063 = VECTOR ( 'NONE', #82068, 1000.000000000000000 ) ;
#3064 = DIRECTION ( 'NONE',  ( 0.000000000000000000, 0.000000000000000000, 1.000000000000000000 ) ) ;
#3065 = CARTESIAN_POINT ( 'NONE',  ( 146.8058449195592061, 276.3718130816831149, 4.181814292810413392 ) ) ;
#3066 = CARTESIAN_POINT ( 'NONE',  ( 31.25301259707286050, 39.81751292744058901, -6.180339887498951690 ) ) ;
#3067 = CARTESIAN_POINT ( 'NONE',  ( 177.8525236415347024, 292.7868308833215565, 5.877363187741069694 ) ) ;
#3068 = CARTESIAN_POINT ( 'NONE',  ( 176.3456817854797691, 291.4259432939911107, 2.560940383191315561 ) ) ;
#3069 = CARTESIAN_POINT ( 'NONE',  ( 196.7881396906236944, 289.7999390593150224, 16.36925548999025537 ) ) ;
#3070 = CARTESIAN_POINT ( 'NONE',  ( 182.4930781751271240, 280.1738083852680461, -16.09858767428634607 ) ) ;
#3071 = CARTESIAN_POINT ( 'NONE',  ( 49.80235952159635815, 85.00000000000000000, -10.00000000000000000 ) ) ;
#3072 = B_SPLINE_SURFACE_WITH_KNOTS ( 'NONE', 3, 1, ( 
 ( #8719, #63417 ),
 ( #77638, #8223 ),
 ( #17830, #40094 ),
 ( #32523, #47209 ),
 ( #32001, #71037 ),
 ( #85785, #1123 ),
 ( #16315, #71537 ),
 ( #94356, #62393 ),
 ( #31009, #39091 ),
 ( #93350, #86777 ),
 ( #23908, #40601 ),
 ( #9743, #2130 ),
 ( #55785, #70005 ),
 ( #23400, #86275 ),
 ( #619, #33011 ),
 ( #24911, #48731 ),
 ( #63912, #78132 ),
 ( #17312, #39589 ),
 ( #56303, #94850 ),
 ( #54808, #70510 ),
 ( #62912, #93862 ),
 ( #25411, #46711 ),
 ( #41096, #61899 ),
 ( #92849, #24418 ),
 ( #54290, #55294 ),
 ( #16811, #47698 ),
 ( #42593, #3151 ),
 ( #43599, #10727 ),
 ( #34036, #58302 ),
 ( #64924, #12224 ),
 ( #19827, #50698 ),
 ( #42106, #35508 ),
 ( #58785, #95868 ),
 ( #4615, #18829 ) ),
 .UNSPECIFIED., .T., .F., .F.,
 ( 4, 2, 2, 2, 2, 2, 2, 2, 2, 2, 2, 2, 2, 2, 2, 2, 4 ),
 ( 2, 2 ),
 ( 0.000000000000000000, 0.06250000000000000000, 0.1250000000000000000, 0.1875000000000000000, 0.2500000000000000000, 0.3125000000000000000, 0.3750000000000000000, 0.4375000000000000000, 0.5000000000000000000, 0.5625000000000000000, 0.6250000000000000000, 0.6875000000000000000, 0.7500000000000000000, 0.8125000000000000000, 0.8750000000000000000, 0.9375000000000000000, 1.000000000000000000 ),
 ( 0.000000000000000000, 1.000000000000000000 ),
 .UNSPECIFIED. ) ;
#3073 = CARTESIAN_POINT ( 'NONE',  ( 167.0943254138853717, 257.9640194188826285, -15.42997351562387642 ) ) ;
#3074 = CARTESIAN_POINT ( 'NONE',  ( 83.37296956034944628, 51.74080471427829764, 14.95189368521466733 ) ) ;
#3075 = CARTESIAN_POINT ( 'NONE',  ( 91.45997379709665154, 213.6115022471902023, -5.000000000000041744 ) ) ;
#3076 = DIRECTION ( 'NONE',  ( -0.5369817302126890235, 0.8435938723211464652, 0.000000000000000000 ) ) ;
#3077 = CARTESIAN_POINT ( 'NONE',  ( 45.85867072306329817, 185.0327760586659451, 1.948934522072303157E-15 ) ) ;
#3078 = CARTESIAN_POINT ( 'NONE',  ( -22.42236680055709641, 157.8615022471902591, 0.000000000000000000 ) ) ;
#3079 = ORIENTED_EDGE ( 'NONE', *, *, #9028, .T. ) ;
#3080 = CARTESIAN_POINT ( 'NONE',  ( 163.1015652178793403, 263.5875002883286129, 17.00931977151094188 ) ) ;
#3081 = CARTESIAN_POINT ( 'NONE',  ( 147.5634954182374372, 275.0595239235922236, 4.682022975662822439 ) ) ;
#3082 = CARTESIAN_POINT ( 'NONE',  ( -68.10632939235270555, 44.28490124273479012, -10.00000000000000000 ) ) ;
#3083 = VERTEX_POINT ( 'NONE', #41528 ) ;
#3084 = CARTESIAN_POINT ( 'NONE',  ( 168.2938362192519435, 285.1573150202705165, 7.602421082290971910 ) ) ;
#3085 = CARTESIAN_POINT ( 'NONE',  ( 207.2383675728608239, 271.6996134166075763, 7.873592648726489784 ) ) ;
#3086 = CARTESIAN_POINT ( 'NONE',  ( -27.42236680055714260, 166.5217562850347406, 1.224646799147364892E-15 ) ) ;
#3087 = CARTESIAN_POINT ( 'NONE',  ( 191.0083787145144925, 298.9706005401350808, -7.573825802859819767 ) ) ;
#3088 = CARTESIAN_POINT ( 'NONE',  ( 29.87828763904599683, 19.11110640527293469, -2.839279412974138328 ) ) ;
#3089 = CARTESIAN_POINT ( 'NONE',  ( 202.3139361598622372, 280.2289788223093865, 15.93832709035092421 ) ) ;
#3090 = CARTESIAN_POINT ( 'NONE',  ( 148.9504735598738137, 272.6572073132907690, -11.88406006066344744 ) ) ;
#3091 = CARTESIAN_POINT ( 'NONE',  ( 157.0482715255472215, 258.6314098073167997, 18.43444315619183271 ) ) ;
#3092 = ORIENTED_EDGE ( 'NONE', *, *, #37488, .F. ) ;
#3093 = CARTESIAN_POINT ( 'NONE',  ( 15.46319120177094142, 20.87878583063840665, -9.188101187500006262 ) ) ;
#3094 = CARTESIAN_POINT ( 'NONE',  ( 189.0720805967732758, 299.7343203868808246, 4.955419684386629164 ) ) ;
#3095 = CARTESIAN_POINT ( 'NONE',  ( 172.9532272929666306, 253.9275976348661743, 8.329286765949929006 ) ) ;
#3096 = CARTESIAN_POINT ( 'NONE',  ( -52.33464467766007289, 32.58262665401804270, -10.00000000000000000 ) ) ;
#3097 = ORIENTED_EDGE ( 'NONE', *, *, #26150, .T. ) ;
#3099 = ADVANCED_FACE ( 'NONE', ( #51123 ), #59201, .F. ) ;
#3098 = CARTESIAN_POINT ( 'NONE',  ( -46.74660806181546491, 29.87360136034011049, 10.00000000000000000 ) ) ;
#3100 = CARTESIAN_POINT ( 'NONE',  ( 151.3560786774222322, 268.4905770267490652, 15.54402364351346932 ) ) ;
#3101 = CARTESIAN_POINT ( 'NONE',  ( -19.61423149679382050, 93.20142602126372822, 59.99999999999999289 ) ) ;
#3102 = B_SPLINE_CURVE_WITH_KNOTS ( 'NONE', 3,
 ( #7657, #76096, #75579, #23344 ),
 .UNSPECIFIED., .F., .F.,
 ( 4, 4 ),
 ( 0.001104354452915805437, 0.009031582544426527970 ),
 .UNSPECIFIED. ) ;
#3103 = CARTESIAN_POINT ( 'NONE',  ( -22.42236680055709641, 157.8615022471902591, 0.000000000000000000 ) ) ;
#3104 = EDGE_CURVE ( 'NONE', #49232, #28990, #4036, .T. ) ;
#3105 = VERTEX_POINT ( 'NONE', #27346 ) ;
#3106 = ORIENTED_EDGE ( 'NONE', *, *, #73261, .T. ) ;
#3108 = CARTESIAN_POINT ( 'NONE',  ( -20.39262980780284096, 59.83893478986780678, -10.00000000000000000 ) ) ;
#3107 = CARTESIAN_POINT ( 'NONE',  ( 207.1432938686257046, 271.8642859028066141, -6.405155839440290322 ) ) ;
#3109 = CARTESIAN_POINT ( 'NONE',  ( 149.4965729687386045, 271.7113353911534546, -11.48413836595348059 ) ) ;
#3110 = ORIENTED_EDGE ( 'NONE', *, *, #2190, .F. ) ;
#3111 = CARTESIAN_POINT ( 'NONE',  ( 152.9273493951901628, 265.7690563111299298, -17.70273273795505631 ) ) ;
#3112 = ADVANCED_FACE ( 'NONE', ( #96786 ), #58227, .F. ) ;
#3113 = AXIS2_PLACEMENT_3D ( 'NONE', #32758, #10474, #42348 ) ;
#3114 = DIRECTION ( 'NONE',  ( -1.000000000000000000, 0.000000000000000000, 0.000000000000000000 ) ) ;
#3115 = CARTESIAN_POINT ( 'NONE',  ( 72.99394114207360929, 57.42839372474189474, -15.86952975956620193 ) ) ;
#3116 = CARTESIAN_POINT ( 'NONE',  ( 78.36638819403545142, 61.52197373328140628, -15.82278474554905578 ) ) ;
#3118 = EDGE_CURVE ( 'NONE', #33408, #39284, #47180, .T. ) ;
#3117 = CARTESIAN_POINT ( 'NONE',  ( 205.2937235227012707, 275.0678357141204629, -12.80017165135291535 ) ) ;
#3119 = AXIS2_PLACEMENT_3D ( 'NONE', #10889, #11890, #12386 ) ;
#3120 = CIRCLE ( 'NONE', #62712, 9.999999999999998224 ) ;
#3121 = CARTESIAN_POINT ( 'NONE',  ( 86.17361039128121547, 213.8927522451417929, -10.00000000000009237 ) ) ;
#3122 = AXIS2_PLACEMENT_3D ( 'NONE', #17440, #94987, #27052 ) ;
#3123 = CARTESIAN_POINT ( 'NONE',  ( 164.0854748117396582, 246.4426161724408928, -5.757837433625331514 ) ) ;
#3124 = VERTEX_POINT ( 'NONE', #72471 ) ;
#3125 = CARTESIAN_POINT ( 'NONE',  ( 30.86762485498029207, 38.79752408145593989, -5.678558825948271327 ) ) ;
#3126 = CARTESIAN_POINT ( 'NONE',  ( 159.2876523829509665, 254.7526883847961017, 15.64395448151312351 ) ) ;
#3127 = CARTESIAN_POINT ( 'NONE',  ( 78.14223614238626681, 47.72510913427617396, -13.95591167936428612 ) ) ;
#3128 = CARTESIAN_POINT ( 'NONE',  ( 59.87693630317638593, 211.5024278399160949, -9.188101187500093303 ) ) ;
#3129 = CARTESIAN_POINT ( 'NONE',  ( 73.79815732168846409, 68.46225211080071915, 10.93730676814644553 ) ) ;
#3130 = CARTESIAN_POINT ( 'NONE',  ( 191.3638605175971747, 299.1950661814348678, 7.382965314423603154 ) ) ;
#3131 = CARTESIAN_POINT ( 'NONE',  ( 198.0788209437629916, 287.5644135525011507, 18.31867165462247726 ) ) ;
#3132 = CARTESIAN_POINT ( 'NONE',  ( 172.7371573690596449, 271.6299009131761864, 17.79590902495428040 ) ) ;
#3133 = EDGE_LOOP ( 'NONE', ( #72550, #571, #30596, #36949 ) ) ;
#3134 = VECTOR ( 'NONE', #87868, 1000.000000000000000 ) ;
#3135 = LINE ( 'NONE', #34019, #15681 ) ;
#3136 = CARTESIAN_POINT ( 'NONE',  ( 78.70624514232692093, 57.96118622721134983, 16.60064729657024074 ) ) ;
#3137 = VERTEX_POINT ( 'NONE', #61715 ) ;
#3138 = CARTESIAN_POINT ( 'NONE',  ( 171.7735634000264895, 259.5473476820295673, -13.86153561918547261 ) ) ;
#3139 = DIRECTION ( 'NONE',  ( 1.000000000000000000, 0.000000000000000000, -5.984665299743594308E-16 ) ) ;
#3140 = CARTESIAN_POINT ( 'NONE',  ( 161.7412967960748915, 250.5028515975580774, -14.36228887024421041 ) ) ;
#3141 = CARTESIAN_POINT ( 'NONE',  ( 206.7630081259394785, 270.7710843149401967, 2.449322393346784033 ) ) ;
#3142 = CARTESIAN_POINT ( 'NONE',  ( -62.06645187246650153, 33.74130844118091943, -10.00000000000000000 ) ) ;
#3143 = CARTESIAN_POINT ( 'NONE',  ( 42.43386700773090325, 183.7592609112380444, 2.679491924311254714 ) ) ;
#3144 = CARTESIAN_POINT ( 'NONE',  ( 152.2107918078027637, 269.9234269244417987, -14.46751604775859690 ) ) ;
#3145 = CARTESIAN_POINT ( 'NONE',  ( 164.1289849693733913, 253.9388421045659072, 14.48896490727248043 ) ) ;
#3146 = CARTESIAN_POINT ( 'NONE',  ( 164.2090401137261892, 246.2285947913476889, -5.787448100099915393 ) ) ;
#3147 = CARTESIAN_POINT ( 'NONE',  ( 119.6326891643026471, 246.0024278399160949, -9.188101187500093303 ) ) ;
#3148 = ORIENTED_EDGE ( 'NONE', *, *, #31406, .T. ) ;
#3149 = CARTESIAN_POINT ( 'NONE',  ( 84.12081806601244693, 44.16637391680080782, -7.839909042555411212 ) ) ;
#3150 = CARTESIAN_POINT ( 'NONE',  ( 83.43076169397228625, 41.65753570452999099, 2.225996872481429190 ) ) ;
#3151 = CARTESIAN_POINT ( 'NONE',  ( 155.0453531195792038, 262.1005662498678817, -18.46987289964740953 ) ) ;
#3152 = DIRECTION ( 'NONE',  ( 0.000000000000000000, 1.000000000000000000, 0.000000000000000000 ) ) ;
#3153 = CARTESIAN_POINT ( 'NONE',  ( -7.772103719870364635, 172.9865022471903160, 10.00000000000009415 ) ) ;
#3154 = DIRECTION ( 'NONE',  ( 0.9364604334398946017, -0.2023802897980881699, 0.2865031848039507056 ) ) ;
#3155 = ORIENTED_EDGE ( 'NONE', *, *, #18849, .T. ) ;
#3156 = CARTESIAN_POINT ( 'NONE',  ( 80.24454609401104221, 57.41156006636176556, -16.59009416930489422 ) ) ;
#3157 = CARTESIAN_POINT ( 'NONE',  ( 158.3970702420060945, 275.2847853859153133, -12.36479235985845904 ) ) ;
#3159 = CARTESIAN_POINT ( 'NONE',  ( 182.0448786185565950, 260.4843149835525082, 9.534127780721211920 ) ) ;
#3158 = CARTESIAN_POINT ( 'NONE',  ( 147.6970978007492761, 275.3689941975056286, 3.616184303788550825 ) ) ;
#3160 = CARTESIAN_POINT ( 'NONE',  ( 154.5391432594492755, 279.1751768281744717, -6.541910729268716196 ) ) ;
#3161 = CARTESIAN_POINT ( 'NONE',  ( 149.7817191771959244, 245.0327760586659451, 1.948934522072302763E-15 ) ) ;
#3162 = CARTESIAN_POINT ( 'NONE',  ( 18.26047324907200675, 192.8967562850347122, -4.648177544792955347E-16 ) ) ;
#3163 = CARTESIAN_POINT ( 'NONE',  ( -19.51143224695965017, 93.05905879050990848, 59.99999999999999289 ) ) ;
#3164 = CARTESIAN_POINT ( 'NONE',  ( 65.61435460324827318, 214.8149278399160664, 9.188101187500093303 ) ) ;
#3165 = ADVANCED_FACE ( 'NONE', ( #90686 ), #61218, .T. ) ;
#3166 = CARTESIAN_POINT ( 'NONE',  ( 170.6732825991835796, 250.4417675700726420, 3.839369570936610021 ) ) ;
#3167 = CARTESIAN_POINT ( 'NONE',  ( 21.02495994229494514, 13.10801979619928304, 3.090169943749476733 ) ) ;
#3168 = CARTESIAN_POINT ( 'NONE',  ( 149.6700657135140489, 271.4108371424580355, 12.58635654151485284 ) ) ;
#3169 = CARTESIAN_POINT ( 'NONE',  ( 190.3081770915147217, 296.7547009589226832, -11.12978463209281799 ) ) ;
#3170 = DIRECTION ( 'NONE',  ( -0.8660254037844361541, -0.5000000000000042188, 0.000000000000000000 ) ) ;
#3171 = CARTESIAN_POINT ( 'NONE',  ( 203.1526193585190470, 278.7763369107815379, -16.67658907091021447 ) ) ;
#3172 = CARTESIAN_POINT ( 'NONE',  ( 195.8377875905904659, 289.9203488409928013, 16.32594698151886092 ) ) ;
#3173 =( BOUNDED_CURVE ( )  B_SPLINE_CURVE ( 2, ( #35403, #88672, #19246, #67297, #97243, #96753, #58203, #20722, #43983, #50596, #35899, #90145, #51607 ),
 .UNSPECIFIED., .F., .T. ) 
 B_SPLINE_CURVE_WITH_KNOTS ( ( 3, 2, 2, 2, 2, 2, 3 ),
 ( 0.1125000000000000028, 0.1150000000000000050, 0.1199999999999999956, 0.1250000000000000000, 0.1300000000000000044, 0.1350000000000000089, 0.1375000000000000111 ),
 .UNSPECIFIED. ) 
 CURVE ( )  GEOMETRIC_REPRESENTATION_ITEM ( )  RATIONAL_B_SPLINE_CURVE ( ( 0.9755282581475768211, 0.9755282581475768211, 1.000000000000000000, 0.9510565162951535312, 1.000000000000000000, 0.9510565162951535312, 1.000000000000000000, 0.9510565162951535312, 1.000000000000000000, 0.9510565162951535312, 1.000000000000000000, 0.9755282581475768211, 0.9755282581475768211 ) ) 
 REPRESENTATION_ITEM ( '' )  );
#3174 = CARTESIAN_POINT ( 'NONE',  ( 115.4741365526546275, 244.1427522451419350, 10.00000000000009237 ) ) ;
#3175 = CARTESIAN_POINT ( 'NONE',  ( 76.43834045353088413, 53.21192047009603954, -15.94639307102674586 ) ) ;
#3176 = ORIENTED_EDGE ( 'NONE', *, *, #28774, .F. ) ;
#3177 = EDGE_CURVE ( 'NONE', #45420, #31691, #65313, .T. ) ;
#3178 = CARTESIAN_POINT ( 'NONE',  ( 196.2048238403250764, 290.8102717488927169, 17.53926796892840656 ) ) ;
#3179 = CARTESIAN_POINT ( 'NONE',  ( 190.4750160083620472, 300.7345900314585947, -1.159659205620361400 ) ) ;
#3181 = CARTESIAN_POINT ( 'NONE',  ( -0.9067010812963882671, 158.0327760586659451, 1.948934522072302763E-15 ) ) ;
#3180 = B_SPLINE_CURVE_WITH_KNOTS ( 'NONE', 3,
 ( #99700, #14095, #46466, #54064, #85019, #44475, #91130, #75917, #22695, #5992 ),
 .UNSPECIFIED., .F., .F.,
 ( 4, 2, 2, 2, 4 ),
 ( 0.000000000000000000, 0.0002622400424272788768, 0.0005244800848545577536, 0.0007867201272818366304, 0.001048960169709115507 ),
 .UNSPECIFIED. ) ;
#3182 = CARTESIAN_POINT ( 'NONE',  ( 46.18343024948246978, 185.2202760586659736, -5.415160957724236172E-17 ) ) ;
#3183 = VECTOR ( 'NONE', #74444, 1000.000000000000000 ) ;
#3184 = CARTESIAN_POINT ( 'NONE',  ( 192.7218293306584656, 264.9217214401847400, 8.853126855886975122 ) ) ;
#3185 = CARTESIAN_POINT ( 'NONE',  ( 26.76913962382671031, 17.58380873178787951, 6.180339887498953466 ) ) ;
#3186 = CYLINDRICAL_SURFACE ( 'NONE', #6046, 17.82106496071139645 ) ;
#3187 = CARTESIAN_POINT ( 'NONE',  ( 66.22544472841278207, 69.36168339246577830, 0.1681495645362227065 ) ) ;
#3188 = CARTESIAN_POINT ( 'NONE',  ( 192.5691088913182796, 292.3284985076070939, -14.35085839917381101 ) ) ;
#3189 = CARTESIAN_POINT ( 'NONE',  ( 147.5498377207569263, 275.0831797495432056, 4.097967709737811326 ) ) ;
#3190 = CARTESIAN_POINT ( 'NONE',  ( 73.89341774252514483, 54.96439960668192981, -16.13050749448415289 ) ) ;
#3192 = CARTESIAN_POINT ( 'NONE',  ( 53.62548896571598078, 211.7677522451419350, -5.000000000000047962 ) ) ;
#3191 = CARTESIAN_POINT ( 'NONE',  ( 170.9108195568088888, 258.2889562468841973, 13.94820864694325202 ) ) ;
#3193 = CARTESIAN_POINT ( 'NONE',  ( 163.0642942239685738, 256.3512231501143219, -15.96636853477880003 ) ) ;
#3194 = CARTESIAN_POINT ( 'NONE',  ( 205.2414727015710412, 275.1583367910551488, -12.71338796362297963 ) ) ;
#3195 = CARTESIAN_POINT ( 'NONE',  ( 150.3996455637841621, 270.1471677736116703, 15.13740740754872327 ) ) ;
#3196 = AXIS2_PLACEMENT_3D ( 'NONE', #73864, #72891, #65255 ) ;
#3197 = CARTESIAN_POINT ( 'NONE',  ( 48.66388509341562241, 192.2365022471902023, -10.00000000000009059 ) ) ;
#3198 = CARTESIAN_POINT ( 'NONE',  ( 185.1034421103952923, 294.2212680083668488, 9.756692795348159919 ) ) ;
#3199 = CARTESIAN_POINT ( 'NONE',  ( 163.1008115941903895, 248.1481028935802442, 11.25332017433677834 ) ) ;
#3200 = CARTESIAN_POINT ( 'NONE',  ( -0.8802452050168975139, 179.4869531367911293, 4.594050593750046652 ) ) ;
#3201 = CARTESIAN_POINT ( 'NONE',  ( 40.59535201087842182, 25.29860640527295601, -2.839279412974138328 ) ) ;
#3202 = CARTESIAN_POINT ( 'NONE',  ( 164.3036517873781008, 252.3706336020835579, 13.60069832213670082 ) ) ;
#3203 = CARTESIAN_POINT ( 'NONE',  ( 192.5712965840290849, 297.1037255674836501, 11.03742858512898906 ) ) ;
#3204 = CARTESIAN_POINT ( 'NONE',  ( 29.80674373534435162, 38.18502408145592852, 5.678558825948277544 ) ) ;
#3205 = CARTESIAN_POINT ( 'NONE',  ( 75.31289280905393468, 53.62176160565092431, -16.53289957284814093 ) ) ;
#3206 = CARTESIAN_POINT ( 'NONE',  ( 183.2977132992604368, 278.9993326301736261, 16.98963108586711712 ) ) ;
#3207 = CARTESIAN_POINT ( 'NONE',  ( 191.5520471495731840, 262.7669810543075641, 7.572277432245083872 ) ) ;
#3208 = CARTESIAN_POINT ( 'NONE',  ( 178.3071527192634562, 261.8922108035372389, -12.91157669021449195 ) ) ;
#3209 = CARTESIAN_POINT ( 'NONE',  ( 4.886862741447147940, 23.79752408145590081, -5.678558825948271327 ) ) ;
#3210 = CARTESIAN_POINT ( 'NONE',  ( 167.0271109968743417, 287.8086958075197686, 0.5416428030073258126 ) ) ;
#3211 = CARTESIAN_POINT ( 'NONE',  ( 21.36958804686389612, 14.19860640527291906, 2.839279412974134775 ) ) ;
#3212 = CIRCLE ( 'NONE', #20989, 70.00000000000001421 ) ;
#3213 = CARTESIAN_POINT ( 'NONE',  ( 67.50789586100057704, 221.3297689869269504, -2.679491924311252493 ) ) ;
#3214 = CARTESIAN_POINT ( 'NONE',  ( 153.0539157576005209, 277.5780052395393795, -5.206865708505814538 ) ) ;
#3215 = CARTESIAN_POINT ( 'NONE',  ( 156.8874040700877117, 276.4568989644782278, 10.40147400811322420 ) ) ;
#3216 = CARTESIAN_POINT ( 'NONE',  ( 159.4491226731523454, 254.4730136382542582, -15.39140229921534520 ) ) ;
#3217 = EDGE_CURVE ( 'NONE', #33352, #52344, #30328, .T. ) ;
#3218 = ORIENTED_EDGE ( 'NONE', *, *, #62509, .F. ) ;
#3219 = CARTESIAN_POINT ( 'NONE',  ( 152.7314557461996571, 266.1083540640618708, 17.39314074348802208 ) ) ;
#3220 = CARTESIAN_POINT ( 'NONE',  ( 66.10853026158757473, 68.52245927072395659, 4.666879336207867546 ) ) ;
#3221 = CARTESIAN_POINT ( 'NONE',  ( 87.62713558190685603, 45.48188874142729787, 6.789248154466972274 ) ) ;
#3222 = ORIENTED_EDGE ( 'NONE', *, *, #9052, .T. ) ;
#3223 = ORIENTED_EDGE ( 'NONE', *, *, #23057, .T. ) ;
#3224 = CARTESIAN_POINT ( 'NONE',  ( 156.0916382163451601, 277.5285333452508212, -10.52960063827285886 ) ) ;
#3225 = CARTESIAN_POINT ( 'NONE',  ( 86.35455787144825024, 47.24910468700996091, 10.80869237663237570 ) ) ;
#3226 = ORIENTED_EDGE ( 'NONE', *, *, #91621, .T. ) ;
#3227 = LINE ( 'NONE', #73120, #69319 ) ;
#3228 = CARTESIAN_POINT ( 'NONE',  ( 178.3112482654562996, 264.0450902665834860, 14.95807064277194698 ) ) ;
#3229 = EDGE_LOOP ( 'NONE', ( #70706, #95231, #49675, #30782 ) ) ;
#3231 = ADVANCED_FACE ( 'NONE', ( #44008 ), #70377, .F. ) ;
#3230 = CARTESIAN_POINT ( 'NONE',  ( 78.32967510012902324, 61.10706999557027075, -15.90745784467399382 ) ) ;
#3232 = CARTESIAN_POINT ( 'NONE',  ( 162.9821135744430478, 258.3369963296131004, -16.89381123770511195 ) ) ;
#3233 = CARTESIAN_POINT ( 'NONE',  ( 19.55501378379531019, 16.45404122711132899, -8.090169943749478065 ) ) ;
#3234 = VERTEX_POINT ( 'NONE', #63225 ) ;
#3235 = CARTESIAN_POINT ( 'NONE',  ( 174.0669043376117600, 267.5140543244703508, 16.51994157467699509 ) ) ;
#3236 = CARTESIAN_POINT ( 'NONE',  ( 168.8717317207870963, 276.2693029408995358, -16.23631712967058860 ) ) ;
#3237 = LINE ( 'NONE', #96450, #23493 ) ;
#3238 = ORIENTED_EDGE ( 'NONE', *, *, #36089, .T. ) ;
#3239 = CARTESIAN_POINT ( 'NONE',  ( 171.2643466405970401, 254.4411532906372599, -11.87753971852902701 ) ) ;
#3240 = CARTESIAN_POINT ( 'NONE',  ( 36.77241830740854311, 76.97224366495252923, 59.99999999999999289 ) ) ;
#3241 = EDGE_LOOP ( 'NONE', ( #64627, #79209, #100249, #86032 ) ) ;
#3242 = CARTESIAN_POINT ( 'NONE',  ( 160.3032094352624597, 268.8024171257220587, -16.64298077618573757 ) ) ;
#3243 = VERTEX_POINT ( 'NONE', #24231 ) ;
#3244 = CARTESIAN_POINT ( 'NONE',  ( 176.1640045926653499, 252.3529155287689321, -3.563159428949892682 ) ) ;
#3245 = ORIENTED_EDGE ( 'NONE', *, *, #52583, .T. ) ;
#3246 = CARTESIAN_POINT ( 'NONE',  ( 166.0416043136671931, 271.3796547996244612, 16.27046467588942846 ) ) ;
#3247 = CARTESIAN_POINT ( 'NONE',  ( 147.2754198212952303, 275.5584854939172601, 7.218566409973668385 ) ) ;
#3248 = CARTESIAN_POINT ( 'NONE',  ( 177.3417901484068295, 288.7674540264798111, -9.484566118077653485 ) ) ;
#3249 = CARTESIAN_POINT ( 'NONE',  ( 69.97819147249884963, 66.34545571799995400, 10.67815867109653638 ) ) ;
#3250 = LINE ( 'NONE', #26535, #30696 ) ;
#3252 = CARTESIAN_POINT ( 'NONE',  ( 11.76667899187106059, 31.90941714274742225, -10.00000000000000000 ) ) ;
#3251 = AXIS2_PLACEMENT_3D ( 'NONE', #29631, #89972, #60504 ) ;
#3253 = CARTESIAN_POINT ( 'NONE',  ( 197.1461414061409130, 289.1798618988426597, -16.76433772241966835 ) ) ;
#3254 = ORIENTED_EDGE ( 'NONE', *, *, #97395, .F. ) ;
#3255 = CARTESIAN_POINT ( 'NONE',  ( 160.3083099072513846, 277.9173855857870308, -12.60700862289685809 ) ) ;
#3256 = CARTESIAN_POINT ( 'NONE',  ( 22.95008440877049338, 15.11110640527292226, -2.839279412974138328 ) ) ;
#3257 = PLANE ( 'NONE',  #87178 ) ;
#3259 = ORIENTED_EDGE ( 'NONE', *, *, #16537, .F. ) ;
#3258 = LINE ( 'NONE', #34141, #25027 ) ;
#3260 = ORIENTED_EDGE ( 'NONE', *, *, #41666, .T. ) ;
#3261 = CARTESIAN_POINT ( 'NONE',  ( 190.3538263673709423, 300.9444966470061900, 5.721980729251035847 ) ) ;
#3262 = CARTESIAN_POINT ( 'NONE',  ( 69.40440858250356371, 62.73539878346245757, 13.77383303921267377 ) ) ;
#3263 = CARTESIAN_POINT ( 'NONE',  ( 50.12332653952445582, 98.65487733484057742, -10.00000000000000000 ) ) ;
#3264 = DIRECTION ( 'NONE',  ( -0.000000000000000000, 0.000000000000000000, -1.000000000000000000 ) ) ;
#3265 = CARTESIAN_POINT ( 'NONE',  ( 199.4166651881534449, 285.2471993486035444, -17.96931216571487511 ) ) ;
#3266 = DIRECTION ( 'NONE',  ( -1.000000000000000000, 0.000000000000000000, 0.000000000000000000 ) ) ;
#3267 = AXIS2_PLACEMENT_3D ( 'NONE', #52084, #45958, #52573 ) ;
#3268 = EDGE_LOOP ( 'NONE', ( #42673, #98072, #9177, #22911 ) ) ;
#3269 = CARTESIAN_POINT ( 'NONE',  ( 181.1374228341973662, 274.2894623748312597, -17.79777986536515755 ) ) ;
#3270 = FACE_OUTER_BOUND ( 'NONE', #41973, .T. ) ;
#3271 = CARTESIAN_POINT ( 'NONE',  ( 44.46005344233068257, 203.1427522451419350, -10.00000000000009592 ) ) ;
#3272 = CARTESIAN_POINT ( 'NONE',  ( -10.31836507581447471, 176.3967562850347406, -4.648177544792955347E-16 ) ) ;
#3273 = CARTESIAN_POINT ( 'NONE',  ( 25.04665064082954729, 185.2677522451418497, 10.00000000000009592 ) ) ;
#3274 = CARTESIAN_POINT ( 'NONE',  ( 109.7008941843561445, 224.9548013555409796, -4.594050593750042211 ) ) ;
#3275 = FACE_OUTER_BOUND ( 'NONE', #67716, .T. ) ;
#3276 = CARTESIAN_POINT ( 'NONE',  ( 171.0056477905797863, 288.0889058818636386, -7.731614188742962135 ) ) ;
#3277 = CARTESIAN_POINT ( 'NONE',  ( 162.2049812978500540, 253.7488527073383864, -15.21977816412132611 ) ) ;
#3278 = CARTESIAN_POINT ( 'NONE',  ( 14.27519936121077926, 188.2369531367911293, -4.594050593750048428 ) ) ;
#3279 = AXIS2_PLACEMENT_3D ( 'NONE', #58574, #89547, #20108 ) ;
#3280 = EDGE_CURVE ( 'NONE', #93038, #5980, #56109, .T. ) ;
#3281 = CARTESIAN_POINT ( 'NONE',  ( 168.2356071464602962, 248.8554872198452301, 6.669745218284529820 ) ) ;
#3282 = ORIENTED_EDGE ( 'NONE', *, *, #41263, .T. ) ;
#3283 = ORIENTED_EDGE ( 'NONE', *, *, #54765, .T. ) ;
#3284 = CARTESIAN_POINT ( 'NONE',  ( 187.3379511102435799, 261.0847295920454485, -5.858954167403199520 ) ) ;
#3285 = EDGE_CURVE ( 'NONE', #94911, #74392, #83065, .T. ) ;
#3286 = CARTESIAN_POINT ( 'NONE',  ( 88.30098027080434520, 44.15648434567072655, 0.4058311546344762766 ) ) ;
#3287 = CARTESIAN_POINT ( 'NONE',  ( 172.2467550100553808, 258.4300157609564508, -14.58559033337875377 ) ) ;
#3288 = DIRECTION ( 'NONE',  ( 0.8218955677251033043, 0.5696381972391160176, 0.000000000000000000 ) ) ;
#3289 = CARTESIAN_POINT ( 'NONE',  ( 207.3646600298985447, 271.4808684644054324, -5.284084612275558257 ) ) ;
#3290 = CARTESIAN_POINT ( 'NONE',  ( 68.55513178119723250, 64.39780669069259034, 11.67030924314737206 ) ) ;
#3291 = CARTESIAN_POINT ( 'NONE',  ( 108.6384560342674064, 221.9824982072974251, 3.021315404115420679E-15 ) ) ;
#3292 = CARTESIAN_POINT ( 'NONE',  ( 44.12627281972940807, 196.2833772461660828, -9.188101187500095079 ) ) ;
#3293 = CARTESIAN_POINT ( 'NONE',  ( 70.58515312316123413, 224.8927522451419350, 2.944929066748280225E-16 ) ) ;
#3294 = ORIENTED_EDGE ( 'NONE', *, *, #56721, .T. ) ;
#3295 = EDGE_CURVE ( 'NONE', #11375, #28770, #24719, .T. ) ;
#3296 = CARTESIAN_POINT ( 'NONE',  ( 82.18584245047638603, 43.47170607935511555, 8.378381801397722484 ) ) ;
#3297 = CARTESIAN_POINT ( 'NONE',  ( -2.070769811622779510, 169.6115022471902591, 10.00000000000009592 ) ) ;
#3298 = CARTESIAN_POINT ( 'NONE',  ( -8.349714312657674498, 175.1744531367911293, 4.594050593750047540 ) ) ;
#3299 = CARTESIAN_POINT ( 'NONE',  ( 68.82157586999431942, 64.23696645290118568, -11.91704851694915135 ) ) ;
#3300 = CARTESIAN_POINT ( 'NONE',  ( 198.7136873185829984, 286.4647927352960437, -18.57144721070432070 ) ) ;
#3301 = DIRECTION ( 'NONE',  ( 0.2503889871761774688, 0.9681453171404013069, 0.000000000000000000 ) ) ;
#3302 = CARTESIAN_POINT ( 'NONE',  ( 147.2089949622447875, 275.6735367246781720, -3.633014386235353221 ) ) ;
#3303 = DIRECTION ( 'NONE',  ( -1.000000000000000000, 0.000000000000000000, 0.000000000000000000 ) ) ;
#3304 = CARTESIAN_POINT ( 'NONE',  ( 163.8670932201372352, 246.8208641845333773, 5.912697114930636211 ) ) ;
#3305 = DIRECTION ( 'NONE',  ( 0.8660254037844395958, 0.4999999999999985567, 0.000000000000000000 ) ) ;
#3306 = CARTESIAN_POINT ( 'NONE',  ( 207.3062152119541679, 271.5820978585240368, 7.879821064966149535 ) ) ;
#3307 = EDGE_CURVE ( 'NONE', #70075, #55525, #71850, .T. ) ;
#3308 = ORIENTED_EDGE ( 'NONE', *, *, #19349, .F. ) ;
#3309 = CARTESIAN_POINT ( 'NONE',  ( 207.6932907333322191, 270.9116633891313199, 2.120963121341169710 ) ) ;
#3310 = CARTESIAN_POINT ( 'NONE',  ( -5.895715345004106211, 180.7365022471903444, 2.944929066748280225E-16 ) ) ;
#3311 = LINE ( 'NONE', #43763, #61127 ) ;
#3312 = CARTESIAN_POINT ( 'NONE',  ( 127.2647115830355347, 244.2833772461660544, -9.188101187500095079 ) ) ;
#3313 = CARTESIAN_POINT ( 'NONE',  ( 22.55376741186237055, 15.94754757982089544, 5.678558825948272215 ) ) ;
#3314 = CARTESIAN_POINT ( 'NONE',  ( 74.95681149046626501, 67.19672641238656752, 12.53511022654090290 ) ) ;
#3315 = VECTOR ( 'NONE', #35069, 1000.000000000000000 ) ;
#3316 = CARTESIAN_POINT ( 'NONE',  ( 151.1268740129666526, 270.4373661374733615, 13.95431671769892823 ) ) ;
#3317 = CARTESIAN_POINT ( 'NONE',  ( 157.7233946900069839, 257.4620621851055375, 16.86796251324260254 ) ) ;
#3318 = CARTESIAN_POINT ( 'NONE',  ( 22.49293824011677856, 13.39040679176982707, 1.333680081654574804E-15 ) ) ;
#3319 = ORIENTED_EDGE ( 'NONE', *, *, #5913, .F. ) ;
#3320 = CARTESIAN_POINT ( 'NONE',  ( 190.8001679306945277, 300.1714103817999444, 7.815449226872675403 ) ) ;
#3321 = CARTESIAN_POINT ( 'NONE',  ( 149.7072529793668707, 271.3464269086063041, -11.98883662638834657 ) ) ;
#3322 = CARTESIAN_POINT ( 'NONE',  ( 193.0126352936363503, 264.4189281174865869, 8.906082567666748773 ) ) ;
#3323 = CARTESIAN_POINT ( 'NONE',  ( 175.8552468537395725, 291.6480507690039872, -1.084866266826680192 ) ) ;
#3324 = CARTESIAN_POINT ( 'NONE',  ( 81.44563236102617054, 56.14986361120382696, -16.42609089136781364 ) ) ;
#3325 = EDGE_LOOP ( 'NONE', ( #87906, #41347, #44835, #33520 ) ) ;
#3326 = CARTESIAN_POINT ( 'NONE',  ( 73.41722143124820832, 65.21547532963855076, -13.68388213405907194 ) ) ;
#3327 = B_SPLINE_CURVE_WITH_KNOTS ( 'NONE', 3,
 ( #31912, #84180, #62817, #14730 ),
 .UNSPECIFIED., .F., .F.,
 ( 4, 4 ),
 ( 0.03150042049964920515, 0.04052083632573695582 ),
 .UNSPECIFIED. ) ;
#3328 = CARTESIAN_POINT ( 'NONE',  ( 175.9876842035281186, 278.7540883045039095, 15.46622700675096240 ) ) ;
#3329 = CARTESIAN_POINT ( 'NONE',  ( 168.9176169510960506, 271.9055336743668363, -16.92632823138126952 ) ) ;
#3330 = ADVANCED_FACE ( 'NONE', ( #55109 ), #48016, .T. ) ;
#3331 = CARTESIAN_POINT ( 'NONE',  ( 71.92952260767445694, 72.55458961131338924, 1.705568256100856273 ) ) ;
#3332 = CARTESIAN_POINT ( 'NONE',  ( 196.3460172103508228, 270.8952704866825343, 12.02876777916156570 ) ) ;
#3333 = CARTESIAN_POINT ( 'NONE',  ( 83.85849937899710937, 52.02177296427104380, -14.56386478986045496 ) ) ;
#3334 = CARTESIAN_POINT ( 'NONE',  ( 175.0809028706871118, 261.2525943152746208, 15.25527675994286092 ) ) ;
#3335 = VECTOR ( 'NONE', #66903, 1000.000000000000000 ) ;
#3336 = CARTESIAN_POINT ( 'NONE',  ( 153.3127735718713609, 265.1014820546527631, 17.57722645152040641 ) ) ;
#3337 = EDGE_CURVE ( 'NONE', #51615, #45796, #52840, .T. ) ;
#3338 = ORIENTED_EDGE ( 'NONE', *, *, #47099, .F. ) ;
#3339 = DIRECTION ( 'NONE',  ( 0.4999999999999992784, -0.8660254037844390407, 0.000000000000000000 ) ) ;
#3340 = CARTESIAN_POINT ( 'NONE',  ( 1.572689338377429191, 25.00034080476287457, -1.878358725466461243E-16 ) ) ;
#3341 = CARTESIAN_POINT ( 'NONE',  ( 191.8232983172789261, 287.9405117321300054, -15.86170699942114659 ) ) ;
#3342 = EDGE_LOOP ( 'NONE', ( #59544, #46564 ) ) ;
#3343 = CARTESIAN_POINT ( 'NONE',  ( 167.0385653880582311, 280.6345426807069998, 11.66514859715476859 ) ) ;
#3345 = EDGE_CURVE ( 'NONE', #1951, #44012, #85061, .T. ) ;
#3344 = CARTESIAN_POINT ( 'NONE',  ( 194.5252985417586729, 293.7192948986070178, -14.54632727629426370 ) ) ;
#3346 = CARTESIAN_POINT ( 'NONE',  ( 107.7317227740038987, 244.5530062829863311, -4.648177544792955347E-16 ) ) ;
#3347 = ORIENTED_EDGE ( 'NONE', *, *, #35077, .F. ) ;
#3349 = EDGE_CURVE ( 'NONE', #49368, #37697, #77535, .T. ) ;
#3348 = CARTESIAN_POINT ( 'NONE',  ( 79.22635074364777097, 59.80166750096645245, 16.50638431802919825 ) ) ;
#3350 = CARTESIAN_POINT ( 'NONE',  ( -33.52748748567718451, 62.86531959580030104, -10.00000000000000000 ) ) ;
#3351 = CARTESIAN_POINT ( 'NONE',  ( 77.21081030551935953, 52.27152845490210353, -15.72840955207014879 ) ) ;
#3352 = CARTESIAN_POINT ( 'NONE',  ( 198.1679321590325458, 277.6257778925182720, -16.56331389466651061 ) ) ;
#3353 = CARTESIAN_POINT ( 'NONE',  ( 81.47460321488800616, 41.92273497686812789, -7.570820128221508405 ) ) ;
#3354 = ADVANCED_FACE ( 'NONE', ( #93158, #47025, #11548, #50029 ), #89577, .T. ) ;
#3355 = ORIENTED_EDGE ( 'NONE', *, *, #29773, .F. ) ;
#3356 = ADVANCED_FACE ( 'NONE', ( #3449 ), #66230, .F. ) ;
#3357 = ORIENTED_EDGE ( 'NONE', *, *, #33134, .T. ) ;
#3358 = FACE_OUTER_BOUND ( 'NONE', #52409, .T. ) ;
#3359 = ORIENTED_EDGE ( 'NONE', *, *, #66562, .T. ) ;
#3360 = DIRECTION ( 'NONE',  ( -0.8660254037844379305, -0.5000000000000014433, -0.000000000000000000 ) ) ;
#3362 = EDGE_LOOP ( 'NONE', ( #1156, #7685, #76376, #61602 ) ) ;
#3361 = B_SPLINE_CURVE_WITH_KNOTS ( 'NONE', 3,
 ( #37476, #15679, #99312, #61282 ),
 .UNSPECIFIED., .F., .F.,
 ( 4, 4 ),
 ( 0.001425702847953698189, 0.001426788465073381296 ),
 .UNSPECIFIED. ) ;
#3363 = CARTESIAN_POINT ( 'NONE',  ( 74.25393038840245197, 55.45593832152543712, 16.12141555578006091 ) ) ;
#3364 = CARTESIAN_POINT ( 'NONE',  ( 154.8579861482817535, 262.4250953638155011, -17.69813260923097786 ) ) ;
#3365 = ORIENTED_EDGE ( 'NONE', *, *, #21554, .T. ) ;
#3366 = CARTESIAN_POINT ( 'NONE',  ( 82.30911433263591448, 41.22987874057414359, 3.253666625269970858 ) ) ;
#3367 = CARTESIAN_POINT ( 'NONE',  ( 189.9707338884078638, 301.6080322845677415, 2.301871164863099395 ) ) ;
#3368 = CARTESIAN_POINT ( 'NONE',  ( 161.9937702561999515, 277.3490201517574292, -12.90888215145142937 ) ) ;
#3369 = CARTESIAN_POINT ( 'NONE',  ( 193.1028332910263998, 296.1830769848763225, -12.04975758233223893 ) ) ;
#3370 = B_SPLINE_CURVE_WITH_KNOTS ( 'NONE', 3,
 ( #69167, #62047, #37765, #84910, #75806, #29196, #14963, #15453, #93000, #38252, #45368, #36776, #6390, #46351, #31158, #76774 ),
 .UNSPECIFIED., .F., .F.,
 ( 4, 1, 2, 2, 2, 1, 2, 2, 4 ),
 ( 0.000000000000000000, 0.1249999999999972800, 0.1874999999999960310, 0.2499999999999947820, 0.4999999999999953371, 0.6249999999999955591, 0.6874999999999958922, 0.7499999999999961142, 1.000000000000000000 ),
 .UNSPECIFIED. ) ;
#3371 = FACE_OUTER_BOUND ( 'NONE', #26021, .T. ) ;
#3372 = CARTESIAN_POINT ( 'NONE',  ( 65.36586985908989789, 182.5653022007868742, 0.000000000000000000 ) ) ;
#3373 = CARTESIAN_POINT ( 'NONE',  ( 135.2750994722765654, 261.1589784336661637, -6.496448406907675876E-16 ) ) ;
#3375 = DIRECTION ( 'NONE',  ( -0.8321961394790213795, 0.5544813661758285495, 0.000000000000000000 ) ) ;
#3374 = B_SPLINE_CURVE_WITH_KNOTS ( 'NONE', 3,
 ( #30001, #39080, #62382, #69992, #77626, #31991, #16303, #85773, #93852, #15793, #114, #61396, #30505, #38081, #92347, #38595, #99920, #22896, #8708, #39575, #47196, #91846, #15285, #7197, #61884, #607, #14313, #53781, #22408, #31490, #45198, #1113, #46181, #46699, #76138, #93339 ),
 .UNSPECIFIED., .F., .F.,
 ( 4, 2, 2, 2, 2, 2, 2, 2, 2, 2, 2, 2, 2, 2, 2, 2, 2, 4 ),
 ( 0.001074311027334474630, 0.001255084196826616264, 0.001435857366318757898, 0.001797403705303101448, 0.002520496383271696172, 0.003966681739208911643, 0.004689774417177518945, 0.005051320756161901092, 0.005232093925654099538, 0.005322480510400157128, 0.005412867095146215585, 0.005458060387519308998, 0.005503253679892403279, 0.005593640264638590105, 0.005774413434130967228, 0.006135959773115820352, 0.006497506112100673477, 0.006859052451085527469 ),
 .UNSPECIFIED. ) ;
#3376 = B_SPLINE_CURVE_WITH_KNOTS ( 'NONE', 3,
 ( #74850, #43413, #36813, #5922, #51014, #81965, #28220, #12541, #90067, #56748, #67723, #72485, #3087, #33978, #5431, #20637 ),
 .UNSPECIFIED., .F., .F.,
 ( 4, 2, 2, 2, 2, 2, 2, 4 ),
 ( 2.934965519869990483E-17, 0.0003787177898467209997, 0.0007574355796934127260, 0.001136153369540104235, 0.001514871159386795962, 0.001893588949233487688, 0.002272306739080179414, 0.003029742318773616643 ),
 .UNSPECIFIED. ) ;
#3377 = CARTESIAN_POINT ( 'NONE',  ( 36.18707552304946518, 42.93396525600392977, 2.839279412974139660 ) ) ;
#3378 = EDGE_LOOP ( 'NONE', ( #28357, #63527, #37847, #4040 ) ) ;
#3380 = VERTEX_POINT ( 'NONE', #64739 ) ;
#3379 = CARTESIAN_POINT ( 'NONE',  ( 204.0723286345250926, 271.5096690584438761, 9.850150987350732024 ) ) ;
#3381 = CARTESIAN_POINT ( 'NONE',  ( -6.542761065016642341, 25.57183462804972507, 10.00000000000000000 ) ) ;
#3382 = CARTESIAN_POINT ( 'NONE',  ( 202.3421728196210552, 280.1800714929709670, 16.85915999540957344 ) ) ;
#3383 = CARTESIAN_POINT ( 'NONE',  ( 76.27979237450192329, 64.97140225463311936, -14.28508825889822376 ) ) ;
#3384 = LINE ( 'NONE', #28020, #56298 ) ;
#3385 = CARTESIAN_POINT ( 'NONE',  ( 157.8501323257721083, 280.8042112442767007, -7.123878780571343050 ) ) ;
#3386 = CYLINDRICAL_SURFACE ( 'NONE', #48073, 10.00000000000010658 ) ;
#3387 = CARTESIAN_POINT ( 'NONE',  ( 172.0111262547279125, 280.2166085468118126, 13.88871956038429190 ) ) ;
#3388 = CARTESIAN_POINT ( 'NONE',  ( 68.91022223105564137, 64.71151235087043574, -12.22836756590942997 ) ) ;
#3389 = CARTESIAN_POINT ( 'NONE',  ( 177.2202596218039048, 256.1409925865689843, -7.582792283667149746 ) ) ;
#3390 = ORIENTED_EDGE ( 'NONE', *, *, #85117, .T. ) ;
#3391 = CARTESIAN_POINT ( 'NONE',  ( 194.6050500505458842, 285.5465367126718093, -17.70104686455487553 ) ) ;
#3392 = ORIENTED_EDGE ( 'NONE', *, *, #23167, .F. ) ;
#3393 = CARTESIAN_POINT ( 'NONE',  ( 163.8398204947978627, 278.2177931945711862, 13.52153232863776289 ) ) ;
#3394 = CARTESIAN_POINT ( 'NONE',  ( 200.9826050441883183, 267.6805681769415060, -2.536256614860724845 ) ) ;
#3395 = CARTESIAN_POINT ( 'NONE',  ( 164.0110128646736598, 246.5715880479891382, -7.582345067072046696 ) ) ;
#3396 = CARTESIAN_POINT ( 'NONE',  ( 81.27257538021680716, 44.83877995622705726, -10.61750955095084592 ) ) ;
#3397 = CARTESIAN_POINT ( 'NONE',  ( 162.6937333994314656, 248.8531830095558632, 10.02305144031113926 ) ) ;
#3399 = CARTESIAN_POINT ( 'NONE',  ( 88.26624674143728555, 44.30546972661463911, 2.125762532784985837 ) ) ;
#3398 = CARTESIAN_POINT ( 'NONE',  ( 161.1867049071889824, 281.8197337930336630, -7.641306719448324181 ) ) ;
#3400 = EDGE_CURVE ( 'NONE', #82839, #79646, #73568, .T. ) ;
#3401 = LINE ( 'NONE', #96620, #5789 ) ;
#3402 = ORIENTED_EDGE ( 'NONE', *, *, #67790, .F. ) ;
#3403 = CARTESIAN_POINT ( 'NONE',  ( 1.210598108517954463, 183.0530062829863596, 2.649461200531984646E-14 ) ) ;
#3404 = CARTESIAN_POINT ( 'NONE',  ( 80.26979669126045280, 58.08567880715743570, 16.26339599281328674 ) ) ;
#3405 = DIRECTION ( 'NONE',  ( -0.8278489937552534483, 0.5609510170580086497, 0.000000000000000000 ) ) ;
#3406 = LINE ( 'NONE', #89059, #22615 ) ;
#3407 = CIRCLE ( 'NONE', #69677, 17.82106496071138935 ) ;
#3408 = CARTESIAN_POINT ( 'NONE',  ( 80.84396924949311369, 43.27153703455048372, -9.948315819065333798 ) ) ;
#3409 = CARTESIAN_POINT ( 'NONE',  ( 34.30728256194431225, 70.01911717335251240, 59.99999999999999289 ) ) ;
#3410 = B_SPLINE_CURVE_WITH_KNOTS ( 'NONE', 3,
 ( #47051, #94193, #70346, #38436, #69351, #39925, #9057, #70861, #16649, #76469, #31347, #47544, #24747, #1470, #62230, #32351, #54630, #15636, #77965, #22760, #7049, #84108, #92206, #69844, #78471, #85611, #68843, #14661, #63252, #8560, #37930, #77471, #53638, #54127, #45537, #84593, #456, #30354, #958, #61240, #76945, #93182, #7545, #23239, #31834, #100270, #23736, #30855 ),
 .UNSPECIFIED., .F., .F.,
 ( 4, 2, 2, 2, 2, 2, 2, 2, 2, 2, 2, 2, 2, 2, 2, 2, 2, 2, 2, 2, 2, 2, 2, 4 ),
 ( 0.0003844728647056017330, 0.001402722206477688372, 0.001911846877363706674, 0.002166409212806677878, 0.002293690380528164673, 0.002420971548249651467, 0.002675533883692692710, 0.002930096219135733520, 0.003439220890021694576, 0.004457470231793539926, 0.005475719573565384843, 0.005984844244451306867, 0.006239406579894231017, 0.006493968915337156034, 0.006557609499197887722, 0.006621250083058618542, 0.006684890666919349363, 0.006748531250780081051, 0.007003093586223157856, 0.007512218257109299323, 0.007766780592552338831, 0.008021342927995377473, 0.008275905263438416981, 0.008530467598881454755 ),
 .UNSPECIFIED. ) ;
#3411 = CARTESIAN_POINT ( 'NONE',  ( 202.6560281492536717, 279.6364581158209717, 17.15553667345918853 ) ) ;
#3412 = CARTESIAN_POINT ( 'NONE',  ( 3.097972219676621730, 184.8464784336661637, 1.353441290958777525E-15 ) ) ;
#3413 = CARTESIAN_POINT ( 'NONE',  ( 111.8659576938172364, 226.2048013555410080, 4.594050593750051981 ) ) ;
#3414 = CARTESIAN_POINT ( 'NONE',  ( 203.1705638993064156, 278.7452560544191442, -15.08126533799095093 ) ) ;
#3415 = CARTESIAN_POINT ( 'NONE',  ( 162.8386403195304410, 249.0994062285972461, 10.29435687412694911 ) ) ;
#3416 = CARTESIAN_POINT ( 'NONE',  ( 179.9997804975865563, 255.3430733840098696, -2.381954882531521100 ) ) ;
#3417 = ADVANCED_FACE ( 'NONE', ( #42406 ), #90580, .F. ) ;
#3418 = DIRECTION ( 'NONE',  ( -0.8660254037844379305, -0.5000000000000014433, -0.000000000000000000 ) ) ;
#3419 = CARTESIAN_POINT ( 'NONE',  ( 197.1346277874646375, 285.2336655192412991, 17.81342416061711376 ) ) ;
#3420 = CARTESIAN_POINT ( 'NONE',  ( 160.2798150919779232, 282.6907811372386163, 5.236356400565768787 ) ) ;
#3421 = LINE ( 'NONE', #24689, #27382 ) ;
#3422 = CARTESIAN_POINT ( 'NONE',  ( 181.8525389448113287, 291.4924873961389267, 9.560256996614759473 ) ) ;
#3423 = EDGE_CURVE ( 'NONE', #72480, #83576, #21144, .T. ) ;
#3424 = CARTESIAN_POINT ( 'NONE',  ( 205.3532617248650922, 274.9647125229813582, -13.76587875506490199 ) ) ;
#3425 = CARTESIAN_POINT ( 'NONE',  ( 82.03542799465949997, 53.49766676369745255, -15.45754095158874186 ) ) ;
#3426 = CARTESIAN_POINT ( 'NONE',  ( 166.2132108024410400, 253.5770524951610412, -13.49425642745076459 ) ) ;
#3427 = EDGE_CURVE ( 'NONE', #88229, #56147, #52023, .T. ) ;
#3428 = CARTESIAN_POINT ( 'NONE',  ( 77.07149570696485341, 63.73492570656748057, -15.36167024187155228 ) ) ;
#3429 = CARTESIAN_POINT ( 'NONE',  ( 84.66726058227095564, 213.5643266524160140, 9.188101187500095079 ) ) ;
#3430 = CARTESIAN_POINT ( 'NONE',  ( 207.6357208050208101, 271.0113774299547913, -6.790259683043212036 ) ) ;
#3431 = CARTESIAN_POINT ( 'NONE',  ( 87.73298548431468191, 44.18903561216112763, 4.633618514853090176 ) ) ;
#3432 = CARTESIAN_POINT ( 'NONE',  ( -55.56624327025929944, 44.99999999999998579, 59.99999999999999289 ) ) ;
#3434 = LINE ( 'NONE', #73323, #5297 ) ;
#3433 = CARTESIAN_POINT ( 'NONE',  ( -22.42236680055709641, 157.8615022471902591, 0.000000000000000000 ) ) ;
#3435 = CARTESIAN_POINT ( 'NONE',  ( 176.7763917151297903, 270.1915396991327043, -17.04233178615594113 ) ) ;
#3436 = CARTESIAN_POINT ( 'NONE',  ( 30.58134869734400851, 35.84336893147758474, -7.433330006724137462 ) ) ;
#3437 = CARTESIAN_POINT ( 'NONE',  ( 77.56105267981614304, 49.72783448595330924, -15.46007777815280981 ) ) ;
#3438 = CARTESIAN_POINT ( 'NONE',  ( 47.28113444070024229, 72.57591296950350568, -10.00000000000000000 ) ) ;
#3439 = ORIENTED_EDGE ( 'NONE', *, *, #65985, .T. ) ;
#3440 = CARTESIAN_POINT ( 'NONE',  ( 22.90017757337614768, 16.14754757982090183, -5.678558825948276656 ) ) ;
#3441 = CARTESIAN_POINT ( 'NONE',  ( 74.81622161422296813, 207.8768266524159856, -9.188101187500093303 ) ) ;
#3442 = CARTESIAN_POINT ( 'NONE',  ( 170.5832237462292085, 288.4275712266821756, -1.073378329848412305 ) ) ;
#3443 = CARTESIAN_POINT ( 'NONE',  ( 192.8301672656986341, 296.6553483942417415, -13.40355799340913556 ) ) ;
#3444 = CARTESIAN_POINT ( 'NONE',  ( 201.9921138689924476, 280.7863913811041812, 16.46984661270056804 ) ) ;
#3445 = CARTESIAN_POINT ( 'NONE',  ( 86.61846192408904699, 47.19909516036467068, 10.60101820161781561 ) ) ;
#3446 = CARTESIAN_POINT ( 'NONE',  ( 72.04811769650321196, 71.35602353065118564, 5.168332083721268511 ) ) ;
#3448 =( BOUNDED_CURVE ( )  B_SPLINE_CURVE ( 2, ( #29303, #60165, #22189, #44978, #6499, #30287, #61174, #92142, #884 ),
 .UNSPECIFIED., .F., .T. ) 
 B_SPLINE_CURVE_WITH_KNOTS ( ( 3, 2, 2, 2, 3 ),
 ( 0.2620967741935483764, 0.2634408602150537515, 0.2661290322580645018, 0.2688172043010752521, 0.2701612903225806273 ),
 .UNSPECIFIED. ) 
 CURVE ( )  GEOMETRIC_REPRESENTATION_ITEM ( )  RATIONAL_B_SPLINE_CURVE ( ( 0.9330127018922194093, 0.9330127018922194093, 1.000000000000000000, 0.8660254037844387076, 1.000000000000000000, 0.8660254037844387076, 1.000000000000000000, 0.9330127018922194093, 0.9330127018922194093 ) ) 
 REPRESENTATION_ITEM ( '' )  );
#3447 = CARTESIAN_POINT ( 'NONE',  ( 123.8637576553643100, 248.9865022471902876, -10.00000000000009415 ) ) ;
#3449 = FACE_OUTER_BOUND ( 'NONE', #56451, .T. ) ;
#3450 = EDGE_CURVE ( 'NONE', #81863, #33648, #99027, .T. ) ;
#3451 = CARTESIAN_POINT ( 'NONE',  ( 20.95177465265983585, 30.83478043621388665, -8.090169943749479842 ) ) ;
#3452 = VERTEX_POINT ( 'NONE', #7278 ) ;
#3453 = CARTESIAN_POINT ( 'NONE',  ( 169.5334234935042730, 248.6278552856955457, -1.925906227684481609 ) ) ;
#3454 = ORIENTED_EDGE ( 'NONE', *, *, #10699, .F. ) ;
#3455 = CARTESIAN_POINT ( 'NONE',  ( 202.3894997978090373, 280.0980987621804275, 16.95659012541789323 ) ) ;
#3456 = CARTESIAN_POINT ( 'NONE',  ( 207.4268178751038079, 270.9325979257727681, -1.158184821002688158 ) ) ;
#3457 = CARTESIAN_POINT ( 'NONE',  ( -19.65312891409030271, 93.06504152958497400, -40.00000000000000000 ) ) ;
#3458 = ORIENTED_EDGE ( 'NONE', *, *, #97604, .F. ) ;
#3460 = EDGE_CURVE ( 'NONE', #15274, #25562, #39990, .T. ) ;
#3459 = FACE_OUTER_BOUND ( 'NONE', #71738, .T. ) ;
#3461 = ORIENTED_EDGE ( 'NONE', *, *, #74575, .F. ) ;
#3463 = EDGE_CURVE ( 'NONE', #86428, #91729, #26751, .T. ) ;
#3462 = CARTESIAN_POINT ( 'NONE',  ( 189.3986374548728406, 289.9821967149230204, 14.43509327751535132 ) ) ;
#3464 = CARTESIAN_POINT ( 'NONE',  ( 167.9378326867459919, 248.4084500838292797, 3.496453975134492076 ) ) ;
#3465 = CARTESIAN_POINT ( 'NONE',  ( 157.8493099884071285, 257.7921011362392392, -16.71337817344635468 ) ) ;
#3466 = CARTESIAN_POINT ( 'NONE',  ( 83.95255218473330672, 50.75189519228615609, 14.35568035062530967 ) ) ;
#3467 = ORIENTED_EDGE ( 'NONE', *, *, #38757, .T. ) ;
#3468 = ADVANCED_FACE ( 'NONE', ( #94920 ), #31530, .F. ) ;
#3469 = CARTESIAN_POINT ( 'NONE',  ( 31.76492312988469280, 26.84335787977765264, 9.188101187500006262 ) ) ;
#3470 = CARTESIAN_POINT ( 'NONE',  ( 82.71201993963725840, 48.44912912001353789, -12.92290741477395422 ) ) ;
#3471 = EDGE_CURVE ( 'NONE', #73274, #82623, #43663, .T. ) ;
#3472 = DIRECTION ( 'NONE',  ( -1.000000000000000000, 0.000000000000000000, 0.000000000000000000 ) ) ;
#3473 = DIRECTION ( 'NONE',  ( 0.7226656227773233798, 0.6911977992267216431, 0.000000000000000000 ) ) ;
#3474 = VERTEX_POINT ( 'NONE', #51785 ) ;
#3475 = VECTOR ( 'NONE', #70481, 1000.000000000000114 ) ;
#3476 = VERTEX_POINT ( 'NONE', #26989 ) ;
#3477 = CARTESIAN_POINT ( 'NONE',  ( 186.2976226307126524, 298.7307822690146395, 1.075632280427271992 ) ) ;
#3479 = CARTESIAN_POINT ( 'NONE',  ( 194.4666154385731431, 293.8209370148700827, -14.56896502715340702 ) ) ;
#3478 = CARTESIAN_POINT ( 'NONE',  ( 204.3574891606595827, 276.6894411969685166, 13.41627538812899978 ) ) ;
#3480 = CARTESIAN_POINT ( 'NONE',  ( 85.35443477132466228, 48.30880629543902671, -11.80360700664790663 ) ) ;
#3481 = FACE_OUTER_BOUND ( 'NONE', #69465, .T. ) ;
#3482 = DIRECTION ( 'NONE',  ( 0.000000000000000000, 0.000000000000000000, 1.000000000000000000 ) ) ;
#3483 = CARTESIAN_POINT ( 'NONE',  ( 187.6361772789746567, 291.3791347085116854, -13.85621784405196166 ) ) ;
#3484 = CARTESIAN_POINT ( 'NONE',  ( 208.1115139972721977, 270.1872794470800159, -4.030174891007424876 ) ) ;
#3485 = CARTESIAN_POINT ( 'NONE',  ( 165.9640472274821263, 265.7646867401422242, 16.70851906738806392 ) ) ;
#3486 = CARTESIAN_POINT ( 'NONE',  ( 169.5007657120409874, 248.2156828994837099, -1.963647642838588503 ) ) ;
#3487 = CARTESIAN_POINT ( 'NONE',  ( 109.7008941843561445, 224.9548013555409796, -4.594050593750042211 ) ) ;
#3488 = VERTEX_POINT ( 'NONE', #73591 ) ;
#3489 = CARTESIAN_POINT ( 'NONE',  ( 150.6655900823359389, 269.6865383554857090, 15.31288044136207205 ) ) ;
#3490 = CARTESIAN_POINT ( 'NONE',  ( -14.15357965443277877, 60.28889183820906794, -10.00000000000000000 ) ) ;
#3491 = CARTESIAN_POINT ( 'NONE',  ( 166.7548757565938047, 278.1757261261363396, -13.35741561976894154 ) ) ;
#3492 = VERTEX_POINT ( 'NONE', #96423 ) ;
#3493 = ORIENTED_EDGE ( 'NONE', *, *, #23976, .F. ) ;
#3494 = CARTESIAN_POINT ( 'NONE',  ( 87.20555836939593064, 45.98127448902955905, -8.722945138008007859 ) ) ;
#3495 = CARTESIAN_POINT ( 'NONE',  ( 32.28746131679088904, 82.40185739040765611, 59.99999999999999289 ) ) ;
#3496 = CARTESIAN_POINT ( 'NONE',  ( -19.65312891409030271, 93.06504152958497400, 177.5919119679930134 ) ) ;
#3497 = CARTESIAN_POINT ( 'NONE',  ( 160.0081047537594543, 253.5048282741223602, -16.11956848123596941 ) ) ;
#3498 = CARTESIAN_POINT ( 'NONE',  ( 163.1306191313178431, 248.0964747248268338, 10.50682697533535048 ) ) ;
#3499 = CARTESIAN_POINT ( 'NONE',  ( 87.77910550741502504, 230.6744531367911293, 4.594050593750047540 ) ) ;
#3500 = ORIENTED_EDGE ( 'NONE', *, *, #30809, .T. ) ;
#3501 = ORIENTED_EDGE ( 'NONE', *, *, #1428, .T. ) ;
#3502 = LINE ( 'NONE', #88144, #52781 ) ;
#3503 = DIRECTION ( 'NONE',  ( -0.2194785493951510180, 0.9756173257765569096, 0.000000000000000000 ) ) ;
#3504 = ORIENTED_EDGE ( 'NONE', *, *, #53633, .F. ) ;
#3505 = EDGE_CURVE ( 'NONE', #66517, #65850, #29436, .T. ) ;
#3506 = CARTESIAN_POINT ( 'NONE',  ( 29.94731862920856358, 22.45404122711134676, -8.090169943749478065 ) ) ;
#3507 = CARTESIAN_POINT ( 'NONE',  ( 153.4475728592434791, 265.3059609131843217, 16.25445176718542584 ) ) ;
#3508 = CARTESIAN_POINT ( 'NONE',  ( 70.90832346156993538, 69.40020835857261261, -7.639751975664101025 ) ) ;
#3510 = CARTESIAN_POINT ( 'NONE',  ( 69.68654088143662761, 62.27729828303051107, -13.56154521557472314 ) ) ;
#3509 = CARTESIAN_POINT ( 'NONE',  ( 142.3662031094091844, 246.8768266524159856, -9.188101187500091527 ) ) ;
#3511 = CARTESIAN_POINT ( 'NONE',  ( -14.42967401501114999, 169.1427522451419065, 10.00000000000009237 ) ) ;
#3512 = DIRECTION ( 'NONE',  ( -0.4556638457577291690, 0.000000000000000000, -0.8901519306664882336 ) ) ;
#3513 = VERTEX_POINT ( 'NONE', #27496 ) ;
#3514 = CARTESIAN_POINT ( 'NONE',  ( 204.6244483240926400, 276.2270543623566255, 13.10813453876796864 ) ) ;
#3515 = CARTESIAN_POINT ( 'NONE',  ( 159.6438702623246968, 275.1686529806921158, 12.86435351470504962 ) ) ;
#3516 = CARTESIAN_POINT ( 'NONE',  ( 81.96170391062356941, 40.98971803353019538, -3.100310559334822802 ) ) ;
#3517 = CARTESIAN_POINT ( 'NONE',  ( 192.3297092044942076, 271.8923391751263239, 14.13782850498305699 ) ) ;
#3518 = CARTESIAN_POINT ( 'NONE',  ( 178.0095323540602124, 285.1773387558561694, 13.03190070314914628 ) ) ;
#3519 = CARTESIAN_POINT ( 'NONE',  ( 83.13520543127567919, 52.15262426605146118, 14.79738518802719049 ) ) ;
#3520 = CARTESIAN_POINT ( 'NONE',  ( -22.42236680055709641, 157.8615022471902591, 0.000000000000000000 ) ) ;
#3521 = CARTESIAN_POINT ( 'NONE',  ( 93.96857342517719758, 20.00000000000000000, 0.000000000000000000 ) ) ;
#3522 = CARTESIAN_POINT ( 'NONE',  ( 200.6129772034685175, 283.1751261563724142, 18.36811917402039640 ) ) ;
#3523 = B_SPLINE_CURVE_WITH_KNOTS ( 'NONE', 3,
 ( #35166, #36156, #37643, #90423 ),
 .UNSPECIFIED., .F., .F.,
 ( 4, 4 ),
 ( 0.005280122280043920285, 0.01026413765061139072 ),
 .UNSPECIFIED. ) ;
#3524 = CARTESIAN_POINT ( 'NONE',  ( 200.2093391412865060, 269.7417714514684803, 10.46510648850140157 ) ) ;
#3525 = CARTESIAN_POINT ( 'NONE',  ( 159.9997000813754084, 253.5193855937126841, -16.28798248637880519 ) ) ;
#3526 = CARTESIAN_POINT ( 'NONE',  ( 83.50487366122874278, 51.96486753097844513, 15.01313857892666803 ) ) ;
#3527 = CARTESIAN_POINT ( 'NONE',  ( 174.8675334118165665, 290.2565163415771394, -6.409605830264317738 ) ) ;
#3528 = CARTESIAN_POINT ( 'NONE',  ( 7.411877368840288582, 73.77757239660104460, -10.00000000000000000 ) ) ;
#3529 = ADVANCED_FACE ( 'NONE', ( #90323 ), #66474, .F. ) ;
#3530 = CARTESIAN_POINT ( 'NONE',  ( 207.6918009085542849, 270.9142438413412037, 7.009114282139513818 ) ) ;
#3532 = CARTESIAN_POINT ( 'NONE',  ( 192.7790337852146081, 267.5346380212243389, -12.58653425593504593 ) ) ;
#3531 = CARTESIAN_POINT ( 'NONE',  ( 180.6314016098794184, 266.8740464315611121, -14.78152555368366272 ) ) ;
#3533 = CARTESIAN_POINT ( 'NONE',  ( 84.14312167556933275, 48.98415679381830756, 0.000000000000000000 ) ) ;
#3534 = EDGE_CURVE ( 'NONE', #13682, #35306, #43152, .T. ) ;
#3535 = CARTESIAN_POINT ( 'NONE',  ( 38.93409909807770219, 22.28848085856233752, 1.475505719884397138E-15 ) ) ;
#3536 = DIRECTION ( 'NONE',  ( 0.5000000000000002220, -0.8660254037844387076, -0.000000000000000000 ) ) ;
#3537 = CARTESIAN_POINT ( 'NONE',  ( 155.4495868485232108, 261.4004128932040203, -18.48326470492642315 ) ) ;
#3538 = CARTESIAN_POINT ( 'NONE',  ( 181.8336903648691134, 273.8601736245342408, 16.48343320725793149 ) ) ;
#3539 = CARTESIAN_POINT ( 'NONE',  ( 161.0616241103177515, 273.2725257209350502, -15.13342039239440240 ) ) ;
#3540 = CARTESIAN_POINT ( 'NONE',  ( 87.21930977929280004, 43.81522300531741365, -2.732277708072506250 ) ) ;
#3541 = ADVANCED_FACE ( 'NONE', ( #73107 ), #23429, .T. ) ;
#3542 = CARTESIAN_POINT ( 'NONE',  ( 22.31343150979137846, 177.5643266524160424, 9.188101187500095079 ) ) ;
#3543 = CARTESIAN_POINT ( 'NONE',  ( -32.64350997085662698, 85.56504152958518716, 0.000000000000000000 ) ) ;
#3544 = VERTEX_POINT ( 'NONE', #77052 ) ;
#3545 = CARTESIAN_POINT ( 'NONE',  ( 87.29394575703194903, 46.02912284201620707, 8.718719511823859847 ) ) ;
#3546 = CARTESIAN_POINT ( 'NONE',  ( 175.5746833524315775, 278.5347786252573314, 16.94864957847115505 ) ) ;
#3547 = CARTESIAN_POINT ( 'NONE',  ( -50.03187330694644430, 79.58717375443625031, -10.00000000000000000 ) ) ;
#3548 = CARTESIAN_POINT ( 'NONE',  ( 40.17520546284541894, 187.8768266524160140, 9.188101187500096856 ) ) ;
#3549 = CARTESIAN_POINT ( 'NONE',  ( 87.37270799788964837, 45.80620788475513905, 8.330021955613661433 ) ) ;
#3550 = CARTESIAN_POINT ( 'NONE',  ( 190.2236813008869660, 301.1699145145108218, -5.401374690107298093 ) ) ;
#3551 = CARTESIAN_POINT ( 'NONE',  ( 41.47628181354097165, 29.11029122506297995, -8.090169943749478065 ) ) ;
#3552 = CARTESIAN_POINT ( 'NONE',  ( 178.6162270217735681, 291.6660180747913387, 6.059679334779388249 ) ) ;
#3553 = CARTESIAN_POINT ( 'NONE',  ( 191.2211340522693774, 299.4422756709672626, -8.405362570633277741 ) ) ;
#3554 = DIRECTION ( 'NONE',  ( 0.7891516029629116469, -0.6141984594095518668, 0.000000000000000000 ) ) ;
#3555 = CARTESIAN_POINT ( 'NONE',  ( -11.66892150670920891, 34.93507448871975640, 59.99999999999999289 ) ) ;
#3556 = CARTESIAN_POINT ( 'NONE',  ( 165.3037345041042840, 257.2179537824439421, -14.95315835255182613 ) ) ;
#3557 = CARTESIAN_POINT ( 'NONE',  ( 83.37579341631962393, 51.76272850660086533, 14.96038908820327329 ) ) ;
#3558 = CARTESIAN_POINT ( 'NONE',  ( 79.84079962965532218, 230.2365022471903444, 2.944929066748280225E-16 ) ) ;
#3559 = FACE_OUTER_BOUND ( 'NONE', #16522, .T. ) ;
#3560 = EDGE_CURVE ( 'NONE', #68558, #43956, #83961, .T. ) ;
#3561 = CARTESIAN_POINT ( 'NONE',  ( 161.7665152264152937, 267.7794624542035535, -16.93321476133663239 ) ) ;
#3562 = CARTESIAN_POINT ( 'NONE',  ( 55.14129374593650113, 193.4548013555410080, -4.594050593750042211 ) ) ;
#3563 = ORIENTED_EDGE ( 'NONE', *, *, #24551, .F. ) ;
#3564 = CARTESIAN_POINT ( 'NONE',  ( -16.79375656932349870, 82.86235307299436670, 14.77409422163848518 ) ) ;
#3565 = CARTESIAN_POINT ( 'NONE',  ( 146.8729474948188454, 276.2555880120147549, 3.934020695290606273 ) ) ;
#3566 = CARTESIAN_POINT ( 'NONE',  ( 67.26028111370726492, 66.44647860927366878, -8.734192759284999497 ) ) ;
#3567 = EDGE_LOOP ( 'NONE', ( #87993, #56635, #95728, #2527 ) ) ;
#3568 = CARTESIAN_POINT ( 'NONE',  ( 168.5910505471324257, 286.4687829538495976, 8.106709794022206594 ) ) ;
#3569 = CARTESIAN_POINT ( 'NONE',  ( 206.9258336080761183, 272.2409381227055292, 6.776000910836894597 ) ) ;
#3570 = DIRECTION ( 'NONE',  ( -0.9994626398093606756, -0.03277852384266333186, 0.000000000000000000 ) ) ;
#3571 = CARTESIAN_POINT ( 'NONE',  ( 24.12344523961532161, 25.87878583063842086, -9.188101187500006262 ) ) ;
#3572 = CARTESIAN_POINT ( 'NONE',  ( 73.06604476908140100, 70.70555935200820841, -7.638416365798065044 ) ) ;
#3573 = CARTESIAN_POINT ( 'NONE',  ( 196.4170778717353585, 290.4426369823788718, -17.78762421190030452 ) ) ;
#3574 = CARTESIAN_POINT ( 'NONE',  ( -22.42236680055716036, 157.8615022471903444, 5.188172501216621122E-14 ) ) ;
#3576 = ORIENTED_EDGE ( 'NONE', *, *, #62774, .T. ) ;
#3575 = VECTOR ( 'NONE', #23234, 1000.000000000000227 ) ;
#3577 = CARTESIAN_POINT ( 'NONE',  ( 14.66813190280496570, 26.65586893147755276, -7.433330006724137462 ) ) ;
#3578 = CARTESIAN_POINT ( 'NONE',  ( 173.6495897994842323, 254.4294486916353151, 8.278733075952791509 ) ) ;
#3579 = CARTESIAN_POINT ( 'NONE',  ( 77.77867966053455007, 61.43039905302717330, -16.12786080876373873 ) ) ;
#3580 = EDGE_CURVE ( 'NONE', #75751, #55973, #71245, .T. ) ;
#3581 = ORIENTED_EDGE ( 'NONE', *, *, #32602, .F. ) ;
#3582 = CARTESIAN_POINT ( 'NONE',  ( 71.99762221142530905, 71.50039512193581004, -5.770478025556951884 ) ) ;
#3583 = CARTESIAN_POINT ( 'NONE',  ( 191.4922467593309250, 298.9726946877590876, 7.604184559945784017 ) ) ;
#3584 = CARTESIAN_POINT ( 'NONE',  ( 177.3608330322163908, 256.1156063845999711, -7.251559029670058720 ) ) ;
#3585 = CARTESIAN_POINT ( 'NONE',  ( 70.85892616739612038, 65.15884113644888487, -12.74389673638816944 ) ) ;
#3586 = VERTEX_POINT ( 'NONE', #78581 ) ;
#3588 = DIRECTION ( 'NONE',  ( 0.1239754375649568946, 0.9922852870422788074, 0.000000000000000000 ) ) ;
#3587 = CARTESIAN_POINT ( 'NONE',  ( 207.8431546909062320, 270.6520914003897360, -6.441273666418043220 ) ) ;
#3589 = CARTESIAN_POINT ( 'NONE',  ( 62.42776884207837895, 218.3967562850346837, -4.648177544792955347E-16 ) ) ;
#3590 = ORIENTED_EDGE ( 'NONE', *, *, #39192, .F. ) ;
#3591 = FACE_OUTER_BOUND ( 'NONE', #73455, .T. ) ;
#3592 = CARTESIAN_POINT ( 'NONE',  ( 198.1230806404959139, 287.4877535090322453, 17.00698319228197164 ) ) ;
#3593 = CARTESIAN_POINT ( 'NONE',  ( 71.92782195476812035, 71.87540567707925732, -4.706787814905536216 ) ) ;
#3594 = CARTESIAN_POINT ( 'NONE',  ( 77.99937045744943021, 62.11896432438783933, -16.00068414206377554 ) ) ;
#3595 = CARTESIAN_POINT ( 'NONE',  ( 204.8385597977314490, 275.8562024115307167, -12.64672659107585240 ) ) ;
#3596 = CARTESIAN_POINT ( 'NONE',  ( 119.4704829489755724, 239.7833772461660544, -9.188101187500095079 ) ) ;
#3597 = DIRECTION ( 'NONE',  ( 0.000000000000000000, 0.000000000000000000, 1.000000000000000000 ) ) ;
#3598 = EDGE_CURVE ( 'NONE', #18179, #41317, #8430, .T. ) ;
#3599 = CARTESIAN_POINT ( 'NONE',  ( 66.04647798856640861, 220.4860189848785694, -2.679491924311252493 ) ) ;
#3600 = ORIENTED_EDGE ( 'NONE', *, *, #34182, .F. ) ;
#3601 = CARTESIAN_POINT ( 'NONE',  ( 164.1146561143383167, 246.3920726737087534, -7.362905700427413436 ) ) ;
#3602 = ORIENTED_EDGE ( 'NONE', *, *, #79291, .T. ) ;
#3603 = CARTESIAN_POINT ( 'NONE',  ( 37.81746515356308436, 24.76004757982092741, 5.678558825948272215 ) ) ;
#3604 = CARTESIAN_POINT ( 'NONE',  ( 198.2414483977475754, 287.2827345394944700, 16.94931984969033678 ) ) ;
#3605 = CARTESIAN_POINT ( 'NONE',  ( 204.7121744066665201, 275.6653527038535572, -12.51300999821487459 ) ) ;
#3606 = CARTESIAN_POINT ( 'NONE',  ( 70.62149783858335184, 202.3923013555409796, 4.594050593750050204 ) ) ;
#3607 = CARTESIAN_POINT ( 'NONE',  ( -32.02765978341597730, 96.24804957567249630, 11.90709431551868214 ) ) ;
#3608 = CARTESIAN_POINT ( 'NONE',  ( 190.8443993347725325, 300.0947993426467519, 8.522468760355437212 ) ) ;
#3609 = CARTESIAN_POINT ( 'NONE',  ( 150.9158774466703221, 269.2530279239659308, 15.11407781020157515 ) ) ;
#3610 = CARTESIAN_POINT ( 'NONE',  ( 175.7525910197133214, 278.2325559912325730, 16.72575950286108082 ) ) ;
#3611 = ORIENTED_EDGE ( 'NONE', *, *, #57154, .T. ) ;
#3612 = ADVANCED_FACE ( 'NONE', ( #10173 ), #32954, .F. ) ;
#3613 = CARTESIAN_POINT ( 'NONE',  ( 77.41840195283046455, 57.61794442662724691, -16.16528434754481580 ) ) ;
#3614 = CARTESIAN_POINT ( 'NONE',  ( 88.05252050592584112, 44.08395231509391721, 3.677241261923597460 ) ) ;
#3615 = VERTEX_POINT ( 'NONE', #63859 ) ;
#3616 = DIRECTION ( 'NONE',  ( -0.8660254037844378194, -0.5000000000000013323, -0.000000000000000000 ) ) ;
#3617 = CARTESIAN_POINT ( 'NONE',  ( 173.8847286580779326, 277.9849265731808146, -16.77224647300125326 ) ) ;
#3619 = EDGE_CURVE ( 'NONE', #23455, #58437, #95818, .T. ) ;
#3618 = B_SPLINE_CURVE_WITH_KNOTS ( 'NONE', 3,
 ( #52140, #13174, #65841, #44030, #82608, #74971, #36437, #66355, #67344, #75463, #98271, #28859, #90705, #34458, #26864, #88720, #42538, #73471, #4054, #29848, #30347, #52632, #45038, #15626, #7538, #69344, #60223, #15124, #77464, #6556, #60717, #93175, #46525, #22242, #45529, #53143, #83588, #61233, #37429, #47043, #68835, #31339, #46019, #38429, #30845, #61731 ),
 .UNSPECIFIED., .F., .F.,
 ( 4, 1, 2, 2, 1, 2, 2, 1, 1, 2, 2, 1, 1, 2, 2, 1, 1, 2, 2, 1, 1, 1, 2, 2, 1, 1, 1, 2, 2, 4 ),
 ( 0.000000000000000000, 0.06250000000000467681, 0.09375000000000667522, 0.1250000000000086875, 0.1875000000000168754, 0.2187500000000201505, 0.2500000000000234257, 0.3125000000000278111, 0.3437500000000300870, 0.3593750000000310307, 0.3750000000000320299, 0.4375000000000314748, 0.4687500000000301426, 0.4843750000000304201, 0.5000000000000306422, 0.5625000000000296430, 0.5937500000000290878, 0.6093750000000288658, 0.6250000000000285327, 0.6875000000000228706, 0.7187500000000199840, 0.7343750000000185407, 0.7421875000000177636, 0.7500000000000169864, 0.8125000000000105471, 0.8437500000000067724, 0.8593750000000044409, 0.8671875000000036637, 0.8750000000000029976, 1.000000000000000000 ),
 .UNSPECIFIED. ) ;
#3620 = CARTESIAN_POINT ( 'NONE',  ( 160.4332679175176963, 258.1579911225197179, -17.11564559875521141 ) ) ;
#3621 = CARTESIAN_POINT ( 'NONE',  ( 206.4797064717481305, 270.5928626827364383, 2.315921482892212779 ) ) ;
#3622 = DIRECTION ( 'NONE',  ( 0.000000000000000000, 0.000000000000000000, 1.000000000000000000 ) ) ;
#3623 = CARTESIAN_POINT ( 'NONE',  ( 164.8537203408104972, 245.1119758834023230, 2.926011033004258355 ) ) ;
#3624 = CARTESIAN_POINT ( 'NONE',  ( 71.41016749218992743, 59.45273978182970609, 15.69346469599747174 ) ) ;
#3625 = CARTESIAN_POINT ( 'NONE',  ( 39.25774830830064133, 55.25619937740606957, 177.5919119679930134 ) ) ;
#3626 = CARTESIAN_POINT ( 'NONE',  ( 167.2877554666358435, 256.3763460065391087, 13.71623913248891036 ) ) ;
#3627 = ORIENTED_EDGE ( 'NONE', *, *, #50446, .T. ) ;
#3628 = CARTESIAN_POINT ( 'NONE',  ( 1.663964738649655661, 181.7677522451419350, -5.000000000000047962 ) ) ;
#3629 = CARTESIAN_POINT ( 'NONE',  ( 122.5830220656496579, 232.3923013555409796, 4.594050593750050204 ) ) ;
#3630 = ORIENTED_EDGE ( 'NONE', *, *, #1304, .T. ) ;
#3631 = CARTESIAN_POINT ( 'NONE',  ( 191.0933613939813540, 299.6635844069401173, -8.689828987424775164 ) ) ;
#3632 = CARTESIAN_POINT ( 'NONE',  ( 15.66239703771868719, 191.3967562850346837, -4.648177544792955347E-16 ) ) ;
#3633 = CARTESIAN_POINT ( 'NONE',  ( -14.83262083840143575, 124.7156766241961208, 21.50000000000006750 ) ) ;
#3634 = CARTESIAN_POINT ( 'NONE',  ( 24.35067441160642687, 40.23626134430271861, -10.00000000000000000 ) ) ;
#3635 = CARTESIAN_POINT ( 'NONE',  ( 75.51323141522172477, 65.35427051582675517, 13.87231131232226744 ) ) ;
#3636 = CARTESIAN_POINT ( 'NONE',  ( 174.2379957965557651, 251.2590728793752248, 3.639292605338433795 ) ) ;
#3637 = ORIENTED_EDGE ( 'NONE', *, *, #82056, .F. ) ;
#3638 = CARTESIAN_POINT ( 'NONE',  ( 80.41409615687595647, 57.98253562157035645, -16.60360993379744343 ) ) ;
#3639 = CARTESIAN_POINT ( 'NONE',  ( 157.9225728654248257, 276.1116997103654285, -12.95724163227552239 ) ) ;
#3641 = CARTESIAN_POINT ( 'NONE',  ( 206.9349434189263661, 269.8064106017384916, 1.784245431258210113 ) ) ;
#3640 = DIRECTION ( 'NONE',  ( -0.8082118706970125022, -0.5888918169447047157, 0.000000000000000000 ) ) ;
#3642 = CARTESIAN_POINT ( 'NONE',  ( 206.7074763235984562, 272.6191440336236838, -10.69202547607624609 ) ) ;
#3643 = CARTESIAN_POINT ( 'NONE',  ( 142.3662031094092129, 246.8768266524159856, -9.188101187500093303 ) ) ;
#3644 = CARTESIAN_POINT ( 'NONE',  ( 190.2236813008869660, 301.1699145145108218, -5.401374690107298093 ) ) ;
#3645 = CARTESIAN_POINT ( 'NONE',  ( -77.42978507651396569, 55.80833764325424085, -10.00000000000000000 ) ) ;
#3646 = CARTESIAN_POINT ( 'NONE',  ( 174.6784134397683488, 251.9041659443967376, 3.568609730242054301 ) ) ;
#3647 = B_SPLINE_SURFACE_WITH_KNOTS ( 'NONE', 3, 1, ( 
 ( #86992, #57013 ),
 ( #80373, #18041 ),
 ( #16520, #17014 ),
 ( #95588, #26134 ),
 ( #47906, #78848 ),
 ( #56520, #9429 ),
 ( #87992, #72761 ),
 ( #55997, #95074 ),
 ( #18540, #48934 ),
 ( #78342, #40305 ),
 ( #49423, #10944 ),
 ( #41814, #71243 ),
 ( #1838, #8924 ),
 ( #39790, #31699 ),
 ( #62606, #32719 ),
 ( #63623, #94560 ),
 ( #25115, #17522 ),
 ( #79873, #48429 ),
 ( #40802, #79377 ),
 ( #9939, #71748 ),
 ( #2340, #33223 ),
 ( #24224, #31310 ),
 ( #17111, #69811 ),
 ( #70826, #86091 ),
 ( #93659, #71338 ),
 ( #16615, #54595 ),
 ( #8525, #9019 ),
 ( #54097, #55104 ),
 ( #63217, #421 ),
 ( #924, #70311 ),
 ( #31800, #47511 ),
 ( #1435, #32316 ),
 ( #78438, #78952 ),
 ( #85577, #63721 ) ),
 .UNSPECIFIED., .T., .F., .F.,
 ( 4, 2, 2, 2, 2, 2, 2, 2, 2, 2, 2, 2, 2, 2, 2, 2, 4 ),
 ( 2, 2 ),
 ( 0.000000000000000000, 0.06250000000000000000, 0.1250000000000000000, 0.1875000000000000000, 0.2500000000000000000, 0.3125000000000000000, 0.3750000000000000000, 0.4375000000000000000, 0.5000000000000000000, 0.5625000000000000000, 0.6250000000000000000, 0.6875000000000000000, 0.7500000000000000000, 0.8125000000000000000, 0.8750000000000000000, 0.9375000000000000000, 1.000000000000000000 ),
 ( 0.000000000000000000, 1.000000000000000000 ),
 .UNSPECIFIED. ) ;
#3648 = EDGE_CURVE ( 'NONE', #88304, #99270, #74813, .T. ) ;
#3649 = CARTESIAN_POINT ( 'NONE',  ( 13.69704499135956155, 32.00034080476289944, -1.878358725466461243E-16 ) ) ;
#3650 = CARTESIAN_POINT ( 'NONE',  ( 175.0864214957619822, 292.0986614963166517, -3.428571861336215054 ) ) ;
#3651 = FACE_OUTER_BOUND ( 'NONE', #3977, .T. ) ;
#3652 = CARTESIAN_POINT ( 'NONE',  ( 169.8838196135249348, 285.4608273923216188, -7.965848187381914691 ) ) ;
#3653 = CARTESIAN_POINT ( 'NONE',  ( 154.9067123643522734, 262.3406990819208886, -18.18534662427576265 ) ) ;
#3654 = ADVANCED_FACE ( 'NONE', ( #2582 ), #54741, .F. ) ;
#3655 = CARTESIAN_POINT ( 'NONE',  ( 193.6272073153312476, 288.5543963742453570, 16.06608169681408782 ) ) ;
#3656 = CARTESIAN_POINT ( 'NONE',  ( 144.1251436611898953, 244.0177522451417644, 5.000000000000051514 ) ) ;
#3657 = EDGE_CURVE ( 'NONE', #99249, #18043, #18277, .T. ) ;
#3658 = CARTESIAN_POINT ( 'NONE',  ( 78.05914692549418987, 52.71672065815211994, -15.71920831139273211 ) ) ;
#3659 = ORIENTED_EDGE ( 'NONE', *, *, #78524, .F. ) ;
#3660 = EDGE_CURVE ( 'NONE', #95480, #29721, #41549, .T. ) ;
#3662 = CARTESIAN_POINT ( 'NONE',  ( 196.1241105319816143, 290.9500712997905794, 15.97146679939154268 ) ) ;
#3661 = AXIS2_PLACEMENT_3D ( 'NONE', #53912, #75264, #76263 ) ;
#3663 = CARTESIAN_POINT ( 'NONE',  ( 190.4281805785508084, 300.8157113754859893, -1.233909217199055774 ) ) ;
#3664 = CARTESIAN_POINT ( 'NONE',  ( -10.75808714510939090, 164.5958772461660544, -9.188101187500095079 ) ) ;
#3665 = CARTESIAN_POINT ( 'NONE',  ( 33.89617418964321871, 196.5024278399160949, -9.188101187500093303 ) ) ;
#3666 = CARTESIAN_POINT ( 'NONE',  ( 178.4777856415780946, 273.6615857960989047, -17.31426804045896617 ) ) ;
#3667 = CARTESIAN_POINT ( 'NONE',  ( 20.17205688044380452, 16.81029122506294371, 8.090169943749479842 ) ) ;
#3668 = FACE_OUTER_BOUND ( 'NONE', #77964, .T. ) ;
#3669 = CARTESIAN_POINT ( 'NONE',  ( 157.1965120183049578, 258.3746497421212780, -18.06591467563559306 ) ) ;
#3670 = CARTESIAN_POINT ( 'NONE',  ( 72.02714983513547509, 72.27104924840581646, -3.542005090554713576 ) ) ;
#3671 = CARTESIAN_POINT ( 'NONE',  ( 146.8000281410530192, 276.3818880375922049, 4.652863924796177386 ) ) ;
#3672 = CARTESIAN_POINT ( 'NONE',  ( 73.91582514665041970, 54.93225018311873953, -16.13162452324062102 ) ) ;
#3674 = CARTESIAN_POINT ( 'NONE',  ( 67.98707691180791812, 223.3927522451419350, 2.944929066748280225E-16 ) ) ;
#3673 = CARTESIAN_POINT ( 'NONE',  ( 167.5121282280925925, 256.6568260522151945, 13.80861252335286515 ) ) ;
#3675 = CARTESIAN_POINT ( 'NONE',  ( 74.71692913107121115, 67.15988951933469764, 12.46506041926016728 ) ) ;
#3676 = CARTESIAN_POINT ( 'NONE',  ( 27.47308016966368882, 31.56454794089043503, 10.00000000000000355 ) ) ;
#3677 = FACE_OUTER_BOUND ( 'NONE', #17782, .T. ) ;
#3678 = CARTESIAN_POINT ( 'NONE',  ( 43.39556388706024848, 195.8615022471902591, -10.00000000000009592 ) ) ;
#3679 = CARTESIAN_POINT ( 'NONE',  ( -22.42236680055709641, 157.8615022471902591, 0.000000000000000000 ) ) ;
#3680 = CARTESIAN_POINT ( 'NONE',  ( 83.37296956034944628, 51.74080471427829764, 14.95189368521466733 ) ) ;
#3681 = CARTESIAN_POINT ( 'NONE',  ( 4.668163907683432257, 167.3768266524159856, -9.188101187500091527 ) ) ;
#3682 = CARTESIAN_POINT ( 'NONE',  ( 37.28583507901048932, 30.03085787977765975, 9.188101187500006262 ) ) ;
#3683 = CYLINDRICAL_SURFACE ( 'NONE', #20134, 17.82106496071139645 ) ;
#3684 = CARTESIAN_POINT ( 'NONE',  ( 33.29424590502123493, 178.4824982072973683, 3.021315404115420679E-15 ) ) ;
#3685 = CARTESIAN_POINT ( 'NONE',  ( 40.42214693012152793, 25.19860640527295104, 2.839279412974134775 ) ) ;
#3686 = CARTESIAN_POINT ( 'NONE',  ( 206.4943150373521803, 272.9883502116088039, 11.34100825923693101 ) ) ;
#3687 = CARTESIAN_POINT ( 'NONE',  ( 180.1994282899806592, 277.1211297568123086, 16.31084869235452217 ) ) ;
#3688 = CARTESIAN_POINT ( 'NONE',  ( 193.7999837595647250, 294.9755769528473479, 15.24609078262870199 ) ) ;
#3689 = CARTESIAN_POINT ( 'NONE',  ( 196.2878005184348353, 290.6665519265632724, -16.69183432842427806 ) ) ;
#3690 = CARTESIAN_POINT ( 'NONE',  ( 179.6275593323862267, 262.7184705051237188, -12.85240121697976612 ) ) ;
#3691 = DIRECTION ( 'NONE',  ( 1.000000000000000000, 0.000000000000000000, 0.000000000000000000 ) ) ;
#3692 = CARTESIAN_POINT ( 'NONE',  ( 6.089662503932698812, 18.91421378149916421, 9.188101187500008038 ) ) ;
#3693 = CARTESIAN_POINT ( 'NONE',  ( 172.3986314675530309, 263.7922717222033384, -16.89442142407995107 ) ) ;
#3694 = CARTESIAN_POINT ( 'NONE',  ( 12.04840505635704417, 25.14336893147754282, 7.433330006724141015 ) ) ;
#3695 = FACE_OUTER_BOUND ( 'NONE', #33468, .T. ) ;
#3696 = CARTESIAN_POINT ( 'NONE',  ( 26.18314342202568668, 41.82794442100486521, -10.00000000000000000 ) ) ;
#3697 = ORIENTED_EDGE ( 'NONE', *, *, #51113, .F. ) ;
#3698 = CARTESIAN_POINT ( 'NONE',  ( 155.8897943095830954, 276.0389231161490784, 10.29249315839296663 ) ) ;
#3699 = CARTESIAN_POINT ( 'NONE',  ( 81.10883903633204284, 42.55625711771581621, 7.933723778126640092 ) ) ;
#3700 = VERTEX_POINT ( 'NONE', #43029 ) ;
#3701 = PRODUCT_DEFINITION ( 'UNKNOWN', '', #60799, #41236 ) ;
#3702 = CARTESIAN_POINT ( 'NONE',  ( 192.7944000592152634, 296.7172990131160759, 11.44860011299869740 ) ) ;
#3703 = CARTESIAN_POINT ( 'NONE',  ( 206.9878665138179770, 272.1334939782196329, 6.566295309274049252 ) ) ;
#3704 = CARTESIAN_POINT ( 'NONE',  ( 29.42114147039228200, 17.39040679176983772, 1.333680081654574804E-15 ) ) ;
#3705 = ORIENTED_EDGE ( 'NONE', *, *, #85328, .T. ) ;
#3706 = ORIENTED_EDGE ( 'NONE', *, *, #52020, .F. ) ;
#3708 = CARTESIAN_POINT ( 'NONE',  ( 72.26538907532096800, 200.9824982072973967, 3.021315404115420679E-15 ) ) ;
#3707 = CARTESIAN_POINT ( 'NONE',  ( 159.1993561622898596, 279.5966400365493882, -9.758000324901335176 ) ) ;
#3709 = CARTESIAN_POINT ( 'NONE',  ( 85.85265132163431190, 47.44586991713101298, 10.77177032529229983 ) ) ;
#3710 = ORIENTED_EDGE ( 'NONE', *, *, #70214, .T. ) ;
#3711 = CARTESIAN_POINT ( 'NONE',  ( 77.46027058111894803, 55.89456704637984785, 16.15791935774714361 ) ) ;
#3712 = PLANE ( 'NONE',  #92097 ) ;
#3713 = ORIENTED_EDGE ( 'NONE', *, *, #64048, .T. ) ;
#3714 = CARTESIAN_POINT ( 'NONE',  ( 38.63240046701410080, 22.70852965304481330, 1.583844403245330712 ) ) ;
#3715 = CARTESIAN_POINT ( 'NONE',  ( 78.81221140396398539, 50.25556598462433300, -14.90820057926957176 ) ) ;
#3716 = CARTESIAN_POINT ( 'NONE',  ( 196.9976074755333286, 289.4371302133026802, -16.79549473444794216 ) ) ;
#3717 = EDGE_CURVE ( 'NONE', #5821, #7928, #4334, .T. ) ;
#3718 = VECTOR ( 'NONE', #72842, 1000.000000000000114 ) ;
#3719 = CARTESIAN_POINT ( 'NONE',  ( 80.70996417611414131, 43.44255574045367041, 9.435838178707639301 ) ) ;
#3720 = ORIENTED_EDGE ( 'NONE', *, *, #32301, .F. ) ;
#3721 = CARTESIAN_POINT ( 'NONE',  ( 200.9110265982630779, 282.6588894614233141, 17.52479721249226685 ) ) ;
#3722 = CARTESIAN_POINT ( 'NONE',  ( 166.5515458049821973, 274.4079129713531415, -15.18104102794923982 ) ) ;
#3723 = CARTESIAN_POINT ( 'NONE',  ( 73.18824967679846338, 57.61170437758888596, 15.86128386422620196 ) ) ;
#3724 = ORIENTED_EDGE ( 'NONE', *, *, #21888, .T. ) ;
#3725 = CARTESIAN_POINT ( 'NONE',  ( 174.5155504680193417, 276.9095236141292844, -16.96454991327265205 ) ) ;
#3726 = CARTESIAN_POINT ( 'NONE',  ( 42.18527710189642477, 24.75978393459168458, -1.583844403245396437 ) ) ;
#3727 = VECTOR ( 'NONE', #91936, 1000.000000000000114 ) ;
#3728 = ORIENTED_EDGE ( 'NONE', *, *, #20597, .T. ) ;
#3729 = CARTESIAN_POINT ( 'NONE',  ( 156.6812872898450735, 261.2670451491295012, 0.000000000000000000 ) ) ;
#3730 = ORIENTED_EDGE ( 'NONE', *, *, #19548, .T. ) ;
#3731 = CYLINDRICAL_SURFACE ( 'NONE', #89747, 17.82106496071139645 ) ;
#3732 = ORIENTED_EDGE ( 'NONE', *, *, #73853, .F. ) ;
#3733 = CARTESIAN_POINT ( 'NONE',  ( 168.6570739278365068, 272.7872155009642370, 15.97839558931424975 ) ) ;
#3734 = CARTESIAN_POINT ( 'NONE',  ( 194.0793808334966570, 294.4916470253114085, 14.16320079385157626 ) ) ;
#3735 = CYLINDRICAL_SURFACE ( 'NONE', #52900, 10.00000000000010658 ) ;
#3737 = EDGE_CURVE ( 'NONE', #14175, #86029, #76396, .T. ) ;
#3736 = CARTESIAN_POINT ( 'NONE',  ( 69.63741438990557242, 65.54831403221679409, 11.22893310010135437 ) ) ;
#3738 = LINE ( 'NONE', #9847, #43625 ) ;
#3739 = CARTESIAN_POINT ( 'NONE',  ( 86.61622014653730162, 43.24285245142148426, 0.7059395827112208144 ) ) ;
#3740 = CARTESIAN_POINT ( 'NONE',  ( 197.6052335461745599, 288.3846909869485557, -16.86014524025736350 ) ) ;
#3741 = VECTOR ( 'NONE', #88105, 1000.000000000000227 ) ;
#3742 = VERTEX_POINT ( 'NONE', #57247 ) ;
#3743 = LINE ( 'NONE', #65519, #77134 ) ;
#3744 = B_SPLINE_CURVE_WITH_KNOTS ( 'NONE', 3,
 ( #68238, #37335, #59122, #29259, #67245, #51040, #76367, #44439, #5952, #51552, #22148, #90606, #99161, #13568, #12570, #75371, #5459, #52537, #90095, #53039, #36343, #81997, #91090, #14054, #21655, #60127, #83994, #29749, #60621, #20663, #82991, #91576, #13076, #82514, #43937, #74876, #21172, #98175, #28754, #14558, #45433, #97196, #43446, #59633, #52053, #36846, #83488, #6939, #67754, #74388, #44933, #27763 ),
 .UNSPECIFIED., .F., .F.,
 ( 4, 2, 2, 2, 2, 2, 2, 2, 2, 2, 2, 2, 2, 2, 2, 2, 2, 2, 2, 2, 2, 2, 2, 2, 2, 4 ),
 ( 0.0002156964707596482531, 0.001236790380387270492, 0.001747337335201052094, 0.002002610812607897358, 0.002130247551311319557, 0.002257884290014742189, 0.002385521028718164387, 0.002513157767421587020, 0.002768431244828421876, 0.003278978199642059495, 0.004300072109269333434, 0.005321166018896607806, 0.005831712973710208130, 0.006086986451116970995, 0.006342259928523734727, 0.006406078297875446477, 0.006469896667227158227, 0.006533715036578869977, 0.006597533405930581726, 0.006725170144634006961, 0.006852806883337431328, 0.007363353838151069815, 0.007618627315557889058, 0.007873900792964709169, 0.008129174270371528413, 0.008384447747778347657 ),
 .UNSPECIFIED. ) ;
#3745 = CARTESIAN_POINT ( 'NONE',  ( 28.38260615371904905, 22.10170272979928185, -7.433330006724141015 ) ) ;
#3746 = CARTESIAN_POINT ( 'NONE',  ( 178.3810821012210113, 281.7766761570669587, -16.43735388118292917 ) ) ;
#3747 = FACE_OUTER_BOUND ( 'NONE', #68337, .T. ) ;
#3748 = ORIENTED_EDGE ( 'NONE', *, *, #81477, .T. ) ;
#3749 = CARTESIAN_POINT ( 'NONE',  ( 187.3225772020536795, 276.9076140642868609, 17.54334712858875989 ) ) ;
#3750 = CARTESIAN_POINT ( 'NONE',  ( 171.7154418923348942, 259.3365693118849435, -15.26938553599716641 ) ) ;
#3751 = CARTESIAN_POINT ( 'NONE',  ( -15.23834836788960345, 40.22511121182390070, 59.99999999999999289 ) ) ;
#3752 = CARTESIAN_POINT ( 'NONE',  ( 130.8844835975280887, 234.8262482093457493, 3.021315404115420679E-15 ) ) ;
#3753 = CARTESIAN_POINT ( 'NONE',  ( 198.6303137791167330, 286.6091999416584599, -17.67087462607727488 ) ) ;
#3754 = CARTESIAN_POINT ( 'NONE',  ( 190.0302884585784398, 301.5048807432094122, -1.372174654977964536 ) ) ;
#3755 = ORIENTED_EDGE ( 'NONE', *, *, #56258, .T. ) ;
#3756 = CARTESIAN_POINT ( 'NONE',  ( -44.49648453423614569, 28.96346851210257967, 10.00000000000000000 ) ) ;
#3757 = LINE ( 'NONE', #87431, #80368 ) ;
#3758 = CARTESIAN_POINT ( 'NONE',  ( 155.4341113147262945, 261.7935976400785876, 16.97053765338380771 ) ) ;
#3759 = CARTESIAN_POINT ( 'NONE',  ( 38.03703169759612734, 192.7677522451418781, 10.00000000000009592 ) ) ;
#3760 = CARTESIAN_POINT ( 'NONE',  ( 104.8563042601131770, 231.3458772461660544, 9.188101187500095079 ) ) ;
#3761 = CARTESIAN_POINT ( 'NONE',  ( 82.76725405737721530, 40.62549709574067691, -1.366123307036881229 ) ) ;
#3762 = FACE_OUTER_BOUND ( 'NONE', #47597, .T. ) ;
#3763 = PLANE ( 'NONE',  #69243 ) ;
#3764 = CARTESIAN_POINT ( 'NONE',  ( 20.41882739113040302, 182.5958772461660544, -9.188101187500095079 ) ) ;
#3765 = CARTESIAN_POINT ( 'NONE',  ( 170.8463542321686077, 287.4393069310528972, -8.645854640182026429 ) ) ;
#3766 = ORIENTED_EDGE ( 'NONE', *, *, #38014, .F. ) ;
#3767 = ORIENTED_EDGE ( 'NONE', *, *, #10271, .T. ) ;
#3768 = CARTESIAN_POINT ( 'NONE',  ( 187.6513412634644169, 261.2126229280032135, -5.876874455337775416 ) ) ;
#3769 = B_SPLINE_CURVE_WITH_KNOTS ( 'NONE', 3,
 ( #25085, #57480, #71723, #26107, #34689, #9400, #87480, #87967, #72733, #33714, #18511, #49897, #42279, #49397, #80344, #10912, #88463, #41787, #18015, #3323, #33196, #86459, #96047, #65094, #64097, #48907, #55473, #65590, #95043, #79842, #9914, #10408, #19024, #78814, #80855, #40275, #79348, #16984, #47875, #25606, #56493, #11427, #71216, #2825, #1807, #32691, #41278, #55966, #86961, #17496, #48401, #35693 ),
 .UNSPECIFIED., .F., .F.,
 ( 4, 2, 2, 2, 2, 2, 2, 2, 2, 2, 2, 2, 2, 2, 2, 2, 2, 2, 2, 2, 2, 2, 2, 2, 2, 4 ),
 ( 0.0001612845407840359966, 0.0006508920563406033269, 0.001140499571897170793, 0.001385303329675468620, 0.001507705208564656891, 0.001630107087453845595, 0.001752508966343033865, 0.001874910845232222135, 0.002119714603010437563, 0.002609322118566773877, 0.003098929634123110191, 0.004078144665235782819, 0.005057359696348456314, 0.005546967211904781786, 0.005791770969682908526, 0.005914172848572016132, 0.006036574727461122870, 0.006097775666905676240, 0.006158976606350230476, 0.006281378485239340684, 0.006526182243017528140, 0.006770986000795716463, 0.007015789758573903918, 0.007260593516352092242, 0.007505397274130279697, 0.007995004789686802060 ),
 .UNSPECIFIED. ) ;
#3770 = DIRECTION ( 'NONE',  ( 0.5000000000000014433, -0.8660254037844378194, 0.000000000000000000 ) ) ;
#3771 = CARTESIAN_POINT ( 'NONE',  ( 74.56414817410228579, 187.8759306620403322, -17.47570218321536117 ) ) ;
#3772 = CARTESIAN_POINT ( 'NONE',  ( 192.9739757011855659, 263.8060229890649566, -4.212473007787504997 ) ) ;
#3773 = CYLINDRICAL_SURFACE ( 'NONE', #38163, 5.000000000000058620 ) ;
#3774 = LINE ( 'NONE', #34656, #25549 ) ;
#3775 = CARTESIAN_POINT ( 'NONE',  ( 167.6119263830523778, 251.7459577958838679, 10.36624589958357490 ) ) ;
#3776 = CARTESIAN_POINT ( 'NONE',  ( 41.52819660837609916, 194.7833772461660544, -9.188101187500095079 ) ) ;
#3777 = CARTESIAN_POINT ( 'NONE',  ( 87.83349241520130590, 231.5177522451419350, 5.000000000000046185 ) ) ;
#3778 = ORIENTED_EDGE ( 'NONE', *, *, #15190, .F. ) ;
#3779 = CARTESIAN_POINT ( 'NONE',  ( 83.35260738844563377, 45.68874033332231477, 10.31089094078401303 ) ) ;
#3780 = ADVANCED_FACE ( 'NONE', ( #12678 ), #11679, .T. ) ;
#3781 = CARTESIAN_POINT ( 'NONE',  ( -7.604263460676718545, 177.9637435831425023, 2.679491924311251605 ) ) ;
#3782 = CARTESIAN_POINT ( 'NONE',  ( 3.071516343397128423, 163.3923013555410080, 4.594050593750050204 ) ) ;
#3783 = CARTESIAN_POINT ( 'NONE',  ( 68.70848240496243875, 63.96496568607160071, -12.08092966280174529 ) ) ;
#3784 = CARTESIAN_POINT ( 'NONE',  ( 150.9584389135710865, 269.1793093008492406, -15.82751450793727699 ) ) ;
#3785 = CARTESIAN_POINT ( 'NONE',  ( 81.07888283437659993, 54.57333583963867341, 16.21189145771869988 ) ) ;
#3786 = CARTESIAN_POINT ( 'NONE',  ( 146.9700173529739970, 276.0874580858064746, -5.099093031535578469 ) ) ;
#3787 = AXIS2_PLACEMENT_3D ( 'NONE', #20599, #28182, #12003 ) ;
#3788 = DIRECTION ( 'NONE',  ( -0.8660254037844379305, -0.5000000000000012212, 0.000000000000000000 ) ) ;
#3789 = CARTESIAN_POINT ( 'NONE',  ( 164.4761815919938215, 245.7658921781788592, 6.833796894895563412 ) ) ;
#3790 = CARTESIAN_POINT ( 'NONE',  ( 147.2999496562918296, 275.5159985734018164, -0.1418322875769767455 ) ) ;
#3791 = CARTESIAN_POINT ( 'NONE',  ( 207.1059763530604698, 271.9289217357780899, 6.370907250589925575 ) ) ;
#3792 = ORIENTED_EDGE ( 'NONE', *, *, #7604, .F. ) ;
#3793 = CARTESIAN_POINT ( 'NONE',  ( -4.668846022976095966, 168.1115022471902591, 10.00000000000009592 ) ) ;
#3794 = CARTESIAN_POINT ( 'NONE',  ( 85.29362735876655677, 48.41412782346650800, 12.38048700662147716 ) ) ;
#3795 = VECTOR ( 'NONE', #10139, 1000.000000000000227 ) ;
#3796 = CARTESIAN_POINT ( 'NONE',  ( 121.0403275412173656, 234.5643266524160140, 9.188101187500095079 ) ) ;
#3797 = CARTESIAN_POINT ( 'NONE',  ( 19.57800816787531417, 26.70171378149919050, -9.188101187500004485 ) ) ;
#3798 = CARTESIAN_POINT ( 'NONE',  ( 193.5005633302724277, 262.8551920378705518, -5.236817587991198231 ) ) ;
#3799 = CARTESIAN_POINT ( 'NONE',  ( -110.0000000000000142, 0.000000000000000000, -9.212605237762106825 ) ) ;
#3800 = AXIS2_PLACEMENT_3D ( 'NONE', #52280, #74112, #5685 ) ;
#3802 = CARTESIAN_POINT ( 'NONE',  ( 149.3166057054752400, 247.0244633538772234, 5.014128649969458174 ) ) ;
#3801 = CARTESIAN_POINT ( 'NONE',  ( 157.3025066944120454, 258.1910615777721887, 18.21299529665260053 ) ) ;
#3803 = CARTESIAN_POINT ( 'NONE',  ( 150.2762856237821438, 270.3608334573137881, -14.20317525964708061 ) ) ;
#3804 = ORIENTED_EDGE ( 'NONE', *, *, #12922, .F. ) ;
#3805 = CARTESIAN_POINT ( 'NONE',  ( 151.3560786774222322, 268.4905770267490652, 15.54402364351346932 ) ) ;
#3806 = CARTESIAN_POINT ( 'NONE',  ( 207.9405038940993222, 270.4834776343830640, -0.2435786705607262403 ) ) ;
#3807 = CARTESIAN_POINT ( 'NONE',  ( 87.73298548431469612, 44.18903561216111342, 4.633618514853094617 ) ) ;
#3808 = CARTESIAN_POINT ( 'NONE',  ( 180.6066648745947134, 283.7006809008031496, -16.18202752516933174 ) ) ;
#3809 = CARTESIAN_POINT ( 'NONE',  ( 81.78211920620266540, 55.43645730098403135, -15.94077319035399221 ) ) ;
#3810 = ORIENTED_EDGE ( 'NONE', *, *, #20842, .F. ) ;
#3811 = CARTESIAN_POINT ( 'NONE',  ( 139.3620039403755015, 241.2677522451417929, -5.000000000000041744 ) ) ;
#3812 = CARTESIAN_POINT ( 'NONE',  ( 165.3884017376936129, 269.6430054510781815, -16.30567925014516817 ) ) ;
#3813 = CARTESIAN_POINT ( 'NONE',  ( 86.01647438233806042, 46.20655162549090988, 9.232364010202251947 ) ) ;
#3814 = CARTESIAN_POINT ( 'NONE',  ( 80.05167170976248769, 53.91814069023228484, 15.77049608246057488 ) ) ;
#3815 = CARTESIAN_POINT ( 'NONE',  ( 180.7877299985295565, 263.4844111323488960, 14.67210611338813919 ) ) ;
#3816 = DIRECTION ( 'NONE',  ( 0.000000000000000000, 0.000000000000000000, -1.000000000000000000 ) ) ;
#3817 = ORIENTED_EDGE ( 'NONE', *, *, #84109, .T. ) ;
#3818 = CARTESIAN_POINT ( 'NONE',  ( -69.42519150082246426, 45.64199051378594874, -10.00000000000000000 ) ) ;
#3819 = CARTESIAN_POINT ( 'NONE',  ( 45.09207854535236493, 28.96004757982094446, -5.678558825948276656 ) ) ;
#3820 = CARTESIAN_POINT ( 'NONE',  ( 174.4355206875066813, 273.1373033844686802, -16.36721432446067936 ) ) ;
#3821 = ORIENTED_EDGE ( 'NONE', *, *, #28259, .T. ) ;
#3822 = DIRECTION ( 'NONE',  ( 0.5000000000000013323, -0.8660254037844378194, 0.000000000000000000 ) ) ;
#3823 = CARTESIAN_POINT ( 'NONE',  ( 148.3025927079438304, 273.7793698660844939, -8.046026357031887954 ) ) ;
#3824 = CARTESIAN_POINT ( 'NONE',  ( 156.3384060043484567, 261.3563118228615849, -17.44929643486769777 ) ) ;
#3825 = VERTEX_POINT ( 'NONE', #88221 ) ;
#3826 = CARTESIAN_POINT ( 'NONE',  ( 78.98760635313000478, 59.78900401997537273, 16.49402793498109432 ) ) ;
#3827 = CARTESIAN_POINT ( 'NONE',  ( 184.9118810634971339, 291.9181506604203378, 12.13670245241820567 ) ) ;
#3828 = EDGE_CURVE ( 'NONE', #759, #13192, #59173, .T. ) ;
#3829 = ORIENTED_EDGE ( 'NONE', *, *, #24300, .T. ) ;
#3830 = CARTESIAN_POINT ( 'NONE',  ( 76.49585787082935440, 52.49147331306175346, -15.83840385325085265 ) ) ;
#3831 = CARTESIAN_POINT ( 'NONE',  ( 80.55977923476241642, 44.53388773478042140, 11.41474457639882978 ) ) ;
#3832 = CARTESIAN_POINT ( 'NONE',  ( 84.51897762134323955, 49.81277137233040264, -13.22473897856888847 ) ) ;
#3833 = CARTESIAN_POINT ( 'NONE',  ( 184.2569950528642551, 259.4484375049545406, -5.816461788221651830 ) ) ;
#3834 = VERTEX_POINT ( 'NONE', #59223 ) ;
#3835 = EDGE_LOOP ( 'NONE', ( #34684, #69097, #31191, #76041 ) ) ;
#3836 = CARTESIAN_POINT ( 'NONE',  ( 175.1230978711317618, 258.7486093689314544, 12.66210094468590697 ) ) ;
#3837 = ORIENTED_EDGE ( 'NONE', *, *, #61776, .T. ) ;
#3838 = CARTESIAN_POINT ( 'NONE',  ( 77.06564511512083016, 49.52831132331507291, 14.97822083552720329 ) ) ;
#3840 = EDGE_CURVE ( 'NONE', #54783, #63867, #44032, .T. ) ;
#3839 = ORIENTED_EDGE ( 'NONE', *, *, #3660, .T. ) ;
#3841 = CARTESIAN_POINT ( 'NONE',  ( 75.32469880294877385, 60.28293755603083071, 15.62353883029713408 ) ) ;
#3842 = CARTESIAN_POINT ( 'NONE',  ( 154.8833801513861772, 262.3811116602312268, -17.49275566389638215 ) ) ;
#3843 = ORIENTED_EDGE ( 'NONE', *, *, #39130, .F. ) ;
#3844 = CARTESIAN_POINT ( 'NONE',  ( 93.96857342517718337, -8.000000000000000000, 9.212605237762133470 ) ) ;
#3845 = CARTESIAN_POINT ( 'NONE',  ( 82.34058838678610925, 40.67931664917913537, 3.225392581287613414 ) ) ;
#3846 = CARTESIAN_POINT ( 'NONE',  ( 151.6442999004562751, 268.6057199523998520, 14.65032303984580686 ) ) ;
#3847 = CARTESIAN_POINT ( 'NONE',  ( 159.3761195245467377, 275.4568327680622701, -12.53322028322178916 ) ) ;
#3849 = EDGE_CURVE ( 'NONE', #92132, #44698, #74487, .T. ) ;
#3848 = CARTESIAN_POINT ( 'NONE',  ( 153.3859906278383676, 264.9746663937372091, -17.41799046551451013 ) ) ;
#3850 = DIRECTION ( 'NONE',  ( -1.000000000000000000, 0.000000000000000000, 0.000000000000000000 ) ) ;
#3851 = CARTESIAN_POINT ( 'NONE',  ( 157.6439063144099180, 281.5864387313514499, 2.957906020347658593 ) ) ;
#3852 = CARTESIAN_POINT ( 'NONE',  ( 131.1886288721100300, 255.7369531367911293, -4.594050593750048428 ) ) ;
#3853 = CARTESIAN_POINT ( 'NONE',  ( 75.63696794127041301, 54.59993838101707553, 16.11484836142631494 ) ) ;
#3854 = CARTESIAN_POINT ( 'NONE',  ( 11.99908958663318970, 18.87878583063839955, -9.188101187500006262 ) ) ;
#3855 = ORIENTED_EDGE ( 'NONE', *, *, #89326, .T. ) ;
#3857 = ORIENTED_EDGE ( 'NONE', *, *, #24551, .T. ) ;
#3856 = CARTESIAN_POINT ( 'NONE',  ( 85.42558612123971784, 48.32295466858820987, -12.24938428992805406 ) ) ;
#3858 = CARTESIAN_POINT ( 'NONE',  ( 3.578749241215597010, 161.3262482093458061, 3.021315404115420679E-15 ) ) ;
#3859 = CARTESIAN_POINT ( 'NONE',  ( -9.065681333110875428, 177.1199935810941213, 2.679491924311251605 ) ) ;
#3860 = CARTESIAN_POINT ( 'NONE',  ( 170.8526566076953088, 288.1261369771856948, -5.563456055268631850 ) ) ;
#3861 = CARTESIAN_POINT ( 'NONE',  ( 156.7700855017945401, 279.3500026499473279, 7.384081754847029444 ) ) ;
#3862 = CARTESIAN_POINT ( 'NONE',  ( 120.7221038307704788, 252.0530062829862743, -4.648177544792955347E-16 ) ) ;
#3863 = CARTESIAN_POINT ( 'NONE',  ( 173.7893683034945411, 252.1476285642659150, 6.872699842875177545 ) ) ;
#3864 = AXIS2_PLACEMENT_3D ( 'NONE', #49789, #66483, #80752 ) ;
#3865 = CARTESIAN_POINT ( 'NONE',  ( 168.1011763779767989, 253.1388740643201629, 11.70041143357935631 ) ) ;
#3866 = CARTESIAN_POINT ( 'NONE',  ( 88.27690704811887201, 44.27260258506650814, -1.937958420041432595 ) ) ;
#3867 = ORIENTED_EDGE ( 'NONE', *, *, #82047, .F. ) ;
#3868 = FACE_OUTER_BOUND ( 'NONE', #21734, .T. ) ;
#3869 = VECTOR ( 'NONE', #18612, 1000.000000000000114 ) ;
#3870 = ORIENTED_EDGE ( 'NONE', *, *, #76643, .F. ) ;
#3871 = PLANE ( 'NONE',  #32203 ) ;
#3872 = VECTOR ( 'NONE', #44525, 1000.000000000000000 ) ;
#3873 = CARTESIAN_POINT ( 'NONE',  ( 204.8003314451236463, 269.2376841632477635, -2.968733614000913068 ) ) ;
#3874 = DIRECTION ( 'NONE',  ( -0.8660254037844384856, -0.5000000000000002220, -3.252519625699449945E-16 ) ) ;
#3875 = DIRECTION ( 'NONE',  ( 0.000000000000000000, -0.000000000000000000, 1.000000000000000000 ) ) ;
#3876 = CARTESIAN_POINT ( 'NONE',  ( 202.5245888501533216, 279.8641176599742266, 15.60152447840272494 ) ) ;
#3878 = CARTESIAN_POINT ( 'NONE',  ( 88.01573842283471549, 44.26461227791823205, 2.810035873497462422 ) ) ;
#3877 = CARTESIAN_POINT ( 'NONE',  ( 152.3249143222120381, 268.8125044657937792, -15.54600960379902297 ) ) ;
#3879 = CARTESIAN_POINT ( 'NONE',  ( 203.3440828345331965, 270.0445236297473457, 6.009308755609846564 ) ) ;
#3880 = ORIENTED_EDGE ( 'NONE', *, *, #37565, .F. ) ;
#3881 = PRODUCT_DEFINITION_SHAPE ( 'NONE', 'NONE',  #100298 ) ;
#3882 = EDGE_CURVE ( 'NONE', #44895, #75103, #68521, .T. ) ;
#3883 = CARTESIAN_POINT ( 'NONE',  ( 75.77888672275405213, 61.25515952569155331, -15.46323051080574373 ) ) ;
#3884 = CARTESIAN_POINT ( 'NONE',  ( 119.5336306364421404, 246.4865022471903160, 10.00000000000009415 ) ) ;
#3885 = EDGE_CURVE ( 'NONE', #5196, #29361, #26371, .T. ) ;
#3886 = CARTESIAN_POINT ( 'NONE',  ( 14.22133309352410002, 169.0177522451418213, 5.000000000000051514 ) ) ;
#3887 = CARTESIAN_POINT ( 'NONE',  ( 149.0247308281161622, 274.5285899518638075, 9.115861392502811356 ) ) ;
#3888 = DIRECTION ( 'NONE',  ( -0.8660254037844387076, -0.4999999999999998890, -0.000000000000000000 ) ) ;
#3889 = DIRECTION ( 'NONE',  ( 0.4174706225611858335, 0.9086904199442051855, 0.000000000000000000 ) ) ;
#3890 = CARTESIAN_POINT ( 'NONE',  ( 8.781437479894508513, 182.0024278399160949, 9.188101187500095079 ) ) ;
#3891 = CARTESIAN_POINT ( 'NONE',  ( 106.3175485811169239, 238.3149278399160949, -9.188101187500095079 ) ) ;
#3892 = CARTESIAN_POINT ( 'NONE',  ( 154.8786460229866577, 262.3893114111486398, -18.06164891362396929 ) ) ;
#3893 = DIRECTION ( 'NONE',  ( -0.8660254037844387076, -0.4999999999999998890, -0.000000000000000000 ) ) ;
#3894 = CARTESIAN_POINT ( 'NONE',  ( 180.7705417327010196, 254.9826106211711192, -2.480839038887178827 ) ) ;
#3895 = LINE ( 'NONE', #66191, #27036 ) ;
#3896 = ADVANCED_FACE ( 'NONE', ( #19777 ), #81598, .F. ) ;
#3897 = FACE_OUTER_BOUND ( 'NONE', #16165, .T. ) ;
#3898 = CYLINDRICAL_SURFACE ( 'NONE', #59853, 10.00000000000010658 ) ;
#3899 = CARTESIAN_POINT ( 'NONE',  ( 147.6508870500795467, 274.9081571770856272, -8.950912509993816712 ) ) ;
#3900 = EDGE_CURVE ( 'NONE', #37554, #75967, #11186, .T. ) ;
#3901 = ADVANCED_FACE ( 'NONE', ( #42540 ), #89709, .F. ) ;
#3902 = PLANE ( 'NONE',  #60450 ) ;
#3903 = CARTESIAN_POINT ( 'NONE',  ( 205.5958069356747728, 274.5446118947268701, -13.04136175932365305 ) ) ;
#3904 = CARTESIAN_POINT ( 'NONE',  ( 79.48115437758207236, 54.55162964910791601, -15.95922698054103783 ) ) ;
#3905 = CARTESIAN_POINT ( 'NONE',  ( 75.20489394095216085, 55.31235798330321529, -16.61246018749456610 ) ) ;
#3906 = CARTESIAN_POINT ( 'NONE',  ( 172.6644317266046471, 263.3511091774913098, -15.41941820294944421 ) ) ;
#3907 = CARTESIAN_POINT ( 'NONE',  ( 92.94880205384217220, 212.2202760586659736, -5.415160957724236172E-17 ) ) ;
#3908 = CARTESIAN_POINT ( 'NONE',  ( 161.1150691641480535, 251.5875096731584506, -13.48836942566120101 ) ) ;
#3909 = CARTESIAN_POINT ( 'NONE',  ( 77.39025700982266187, 52.99708388390572367, -16.30678418076230329 ) ) ;
#3910 = CARTESIAN_POINT ( 'NONE',  ( 163.2179886388746013, 258.2814482063444075, 16.13245504067606007 ) ) ;
#3912 = CARTESIAN_POINT ( 'NONE',  ( 199.6892316128565028, 284.7751004525801477, 18.03507624704203494 ) ) ;
#3911 = CARTESIAN_POINT ( 'NONE',  ( 196.4994169513186364, 290.3000215130921902, 16.82935102260526961 ) ) ;
#3913 = CARTESIAN_POINT ( 'NONE',  ( 198.8570476668614049, 286.2164853282868080, -17.01721544293231858 ) ) ;
#3914 = CARTESIAN_POINT ( 'NONE',  ( 176.7122878561889365, 270.1790051031098869, -16.88799780853275578 ) ) ;
#3915 = CARTESIAN_POINT ( 'NONE',  ( 84.05461052688725943, 48.09452081518995925, -12.67959057290721603 ) ) ;
#3916 = CARTESIAN_POINT ( 'NONE',  ( 172.8210543149999978, 253.0650713199155177, -9.347212986753337560 ) ) ;
#3917 = VERTEX_POINT ( 'NONE', #4056 ) ;
#3918 = CARTESIAN_POINT ( 'NONE',  ( 15.78795072819010770, 21.06628583063840665, -9.188101187500006262 ) ) ;
#3919 = CARTESIAN_POINT ( 'NONE',  ( 72.92127039979698111, 225.1589784336661353, -6.496448406907676862E-16 ) ) ;
#3920 = CARTESIAN_POINT ( 'NONE',  ( 173.1254351131793499, 289.7002511501680715, -0.9735186482341396941 ) ) ;
#3921 = CARTESIAN_POINT ( 'NONE',  ( -32.85596848784926038, 94.38113866725780099, 10.43451941826970319 ) ) ;
#3922 = CARTESIAN_POINT ( 'NONE',  ( 191.2712410773971499, 288.8438557170641729, -16.41810066034774707 ) ) ;
#3923 = CARTESIAN_POINT ( 'NONE',  ( 86.32803123799460820, 47.24229282936711627, 10.81726845165080064 ) ) ;
#3924 = VECTOR ( 'NONE', #40267, 1000.000000000000000 ) ;
#3925 = CARTESIAN_POINT ( 'NONE',  ( 190.4756535880310651, 286.7931554109379135, 16.24365846582493589 ) ) ;
#3926 = LINE ( 'NONE', #42890, #56608 ) ;
#3927 = CARTESIAN_POINT ( 'NONE',  ( 126.5340026503663466, 243.8615022471902591, -10.00000000000009592 ) ) ;
#3928 = CARTESIAN_POINT ( 'NONE',  ( 205.2660270307054304, 275.1158074454486382, -13.97598661256119179 ) ) ;
#3929 = CARTESIAN_POINT ( 'NONE',  ( 74.72588123256606707, 53.65605547442924461, 16.08708352512548245 ) ) ;
#3930 = ORIENTED_EDGE ( 'NONE', *, *, #59767, .T. ) ;
#3931 = CARTESIAN_POINT ( 'NONE',  ( 169.4751163247794921, 248.6553299212260413, -1.920092548325727844 ) ) ;
#3932 = ORIENTED_EDGE ( 'NONE', *, *, #2588, .T. ) ;
#3933 = CARTESIAN_POINT ( 'NONE',  ( 163.1484656051875106, 248.0655637253488806, 9.714247672444804138 ) ) ;
#3934 = CARTESIAN_POINT ( 'NONE',  ( 185.1491161497484370, 292.9437783688060222, -11.97406807593424993 ) ) ;
#3935 = ORIENTED_EDGE ( 'NONE', *, *, #49800, .T. ) ;
#3936 = LINE ( 'NONE', #34820, #40234 ) ;
#3938 = EDGE_LOOP ( 'NONE', ( #39237, #94553, #45036, #75603 ) ) ;
#3937 = AXIS2_PLACEMENT_3D ( 'NONE', #78855, #34236, #40312 ) ;
#3939 = CARTESIAN_POINT ( 'NONE',  ( 190.5002508066484097, 290.6439963610214363, 14.51933001755366881 ) ) ;
#3940 = CARTESIAN_POINT ( 'NONE',  ( 158.7734878439422630, 255.6432474898095393, 16.04789767506137466 ) ) ;
#3941 = CARTESIAN_POINT ( 'NONE',  ( 151.5948730924283723, 249.1423013555410080, -4.594050593750043987 ) ) ;
#3942 = CARTESIAN_POINT ( 'NONE',  ( 153.9854481409094547, 263.9363755241191711, -17.91143416251955856 ) ) ;
#3943 = CARTESIAN_POINT ( 'NONE',  ( 192.8645107159946122, 296.1983763133186471, -11.90925672746789310 ) ) ;
#3944 = EDGE_CURVE ( 'NONE', #45874, #69600, #13297, .T. ) ;
#3945 = CARTESIAN_POINT ( 'NONE',  ( 32.45774345291223995, 27.24335787977765833, -9.188101187500008038 ) ) ;
#3946 = CARTESIAN_POINT ( 'NONE',  ( 74.55827288133576758, 60.13454576714501343, -15.53984938263620030 ) ) ;
#3947 = EDGE_CURVE ( 'NONE', #81604, #81790, #65843, .T. ) ;
#3948 = DIRECTION ( 'NONE',  ( -0.8660254037844387076, -0.4999999999999998890, -0.000000000000000000 ) ) ;
#3949 = CARTESIAN_POINT ( 'NONE',  ( -22.42236680055709641, 157.8615022471902591, 0.000000000000000000 ) ) ;
#3950 = VERTEX_POINT ( 'NONE', #83590 ) ;
#3951 = EDGE_LOOP ( 'NONE', ( #33969, #81656, #68752, #43358 ) ) ;
#3952 = CARTESIAN_POINT ( 'NONE',  ( 198.2391837281077756, 286.3575794386269422, 17.25947343406376078 ) ) ;
#3954 = CARTESIAN_POINT ( 'NONE',  ( 147.6512387128590262, 274.9075480792844246, -8.209968531507987777 ) ) ;
#3953 = CARTESIAN_POINT ( 'NONE',  ( 68.19833798964504012, 65.85959993625948528, 10.83357887337748338 ) ) ;
#3955 = CARTESIAN_POINT ( 'NONE',  ( 85.75965168945023720, 48.55180427257402442, -11.81072568050767657 ) ) ;
#3956 = CARTESIAN_POINT ( 'NONE',  ( 201.3693897336875693, 274.8123126220266386, -14.20577604999000698 ) ) ;
#3957 = FACE_OUTER_BOUND ( 'NONE', #84294, .T. ) ;
#3958 = CARTESIAN_POINT ( 'NONE',  ( 70.40802990919080173, 60.99707565408044729, 14.93107424293364360 ) ) ;
#3960 = ADVANCED_FACE ( 'NONE', ( #6050 ), #76936, .F. ) ;
#3959 = CARTESIAN_POINT ( 'NONE',  ( 207.9353140363083128, 270.4924667317612830, -5.099483218880686231 ) ) ;
#3961 = CARTESIAN_POINT ( 'NONE',  ( 169.8458979940169229, 267.4598849057458096, 17.28316019494766209 ) ) ;
#3962 = CARTESIAN_POINT ( 'NONE',  ( 156.6812872898450735, 261.2670451491295012, 0.000000000000000000 ) ) ;
#3963 = CARTESIAN_POINT ( 'NONE',  ( 100.4447270377624477, 237.9869531367911293, 4.594050593750046652 ) ) ;
#3964 = ORIENTED_EDGE ( 'NONE', *, *, #16416, .T. ) ;
#3965 = PLANE ( 'NONE',  #39871 ) ;
#3966 = CARTESIAN_POINT ( 'NONE',  ( 166.5240211178292782, 278.8801525804102539, -13.25163146027725425 ) ) ;
#3967 = EDGE_LOOP ( 'NONE', ( #15948, #54520, #89344, #74308 ) ) ;
#3968 = ORIENTED_EDGE ( 'NONE', *, *, #86274, .T. ) ;
#3969 = CARTESIAN_POINT ( 'NONE',  ( 87.12419840511867619, 46.02342392002756810, -8.190366543198424054 ) ) ;
#3970 = EDGE_CURVE ( 'NONE', #3742, #55035, #84588, .T. ) ;
#3971 = CARTESIAN_POINT ( 'NONE',  ( 177.2663517457237106, 293.3853303008062312, -2.825851527699106303 ) ) ;
#3972 = CARTESIAN_POINT ( 'NONE',  ( 83.30594405552706405, 41.61771957242412867, -2.403535763665288538 ) ) ;
#3973 = CARTESIAN_POINT ( 'NONE',  ( 161.9974668067621622, 270.5451527692481477, -16.99912248473486187 ) ) ;
#3974 = CARTESIAN_POINT ( 'NONE',  ( 206.9436690247072193, 270.9240130450578476, -4.881398567238052877 ) ) ;
#3975 = EDGE_CURVE ( 'NONE', #49412, #13462, #77466, .T. ) ;
#3976 = CARTESIAN_POINT ( 'NONE',  ( 87.34609280552280097, 230.4244531367911009, -4.594050593750046652 ) ) ;
#3977 = EDGE_LOOP ( 'NONE', ( #212, #97501, #20928, #87142 ) ) ;
#3978 = VERTEX_POINT ( 'NONE', #15628 ) ;
#3979 = DIRECTION ( 'NONE',  ( 0.001368469433193686413, -0.9999990636452668058, 0.000000000000000000 ) ) ;
#3980 = ORIENTED_EDGE ( 'NONE', *, *, #55904, .F. ) ;
#3981 = DIRECTION ( 'NONE',  ( -0.2925570654631255985, 0.000000000000000000, 0.9562480658530004840 ) ) ;
#3982 = CARTESIAN_POINT ( 'NONE',  ( 153.9627345078393716, 265.2571514742093655, 16.78486123779136463 ) ) ;
#3983 = CARTESIAN_POINT ( 'NONE',  ( 68.68961001230228192, 69.20649816010151767, -5.408517505406226888 ) ) ;
#3985 = CARTESIAN_POINT ( 'NONE',  ( 69.67644213241599971, 62.68400490086408183, -13.31948877326700931 ) ) ;
#3984 = CARTESIAN_POINT ( 'NONE',  ( 122.2847184155099995, 253.6589784336661069, -6.496448406907675876E-16 ) ) ;
#3986 = CARTESIAN_POINT ( 'NONE',  ( -8.728340106763567974, 165.7677522451418781, 10.00000000000009592 ) ) ;
#3987 = PLANE ( 'NONE',  #38159 ) ;
#3988 = VERTEX_POINT ( 'NONE', #99759 ) ;
#3989 = CARTESIAN_POINT ( 'NONE',  ( 205.0302908362115772, 275.5241145114948154, 13.44798751587103425 ) ) ;
#3990 = CARTESIAN_POINT ( 'NONE',  ( 81.51672219897599803, 48.01526152666208702, 13.05833413880630722 ) ) ;
#3991 = EDGE_CURVE ( 'NONE', #2782, #41802, #80977, .T. ) ;
#3992 = CARTESIAN_POINT ( 'NONE',  ( 206.7680519836501958, 272.5142239127119979, -10.57935479673322021 ) ) ;
#3993 = CARTESIAN_POINT ( 'NONE',  ( 25.48331929688331243, 38.21091486745862653, 7.012934429366973338E-14 ) ) ;
#3994 = CARTESIAN_POINT ( 'NONE',  ( 168.5554356917367045, 285.0925123692317129, 10.08420881268239455 ) ) ;
#3995 = DIRECTION ( 'NONE',  ( -0.6384778167143279060, 0.7696402260561132636, 0.000000000000000000 ) ) ;
#3996 = VECTOR ( 'NONE', #17041, 1000.000000000000000 ) ;
#3997 = CARTESIAN_POINT ( 'NONE',  ( 89.54518929453067244, 234.0530062829863027, -4.648177544792955347E-16 ) ) ;
#3998 = FACE_OUTER_BOUND ( 'NONE', #36994, .T. ) ;
#3999 = EDGE_CURVE ( 'NONE', #5430, #2810, #90662, .T. ) ;
#4000 = CARTESIAN_POINT ( 'NONE',  ( 80.44641172169940546, 52.15703007935309188, 15.27578981345033959 ) ) ;
#4001 = CARTESIAN_POINT ( 'NONE',  ( 69.44037796687385367, 70.26988621369126520, -3.529725965421429468 ) ) ;
#4002 = CARTESIAN_POINT ( 'NONE',  ( 167.6224482745345767, 249.9459711549417591, 7.039320684982598664 ) ) ;
#4003 = CARTESIAN_POINT ( 'NONE',  ( 83.41128051646016672, 51.86661034151835281, 14.99497567496408479 ) ) ;
#4004 = CARTESIAN_POINT ( 'NONE',  ( 208.3829315663354862, 269.7171704273955015, -1.768817828503133072 ) ) ;
#4005 = CARTESIAN_POINT ( 'NONE',  ( 202.7005662011214042, 279.5593159471158629, -16.25860390100328345 ) ) ;
#4006 = VECTOR ( 'NONE', #42693, 1000.000000000000000 ) ;
#4007 = EDGE_CURVE ( 'NONE', #52344, #77213, #15126, .T. ) ;
#4008 = ADVANCED_FACE ( 'NONE', ( #14653 ), #76462, .T. ) ;
#4009 = CARTESIAN_POINT ( 'NONE',  ( 182.4036492637225138, 264.0684302237640395, 14.07752408005863920 ) ) ;
#4010 = ADVANCED_FACE ( 'NONE', ( #38431 ), #68837, .T. ) ;
#4011 = CARTESIAN_POINT ( 'NONE',  ( 79.17323837735700920, 206.5177522451417929, 5.000000000000051514 ) ) ;
#4012 = ADVANCED_FACE ( 'NONE', ( #54121 ), #76811, .T. ) ;
#4013 = CARTESIAN_POINT ( 'NONE',  ( 28.14208253200458287, 39.18080186712595037, 3.090169943749475401 ) ) ;
#4014 = LINE ( 'NONE', #33416, #90354 ) ;
#4015 = FACE_OUTER_BOUND ( 'NONE', #9926, .T. ) ;
#4016 = CARTESIAN_POINT ( 'NONE',  ( 82.14625348271364658, 43.20029849263703170, -8.033064318764047584 ) ) ;
#4017 =( BOUNDED_CURVE ( )  B_SPLINE_CURVE ( 2, ( #2561, #56737, #80086, #95798, #65822, #49633, #58228, #96787, #11658, #82086, #87719, #25861, #26848 ),
 .UNSPECIFIED., .F., .T. ) 
 B_SPLINE_CURVE_WITH_KNOTS ( ( 3, 2, 2, 2, 2, 2, 3 ),
 ( 0.7625000000000000666, 0.7650000000000000133, 0.7700000000000000178, 0.7750000000000000222, 0.7800000000000000266, 0.7850000000000000311, 0.7875000000000000888 ),
 .UNSPECIFIED. ) 
 CURVE ( )  GEOMETRIC_REPRESENTATION_ITEM ( )  RATIONAL_B_SPLINE_CURVE ( ( 0.9755282581475767101, 0.9755282581475772652, 1.000000000000000000, 0.9510565162951535312, 1.000000000000000000, 0.9510565162951535312, 1.000000000000000000, 0.9510565162951535312, 1.000000000000000000, 0.9510565162951535312, 1.000000000000000000, 0.9755282581475761550, 0.9755282581475767101 ) ) 
 REPRESENTATION_ITEM ( '' )  );
#4018 = CARTESIAN_POINT ( 'NONE',  ( 18.65997361151702449, 172.3923013555409796, 4.594050593750050204 ) ) ;
#4019 = CYLINDRICAL_SURFACE ( 'NONE', #45230, 17.82106496071139645 ) ;
#4020 = VERTEX_POINT ( 'NONE', #62729 ) ;
#4021 = CARTESIAN_POINT ( 'NONE',  ( 86.79998443407272646, 45.86195168027221314, 8.882059948630848467 ) ) ;
#4022 = CARTESIAN_POINT ( 'NONE',  ( 183.8274263638271577, 281.3324037098167310, 17.41033114534894111 ) ) ;
#4023 = CARTESIAN_POINT ( 'NONE',  ( 82.25567614043384879, 41.32243640453275901, 5.438163968954911276 ) ) ;
#4024 = CARTESIAN_POINT ( 'NONE',  ( 42.77328167419872074, 189.3768266524160424, 9.188101187500096856 ) ) ;
#4025 = CARTESIAN_POINT ( 'NONE',  ( 200.6449165581618956, 283.1198055712825976, 18.35107460171532523 ) ) ;
#4026 = CARTESIAN_POINT ( 'NONE',  ( 190.6954410837624607, 300.3528026016029457, -5.728531842148099962 ) ) ;
#4027 = CARTESIAN_POINT ( 'NONE',  ( 38.71056063283548809, 34.30066082961425167, -10.00000000000000533 ) ) ;
#4028 = CARTESIAN_POINT ( 'NONE',  ( 178.5837403247565192, 291.6510475641956646, 6.049951385461257658 ) ) ;
#4029 = CARTESIAN_POINT ( 'NONE',  ( 191.7934382699952494, 298.4510156884799699, -8.680100145728863126 ) ) ;
#4030 = CARTESIAN_POINT ( 'NONE',  ( 178.9534601940523260, 278.3064132268250432, -16.87083665727369919 ) ) ;
#4031 = CARTESIAN_POINT ( 'NONE',  ( -19.65312891409030271, 93.06504152958497400, 10.00000000000000888 ) ) ;
#4032 = CARTESIAN_POINT ( 'NONE',  ( 118.9147354758962081, 227.9155109091896065, 2.679491924311254714 ) ) ;
#4033 = CARTESIAN_POINT ( 'NONE',  ( 49.60098510475376088, 81.22027839155747131, -10.00000000000000000 ) ) ;
#4034 = CARTESIAN_POINT ( 'NONE',  ( 192.3926678149021825, 295.4131196713046847, -13.42882169270698256 ) ) ;
#4035 = CARTESIAN_POINT ( 'NONE',  ( 79.84079962965540744, 210.2365022471902023, -10.00000000000009059 ) ) ;
#4036 = LINE ( 'NONE', #42518, #63572 ) ;
#4037 = DIRECTION ( 'NONE',  ( -0.8660254037844387076, -0.4999999999999998890, -0.000000000000000000 ) ) ;
#4038 = ORIENTED_EDGE ( 'NONE', *, *, #97659, .F. ) ;
#4039 = CARTESIAN_POINT ( 'NONE',  ( 38.09089796528284211, 201.9869531367911293, 4.594050593750046652 ) ) ;
#4040 = ORIENTED_EDGE ( 'NONE', *, *, #49837, .T. ) ;
#4041 = CARTESIAN_POINT ( 'NONE',  ( 162.5350674691047459, 263.2285193240729768, 17.40336567648585131 ) ) ;
#4042 = CARTESIAN_POINT ( 'NONE',  ( 147.4317198359019301, 275.2877659273946733, 3.797273160043843188 ) ) ;
#4043 = CARTESIAN_POINT ( 'NONE',  ( 67.26837558547590845, 67.21133208665345649, -8.574135192023929264 ) ) ;
#4044 = ORIENTED_EDGE ( 'NONE', *, *, #30539, .T. ) ;
#4045 = LINE ( 'NONE', #25870, #94487 ) ;
#4046 = CARTESIAN_POINT ( 'NONE',  ( 206.8968397926183229, 272.2911568841838061, 7.145103750817420440 ) ) ;
#4047 = LINE ( 'NONE', #87232, #75251 ) ;
#4048 = CARTESIAN_POINT ( 'NONE',  ( 31.76492312988469280, 26.84335787977765264, 9.188101187500006262 ) ) ;
#4049 = CARTESIAN_POINT ( 'NONE',  ( 186.1775172130778344, 263.6544597137042274, 10.94427764037104822 ) ) ;
#4050 = CARTESIAN_POINT ( 'NONE',  ( 74.14312167556930433, 66.30466486950707861, 1.224646799147354045E-15 ) ) ;
#4051 = CARTESIAN_POINT ( 'NONE',  ( 174.8699766508015330, 257.3397558657187574, 11.46886032790315646 ) ) ;
#4052 = ORIENTED_EDGE ( 'NONE', *, *, #24922, .F. ) ;
#4053 = CARTESIAN_POINT ( 'NONE',  ( 18.06126741312425921, 22.37878583063840310, 9.188101187500006262 ) ) ;
#4054 = CARTESIAN_POINT ( 'NONE',  ( 75.93655505379200576, 59.57132730434130963, 15.86584733416168014 ) ) ;
#4055 = CARTESIAN_POINT ( 'NONE',  ( 174.7032039963333716, 255.1089386847479830, 8.234442070018992865 ) ) ;
#4056 = CARTESIAN_POINT ( 'NONE',  ( 85.85265132163429769, 47.44586991713102009, 10.77177032529229450 ) ) ;
#4057 = EDGE_LOOP ( 'NONE', ( #75868, #62612, #50767, #29149 ) ) ;
#4058 = DIRECTION ( 'NONE',  ( 0.000000000000000000, 0.000000000000000000, -1.000000000000000000 ) ) ;
#4059 = CARTESIAN_POINT ( 'NONE',  ( 150.8888667059421209, 269.2998118992572927, 15.79021133717968617 ) ) ;
#4060 = LINE ( 'NONE', #19782, #90121 ) ;
#4061 = AXIS2_PLACEMENT_3D ( 'NONE', #25282, #39460, #38476 ) ;
#4062 = ORIENTED_EDGE ( 'NONE', *, *, #77189, .T. ) ;
#4063 = ORIENTED_EDGE ( 'NONE', *, *, #44174, .T. ) ;
#4065 = CARTESIAN_POINT ( 'NONE',  ( -14.83262083840142154, 124.7156766241961208, -37.49999999999995737 ) ) ;
#4064 = CARTESIAN_POINT ( 'NONE',  ( 207.6357208050208101, 271.0113774299547913, -6.790259683043212036 ) ) ;
#4066 = LINE ( 'NONE', #89237, #62676 ) ;
#4067 = ORIENTED_EDGE ( 'NONE', *, *, #53027, .F. ) ;
#4068 = CARTESIAN_POINT ( 'NONE',  ( 66.35522338032015455, 68.72304060489808819, -2.132035597865990173 ) ) ;
#4069 = FACE_OUTER_BOUND ( 'NONE', #8900, .T. ) ;
#4070 = CARTESIAN_POINT ( 'NONE',  ( 81.37739665788856769, 55.81704345181816507, 16.38624498997419110 ) ) ;
#4071 = CARTESIAN_POINT ( 'NONE',  ( 79.14312167556931854, 57.64441083166269664, 0.000000000000000000 ) ) ;
#4072 = CARTESIAN_POINT ( 'NONE',  ( 198.1847055346428590, 286.9842163890704683, 16.95145238430053070 ) ) ;
#4075 = ADVANCED_FACE ( 'NONE', ( #24250 ), #92238, .T. ) ;
#4074 = CARTESIAN_POINT ( 'NONE',  ( 107.0210206738092609, 244.8464784336661353, 1.353441290958777525E-15 ) ) ;
#4073 = AXIS2_PLACEMENT_3D ( 'NONE', #14389, #85321, #99499 ) ;
#4076 = CARTESIAN_POINT ( 'NONE',  ( 27.07533481826667554, 197.9860189848785694, -2.679491924311252493 ) ) ;
#4077 = CARTESIAN_POINT ( 'NONE',  ( 207.5583741822599393, 271.1453457103705205, 3.140867606700001424 ) ) ;
#4078 = ORIENTED_EDGE ( 'NONE', *, *, #41371, .T. ) ;
#4079 = CARTESIAN_POINT ( 'NONE',  ( 33.64972468124413751, 31.37878583063843152, 9.188101187500006262 ) ) ;
#4080 = CARTESIAN_POINT ( 'NONE',  ( 160.0105735053945182, 253.5005522708592594, 16.10371386499367929 ) ) ;
#4081 = CARTESIAN_POINT ( 'NONE',  ( 204.6785851723931557, 274.1332865905380913, -12.34137688749581407 ) ) ;
#4082 = CARTESIAN_POINT ( 'NONE',  ( 81.01380268399661588, 208.3923013555409796, 4.594050593750050204 ) ) ;
#4083 = EDGE_CURVE ( 'NONE', #72864, #14672, #77333, .T. ) ;
#4084 = CARTESIAN_POINT ( 'NONE',  ( 4.102725850843912170, 28.55253618238880620, -10.00000000000000000 ) ) ;
#4085 = CARTESIAN_POINT ( 'NONE',  ( 151.1926529451685326, 268.7736386982768408, 14.30343427984827365 ) ) ;
#4086 = CARTESIAN_POINT ( 'NONE',  ( 154.9683083969241011, 262.2340116239618055, 18.33261662430134109 ) ) ;
#4087 = CARTESIAN_POINT ( 'NONE',  ( 175.4922833695144959, 278.4365452609995373, 15.47038347327790220 ) ) ;
#4088 = ADVANCED_FACE ( 'NONE', ( #41813 ), #89005, .T. ) ;
#4089 = VERTEX_POINT ( 'NONE', #49422 ) ;
#4090 = DIRECTION ( 'NONE',  ( -0.6118251767726360368, -0.7909930170786165782, 0.000000000000000000 ) ) ;
#4091 = CARTESIAN_POINT ( 'NONE',  ( 203.2187760522547819, 278.6617501559703101, -15.08675642319914978 ) ) ;
#4092 = VERTEX_POINT ( 'NONE', #3352 ) ;
#4093 = CARTESIAN_POINT ( 'NONE',  ( 148.4286446168608791, 273.5610415554491510, 8.864897967665541501 ) ) ;
#4094 = CARTESIAN_POINT ( 'NONE',  ( 174.2665823609021913, 277.1739101417822440, -15.63194565161007610 ) ) ;
#4095 = CARTESIAN_POINT ( 'NONE',  ( 207.7666684749232786, 270.7845694125510931, -6.630926507062123498 ) ) ;
#4096 = DIRECTION ( 'NONE',  ( 0.000000000000000000, 1.000000000000000000, 0.000000000000000000 ) ) ;
#4097 = CARTESIAN_POINT ( 'NONE',  ( 176.6128493493775693, 293.2828690831819927, -1.507349561191283493 ) ) ;
#4098 = LINE ( 'NONE', #81153, #83476 ) ;
#4099 = AXIS2_PLACEMENT_3D ( 'NONE', #57184, #65298, #72931 ) ;
#4100 = CARTESIAN_POINT ( 'NONE',  ( 165.0308887387863876, 244.8051112166122891, 1.948365933089477808 ) ) ;
#4101 = LINE ( 'NONE', #42585, #97868 ) ;
#4102 = CARTESIAN_POINT ( 'NONE',  ( 153.8480465357228013, 265.0660884932569843, -16.61306390558784685 ) ) ;
#4103 = CARTESIAN_POINT ( 'NONE',  ( 163.7595992360150490, 247.0070492265414828, -6.976205010573520049 ) ) ;
#4104 = CARTESIAN_POINT ( 'NONE',  ( 132.9753269110629503, 238.3923013555409796, 4.594050593750050204 ) ) ;
#4105 = ORIENTED_EDGE ( 'NONE', *, *, #47542, .F. ) ;
#4106 = CARTESIAN_POINT ( 'NONE',  ( 86.95125388468488836, 44.27950943365674163, -4.934478059872851041 ) ) ;
#4107 = LINE ( 'NONE', #11242, #86991 ) ;
#4108 = CYLINDRICAL_SURFACE ( 'NONE', #34382, 70.00000000000002842 ) ;
#4109 = CARTESIAN_POINT ( 'NONE',  ( 204.3276935076901850, 276.7410487817560920, 13.46217427333259309 ) ) ;
#4110 = CARTESIAN_POINT ( 'NONE',  ( 75.31417462687399222, 64.08252782891483434, 14.41125185447981139 ) ) ;
#4111 = LINE ( 'NONE', #34517, #59913 ) ;
#4112 = VERTEX_POINT ( 'NONE', #26629 ) ;
#4113 = DIRECTION ( 'NONE',  ( 0.000000000000000000, 0.000000000000000000, 1.000000000000000000 ) ) ;
#4114 = EDGE_CURVE ( 'NONE', #27521, #91230, #81373, .T. ) ;
#4115 = CARTESIAN_POINT ( 'NONE',  ( 167.5938299737844943, 249.2181452600659952, -5.555151102822903475 ) ) ;
#4116 = CARTESIAN_POINT ( 'NONE',  ( 206.7182525013508041, 272.6004791462452204, -10.42767927275168205 ) ) ;
#4117 = CARTESIAN_POINT ( 'NONE',  ( 143.4758849319492526, 244.4548013555409796, -4.594050593750042211 ) ) ;
#4118 = CARTESIAN_POINT ( 'NONE',  ( 196.1506231955608257, 263.5440226259423753, 0.8792856859939570668 ) ) ;
#4119 = CARTESIAN_POINT ( 'NONE',  ( 190.2510882691990730, 301.1224442529128851, -5.480893437181090455 ) ) ;
#4120 = EDGE_CURVE ( 'NONE', #71865, #16478, #89479, .T. ) ;
#4121 = CARTESIAN_POINT ( 'NONE',  ( 68.78984366447195953, 69.70809013107415808, 4.131647041545672749 ) ) ;
#4122 = CARTESIAN_POINT ( 'NONE',  ( 179.0678258594554677, 253.8070992628930753, 2.501565655556938772 ) ) ;
#4123 = EDGE_CURVE ( 'NONE', #78500, #61239, #2342, .T. ) ;
#4124 = CARTESIAN_POINT ( 'NONE',  ( 14.28567607145357421, 31.18080186712592550, 3.090169943749475401 ) ) ;
#4125 = CARTESIAN_POINT ( 'NONE',  ( 172.7003033961413223, 290.5754134926764891, -4.014267798627228601 ) ) ;
#4126 = LINE ( 'NONE', #58320, #14331 ) ;
#4127 = CARTESIAN_POINT ( 'NONE',  ( 169.4354079512919213, 285.1812872968449710, -7.984367431210777966 ) ) ;
#4128 = VECTOR ( 'NONE', #100066, 999.9999999999998863 ) ;
#4129 = DIRECTION ( 'NONE',  ( 0.4999999999999992784, -0.8660254037844390407, 0.000000000000000000 ) ) ;
#4130 = CARTESIAN_POINT ( 'NONE',  ( 193.5950831135630494, 288.5422439134695765, 16.06279111291604877 ) ) ;
#4131 = CARTESIAN_POINT ( 'NONE',  ( 130.1965684169901181, 252.6427522451419634, -10.00000000000009415 ) ) ;
#4132 = CARTESIAN_POINT ( 'NONE',  ( 175.9490061063565349, 285.5465045145652425, -11.89368724642156572 ) ) ;
#4133 = EDGE_LOOP ( 'NONE', ( #89229, #65845, #74782, #84473 ) ) ;
#4134 = ADVANCED_FACE ( 'NONE', ( #7270 ), #75697, .T. ) ;
#4135 = CARTESIAN_POINT ( 'NONE',  ( 157.8562613713738472, 257.2319303423452652, 17.81420683562559404 ) ) ;
#4136 = CARTESIAN_POINT ( 'NONE',  ( 189.8147415777049218, 301.8782188922952514, -0.5019643756309712934 ) ) ;
#4137 = CARTESIAN_POINT ( 'NONE',  ( -12.32793173735119652, 169.8149278399161233, 9.188101187500093303 ) ) ;
#4138 = CARTESIAN_POINT ( 'NONE',  ( 38.93012039702277605, 193.2833772461660544, -9.188101187500095079 ) ) ;
#4139 = CARTESIAN_POINT ( 'NONE',  ( 178.6079043543401781, 259.1547383593973564, -10.33114907980992925 ) ) ;
#4140 = CARTESIAN_POINT ( 'NONE',  ( 22.16161828121410338, 13.76426979415089491, 3.090169943749476733 ) ) ;
#4141 = LINE ( 'NONE', #79698, #48062 ) ;
#4142 = CARTESIAN_POINT ( 'NONE',  ( 205.4103625296683617, 274.8658110279089897, -13.38953657917851814 ) ) ;
#4143 = CARTESIAN_POINT ( 'NONE',  ( 192.4574196167241382, 292.2611441422025109, -14.34643084275922043 ) ) ;
#4144 = CARTESIAN_POINT ( 'NONE',  ( 146.8358616138309571, 276.3198226421291679, 4.054088818585255716 ) ) ;
#4145 = CARTESIAN_POINT ( 'NONE',  ( 73.80791270665581294, 55.11249867311061479, -16.60035380508545089 ) ) ;
#4146 = CARTESIAN_POINT ( 'NONE',  ( 170.5175754660751011, 258.1364974620091175, 13.85570805355783897 ) ) ;
#4147 = CARTESIAN_POINT ( 'NONE',  ( 76.93253562831463910, 60.43031639469479188, 16.23105599402710197 ) ) ;
#4148 = CARTESIAN_POINT ( 'NONE',  ( 204.7242223814549504, 276.0542406257275161, -13.93608974681376189 ) ) ;
#4149 = CARTESIAN_POINT ( 'NONE',  ( 193.1030321335636586, 294.1827325794992021, -14.54662778306917481 ) ) ;
#4150 = CARTESIAN_POINT ( 'NONE',  ( 39.06543686813810012, 183.3615022471902023, 5.000000000000051514 ) ) ;
#4151 = LINE ( 'NONE', #80716, #24806 ) ;
#4152 = DIRECTION ( 'NONE',  ( 0.000000000000000000, 0.000000000000000000, -1.000000000000000000 ) ) ;
#4153 = CARTESIAN_POINT ( 'NONE',  ( 0.9332558059805314832, 171.3458772461660544, 9.188101187500095079 ) ) ;
#4154 = CARTESIAN_POINT ( 'NONE',  ( 168.2351335216934558, 286.3770512125953474, 4.694921679824968663 ) ) ;
#4156 = EDGE_CURVE ( 'NONE', #61069, #28867, #25290, .T. ) ;
#4155 = CARTESIAN_POINT ( 'NONE',  ( 80.63243328097439644, 57.57134443808153890, -16.24110709809310293 ) ) ;
#4157 = CARTESIAN_POINT ( 'NONE',  ( 192.8323852661406761, 296.6515067047851062, 11.86505947732313615 ) ) ;
#4158 = CARTESIAN_POINT ( 'NONE',  ( 36.84800447571193160, 26.98920272979929180, 7.433330006724137462 ) ) ;
#4159 = CARTESIAN_POINT ( 'NONE',  ( -27.42236680055714260, 166.5217562850347406, 1.224646799147364892E-15 ) ) ;
#4160 = CARTESIAN_POINT ( 'NONE',  ( 179.6127186018034649, 277.1388513108101961, 16.32392918091530376 ) ) ;
#4161 = CARTESIAN_POINT ( 'NONE',  ( 193.7114073116034945, 295.1289958610702797, 14.86160832869823345 ) ) ;
#4162 = DIRECTION ( 'NONE',  ( 0.3956464567955563782, -0.9184028970038813355, 0.000000000000000000 ) ) ;
#4163 = CARTESIAN_POINT ( 'NONE',  ( 179.7546709676660726, 262.8207191251350423, -12.87104168322583497 ) ) ;
#4164 = CARTESIAN_POINT ( 'NONE',  ( 8.259543914800127951, 22.95586893147753571, 7.433330006724141015 ) ) ;
#4165 = CARTESIAN_POINT ( 'NONE',  ( 115.6419768118483091, 249.1199935810940929, 2.679491924311251605 ) ) ;
#4166 = CARTESIAN_POINT ( 'NONE',  ( 16.65397613197454518, 21.56628583063840310, 9.188101187500006262 ) ) ;
#4167 = DIRECTION ( 'NONE',  ( -0.9404163354663408469, -0.3400251696390411693, 0.000000000000000000 ) ) ;
#4168 = CARTESIAN_POINT ( 'NONE',  ( 154.9455285025717615, 262.2734675583710100, 18.28470720339922551 ) ) ;
#4169 = ORIENTED_EDGE ( 'NONE', *, *, #82733, .T. ) ;
#4170 = CARTESIAN_POINT ( 'NONE',  ( 18.55511606660780899, 34.21091486745861232, -1.111400068045478839E-16 ) ) ;
#4171 = CARTESIAN_POINT ( 'NONE',  ( 74.93188263267299476, 53.45048654396977383, -16.53684691294480302 ) ) ;
#4172 = CARTESIAN_POINT ( 'NONE',  ( 159.5221561062548972, 254.3465160214695118, -16.91023001054109542 ) ) ;
#4173 = EDGE_LOOP ( 'NONE', ( #29992, #27784, #33502, #3705 ) ) ;
#4174 = DIRECTION ( 'NONE',  ( 0.4999999999999992784, -0.8660254037844390407, 0.000000000000000000 ) ) ;
#4175 = CARTESIAN_POINT ( 'NONE',  ( 164.2723164851102808, 246.1189969011916503, -1.993789335506892302 ) ) ;
#4176 = VECTOR ( 'NONE', #60511, 1000.000000000000114 ) ;
#4177 = CARTESIAN_POINT ( 'NONE',  ( 66.34264438788950713, 68.59982612598324181, 4.834438131297811303 ) ) ;
#4178 = CARTESIAN_POINT ( 'NONE',  ( 87.53878856671160236, 45.51437473004847334, 6.953484175700196168 ) ) ;
#4179 = ORIENTED_EDGE ( 'NONE', *, *, #47907, .F. ) ;
#4180 = EDGE_LOOP ( 'NONE', ( #9809, #20008, #50289, #27909 ) ) ;
#4182 = CARTESIAN_POINT ( 'NONE',  ( 163.9149533033796047, 246.7379680887036670, 7.273005089308705706 ) ) ;
#4181 = CARTESIAN_POINT ( 'NONE',  ( -26.08262083840154233, 139.2012482093457493, 37.49999999999996447 ) ) ;
#4183 = CARTESIAN_POINT ( 'NONE',  ( 192.1149248854976861, 297.8941845364767005, 12.26771790733441314 ) ) ;
#4184 = ORIENTED_EDGE ( 'NONE', *, *, #66078, .F. ) ;
#4185 = CARTESIAN_POINT ( 'NONE',  ( 193.8212943487757514, 292.9386659295947197, 15.46346239154970625 ) ) ;
#4186 = CARTESIAN_POINT ( 'NONE',  ( 167.0957737472305666, 246.8272050136007749, 1.963998143010642128 ) ) ;
#4187 = ORIENTED_EDGE ( 'NONE', *, *, #45619, .F. ) ;
#4188 = CYLINDRICAL_SURFACE ( 'NONE', #60388, 17.82106496071139645 ) ;
#4189 = CARTESIAN_POINT ( 'NONE',  ( 77.00817486789581778, 225.2677522451419350, -5.000000000000047962 ) ) ;
#4190 = CARTESIAN_POINT ( 'NONE',  ( 149.5796913320911870, 271.5673701627850960, -12.80793412251569841 ) ) ;
#4191 = CARTESIAN_POINT ( 'NONE',  ( -20.65464553008482795, 23.07220643578491348, -10.00000000000000000 ) ) ;
#4192 = ORIENTED_EDGE ( 'NONE', *, *, #38570, .F. ) ;
#4193 = CARTESIAN_POINT ( 'NONE',  ( 203.0765383200355245, 267.8773628719704334, 2.545970250563589943 ) ) ;
#4194 = CARTESIAN_POINT ( 'NONE',  ( 166.1815834339950015, 273.8822376155316078, -15.37734293452891876 ) ) ;
#4195 = AXIS2_PLACEMENT_3D ( 'NONE', #61422, #43731, #14827 ) ;
#4196 = DIRECTION ( 'NONE',  ( -0.8660254037844387076, -0.4999999999999998890, -0.000000000000000000 ) ) ;
#4197 = VERTEX_POINT ( 'NONE', #74748 ) ;
#4198 = CARTESIAN_POINT ( 'NONE',  ( 148.9266665119372703, 272.6984423298952152, 12.06339424062075061 ) ) ;
#4199 = CARTESIAN_POINT ( 'NONE',  ( 169.2748951493203151, 261.4352243401077658, -16.54128482989432314 ) ) ;
#4200 = ORIENTED_EDGE ( 'NONE', *, *, #25640, .T. ) ;
#4201 = EDGE_CURVE ( 'NONE', #45691, #25393, #5328, .T. ) ;
#4202 = CARTESIAN_POINT ( 'NONE',  ( 159.2204200025353487, 268.0642290086452704, -16.29750726868432409 ) ) ;
#4203 = AXIS2_PLACEMENT_3D ( 'NONE', #59932, #69539, #30546 ) ;
#4204 = ORIENTED_EDGE ( 'NONE', *, *, #68344, .F. ) ;
#4205 = EDGE_CURVE ( 'NONE', #55813, #64236, #62786, .T. ) ;
#4206 = DIRECTION ( 'NONE',  ( 0.000000000000000000, 0.000000000000000000, 1.000000000000000000 ) ) ;
#4207 = ORIENTED_EDGE ( 'NONE', *, *, #74300, .T. ) ;
#4208 = FACE_OUTER_BOUND ( 'NONE', #14757, .T. ) ;
#4209 = CARTESIAN_POINT ( 'NONE',  ( 194.0244658732981122, 294.5867625264709204, 13.70898399957177283 ) ) ;
#4210 = CARTESIAN_POINT ( 'NONE',  ( 82.40357584069326435, 53.81685777417739303, 15.85384499771503464 ) ) ;
#4211 = CARTESIAN_POINT ( 'NONE',  ( 135.1220879045620507, 255.4865022471903160, 10.00000000000009415 ) ) ;
#4212 = CARTESIAN_POINT ( 'NONE',  ( 193.7483724793648037, 294.3783421859641862, 13.84800572152474807 ) ) ;
#4213 = CARTESIAN_POINT ( 'NONE',  ( 162.0489775477180387, 249.9699329032011406, -13.37069569336162012 ) ) ;
#4214 = CARTESIAN_POINT ( 'NONE',  ( 166.2786698706664765, 279.3007919285489606, -14.16120680810289301 ) ) ;
#4215 = CARTESIAN_POINT ( 'NONE',  ( 197.4070200448009587, 288.7280068420738530, -18.25155942860170910 ) ) ;
#4216 = ORIENTED_EDGE ( 'NONE', *, *, #49738, .T. ) ;
#4217 = CARTESIAN_POINT ( 'NONE',  ( -49.78034631855286563, 29.87998972566340683, -10.00000000000000000 ) ) ;
#4219 = CARTESIAN_POINT ( 'NONE',  ( 205.7867067512454184, 274.2139637150027056, 10.62737868262404106 ) ) ;
#4218 = CARTESIAN_POINT ( 'NONE',  ( 77.34929714582419535, 49.75066375701363341, -14.99659801915009893 ) ) ;
#4220 = CARTESIAN_POINT ( 'NONE',  ( 160.0105735053945182, 253.5005522708592594, 16.10371386499367929 ) ) ;
#4221 = VERTEX_POINT ( 'NONE', #32091 ) ;
#4222 = CARTESIAN_POINT ( 'NONE',  ( 185.4126573565306444, 275.9338992703376903, 16.44638672139682711 ) ) ;
#4223 = DIRECTION ( 'NONE',  ( 0.3301025504114333264, 0.9439450758449176027, 0.000000000000000000 ) ) ;
#4224 = CARTESIAN_POINT ( 'NONE',  ( 41.98060738119045965, 32.43677371833805978, -10.00000000000000355 ) ) ;
#4225 = CARTESIAN_POINT ( 'NONE',  ( -71.36129514276957764, 45.88172302328153052, 177.5919119679930134 ) ) ;
#4226 = CARTESIAN_POINT ( 'NONE',  ( 199.2788941474133253, 285.4858257909769463, -18.43300471952202813 ) ) ;
#4227 = CARTESIAN_POINT ( 'NONE',  ( 148.3870282890677288, 273.6331231496113787, -8.845975465985159047 ) ) ;
#4228 = VERTEX_POINT ( 'NONE', #47787 ) ;
#4229 = CARTESIAN_POINT ( 'NONE',  ( 49.32130651720206771, 81.12656353050643077, -10.00000000000000000 ) ) ;
#4230 = CARTESIAN_POINT ( 'NONE',  ( 205.6418006816680304, 274.0625766808819890, 10.49905374274900893 ) ) ;
#4231 = EDGE_CURVE ( 'NONE', #37455, #58141, #39673, .T. ) ;
#4232 = CARTESIAN_POINT ( 'NONE',  ( 134.6192181478005523, 236.9824982072973967, 3.021315404115420679E-15 ) ) ;
#4233 = CARTESIAN_POINT ( 'NONE',  ( 155.3480338107684986, 262.6013740870448601, 17.23779241981489463 ) ) ;
#4234 = CARTESIAN_POINT ( 'NONE',  ( 39.26390101962412871, 180.1427522451417644, 1.119607411625061291E-15 ) ) ;
#4235 = CARTESIAN_POINT ( 'NONE',  ( 98.52331994705697582, 233.8149278399160949, -9.188101187500095079 ) ) ;
#4236 = CARTESIAN_POINT ( 'NONE',  ( 183.8352931141344300, 296.4858501351076825, -2.730139885982957093 ) ) ;
#4237 = CARTESIAN_POINT ( 'NONE',  ( 167.2877005011474694, 283.1435899044605549, -11.30941513220499850 ) ) ;
#4238 = CARTESIAN_POINT ( 'NONE',  ( 23.08833070876649529, 13.73415679381821874, 1.333680081654574804E-15 ) ) ;
#4239 = CARTESIAN_POINT ( 'NONE',  ( 163.2189713653645242, 247.9434441664957944, 10.97120828841990914 ) ) ;
#4240 = CARTESIAN_POINT ( 'NONE',  ( 23.01690360248371903, 184.0958772461660544, -9.188101187500095079 ) ) ;
#4241 = CIRCLE ( 'NONE', #5903, 17.82106496071138935 ) ;
#4242 = CARTESIAN_POINT ( 'NONE',  ( 173.9076247008792393, 277.9417859016587045, -16.84130823774900776 ) ) ;
#4243 = ORIENTED_EDGE ( 'NONE', *, *, #90245, .T. ) ;
#4244 = AXIS2_PLACEMENT_3D ( 'NONE', #91472, #22034, #14922 ) ;
#4245 = ORIENTED_EDGE ( 'NONE', *, *, #38649, .F. ) ;
#4246 = CARTESIAN_POINT ( 'NONE',  ( 73.98997032606590096, 68.61244119570729083, 11.40121143613688304 ) ) ;
#4247 = CARTESIAN_POINT ( 'NONE',  ( 185.5580716964178407, 259.1746232884236747, -5.314944570831372950 ) ) ;
#4248 = CARTESIAN_POINT ( 'NONE',  ( 74.62401959271109320, 66.89443057110609914, 13.05059976691390311 ) ) ;
#4249 = VECTOR ( 'NONE', #2008, 1000.000000000000227 ) ;
#4250 = CARTESIAN_POINT ( 'NONE',  ( 190.3286155001717930, 300.9881631498979004, -5.624828231725103045 ) ) ;
#4251 = CARTESIAN_POINT ( 'NONE',  ( -110.0000000000000142, 15.00000000000000000, 9.212605237762145904 ) ) ;
#4252 = CARTESIAN_POINT ( 'NONE',  ( 207.2683629543511756, 271.6476598918739001, -6.694388351944108528 ) ) ;
#4253 = CARTESIAN_POINT ( 'NONE',  ( 182.4155610542803458, 284.2376793896972345, 14.93425214775039223 ) ) ;
#4254 = CARTESIAN_POINT ( 'NONE',  ( 73.89337880468768560, 68.29732366427398915, -11.63451623248603006 ) ) ;
#4255 = CARTESIAN_POINT ( 'NONE',  ( 52.86797706100236383, 192.1423013555410080, -4.594050593750043987 ) ) ;
#4256 = CARTESIAN_POINT ( 'NONE',  ( 92.09145065047481182, 230.6427522451419065, 10.00000000000009237 ) ) ;
#4257 = ADVANCED_FACE ( 'NONE', ( #31587 ), #21784, .F. ) ;
#4258 = EDGE_LOOP ( 'NONE', ( #49715, #3500, #95242, #1937 ) ) ;
#4259 = DIRECTION ( 'NONE',  ( 0.7033187449715098127, -0.7108746323872447981, 0.000000000000000000 ) ) ;
#4260 = CARTESIAN_POINT ( 'NONE',  ( -7.720288864461156919, 177.8967562850347122, -4.648177544792955347E-16 ) ) ;
#4261 = ADVANCED_FACE ( 'NONE', ( #28878 ), #5568, .T. ) ;
#4262 = CARTESIAN_POINT ( 'NONE',  ( -7.673045192009834814, 172.5024278399160664, -9.188101187500093303 ) ) ;
#4263 = CARTESIAN_POINT ( 'NONE',  ( 68.48685824045450943, 64.40307437426383785, -12.27912010813812138 ) ) ;
#4264 = CARTESIAN_POINT ( 'NONE',  ( 176.9878821292914211, 283.3466992399841615, -15.40003107629192769 ) ) ;
#4265 = VECTOR ( 'NONE', #17081, 1000.000000000000000 ) ;
#4266 = CARTESIAN_POINT ( 'NONE',  ( 176.4425850253208523, 252.1586887174202616, -1.458368723655519394 ) ) ;
#4267 = CARTESIAN_POINT ( 'NONE',  ( 193.0761489135300906, 296.2292956824684893, -11.99675185248219655 ) ) ;
#4268 = DIRECTION ( 'NONE',  ( 0.4270171210482451851, -0.9042435392811322137, 0.000000000000000000 ) ) ;
#4269 = CARTESIAN_POINT ( 'NONE',  ( 164.4272222519600746, 245.8506922426221593, 7.021336339662529902 ) ) ;
#4270 = CARTESIAN_POINT ( 'NONE',  ( 68.29626324166530082, 66.69358781172817885, 9.212701310791057807 ) ) ;
#4271 = CARTESIAN_POINT ( 'NONE',  ( 164.3774690880109119, 245.9368672504194819, -2.805681983503304000 ) ) ;
#4272 = ORIENTED_EDGE ( 'NONE', *, *, #33511, .T. ) ;
#4273 = CARTESIAN_POINT ( 'NONE',  ( -2.575951297163730835, 175.9865022471903160, 10.00000000000009237 ) ) ;
#4274 = CARTESIAN_POINT ( 'NONE',  ( -19.65312891409030271, 93.06504152958497400, 177.5919119679930134 ) ) ;
#4275 = CARTESIAN_POINT ( 'NONE',  ( 120.0114017305758551, 252.3464784336661353, 1.353441290958777327E-15 ) ) ;
#4276 = CARTESIAN_POINT ( 'NONE',  ( 15.95033727479334651, 30.18502408145591787, 5.678558825948277544 ) ) ;
#4277 = CARTESIAN_POINT ( 'NONE',  ( 74.72173318163055455, 67.07206250228034605, 12.96729955693541747 ) ) ;
#4278 = DIRECTION ( 'NONE',  ( 0.000000000000000000, 0.000000000000000000, 1.000000000000000000 ) ) ;
#4279 = B_SPLINE_CURVE_WITH_KNOTS ( 'NONE', 3,
 ( #20640, #59097, #66236, #21630, #6433, #97173, #43418, #43914, #27739, #29234, #81969, #58608, #97655, #59603, #75344, #12045, #89584, #35324, #13053, #91066, #98145, #89107, #19657, #83460, #12545, #90070, #90583, #50519, #5434, #81471, #51525, #42898, #36316, #67220, #60101 ),
 .UNSPECIFIED., .F., .F.,
 ( 4, 2, 2, 2, 2, 2, 1, 2, 2, 1, 2, 2, 1, 2, 2, 1, 1, 1, 1, 2, 4 ),
 ( 0.000000000000000000, 0.1115121842044346223, 0.1672682763066525302, 0.2230243684088704381, 0.3345365526133051159, 0.3902926447155220524, 0.4460487368177389889, 0.4739267828688474293, 0.5018048289199559253, 0.5575609210221736944, 0.6133170131243914636, 0.6690731052266091217, 0.7248291973288267798, 0.7387682203543819437, 0.7527072433799371076, 0.7805852894310503221, 0.8363413815332770840, 0.8642194275843916307, 0.8781584506099474607, 0.8851279621227241545, 0.8920974736355009593 ),
 .UNSPECIFIED. ) ;
#4281 = CARTESIAN_POINT ( 'NONE',  ( 74.96142304803882439, 67.14338225477067112, 13.01358479607535301 ) ) ;
#4280 = CARTESIAN_POINT ( 'NONE',  ( 186.1630411436486554, 296.9614825196608194, -7.488375694256206749 ) ) ;
#4282 = CARTESIAN_POINT ( 'NONE',  ( 17.05992553822454383, 21.80066082961421259, 10.00000000000000533 ) ) ;
#4283 = VERTEX_POINT ( 'NONE', #58754 ) ;
#4284 = CARTESIAN_POINT ( 'NONE',  ( 191.4044787581200069, 299.1247133251352466, 7.435199718141230818 ) ) ;
#4285 = CARTESIAN_POINT ( 'NONE',  ( 163.8402264623212545, 246.8673987741056237, 8.938446005630277469 ) ) ;
#4286 = LINE ( 'NONE', #73212, #52296 ) ;
#4287 = CARTESIAN_POINT ( 'NONE',  ( 164.3036517873781008, 252.3706336020835579, 13.60069832213670082 ) ) ;
#4288 = CARTESIAN_POINT ( 'NONE',  ( 81.60881798005151211, 55.57634303931474307, -16.32954282162994630 ) ) ;
#4289 = ORIENTED_EDGE ( 'NONE', *, *, #15269, .T. ) ;
#4290 = CARTESIAN_POINT ( 'NONE',  ( 68.82014897516015139, 66.62176625695347809, 9.652166363822647810 ) ) ;
#4291 = CARTESIAN_POINT ( 'NONE',  ( 168.9073988155618053, 271.9158883140793250, -17.00354098114102896 ) ) ;
#4292 = CARTESIAN_POINT ( 'NONE',  ( 71.92208958328382096, 72.24687304073742666, 0.6003283116912437878 ) ) ;
#4293 = CARTESIAN_POINT ( 'NONE',  ( 85.28397160125511789, 44.79186958938679197, 7.782623374060775312 ) ) ;
#4294 = CARTESIAN_POINT ( 'NONE',  ( 199.7995805052075866, 272.4254932667536764, 12.42849113847113252 ) ) ;
#4295 = CARTESIAN_POINT ( 'NONE',  ( 185.5553639007409004, 297.2884567403993969, 5.667419552555970519 ) ) ;
#4296 = CARTESIAN_POINT ( 'NONE',  ( 72.21207746560659757, 71.58261399135965064, -5.866756630810175288 ) ) ;
#4297 = DIRECTION ( 'NONE',  ( 0.4999999999999998890, -0.8660254037844385966, 0.000000000000000000 ) ) ;
#4298 = EDGE_LOOP ( 'NONE', ( #14769, #3930, #20433, #36614 ) ) ;
#4299 = DIRECTION ( 'NONE',  ( -0.3668518372888711077, -0.9302793824855948301, 0.000000000000000000 ) ) ;
#4300 = CARTESIAN_POINT ( 'NONE',  ( 4.482002306134333480, 24.36126292948892669, 6.180339887498949913 ) ) ;
#4301 = DIRECTION ( 'NONE',  ( 0.4999999999999992784, -0.8660254037844390407, 0.000000000000000000 ) ) ;
#4302 = ORIENTED_EDGE ( 'NONE', *, *, #72790, .F. ) ;
#4303 = CARTESIAN_POINT ( 'NONE',  ( 73.75884458225044682, 55.19329439359383116, 16.59761296138449538 ) ) ;
#4304 = CARTESIAN_POINT ( 'NONE',  ( 194.2389208611690492, 294.2153155915419802, -15.75132567904764791 ) ) ;
#4305 = CARTESIAN_POINT ( 'NONE',  ( 156.3084473884123042, 262.1325509154355018, -16.95104440301710014 ) ) ;
#4306 = ORIENTED_EDGE ( 'NONE', *, *, #98151, .T. ) ;
#4307 = CARTESIAN_POINT ( 'NONE',  ( 79.45469543192598394, 59.63697030301000979, 16.53293242656297224 ) ) ;
#4308 = FACE_OUTER_BOUND ( 'NONE', #57649, .T. ) ;
#4309 = CARTESIAN_POINT ( 'NONE',  ( 87.73591684602568819, 43.42914754852260018, 0.5750851355217611038 ) ) ;
#4310 = VECTOR ( 'NONE', #39859, 1000.000000000000000 ) ;
#4311 = CARTESIAN_POINT ( 'NONE',  ( 188.5410240070633563, 293.7196559869043426, 13.01390607220156248 ) ) ;
#4312 = ORIENTED_EDGE ( 'NONE', *, *, #48937, .T. ) ;
#4313 = CARTESIAN_POINT ( 'NONE',  ( 81.79837788435251866, 218.0333772461660544, 9.188101187500095079 ) ) ;
#4314 = CARTESIAN_POINT ( 'NONE',  ( 76.52406481382922721, 52.48284444663511294, -15.83437973198601867 ) ) ;
#4315 = CIRCLE ( 'NONE', #28611, 17.82106496071138224 ) ;
#4316 = CARTESIAN_POINT ( 'NONE',  ( 73.31376544620394498, 70.15701068496694859, -9.311920139903870464 ) ) ;
#4317 = CARTESIAN_POINT ( 'NONE',  ( 84.51862751403463392, 49.89385305662934655, -13.69084041065644897 ) ) ;
#4318 = CARTESIAN_POINT ( 'NONE',  ( 185.5169003523186859, 259.2275736936089743, -6.864738593364268837 ) ) ;
#4319 = ORIENTED_EDGE ( 'NONE', *, *, #43064, .F. ) ;
#4321 = VERTEX_POINT ( 'NONE', #10318 ) ;
#4320 =( BOUNDED_CURVE ( )  B_SPLINE_CURVE ( 2, ( #8637, #536, #56216, #31422, #15722, #62823, #93267, #40517, #39504 ),
 .UNSPECIFIED., .F., .T. ) 
 B_SPLINE_CURVE_WITH_KNOTS ( ( 3, 2, 2, 2, 3 ),
 ( 0.9314516129032257563, 0.9327956989247311315, 0.9354838709677418818, 0.9381720430107527431, 0.9395161290322581182 ),
 .UNSPECIFIED. ) 
 CURVE ( )  GEOMETRIC_REPRESENTATION_ITEM ( )  RATIONAL_B_SPLINE_CURVE ( ( 0.9330127018922194093, 0.9330127018922194093, 1.000000000000000000, 0.8660254037844387076, 1.000000000000000000, 0.8660254037844387076, 1.000000000000000000, 0.9330127018922194093, 0.9330127018922194093 ) ) 
 REPRESENTATION_ITEM ( '' )  );
#4322 = EDGE_CURVE ( 'NONE', #84216, #33383, #64004, .T. ) ;
#4324 = CIRCLE ( 'NONE', #15581, 0.1418229129681522482 ) ;
#4323 = CARTESIAN_POINT ( 'NONE',  ( -14.37785915960194494, 174.0530062829862743, 6.972266317189433612E-15 ) ) ;
#4325 = VERTEX_POINT ( 'NONE', #65865 ) ;
#4326 = DIRECTION ( 'NONE',  ( -0.000000000000000000, -0.000000000000000000, -1.000000000000000000 ) ) ;
#4327 = B_SPLINE_CURVE_WITH_KNOTS ( 'NONE', 3,
 ( #50927, #80392, #19573, #48953, #49942, #11473, #27654, #64653, #95603, #2873, #34245, #65634 ),
 .UNSPECIFIED., .F., .F.,
 ( 4, 2, 2, 2, 2, 4 ),
 ( 0.000000000000000000, 0.1937403633080442278, 0.3874807266160884556, 0.5812210899241326834, 0.6780912715781548528, 0.7749614532321769111 ),
 .UNSPECIFIED. ) ;
#4328 = ORIENTED_EDGE ( 'NONE', *, *, #36213, .T. ) ;
#4329 = ADVANCED_FACE ( 'NONE', ( #33106 ), #81615, .F. ) ;
#4330 = CARTESIAN_POINT ( 'NONE',  ( 75.64162694863910019, 61.89125772273574455, 15.26202274178806739 ) ) ;
#4331 = CARTESIAN_POINT ( 'NONE',  ( 203.1044072055706806, 278.8598428092302584, -16.67109798570195878 ) ) ;
#4332 = ORIENTED_EDGE ( 'NONE', *, *, #78318, .F. ) ;
#4333 = CARTESIAN_POINT ( 'NONE',  ( 206.7834510497742713, 272.4875519477961348, -7.518391375580527836 ) ) ;
#4334 =( BOUNDED_CURVE ( )  B_SPLINE_CURVE ( 2, ( #4554, #81111, #5065, #97776, #82107, #35454, #51661, #82610, #34460, #26866, #13176, #96807, #27857 ),
 .UNSPECIFIED., .F., .T. ) 
 B_SPLINE_CURVE_WITH_KNOTS ( ( 3, 2, 2, 2, 2, 2, 3 ),
 ( 0.2374999999999999889, 0.2399999999999999911, 0.2449999999999999956, 0.2500000000000000000, 0.2550000000000000044, 0.2600000000000000089, 0.2625000000000000111 ),
 .UNSPECIFIED. ) 
 CURVE ( )  GEOMETRIC_REPRESENTATION_ITEM ( )  RATIONAL_B_SPLINE_CURVE ( ( 0.9755282581475768211, 0.9755282581475768211, 1.000000000000000000, 0.9510565162951535312, 1.000000000000000000, 0.9510565162951535312, 1.000000000000000000, 0.9510565162951535312, 1.000000000000000000, 0.9510565162951535312, 1.000000000000000000, 0.9755282581475768211, 0.9755282581475768211 ) ) 
 REPRESENTATION_ITEM ( '' )  );
#4335 = CARTESIAN_POINT ( 'NONE',  ( 82.25473147846066979, 40.64636554663949397, 3.297339663603231941 ) ) ;
#4336 = FACE_OUTER_BOUND ( 'NONE', #76567, .T. ) ;
#4337 = EDGE_CURVE ( 'NONE', #32549, #90499, #61991, .T. ) ;
#4338 = DIRECTION ( 'NONE',  ( -0.3077152132536331575, -0.9514785060800222682, 0.000000000000000000 ) ) ;
#4339 = ADVANCED_FACE ( 'NONE', ( #90218 ), #90724, .T. ) ;
#4340 = CARTESIAN_POINT ( 'NONE',  ( 79.14312167556931854, 57.64441083166269664, 0.000000000000000000 ) ) ;
#4341 = CARTESIAN_POINT ( 'NONE',  ( 0.9603191016227148324, 181.3615022471903444, 5.000000000000046185 ) ) ;
#4342 = CARTESIAN_POINT ( 'NONE',  ( 143.8274474304129171, 253.8458772461660260, 9.188101187500095079 ) ) ;
#4343 = CARTESIAN_POINT ( 'NONE',  ( 167.9796227970851703, 267.0069495776506301, -16.94467948695188397 ) ) ;
#4344 = ORIENTED_EDGE ( 'NONE', *, *, #1379, .T. ) ;
#4345 = DIRECTION ( 'NONE',  ( -0.5544813661758285495, -0.8321961394790213795, 0.000000000000000000 ) ) ;
#4346 = ORIENTED_EDGE ( 'NONE', *, *, #1707, .T. ) ;
#4347 = CARTESIAN_POINT ( 'NONE',  ( 164.1398834480021378, 281.6669933700340493, 8.767707422804397410 ) ) ;
#4349 = VERTEX_POINT ( 'NONE', #79754 ) ;
#4348 = CARTESIAN_POINT ( 'NONE',  ( 85.51230132848702681, 48.33290926536287913, -12.21747540207229221 ) ) ;
#4350 = CIRCLE ( 'NONE', #36730, 70.00000000000001421 ) ;
#4351 = CARTESIAN_POINT ( 'NONE',  ( -14.30703472742949245, 105.2809231865207522, 10.47389102980036313 ) ) ;
#4352 = CARTESIAN_POINT ( 'NONE',  ( 202.7865629936218284, 279.4103651332174536, 17.10878160033216133 ) ) ;
#4353 = CARTESIAN_POINT ( 'NONE',  ( 170.6105105942687032, 288.5462187197699109, -5.627715764860385050 ) ) ;
#4354 = CARTESIAN_POINT ( 'NONE',  ( 153.3397897684428131, 276.8807737960509598, 7.109465309109985753 ) ) ;
#4355 = LINE ( 'NONE', #81399, #90694 ) ;
#4356 = CARTESIAN_POINT ( 'NONE',  ( 171.2776707721998264, 280.4287170469435750, 13.77496485982851304 ) ) ;
#4357 = CARTESIAN_POINT ( 'NONE',  ( 168.0584336595957211, 252.9231910825713214, 11.85262793608598031 ) ) ;
#4358 = CARTESIAN_POINT ( 'NONE',  ( 88.41177868068123757, 44.08414425260226466, -2.750064808092239410 ) ) ;
#4359 = ORIENTED_EDGE ( 'NONE', *, *, #28939, .T. ) ;
#4360 = DIRECTION ( 'NONE',  ( 0.000000000000000000, 0.000000000000000000, -1.000000000000000000 ) ) ;
#4361 = CARTESIAN_POINT ( 'NONE',  ( 66.34509500891661560, 68.88037130226740601, 0.1021054603021520624 ) ) ;
#4362 = ORIENTED_EDGE ( 'NONE', *, *, #83987, .T. ) ;
#4363 = CARTESIAN_POINT ( 'NONE',  ( 194.3518562708335651, 293.5167449611453208, -14.44919933576977122 ) ) ;
#4364 = CARTESIAN_POINT ( 'NONE',  ( 201.0458349605253545, 267.5706676224597800, -2.392963673958802939 ) ) ;
#4365 = CARTESIAN_POINT ( 'NONE',  ( 37.44155836008122407, 106.5941701475231724, 59.99999999999999289 ) ) ;
#4366 = CYLINDRICAL_SURFACE ( 'NONE', #60771, 9.212605237762131694 ) ;
#4367 = CARTESIAN_POINT ( 'NONE',  ( 49.54000814145099696, 103.6626726051169527, -10.00000000000000000 ) ) ;
#4369 = CARTESIAN_POINT ( 'NONE',  ( 88.15895072599572302, 44.32995048785090120, 2.709407056482791898 ) ) ;
#4368 = CARTESIAN_POINT ( 'NONE',  ( 160.9155581428462085, 282.2930683307629920, -7.657675304491033508 ) ) ;
#4370 = CARTESIAN_POINT ( 'NONE',  ( 203.2529752088261716, 269.9999405576584763, 6.016569300217926575 ) ) ;
#4371 = VERTEX_POINT ( 'NONE', #72124 ) ;
#4372 = VERTEX_POINT ( 'NONE', #74988 ) ;
#4373 = LINE ( 'NONE', #35272, #92151 ) ;
#4374 = CARTESIAN_POINT ( 'NONE',  ( 189.8703400361598312, 274.0992181554749436, -15.62282287125612434 ) ) ;
#4375 = CARTESIAN_POINT ( 'NONE',  ( 71.52376905861159173, 65.98510282706405405, -11.84387761488746804 ) ) ;
#4376 = CARTESIAN_POINT ( 'NONE',  ( 171.6704389044023458, 289.7300494326029252, 2.700906889728273086 ) ) ;
#4377 = CARTESIAN_POINT ( 'NONE',  ( 192.6797324865049745, 296.9159090750308110, 12.42053959885222625 ) ) ;
#4378 = CARTESIAN_POINT ( 'NONE',  ( 80.77778805714483212, 43.59742387627670723, -9.572361431960153766 ) ) ;
#4379 = CARTESIAN_POINT ( 'NONE',  ( 52.82617185314417441, 189.7592609112379876, 2.679491924311254714 ) ) ;
#4380 = CARTESIAN_POINT ( 'NONE',  ( -2.476892769303202790, 175.5024278399161233, -9.188101187500093303 ) ) ;
#4381 = CARTESIAN_POINT ( 'NONE',  ( 116.0067284296028589, 225.5327760586659451, 1.948934522072303157E-15 ) ) ;
#4382 = CARTESIAN_POINT ( 'NONE',  ( 40.79748767570693246, 194.3615022471902591, -10.00000000000009592 ) ) ;
#4383 = CARTESIAN_POINT ( 'NONE',  ( 184.1809134956363607, 294.4725012015020411, -7.735934973952240945 ) ) ;
#4384 = CARTESIAN_POINT ( 'NONE',  ( 77.79465598582810060, 50.60749197390607890, 15.20047523612101692 ) ) ;
#4386 = ADVANCED_FACE ( 'NONE', ( #59755 ), #36460, .F. ) ;
#4385 = AXIS2_PLACEMENT_3D ( 'NONE', #5734, #75645, #98459 ) ;
#4387 = CARTESIAN_POINT ( 'NONE',  ( 77.50346144362303846, 52.20099699948093530, 15.68093582552386067 ) ) ;
#4388 = VECTOR ( 'NONE', #14547, 1000.000000000000000 ) ;
#4389 = CARTESIAN_POINT ( 'NONE',  ( 160.8590558562208912, 281.7049668674798681, 5.440820967619280246 ) ) ;
#4390 = CARTESIAN_POINT ( 'NONE',  ( 148.3874010092782498, 273.6324775792697892, -8.328854486678444857 ) ) ;
#4391 = CARTESIAN_POINT ( 'NONE',  ( 84.45465033531688448, 50.16481452220934756, 13.87013043972112847 ) ) ;
#4392 = CARTESIAN_POINT ( 'NONE',  ( 85.03695205236203947, 213.2365022471901739, -10.00000000000009237 ) ) ;
#4393 = CARTESIAN_POINT ( 'NONE',  ( 139.3620039403753879, 261.2677522451419350, -5.000000000000047962 ) ) ;
#4394 = EDGE_CURVE ( 'NONE', #28770, #40778, #52157, .T. ) ;
#4395 = VECTOR ( 'NONE', #97820, 1000.000000000000227 ) ;
#4396 = FACE_OUTER_BOUND ( 'NONE', #89210, .T. ) ;
#4397 = ADVANCED_FACE ( 'NONE', ( #34964 ), #82488, .F. ) ;
#4398 = CARTESIAN_POINT ( 'NONE',  ( 71.75763553740291911, 221.4244531367911293, -4.594050593750046652 ) ) ;
#4399 = CARTESIAN_POINT ( 'NONE',  ( 161.8935665241663457, 250.2391126920490194, -13.69501063978231770 ) ) ;
#4400 = CARTESIAN_POINT ( 'NONE',  ( 72.90436461565970205, 57.14737113808597258, 15.90414412829909629 ) ) ;
#4401 = CARTESIAN_POINT ( 'NONE',  ( 163.2100640172580199, 258.2939446478983427, 16.33648908913500364 ) ) ;
#4403 = CARTESIAN_POINT ( 'NONE',  ( 199.6580449488688771, 284.8291173391253892, 17.61636456357554437 ) ) ;
#4402 = CARTESIAN_POINT ( 'NONE',  ( 195.6974783896144174, 291.6890198465123945, 16.70600479393688431 ) ) ;
#4404 = B_SPLINE_CURVE_WITH_KNOTS ( 'NONE', 3,
 ( #54876, #32587, #69082, #92914, #93426, #63485 ),
 .UNSPECIFIED., .F., .F.,
 ( 4, 2, 4 ),
 ( 0.006526230984275955063, 0.006760533473033110939, 0.006994835961790266815 ),
 .UNSPECIFIED. ) ;
#4405 = CARTESIAN_POINT ( 'NONE',  ( 198.9225589249066957, 286.1030165008847916, -17.03502353404871883 ) ) ;
#4406 = CARTESIAN_POINT ( 'NONE',  ( 203.7690284654797210, 275.7086850192775955, -13.99192714286714612 ) ) ;
#4407 = CARTESIAN_POINT ( 'NONE',  ( 34.84050961144773595, 32.06628583063844218, -9.188101187500006262 ) ) ;
#4408 = CARTESIAN_POINT ( 'NONE',  ( 193.2140586456748679, 295.9904290195353269, -12.67640480829088823 ) ) ;
#4409 = CYLINDRICAL_SURFACE ( 'NONE', #40994, 70.00000000000002842 ) ;
#4410 = ORIENTED_EDGE ( 'NONE', *, *, #58194, .T. ) ;
#4411 = CARTESIAN_POINT ( 'NONE',  ( 28.70736568013821355, 22.28920272979928185, -7.433330006724141015 ) ) ;
#4412 = CIRCLE ( 'NONE', #95072, 11.91750000000000043 ) ;
#4413 = CARTESIAN_POINT ( 'NONE',  ( 8.751641773298651117, 23.79103043416547081, 8.090169943749478065 ) ) ;
#4414 = CARTESIAN_POINT ( 'NONE',  ( -52.87923565380747704, 93.80454242329714987, -10.00000000000000000 ) ) ;
#4415 = CARTESIAN_POINT ( 'NONE',  ( 188.3152126950631100, 286.0690311334317357, -16.15890536769158459 ) ) ;
#4416 = ORIENTED_EDGE ( 'NONE', *, *, #70885, .F. ) ;
#4417 = CARTESIAN_POINT ( 'NONE',  ( 86.44281908042910345, 47.25702098485090374, 10.76508247627446302 ) ) ;
#4418 = CARTESIAN_POINT ( 'NONE',  ( 153.6596595523362794, 266.9882342533689439, 16.60685250298524807 ) ) ;
#4419 = CARTESIAN_POINT ( 'NONE',  ( 72.42375743991897252, 71.58586897710435437, 5.137075947767138828 ) ) ;
#4420 = CARTESIAN_POINT ( 'NONE',  ( 141.3286032983506004, 245.7365022471902307, 10.00000000000009592 ) ) ;
#4421 = CARTESIAN_POINT ( 'NONE',  ( 205.4029933437358295, 274.8785748323546159, -13.50815392427034922 ) ) ;
#4423 = VECTOR ( 'NONE', #44882, 1000.000000000000114 ) ;
#4422 = CARTESIAN_POINT ( 'NONE',  ( 74.86122959240560704, 53.28810031052174168, 16.52678853274738913 ) ) ;
#4424 = ORIENTED_EDGE ( 'NONE', *, *, #74556, .T. ) ;
#4425 = CARTESIAN_POINT ( 'NONE',  ( 165.6439160563409416, 246.9868693674390840, -1.864321359011917867 ) ) ;
#4426 = VERTEX_POINT ( 'NONE', #91692 ) ;
#4427 = CARTESIAN_POINT ( 'NONE',  ( 196.7817283509550919, 264.7241178856941701, -4.656590905670582536 ) ) ;
#4428 = CARTESIAN_POINT ( 'NONE',  ( 66.22369928180467014, 68.54468502351485881, 4.796181935161453858 ) ) ;
#4429 = VERTEX_POINT ( 'NONE', #53157 ) ;
#4430 = CARTESIAN_POINT ( 'NONE',  ( 77.15970654835309972, 62.92887492094936874, -15.28573681817205099 ) ) ;
#4431 = ORIENTED_EDGE ( 'NONE', *, *, #95511, .T. ) ;
#4432 = CARTESIAN_POINT ( 'NONE',  ( 189.3260947096056839, 290.0486036062610538, 14.38962922108246900 ) ) ;
#4433 = CARTESIAN_POINT ( 'NONE',  ( 3.886609837484615415, 24.01751292744053856, 6.180339887498949913 ) ) ;
#4434 = CARTESIAN_POINT ( 'NONE',  ( 157.5367219092377695, 258.1941064437173168, -16.74304786559553904 ) ) ;
#4435 = CARTESIAN_POINT ( 'NONE',  ( 87.89481703180801730, 44.20627101738029552, -4.400163950806246227 ) ) ;
#4436 = CARTESIAN_POINT ( 'NONE',  ( 83.30270248594673888, 48.09331988551172543, 12.99346492355625493 ) ) ;
#4437 = B_SPLINE_CURVE_WITH_KNOTS ( 'NONE', 3,
 ( #64718, #34306, #26215, #65206, #73806, #19134, #4400, #57591, #88572, #50007 ),
 .UNSPECIFIED., .F., .F.,
 ( 4, 2, 2, 2, 4 ),
 ( 0.000000000000000000, 0.2500000000000000000, 0.5000000000000000000, 0.7500000000000000000, 1.000000000000000000 ),
 .UNSPECIFIED. ) ;
#4438 = CARTESIAN_POINT ( 'NONE',  ( 38.16387531507685793, 24.96004757982092315, -5.678558825948275768 ) ) ;
#4439 = CARTESIAN_POINT ( 'NONE',  ( 75.11394087589162893, 59.95852931487045367, -15.66470097906968739 ) ) ;
#4440 = EDGE_CURVE ( 'NONE', #73330, #20729, #53097, .T. ) ;
#4441 = LINE ( 'NONE', #59619, #74054 ) ;
#4442 = DIRECTION ( 'NONE',  ( 1.000000000000000000, 0.000000000000000000, -1.082076799516502080E-16 ) ) ;
#4443 = ORIENTED_EDGE ( 'NONE', *, *, #72309, .F. ) ;
#4444 = ORIENTED_EDGE ( 'NONE', *, *, #48746, .F. ) ;
#4445 = CARTESIAN_POINT ( 'NONE',  ( 42.33744422746375591, 122.7866300363639169, -10.00000000000000000 ) ) ;
#4447 = CARTESIAN_POINT ( 'NONE',  ( 147.6508870500795467, 274.9081571770856272, -8.950912509993816712 ) ) ;
#4446 = CARTESIAN_POINT ( 'NONE',  ( 68.31114388777692170, 65.60375069781311197, 10.42464132957602096 ) ) ;
#4448 = CARTESIAN_POINT ( 'NONE',  ( 85.65560247527419335, 48.36830939525689388, -11.71305587975093054 ) ) ;
#4449 = CARTESIAN_POINT ( 'NONE',  ( 155.2419697281468416, 261.7600162942170527, 18.58580762350309357 ) ) ;
#4450 = CARTESIAN_POINT ( 'NONE',  ( 120.8381292345549127, 252.1199935810940929, 2.679491924311251605 ) ) ;
#4451 = CARTESIAN_POINT ( 'NONE',  ( 187.3067335226663772, 291.4160526537789906, -14.11360718373232359 ) ) ;
#4452 = ADVANCED_FACE ( 'NONE', ( #87134 ), #16184, .F. ) ;
#4453 = DIRECTION ( 'NONE',  ( -0.8660254037844387076, -0.4999999999999998890, -0.000000000000000000 ) ) ;
#4454 = EDGE_CURVE ( 'NONE', #50641, #2713, #84542, .T. ) ;
#4455 = CARTESIAN_POINT ( 'NONE',  ( 190.1758200331204876, 279.2204749713225169, -17.78067544974210890 ) ) ;
#4456 = LINE ( 'NONE', #66264, #87262 ) ;
#4457 = CARTESIAN_POINT ( 'NONE',  ( 105.1271107466783121, 225.3768266524159856, 9.188101187500098632 ) ) ;
#4458 = ORIENTED_EDGE ( 'NONE', *, *, #93100, .T. ) ;
#4460 = EDGE_CURVE ( 'NONE', #68256, #29855, #91909, .T. ) ;
#4459 = CARTESIAN_POINT ( 'NONE',  ( 150.6571681785161445, 269.7011255207979730, 15.24894850018880454 ) ) ;
#4461 = DIRECTION ( 'NONE',  ( 1.000000000000000000, 0.000000000000000000, 0.000000000000000000 ) ) ;
#4462 = CARTESIAN_POINT ( 'NONE',  ( 163.0336413175346877, 276.6660547541027881, -14.15222362243524046 ) ) ;
#4463 = CIRCLE ( 'NONE', #23895, 12.50000000000000000 ) ;
#4464 = ORIENTED_EDGE ( 'NONE', *, *, #3944, .T. ) ;
#4465 = AXIS2_PLACEMENT_3D ( 'NONE', #63752, #73361, #41946 ) ;
#4466 = ORIENTED_EDGE ( 'NONE', *, *, #77991, .F. ) ;
#4467 = ORIENTED_EDGE ( 'NONE', *, *, #75237, .F. ) ;
#4468 = CARTESIAN_POINT ( 'NONE',  ( -22.42236680055709641, 157.8615022471902591, 0.000000000000000000 ) ) ;
#4470 = B_SPLINE_SURFACE_WITH_KNOTS ( 'NONE', 3, 1, ( 
 ( #31610, #63526 ),
 ( #48336, #25019 ),
 ( #2755, #70623 ),
 ( #63027, #87420 ),
 ( #77750, #1234 ),
 ( #9855, #93470 ),
 ( #55403, #93971 ),
 ( #86388, #78745 ),
 ( #48847, #79282 ),
 ( #32117, #71658 ),
 ( #16920, #17948 ),
 ( #47809, #9333 ),
 ( #2249, #55899 ),
 ( #64030, #94972 ),
 ( #39201, #8333 ),
 ( #25536, #79779 ),
 ( #64536, #70113 ),
 ( #95495, #26046 ),
 ( #15922, #65034 ),
 ( #82277, #43709 ),
 ( #12338, #96976 ),
 ( #11847, #80788 ),
 ( #5228, #96472 ),
 ( #11362, #4220 ),
 ( #18951, #34623 ),
 ( #97936, #42216 ),
 ( #89389, #49830 ),
 ( #50815, #4739 ),
 ( #27040, #73153 ),
 ( #88903, #74651 ),
 ( #36106, #35623 ),
 ( #19464, #95981 ),
 ( #67011, #56917 ),
 ( #43203, #27544 ) ),
 .UNSPECIFIED., .T., .F., .F.,
 ( 4, 2, 2, 2, 2, 2, 2, 2, 2, 2, 2, 2, 2, 2, 2, 2, 4 ),
 ( 2, 2 ),
 ( 0.000000000000000000, 0.06250000000000000000, 0.1250000000000000000, 0.1875000000000000000, 0.2500000000000000000, 0.3125000000000000000, 0.3750000000000000000, 0.4375000000000000000, 0.5000000000000000000, 0.5625000000000000000, 0.6250000000000000000, 0.6875000000000000000, 0.7500000000000000000, 0.8125000000000000000, 0.8750000000000000000, 0.9375000000000000000, 1.000000000000000000 ),
 ( 0.000000000000000000, 1.000000000000000000 ),
 .UNSPECIFIED. ) ;
#4469 = CARTESIAN_POINT ( 'NONE',  ( 71.48247391640994408, 59.13597001042445811, 15.29777321559891412 ) ) ;
#4471 = CARTESIAN_POINT ( 'NONE',  ( 157.7233946900069839, 257.4620621851055375, 16.86796251324260254 ) ) ;
#4472 = CARTESIAN_POINT ( 'NONE',  ( 159.8188415394622268, 253.8326417772889840, -15.43862849427313222 ) ) ;
#4473 = CARTESIAN_POINT ( 'NONE',  ( 208.3490404761574553, 269.7758715175073689, 2.423947743236856578 ) ) ;
#4474 = ORIENTED_EDGE ( 'NONE', *, *, #48621, .F. ) ;
#4475 = AXIS2_PLACEMENT_3D ( 'NONE', #15081, #1904, #25186 ) ;
#4476 = ORIENTED_EDGE ( 'NONE', *, *, #11776, .T. ) ;
#4477 = CARTESIAN_POINT ( 'NONE',  ( 208.3699316049496133, 269.7396870210121733, -1.898463622294385811 ) ) ;
#4478 = ORIENTED_EDGE ( 'NONE', *, *, #94253, .F. ) ;
#4479 = CARTESIAN_POINT ( 'NONE',  ( 195.1474640768281290, 265.6393084148356252, -8.887799905196541062 ) ) ;
#4480 = CARTESIAN_POINT ( 'NONE',  ( 153.2151911666999808, 266.1153816512735943, 16.19125425417644948 ) ) ;
#4481 = CARTESIAN_POINT ( 'NONE',  ( 83.40135606954622460, 47.43196963034611002, 11.92714562067884465 ) ) ;
#4483 = CARTESIAN_POINT ( 'NONE',  ( 69.54685086556757767, 62.58220806599024399, -13.90877278120082572 ) ) ;
#4482 = CARTESIAN_POINT ( 'NONE',  ( 130.8370663736463655, 246.3458772461660544, 9.188101187500095079 ) ) ;
#4484 = LINE ( 'NONE', #74901, #51114 ) ;
#4485 = ORIENTED_EDGE ( 'NONE', *, *, #23194, .T. ) ;
#4486 = CIRCLE ( 'NONE', #17429, 15.60714546451156970 ) ;
#4487 = CARTESIAN_POINT ( 'NONE',  ( 204.7088172315186512, 276.0809231281156144, 13.09496711537969027 ) ) ;
#4488 = CARTESIAN_POINT ( 'NONE',  ( 71.05939029094800219, 61.29899699392983337, 14.43395936496894372 ) ) ;
#4489 = CARTESIAN_POINT ( 'NONE',  ( 82.17449527959013267, 40.64114721183973700, -3.468282653352762424 ) ) ;
#4490 = CARTESIAN_POINT ( 'NONE',  ( 192.1705252917600433, 271.8754300319524191, 14.16870868845061082 ) ) ;
#4491 = CARTESIAN_POINT ( 'NONE',  ( 159.5180972751518595, 279.0588588540967976, -11.03979334413982016 ) ) ;
#4492 = CARTESIAN_POINT ( 'NONE',  ( 76.13392677502470463, 51.08280539179364865, -16.07326884494762353 ) ) ;
#4493 = CARTESIAN_POINT ( 'NONE',  ( 199.0946232933934539, 281.9005678297153850, -16.60409553737443034 ) ) ;
#4494 = DIRECTION ( 'NONE',  ( -0.000000000000000000, -0.000000000000000000, -1.000000000000000000 ) ) ;
#4495 = CARTESIAN_POINT ( 'NONE',  ( 80.28488664218848214, 51.35788028056815335, 15.03242532107574903 ) ) ;
#4496 = VECTOR ( 'NONE', #18224, 1000.000000000000114 ) ;
#4497 = CARTESIAN_POINT ( 'NONE',  ( 206.3023480738090996, 271.3208467458289874, 7.632938913807082670 ) ) ;
#4498 = CARTESIAN_POINT ( 'NONE',  ( 167.6421291605131785, 249.9379862031578625, 6.991320327740723428 ) ) ;
#4499 = CARTESIAN_POINT ( 'NONE',  ( 77.74340892523753155, 61.62887588481113710, 16.08014808546132457 ) ) ;
#4500 = CARTESIAN_POINT ( 'NONE',  ( 178.4479030810299207, 292.4469683173247176, -5.630510813558092131 ) ) ;
#4501 = ADVANCED_FACE ( 'NONE', ( #73368 ), #59630, .F. ) ;
#4502 = CARTESIAN_POINT ( 'NONE',  ( -20.87573318553691593, 95.07663899570583510, 45.19945584158065799 ) ) ;
#4503 = ADVANCED_FACE ( 'NONE', ( #18671 ), #51037, .T. ) ;
#4504 = CARTESIAN_POINT ( 'NONE',  ( 40.33962347462181697, 28.45404122711136452, -8.090169943749478065 ) ) ;
#4505 = CARTESIAN_POINT ( 'NONE',  ( 67.16990927169524639, 66.79708245693809943, -9.067759095298582039 ) ) ;
#4506 = CARTESIAN_POINT ( 'NONE',  ( -19.75907871001397353, 92.97076332750987149, 59.99999999999999289 ) ) ;
#4507 = CARTESIAN_POINT ( 'NONE',  ( 161.0794898748901858, 273.2957853699189172, -15.15413963670030739 ) ) ;
#4508 = CARTESIAN_POINT ( 'NONE',  ( 83.90373659686035523, 43.27808524138897894, -6.473827899055408786 ) ) ;
#4509 = CARTESIAN_POINT ( 'NONE',  ( 17.19803509898326510, 189.9244531367911293, -4.594050593750046652 ) ) ;
#4510 = CARTESIAN_POINT ( 'NONE',  ( 71.29042387187584495, 72.21982342411818934, 1.426054166102403542 ) ) ;
#4511 = ORIENTED_EDGE ( 'NONE', *, *, #77236, .T. ) ;
#4512 = VECTOR ( 'NONE', #59448, 1000.000000000000000 ) ;
#4513 = EDGE_CURVE ( 'NONE', #99632, #46611, #92611, .T. ) ;
#4514 = CARTESIAN_POINT ( 'NONE',  ( 87.37955803993382631, 45.91052472906853410, 8.478299845497456744 ) ) ;
#4515 = CARTESIAN_POINT ( 'NONE',  ( 194.2158379711820544, 277.1301694417633712, 17.09965426914677167 ) ) ;
#4516 = CARTESIAN_POINT ( 'NONE',  ( 71.70445494439258027, 72.46184198916859032, -1.357087204883099751 ) ) ;
#4517 = CARTESIAN_POINT ( 'NONE',  ( 38.09089796528284211, 201.9869531367911293, 4.594050593750046652 ) ) ;
#4518 = AXIS2_PLACEMENT_3D ( 'NONE', #55902, #40207, #25540 ) ;
#4519 = CARTESIAN_POINT ( 'NONE',  ( 86.99418556918212175, 46.03399372306155612, 8.963501050606421217 ) ) ;
#4520 = CARTESIAN_POINT ( 'NONE',  ( 174.2509005389064498, 289.3797888277572952, 7.946914131557713645 ) ) ;
#4521 = CARTESIAN_POINT ( 'NONE',  ( 147.0670278774466908, 275.9194309285509235, 3.666898409139099257 ) ) ;
#4522 = CARTESIAN_POINT ( 'NONE',  ( 41.98060738119045254, 32.43677371833805978, -10.00000000000000355 ) ) ;
#4523 = CARTESIAN_POINT ( 'NONE',  ( 199.8626824144776606, 267.9900519737070113, -6.523113416085821292 ) ) ;
#4524 = CARTESIAN_POINT ( 'NONE',  ( 178.7159350970735261, 293.8993888918343487, 2.713728331163343555 ) ) ;
#4525 = CARTESIAN_POINT ( 'NONE',  ( 179.1784693145256142, 278.4914505192345473, -17.09466235216729402 ) ) ;
#4526 = CARTESIAN_POINT ( 'NONE',  ( 149.0358100033410267, 277.1350342654116048, 3.013846530473550445 ) ) ;
#4527 = CARTESIAN_POINT ( 'NONE',  ( 167.0744888229918956, 257.9696763678884963, -15.40152651063776013 ) ) ;
#4528 = EDGE_CURVE ( 'NONE', #89364, #31208, #95884, .T. ) ;
#4529 = LINE ( 'NONE', #14131, #47689 ) ;
#4531 = CARTESIAN_POINT ( 'NONE',  ( 87.65912573706349065, 45.31011780831707370, -7.252675111195947544 ) ) ;
#4530 = VECTOR ( 'NONE', #20222, 1000.000000000000114 ) ;
#4532 = CARTESIAN_POINT ( 'NONE',  ( 104.4503548538632316, 221.1115022471901739, -5.000000000000041744 ) ) ;
#4533 = DIRECTION ( 'NONE',  ( 1.000000000000000000, 0.000000000000000000, 0.000000000000000000 ) ) ;
#4534 = CARTESIAN_POINT ( 'NONE',  ( 161.7453106966084704, 267.8664946259053181, -17.40444035468481943 ) ) ;
#4535 = ORIENTED_EDGE ( 'NONE', *, *, #59772, .T. ) ;
#4536 = CARTESIAN_POINT ( 'NONE',  ( 64.04520420253651025, 195.5327760586659736, 1.948934522072303157E-15 ) ) ;
#4537 = ORIENTED_EDGE ( 'NONE', *, *, #66771, .F. ) ;
#4538 = CARTESIAN_POINT ( 'NONE',  ( -6.649575753788274923, 83.58322560409861524, 13.50909007041568621 ) ) ;
#4539 = CARTESIAN_POINT ( 'NONE',  ( 147.3984236761635884, 275.3454365677582700, 5.108566646342994844 ) ) ;
#4540 = CARTESIAN_POINT ( 'NONE',  ( 67.30093204598001932, 67.22481299031751689, -8.581777852237747695 ) ) ;
#4541 = ORIENTED_EDGE ( 'NONE', *, *, #13452, .F. ) ;
#4542 = CARTESIAN_POINT ( 'NONE',  ( 171.1315556791619770, 286.9288989291006828, 8.543482685092364193 ) ) ;
#4543 = CARTESIAN_POINT ( 'NONE',  ( 206.9059968923335475, 272.2752963222270068, 6.902135944297345560 ) ) ;
#4544 = CARTESIAN_POINT ( 'NONE',  ( 193.1459436135753833, 292.3487159552965409, -15.56164613900618754 ) ) ;
#4545 = CARTESIAN_POINT ( 'NONE',  ( 26.65419051621551461, 38.49540643055190259, 3.479690158560446702E-15 ) ) ;
#4546 = CARTESIAN_POINT ( 'NONE',  ( 188.2179220736648233, 265.0898711547592370, 10.74980725069386978 ) ) ;
#4547 = CARTESIAN_POINT ( 'NONE',  ( 86.44477669634372319, 47.51534994824657332, -10.48323238175251504 ) ) ;
#4548 = DIRECTION ( 'NONE',  ( -0.5000000000000003331, 0.8660254037844383745, 0.000000000000000000 ) ) ;
#4549 = VERTEX_POINT ( 'NONE', #12567 ) ;
#4550 = ADVANCED_FACE ( 'NONE', ( #3481 ), #82511, .T. ) ;
#4551 = CARTESIAN_POINT ( 'NONE',  ( 16.17646586176480739, 17.84335787977762422, 9.188101187500006262 ) ) ;
#4552 = CARTESIAN_POINT ( 'NONE',  ( -16.10531488956837975, 22.89493580087430402, -10.00000000000000000 ) ) ;
#4553 = LINE ( 'NONE', #50644, #84057 ) ;
#4554 = CARTESIAN_POINT ( 'NONE',  ( 20.76088743254790003, 12.39040679176982529, 1.333680081654574804E-15 ) ) ;
#4555 = EDGE_CURVE ( 'NONE', #39135, #93866, #4967, .T. ) ;
#4556 = ORIENTED_EDGE ( 'NONE', *, *, #75424, .F. ) ;
#4557 = CARTESIAN_POINT ( 'NONE',  ( 182.4527117421103526, 284.0689693941391738, 15.01769654107919116 ) ) ;
#4558 = CARTESIAN_POINT ( 'NONE',  ( 191.5694344253287511, 298.8390017285333897, 8.250976118904059575 ) ) ;
#4559 = CARTESIAN_POINT ( 'NONE',  ( 70.29419212219671920, 65.26512559587472140, -12.42138800992322345 ) ) ;
#4560 = VERTEX_POINT ( 'NONE', #74873 ) ;
#4561 = VERTEX_POINT ( 'NONE', #5455 ) ;
#4562 = EDGE_CURVE ( 'NONE', #63766, #16186, #49551, .T. ) ;
#4563 = VECTOR ( 'NONE', #36815, 1000.000000000000227 ) ;
#4565 = DIRECTION ( 'NONE',  ( 1.000000000000000000, 0.000000000000000000, 0.000000000000000000 ) ) ;
#4564 = CARTESIAN_POINT ( 'NONE',  ( 161.2977680094314223, 251.2710659906439616, -13.03191437619249982 ) ) ;
#4566 = CARTESIAN_POINT ( 'NONE',  ( 196.2421909983451940, 290.7455499326673021, -17.31908925000307065 ) ) ;
#4567 = ORIENTED_EDGE ( 'NONE', *, *, #30771, .F. ) ;
#4568 = CARTESIAN_POINT ( 'NONE',  ( 66.10902144195793539, 69.14947487106338997, -2.045211508994028815 ) ) ;
#4569 = CYLINDRICAL_SURFACE ( 'NONE', #75553, 17.82106496071139645 ) ;
#4570 = CARTESIAN_POINT ( 'NONE',  ( 82.39721099668476256, 40.42262220707492304, 1.474573639734339192 ) ) ;
#4571 = CARTESIAN_POINT ( 'NONE',  ( 78.14027010749673252, 61.52421145379764766, -16.15198519767693242 ) ) ;
#4572 = CARTESIAN_POINT ( 'NONE',  ( 72.08258120803394320, 72.26635199662449338, -1.519792127538861504 ) ) ;
#4573 = EDGE_CURVE ( 'NONE', #69960, #75741, #26759, .T. ) ;
#4574 = CARTESIAN_POINT ( 'NONE',  ( 118.4422513298640638, 233.0643266524159856, 9.188101187500095079 ) ) ;
#4575 = EDGE_CURVE ( 'NONE', #32378, #29964, #82228, .T. ) ;
#4576 = CARTESIAN_POINT ( 'NONE',  ( 150.8359915840788688, 269.3913942967808453, 15.73449616766854575 ) ) ;
#4577 = CARTESIAN_POINT ( 'NONE',  ( 109.1413257910288479, 240.4865022471902876, 10.00000000000009415 ) ) ;
#4578 = ORIENTED_EDGE ( 'NONE', *, *, #23692, .T. ) ;
#4579 = B_SPLINE_CURVE_WITH_KNOTS ( 'NONE', 3,
 ( #95889, #89295, #94872, #19849, #9761, #87320, #12244, #98344, #59296, #5134 ),
 .UNSPECIFIED., .F., .F.,
 ( 4, 2, 2, 2, 4 ),
 ( 0.000000000000000000, 0.2500000000000000000, 0.5000000000000000000, 0.7500000000000000000, 1.000000000000000000 ),
 .UNSPECIFIED. ) ;
#4580 = CARTESIAN_POINT ( 'NONE',  ( 163.7323023463233937, 247.0543288263758086, -6.244751637846886361 ) ) ;
#4581 = VERTEX_POINT ( 'NONE', #77342 ) ;
#4582 = ORIENTED_EDGE ( 'NONE', *, *, #93275, .T. ) ;
#4583 = EDGE_CURVE ( 'NONE', #11342, #55246, #5949, .T. ) ;
#4584 = FACE_BOUND ( 'NONE', #53871, .T. ) ;
#4585 = CARTESIAN_POINT ( 'NONE',  ( 75.06695094285400671, 67.05599132900850634, -12.66018568268392208 ) ) ;
#4586 = EDGE_CURVE ( 'NONE', #6702, #28883, #37482, .T. ) ;
#4587 = CARTESIAN_POINT ( 'NONE',  ( 74.78872445064843077, 223.1744531367911293, 4.594050593750047540 ) ) ;
#4588 = CARTESIAN_POINT ( 'NONE',  ( 57.60966550219794158, 179.2419560658248940, -18.47570218321542868 ) ) ;
#4589 = CARTESIAN_POINT ( 'NONE',  ( 81.41589984655307433, 56.11952908245346805, 16.07747354504519421 ) ) ;
#4590 = CARTESIAN_POINT ( 'NONE',  ( 150.4572752258758612, 270.0473502708459250, 15.21885120838634187 ) ) ;
#4591 = CARTESIAN_POINT ( 'NONE',  ( 171.8543870755469243, 276.6897476962967630, 16.27073464812542980 ) ) ;
#4592 = ORIENTED_EDGE ( 'NONE', *, *, #75401, .T. ) ;
#4593 = CARTESIAN_POINT ( 'NONE',  ( 75.28832949877902081, 62.89817645449259942, -14.85265024749852003 ) ) ;
#4594 = LINE ( 'NONE', #12204, #86850 ) ;
#4595 = CARTESIAN_POINT ( 'NONE',  ( 155.6048174803203210, 261.1315455520403361, -17.38645169541727498 ) ) ;
#4596 = AXIS2_PLACEMENT_3D ( 'NONE', #87904, #48846, #2248 ) ;
#4597 = ORIENTED_EDGE ( 'NONE', *, *, #25713, .F. ) ;
#4598 = CARTESIAN_POINT ( 'NONE',  ( 195.4228050201512303, 292.1647680779090024, 16.44344289977338391 ) ) ;
#4599 = DIRECTION ( 'NONE',  ( -0.000000000000000000, 0.000000000000000000, -1.000000000000000000 ) ) ;
#4600 = CARTESIAN_POINT ( 'NONE',  ( 207.6357208050208101, 271.0113774299547913, -6.790259683043212036 ) ) ;
#4601 = CARTESIAN_POINT ( 'NONE',  ( 206.5523081671381931, 270.6640731400667050, 2.446578107278855274 ) ) ;
#4602 = VECTOR ( 'NONE', #6037, 1000.000000000000114 ) ;
#4603 = CARTESIAN_POINT ( 'NONE',  ( 200.1505510372172694, 283.2820884176684899, -16.95936656477399396 ) ) ;
#4604 = B_SPLINE_CURVE_WITH_KNOTS ( 'NONE', 3,
 ( #79775, #25532, #3255, #2246 ),
 .UNSPECIFIED., .F., .F.,
 ( 4, 4 ),
 ( 0.03120710976339495860, 0.04024459120465366524 ),
 .UNSPECIFIED. ) ;
#4605 = VECTOR ( 'NONE', #31513, 1000.000000000000227 ) ;
#4606 = CARTESIAN_POINT ( 'NONE',  ( 156.2224770818481545, 267.4677849582849376, -16.91854127892884208 ) ) ;
#4607 = CARTESIAN_POINT ( 'NONE',  ( 164.5259176133158689, 246.1953198488120051, 1.882264443804981813 ) ) ;
#4608 = CARTESIAN_POINT ( 'NONE',  ( -23.47208873469913115, 24.42380372261332155, 10.00000000000000000 ) ) ;
#4609 = CARTESIAN_POINT ( 'NONE',  ( 164.4989226152910646, 245.7265035704120351, -6.575810094723514965 ) ) ;
#4610 = VECTOR ( 'NONE', #92711, 999.9999999999998863 ) ;
#4611 = CARTESIAN_POINT ( 'NONE',  ( 118.9560200436548314, 248.6744531367911293, 4.594050593750047540 ) ) ;
#4612 = ORIENTED_EDGE ( 'NONE', *, *, #79519, .T. ) ;
#4613 = CARTESIAN_POINT ( 'NONE',  ( 81.51908546427152658, 44.28658535684733266, -9.904776572929741008 ) ) ;
#4614 = CARTESIAN_POINT ( 'NONE',  ( 183.7243390097106328, 259.3199907679909870, 6.356928255902579039 ) ) ;
#4615 = CARTESIAN_POINT ( 'NONE',  ( 203.3041373168503299, 278.5139001086923827, -16.61929732091214973 ) ) ;
#4616 = CARTESIAN_POINT ( 'NONE',  ( 204.9608076533459950, 275.6444629144898499, 14.31488288944633069 ) ) ;
#4617 = CARTESIAN_POINT ( 'NONE',  ( 74.48086480164226941, 59.59897794796569315, 15.66551120389625140 ) ) ;
#4618 = CYLINDRICAL_SURFACE ( 'NONE', #72911, 17.82106496071139645 ) ;
#4619 = VERTEX_POINT ( 'NONE', #53035 ) ;
#4620 = CARTESIAN_POINT ( 'NONE',  ( 76.83839478644495102, 56.36739346141288109, 16.18311125838449627 ) ) ;
#4621 = AXIS2_PLACEMENT_3D ( 'NONE', #87595, #71332, #80969 ) ;
#4622 =( BOUNDED_CURVE ( )  B_SPLINE_CURVE ( 2, ( #31584, #22005, #52901, #55868, #3233, #17397, #87872, #80247, #9306, #79749, #9825, #78718, #1209 ),
 .UNSPECIFIED., .F., .T. ) 
 B_SPLINE_CURVE_WITH_KNOTS ( ( 3, 2, 2, 2, 2, 2, 3 ),
 ( 0.2874999999999999778, 0.2899999999999999800, 0.2949999999999999845, 0.2999999999999999889, 0.3049999999999999933, 0.3099999999999999978, 0.3125000000000000000 ),
 .UNSPECIFIED. ) 
 CURVE ( )  GEOMETRIC_REPRESENTATION_ITEM ( )  RATIONAL_B_SPLINE_CURVE ( ( 0.9755282581475768211, 0.9755282581475768211, 1.000000000000000000, 0.9510565162951535312, 1.000000000000000000, 0.9510565162951535312, 1.000000000000000000, 0.9510565162951535312, 1.000000000000000000, 0.9510565162951535312, 1.000000000000000000, 0.9755282581475768211, 0.9755282581475768211 ) ) 
 REPRESENTATION_ITEM ( '' )  );
#4623 = CARTESIAN_POINT ( 'NONE',  ( 182.4292202362132116, 275.0433250554996221, -17.33419130812088582 ) ) ;
#4624 = CARTESIAN_POINT ( 'NONE',  ( 167.5904688695373750, 249.2039005190006549, -5.515356433798250357 ) ) ;
#4625 = CARTESIAN_POINT ( 'NONE',  ( 1.023347710557717782, 26.18841396516313935, 177.5919119679930134 ) ) ;
#4626 = CARTESIAN_POINT ( 'NONE',  ( 198.5413888763568195, 266.2629941491867953, 0.8512800372524856884 ) ) ;
#4627 = CARTESIAN_POINT ( 'NONE',  ( 190.6954410837624607, 300.3528026016029457, -5.728531842148099962 ) ) ;
#4628 = CARTESIAN_POINT ( 'NONE',  ( 68.45839193658751753, 69.34571607991892961, 4.633211366208406012 ) ) ;
#4629 = CARTESIAN_POINT ( 'NONE',  ( 157.2104826425669728, 258.3504519110855995, -16.92635148710569482 ) ) ;
#4630 = CARTESIAN_POINT ( 'NONE',  ( 170.7941491505363842, 250.2313031156421914, 4.188098645002056308 ) ) ;
#4631 = B_SPLINE_CURVE_WITH_KNOTS ( 'NONE', 3,
 ( #53069, #84024, #7983, #1385, #8969, #47953, #2390, #38859, #25163, #87552, #70260, #55548, #9986, #62148, #71289, #78896, #79420, #373, #17571, #33270, #94608, #32763, #40846, #77889, #93604, #48478 ),
 .UNSPECIFIED., .F., .F.,
 ( 4, 2, 2, 2, 2, 2, 2, 2, 2, 2, 2, 2, 4 ),
 ( 0.0003107992373423731349, 0.002113324222800152651, 0.002338639845982365319, 0.002451297657573469919, 0.002563955469164574084, 0.002592119922062337441, 0.002620284374960100797, 0.002676613280755630545, 0.002789271092346726905, 0.003014586715528822913, 0.003465217961892969826, 0.003690533585075043716, 0.003915849208257117173 ),
 .UNSPECIFIED. ) ;
#4632 = CARTESIAN_POINT ( 'NONE',  ( 17.48767303752208235, 28.83478043621388309, -8.090169943749479842 ) ) ;
#4633 = CARTESIAN_POINT ( 'NONE',  ( 190.3572031550745294, 300.9386478791372497, 3.093832330100951378 ) ) ;
#4634 = DIRECTION ( 'NONE',  ( 0.000000000000000000, 0.000000000000000000, -1.000000000000000000 ) ) ;
#4635 = CARTESIAN_POINT ( 'NONE',  ( 41.24097861217908445, 35.76159833115055164, -9.594050593750004907 ) ) ;
#4636 = CARTESIAN_POINT ( 'NONE',  ( 155.0453531195792038, 262.1005662498678817, -18.46987289964740953 ) ) ;
#4637 = CARTESIAN_POINT ( 'NONE',  ( 194.9146483705927153, 289.3315033412051207, 16.17650949137597749 ) ) ;
#4638 = B_SPLINE_CURVE_WITH_KNOTS ( 'NONE', 3,
 ( #14535, #70204, #31693, #37806, #100142, #84957, #14031, #75855, #6437, #61607, #53996, #68215, #29727, #60601, #57007, #16515 ),
 .UNSPECIFIED., .F., .F.,
 ( 4, 2, 2, 2, 2, 2, 2, 4 ),
 ( 3.925231146709437917E-17, 0.0003558565760979790437, 0.0007117131521959188393, 0.001067569728293858581, 0.001423426304391798430, 0.001779282880489738280, 0.002135139456587678130, 0.002846852608783629387 ),
 .UNSPECIFIED. ) ;
#4639 = CARTESIAN_POINT ( 'NONE',  ( 133.7328388157766312, 238.0177522451417929, 5.000000000000051514 ) ) ;
#4640 = CARTESIAN_POINT ( 'NONE',  ( 172.6748435171904532, 283.7256293223668422, -12.33524359727445763 ) ) ;
#4641 = VERTEX_POINT ( 'NONE', #69732 ) ;
#4642 = EDGE_CURVE ( 'NONE', #14677, #64537, #68885, .T. ) ;
#4643 = PLANE ( 'NONE',  #42733 ) ;
#4644 = CARTESIAN_POINT ( 'NONE',  ( 198.7829547491859330, 286.3448180261817129, -18.59838968157616179 ) ) ;
#4645 = CARTESIAN_POINT ( 'NONE',  ( -14.92600794870450898, 168.3149278399161233, 9.188101187500093303 ) ) ;
#4646 = VECTOR ( 'NONE', #2655, 1000.000000000000000 ) ;
#4647 = CARTESIAN_POINT ( 'NONE',  ( 45.77687342386973057, 206.4244531367911293, -4.594050593750046652 ) ) ;
#4648 = CARTESIAN_POINT ( 'NONE',  ( 178.6152369244925637, 259.3283413532399777, -10.64205949810462926 ) ) ;
#4649 = CARTESIAN_POINT ( 'NONE',  ( 19.14394661871191161, 29.79103043416549212, 8.090169943749478065 ) ) ;
#4650 = CARTESIAN_POINT ( 'NONE',  ( 85.35014107232977665, 49.09618135595809463, 12.41884494283699070 ) ) ;
#4651 = CARTESIAN_POINT ( 'NONE',  ( 204.6470611188870521, 276.1878878528713130, -13.02652554726987866 ) ) ;
#4652 = CARTESIAN_POINT ( 'NONE',  ( 192.6054495295585696, 292.3993297283804509, -14.32894417406807364 ) ) ;
#4653 = CARTESIAN_POINT ( 'NONE',  ( 150.0179852530401092, 276.4561033902535883, 3.706981700497388843 ) ) ;
#4655 = CARTESIAN_POINT ( 'NONE',  ( 76.57516216600367898, 205.0177522451417929, 5.000000000000051514 ) ) ;
#4654 = CARTESIAN_POINT ( 'NONE',  ( 74.91528014208350328, 207.3927522451418213, 10.00000000000009948 ) ) ;
#4656 = CARTESIAN_POINT ( 'NONE',  ( 179.0862785926605341, 254.3646952837514448, -4.132455289343337945 ) ) ;
#4657 = ADVANCED_FACE ( 'NONE', ( #85487 ), #14528, .F. ) ;
#4658 = CARTESIAN_POINT ( 'NONE',  ( 157.1965120183049578, 258.3746497421212780, -18.06591467563559306 ) ) ;
#4659 = CARTESIAN_POINT ( 'NONE',  ( 198.1444248750829047, 287.4507842102791528, 18.42558436659502519 ) ) ;
#4660 = EDGE_CURVE ( 'NONE', #76868, #60705, #9517, .T. ) ;
#4661 = CARTESIAN_POINT ( 'NONE',  ( 36.39519187313601378, 198.4865022471902876, 10.00000000000009237 ) ) ;
#4662 = CARTESIAN_POINT ( 'NONE',  ( 181.7016834730597736, 291.7820365442338471, 9.111168900057094788 ) ) ;
#4663 = FACE_OUTER_BOUND ( 'NONE', #68106, .T. ) ;
#4664 = AXIS2_PLACEMENT_3D ( 'NONE', #7336, #78258, #23523 ) ;
#4665 = CARTESIAN_POINT ( 'NONE',  ( -1.313257906909115480, 179.2369531367911293, -4.594050593750048428 ) ) ;
#4666 = CARTESIAN_POINT ( 'NONE',  ( 72.69493809724967548, 71.16443809380129437, -7.267007365939472052 ) ) ;
#4667 = CARTESIAN_POINT ( 'NONE',  ( 79.24135755033685768, 59.96798256686211204, 16.14279214841722521 ) ) ;
#4668 = CARTESIAN_POINT ( 'NONE',  ( 37.36761971798259196, 27.28920272979929607, -7.433330006724141015 ) ) ;
#4669 = CARTESIAN_POINT ( 'NONE',  ( 79.76863084600667264, 216.8615022471902591, -10.00000000000009592 ) ) ;
#4671 = CARTESIAN_POINT ( 'NONE',  ( 164.3706594650489023, 245.9486618633701482, -1.665857659249071698 ) ) ;
#4670 = AXIS2_PLACEMENT_3D ( 'NONE', #92154, #70284, #895 ) ;
#4672 = LINE ( 'NONE', #49771, #7671 ) ;
#4673 = CARTESIAN_POINT ( 'NONE',  ( 153.5916109235682541, 265.1562792198043326, -16.36868264138671591 ) ) ;
#4674 = CARTESIAN_POINT ( 'NONE',  ( 176.4634627281214421, 260.3851565349380053, -13.39184936855075136 ) ) ;
#4675 = CARTESIAN_POINT ( 'NONE',  ( 0.000000000000000000, 0.000000000000000000, 0.000000000000000000 ) ) ;
#4676 = VECTOR ( 'NONE', #52790, 1000.000000000000000 ) ;
#4677 = CARTESIAN_POINT ( 'NONE',  ( 12.79778405566451482, 30.49540643055186351, 3.479690158560446702E-15 ) ) ;
#4678 = CARTESIAN_POINT ( 'NONE',  ( 71.55389639452420170, 72.40420208557203807, 1.000837480472094088 ) ) ;
#4679 = CARTESIAN_POINT ( 'NONE',  ( 82.40357584069326435, 53.81685777417738592, 15.85384499771503819 ) ) ;
#4680 = CYLINDRICAL_SURFACE ( 'NONE', #36010, 3.300000000000010925 ) ;
#4681 = CARTESIAN_POINT ( 'NONE',  ( 193.7706395672514645, 295.0264025848412075, 15.16938698680137065 ) ) ;
#4682 = VERTEX_POINT ( 'NONE', #72775 ) ;
#4683 = CIRCLE ( 'NONE', #98485, 17.82106496071138224 ) ;
#4684 = CARTESIAN_POINT ( 'NONE',  ( 156.7410793263471760, 276.7253777054597208, 11.42669515405709646 ) ) ;
#4685 = CARTESIAN_POINT ( 'NONE',  ( 75.15016756581449897, 53.62953826938981905, -16.54102740569554086 ) ) ;
#4686 = CARTESIAN_POINT ( 'NONE',  ( 81.35004932177496073, 42.10696970585722454, 7.989028237409868005 ) ) ;
#4687 = CARTESIAN_POINT ( 'NONE',  ( 168.0561721676931199, 250.9850586709442837, -10.23605044211346105 ) ) ;
#4688 = EDGE_LOOP ( 'NONE', ( #46285, #11240, #56332, #33994 ) ) ;
#4689 = CARTESIAN_POINT ( 'NONE',  ( 192.7259387352017939, 296.8358775046606297, 11.24705370801146209 ) ) ;
#4690 = CARTESIAN_POINT ( 'NONE',  ( 1.813001633210440611, 27.74720351945397923, 10.00000000000000000 ) ) ;
#4691 = DIRECTION ( 'NONE',  ( 0.9598361373656965068, -0.2805612043866717031, 0.000000000000000000 ) ) ;
#4692 = CARTESIAN_POINT ( 'NONE',  ( 155.2922060645262263, 261.6730044072216401, -16.98884022075611355 ) ) ;
#4693 = ORIENTED_EDGE ( 'NONE', *, *, #39398, .T. ) ;
#4694 = CIRCLE ( 'NONE', #61360, 70.00000000000001421 ) ;
#4695 = ORIENTED_EDGE ( 'NONE', *, *, #22610, .F. ) ;
#4696 = EDGE_CURVE ( 'NONE', #44705, #30119, #60256, .T. ) ;
#4698 = DIRECTION ( 'NONE',  ( -0.000000000000000000, -0.000000000000000000, -1.000000000000000000 ) ) ;
#4697 = CARTESIAN_POINT ( 'NONE',  ( 159.7794170132337683, 278.5358178951433956, -9.739126798237956351 ) ) ;
#4699 = CARTESIAN_POINT ( 'NONE',  ( 192.7944000592152634, 296.7172990131160759, 11.44860011299869740 ) ) ;
#4700 = ORIENTED_EDGE ( 'NONE', *, *, #31697, .F. ) ;
#4701 = CARTESIAN_POINT ( 'NONE',  ( 191.5281967176683509, 298.9104275333885994, 7.715154960566919407 ) ) ;
#4702 = CARTESIAN_POINT ( 'NONE',  ( 80.75322455565131463, 57.27148952657292824, 16.56885343786527898 ) ) ;
#4703 = DIRECTION ( 'NONE',  ( 1.000000000000000000, 0.000000000000000000, 0.000000000000000000 ) ) ;
#4704 = VERTEX_POINT ( 'NONE', #35735 ) ;
#4705 = DIRECTION ( 'NONE',  ( -0.8660254037844377084, -0.5000000000000014433, -0.000000000000000000 ) ) ;
#4706 = CARTESIAN_POINT ( 'NONE',  ( 76.73837805473348794, 50.85003728428209513, -15.44848974388898810 ) ) ;
#4707 = ADVANCED_FACE ( 'NONE', ( #4336 ), #34241, .T. ) ;
#4708 = EDGE_CURVE ( 'NONE', #79972, #88994, #85629, .T. ) ;
#4709 = AXIS2_PLACEMENT_3D ( 'NONE', #93260, #47616, #9650 ) ;
#4710 = CARTESIAN_POINT ( 'NONE',  ( 80.96449997289272460, 43.55881912823607394, 9.398159779699934546 ) ) ;
#4711 = ORIENTED_EDGE ( 'NONE', *, *, #58928, .F. ) ;
#4712 = CARTESIAN_POINT ( 'NONE',  ( 177.5778721735796069, 268.8026387624398694, 16.30278465327989323 ) ) ;
#4713 = CARTESIAN_POINT ( 'NONE',  ( 205.8030308266901898, 274.1856895869457844, 10.55961490432110317 ) ) ;
#4714 = EDGE_CURVE ( 'NONE', #59587, #2096, #71626, .T. ) ;
#4715 = CARTESIAN_POINT ( 'NONE',  ( 73.69818273017419585, 59.72407691843551447, 15.50369470924484716 ) ) ;
#4716 = B_SPLINE_SURFACE_WITH_KNOTS ( 'NONE', 3, 1, ( 
 ( #71471, #2064 ),
 ( #63848, #94787 ),
 ( #87729, #80097 ),
 ( #10663, #88213 ),
 ( #41539, #33977 ),
 ( #95808, #26362 ),
 ( #49642, #80600 ),
 ( #56905, #49326 ),
 ( #42204, #87891 ),
 ( #64525, #95969 ),
 ( #25524, #65512 ),
 ( #57405, #10333 ),
 ( #58402, #73624 ),
 ( #4209, #96461 ),
 ( #56412, #41708 ),
 ( #41199, #81261 ),
 ( #48835, #73139 ),
 ( #3734, #18436 ),
 ( #72652, #80265 ),
 ( #35106, #10828 ),
 ( #79768, #88386 ),
 ( #72137, #2742 ),
 ( #87407, #34612 ),
 ( #27027, #94959 ),
 ( #88890, #34130 ),
 ( #57911, #96965 ),
 ( #19452, #17937 ),
 ( #33631, #95482 ),
 ( #26034, #18940 ),
 ( #64019, #3247 ),
 ( #66016, #49817 ),
 ( #65023, #26532 ),
 ( #27531, #80776 ),
 ( #19930, #11348 ) ),
 .UNSPECIFIED., .T., .F., .F.,
 ( 4, 2, 2, 2, 2, 2, 2, 2, 2, 2, 2, 2, 2, 2, 2, 2, 4 ),
 ( 2, 2 ),
 ( 0.000000000000000000, 0.06250000000000000000, 0.1250000000000000000, 0.1875000000000000000, 0.2500000000000000000, 0.3125000000000000000, 0.3750000000000000000, 0.4375000000000000000, 0.5000000000000000000, 0.5625000000000000000, 0.6250000000000000000, 0.6875000000000000000, 0.7500000000000000000, 0.8125000000000000000, 0.8750000000000000000, 0.9375000000000000000, 1.000000000000000000 ),
 ( 0.000000000000000000, 1.000000000000000000 ),
 .UNSPECIFIED. ) ;
#4717 = ORIENTED_EDGE ( 'NONE', *, *, #51666, .T. ) ;
#4718 = EDGE_CURVE ( 'NONE', #53015, #66626, #47739, .T. ) ;
#4719 = CARTESIAN_POINT ( 'NONE',  ( 190.0607312434325138, 301.4521522931182176, 3.538147641957853473 ) ) ;
#4720 = DIRECTION ( 'NONE',  ( -0.8660254037844387076, -0.4999999999999998890, -0.000000000000000000 ) ) ;
#4721 = EDGE_CURVE ( 'NONE', #84236, #56021, #54148, .T. ) ;
#4722 = ORIENTED_EDGE ( 'NONE', *, *, #83014, .T. ) ;
#4723 = CARTESIAN_POINT ( 'NONE',  ( 47.89168550319195106, 74.68847913791599069, 177.5919119679930134 ) ) ;
#4724 = ORIENTED_EDGE ( 'NONE', *, *, #56609, .F. ) ;
#4725 = CARTESIAN_POINT ( 'NONE',  ( 157.2786326963988586, 269.2986199873796522, 15.63648806844084405 ) ) ;
#4726 = ORIENTED_EDGE ( 'NONE', *, *, #13893, .T. ) ;
#4727 = CARTESIAN_POINT ( 'NONE',  ( 87.11349487006070547, 46.19076519147612458, 8.411924245371466213 ) ) ;
#4728 = CARTESIAN_POINT ( 'NONE',  ( 190.3286155001717930, 300.9881631498979004, -5.624828231725103045 ) ) ;
#4729 = DIRECTION ( 'NONE',  ( -0.8660254037844379305, -0.5000000000000014433, 0.000000000000000000 ) ) ;
#4730 = CARTESIAN_POINT ( 'NONE',  ( 19.66861660350102881, 11.75978393459163662, -1.583844403245362020 ) ) ;
#4731 = CARTESIAN_POINT ( 'NONE',  ( 153.0070714074088016, 265.6309737354857248, 17.74442213480098474 ) ) ;
#4732 = DIRECTION ( 'NONE',  ( -1.000000000000000000, 0.000000000000000000, 0.000000000000000000 ) ) ;
#4733 = CARTESIAN_POINT ( 'NONE',  ( 197.4537186060251486, 288.6471225613934166, -18.22696722856148455 ) ) ;
#4734 = VERTEX_POINT ( 'NONE', #13267 ) ;
#4735 = B_SPLINE_CURVE_WITH_KNOTS ( 'NONE', 3,
 ( #99023, #98026, #82858, #67602 ),
 .UNSPECIFIED., .F., .F.,
 ( 4, 4 ),
 ( 0.003963300069783955853, 0.01194164548429975728 ),
 .UNSPECIFIED. ) ;
#4736 = CARTESIAN_POINT ( 'NONE',  ( 164.9617201910520237, 244.9249146555742414, 2.745022583679548767 ) ) ;
#4738 = FACE_OUTER_BOUND ( 'NONE', #58855, .T. ) ;
#4737 = CARTESIAN_POINT ( 'NONE',  ( 196.6800254274587019, 289.9871984561398222, -17.90749311895638129 ) ) ;
#4740 = VERTEX_POINT ( 'NONE', #65451 ) ;
#4739 = CARTESIAN_POINT ( 'NONE',  ( 159.8416255366773839, 253.7931787365127434, 16.77980437810719394 ) ) ;
#4741 = CARTESIAN_POINT ( 'NONE',  ( 87.86298961015023679, 44.89260222163544256, 6.207647304897665919 ) ) ;
#4742 = VERTEX_POINT ( 'NONE', #96901 ) ;
#4743 = CARTESIAN_POINT ( 'NONE',  ( 186.9332467140213794, 276.6677885244452000, 17.67048876257000600 ) ) ;
#4744 = CARTESIAN_POINT ( 'NONE',  ( 200.5039526449628795, 267.3497397166782434, 6.370409075474873006 ) ) ;
#4745 = CARTESIAN_POINT ( 'NONE',  ( 164.0532584536765626, 247.8859213503266972, 8.571009476567882146 ) ) ;
#4746 = CARTESIAN_POINT ( 'NONE',  ( 15.99984526765731907, 17.43677371833800649, -10.00000000000000355 ) ) ;
#4747 = CARTESIAN_POINT ( 'NONE',  ( 199.3272761551183692, 285.4020256954596562, -18.33026947811089258 ) ) ;
#4748 = CARTESIAN_POINT ( 'NONE',  ( 148.0167748296930199, 274.2744209529264481, -10.15233092020212347 ) ) ;
#4749 = ORIENTED_EDGE ( 'NONE', *, *, #8795, .F. ) ;
#4750 = CARTESIAN_POINT ( 'NONE',  ( 170.3593749743948536, 255.4184166931929951, -11.62125758648799057 ) ) ;
#4751 = CARTESIAN_POINT ( 'NONE',  ( 183.3634088509504352, 284.6525016221286251, -16.42631288611494256 ) ) ;
#4752 = CARTESIAN_POINT ( 'NONE',  ( 125.8664413980679342, 250.1427522451419350, 10.00000000000009415 ) ) ;
#4754 = EDGE_CURVE ( 'NONE', #64642, #50553, #91712, .T. ) ;
#4753 = CARTESIAN_POINT ( 'NONE',  ( 207.6209998424140792, 271.0368748851258260, 6.610167240481342965 ) ) ;
#4755 = CARTESIAN_POINT ( 'NONE',  ( 38.54221318313706490, 186.3927522451418213, 10.00000000000009592 ) ) ;
#4756 = CARTESIAN_POINT ( 'NONE',  ( 94.19319292813476352, 231.3149278399160949, 9.188101187500093303 ) ) ;
#4757 = CARTESIAN_POINT ( 'NONE',  ( 182.4111744044705006, 295.1865784113461473, -2.664051097989806660 ) ) ;
#4758 = CIRCLE ( 'NONE', #61336, 17.82106496071138935 ) ;
#4759 = CARTESIAN_POINT ( 'NONE',  ( 167.6233549396688147, 282.5614550147377031, -10.64682312388593211 ) ) ;
#4760 = CARTESIAN_POINT ( 'NONE',  ( 195.8627871995700502, 291.4026965887302936, 17.41145040657729481 ) ) ;
#4761 = CARTESIAN_POINT ( 'NONE',  ( 163.1968603775171118, 247.9817415208531202, 11.27455733958931994 ) ) ;
#4762 = CARTESIAN_POINT ( 'NONE',  ( 13.65283037618196893, 184.8149278399160664, 9.188101187500093303 ) ) ;
#4763 = DIRECTION ( 'NONE',  ( 0.8660254037844363761, 0.5000000000000039968, 0.000000000000000000 ) ) ;
#4764 = VERTEX_POINT ( 'NONE', #97866 ) ;
#4765 = VECTOR ( 'NONE', #49586, 1000.000000000000000 ) ;
#4766 = VERTEX_POINT ( 'NONE', #96396 ) ;
#4767 = DIRECTION ( 'NONE',  ( -0.8660254037844387076, -0.4999999999999998890, -0.000000000000000000 ) ) ;
#4768 = CARTESIAN_POINT ( 'NONE',  ( 185.1461160444276004, 259.9246127725722886, -5.696222747182419610 ) ) ;
#4769 = CARTESIAN_POINT ( 'NONE',  ( 71.45648812236639458, 71.78579786804675678, -2.123707775780323992 ) ) ;
#4770 = FACE_OUTER_BOUND ( 'NONE', #56164, .T. ) ;
#4771 = CARTESIAN_POINT ( 'NONE',  ( 5.882932626810616128, 22.13478043621385893, 8.090169943749478065 ) ) ;
#4772 = AXIS2_PLACEMENT_3D ( 'NONE', #91117, #15549, #68267 ) ;
#4773 = LINE ( 'NONE', #43740, #22282 ) ;
#4774 = CARTESIAN_POINT ( 'NONE',  ( 168.1671718393196500, 251.7577310522514153, 10.56854090917195421 ) ) ;
#4775 = CARTESIAN_POINT ( 'NONE',  ( 49.48463145776311478, 205.5024278399160949, -9.188101187500093303 ) ) ;
#4776 = CARTESIAN_POINT ( 'NONE',  ( 90.50373741020339935, 216.3927522451417929, 10.00000000000009592 ) ) ;
#4777 = B_SPLINE_CURVE_WITH_KNOTS ( 'NONE', 3,
 ( #15994, #71215, #46893, #32690, #86960, #17495, #12409, #97042, #56981, #42770 ),
 .UNSPECIFIED., .F., .F.,
 ( 4, 2, 2, 2, 4 ),
 ( 0.000000000000000000, 0.2500000000000000000, 0.5000000000000000000, 0.7500000000000000000, 1.000000000000000000 ),
 .UNSPECIFIED. ) ;
#4778 = ORIENTED_EDGE ( 'NONE', *, *, #86915, .T. ) ;
#4779 = CARTESIAN_POINT ( 'NONE',  ( 79.11171798038404290, 59.41904482235663920, -16.53441574648432422 ) ) ;
#4780 = EDGE_CURVE ( 'NONE', #45021, #96468, #68694, .T. ) ;
#4781 = CARTESIAN_POINT ( 'NONE',  ( 162.6257765080958677, 248.9708877980734485, -10.42859054881151160 ) ) ;
#4782 = CIRCLE ( 'NONE', #33870, 0.1418229129683812317 ) ;
#4783 = CARTESIAN_POINT ( 'NONE',  ( -0.9884983804899494242, 179.4244531367911577, -4.594050593750046652 ) ) ;
#4784 = CARTESIAN_POINT ( 'NONE',  ( 150.7691137448031213, 269.5072301123068428, -15.63821625702598084 ) ) ;
#4785 = CARTESIAN_POINT ( 'NONE',  ( 81.00366901594098579, 53.98193135160821754, 16.09339324300580287 ) ) ;
#4786 = CARTESIAN_POINT ( 'NONE',  ( 147.1125781744767949, 275.8405354997948962, -5.216646253929903665 ) ) ;
#4787 = CARTESIAN_POINT ( 'NONE',  ( 73.29014998154374894, 69.82456558858999074, 9.114582937199678270 ) ) ;
#4788 = CARTESIAN_POINT ( 'NONE',  ( 51.40603854846860798, 209.6744531367911293, 4.594050593750047540 ) ) ;
#4789 = CARTESIAN_POINT ( 'NONE',  ( 208.0692320075777957, 270.2605140014760536, 2.043861372130216569 ) ) ;
#4790 = CARTESIAN_POINT ( 'NONE',  ( 72.52494868832852148, 57.36103174889360190, 16.32214684599243881 ) ) ;
#4791 = EDGE_CURVE ( 'NONE', #44920, #79399, #51857, .T. ) ;
#4792 = CARTESIAN_POINT ( 'NONE',  ( 68.30731939365449534, 66.71466498842660542, 9.194818449662610860 ) ) ;
#4793 = FACE_OUTER_BOUND ( 'NONE', #53542, .T. ) ;
#4794 = ORIENTED_EDGE ( 'NONE', *, *, #46383, .F. ) ;
#4795 = EDGE_CURVE ( 'NONE', #45744, #75611, #74883, .T. ) ;
#4796 = CARTESIAN_POINT ( 'NONE',  ( 3.125382611083852957, 172.6115022471902591, 10.00000000000009592 ) ) ;
#4797 = CARTESIAN_POINT ( 'NONE',  ( 82.66943193480358332, 42.37244407833836846, 7.179986229313780832 ) ) ;
#4798 = CARTESIAN_POINT ( 'NONE',  ( 125.9656734773588767, 243.5333772461660544, 9.188101187500095079 ) ) ;
#4799 = CARTESIAN_POINT ( 'NONE',  ( 21.78279761992806129, 35.68290643055188838, 3.479690158560446702E-15 ) ) ;
#4800 = CARTESIAN_POINT ( 'NONE',  ( 164.6112646021906869, 245.5319215412782796, 0.9047594026039291748 ) ) ;
#4801 = DIRECTION ( 'NONE',  ( 0.000000000000000000, -0.000000000000000000, 1.000000000000000000 ) ) ;
#4802 = DIRECTION ( 'NONE',  ( 0.5344452582589497291, -0.8452030915256549815, 0.000000000000000000 ) ) ;
#4804 = CARTESIAN_POINT ( 'NONE',  ( 189.3785535910650424, 289.8996385724929041, 14.46956945346604861 ) ) ;
#4803 = PLANE ( 'NONE',  #19375 ) ;
#4805 = CARTESIAN_POINT ( 'NONE',  ( 68.55513178119723250, 64.39780669069259034, 11.67030924314737916 ) ) ;
#4806 = ORIENTED_EDGE ( 'NONE', *, *, #51075, .F. ) ;
#4807 = B_SPLINE_CURVE_WITH_KNOTS ( 'NONE', 3,
 ( #9845, #79770, #17939, #87409, #72140, #56907, #18438, #49328, #3736, #32620, #18942, #65514, #80778, #3249, #25010, #34614, #10335, #49819, #80267, #95971, #79272, #63517, #86380, #71646, #11350, #33119, #56414, #40197, #34132, #48837, #41201, #55889, #78733, #64021, #71140, #1741, #42206, #65025, #2744, #9323, #33633, #40706, #94961, #86883, #64527, #26534 ),
 .UNSPECIFIED., .F., .F.,
 ( 4, 1, 1, 1, 2, 2, 1, 1, 1, 2, 2, 1, 1, 2, 2, 1, 1, 2, 2, 1, 1, 2, 2, 1, 2, 2, 1, 2, 2, 4 ),
 ( 0.000000000000000000, 0.06249999999997776778, 0.09374999999996665168, 0.1093749999999626965, 0.1171874999999631406, 0.1249999999999635847, 0.1874999999999612255, 0.2187499999999591438, 0.2343749999999581168, 0.2421874999999576172, 0.2499999999999570899, 0.3124999999999558131, 0.3437499999999572564, 0.3593749999999596434, 0.3749999999999620304, 0.4374999999999680256, 0.4687499999999711897, 0.4843749999999705791, 0.4999999999999700240, 0.5624999999999753530, 0.5937499999999779066, 0.6093749999999785727, 0.6249999999999791278, 0.6874999999999807931, 0.7187499999999830136, 0.7499999999999852340, 0.8124999999999895639, 0.8437499999999916733, 0.8749999999999936717, 1.000000000000000000 ),
 .UNSPECIFIED. ) ;
#4808 = CARTESIAN_POINT ( 'NONE',  ( 151.0715479399129606, 268.9833987204304435, 14.24612252017116987 ) ) ;
#4809 = CARTESIAN_POINT ( 'NONE',  ( 208.4115645851568388, 269.6675765840226973, -1.114383557117654133 ) ) ;
#4810 = CARTESIAN_POINT ( 'NONE',  ( 151.3433504153738909, 269.1997824268871113, -14.27012659247592730 ) ) ;
#4811 = CARTESIAN_POINT ( 'NONE',  ( 172.7592676337296211, 268.7804561342234138, -17.20143128700372159 ) ) ;
#4812 = CARTESIAN_POINT ( 'NONE',  ( 4.600586583810874153, 20.84336893147753500, -7.433330006724137462 ) ) ;
#4813 = ORIENTED_EDGE ( 'NONE', *, *, #76838, .F. ) ;
#4814 = CARTESIAN_POINT ( 'NONE',  ( 70.50125601336765158, 69.59879263790479342, 6.833936649965831833 ) ) ;
#4815 = LINE ( 'NONE', #60466, #61975 ) ;
#4816 = CARTESIAN_POINT ( 'NONE',  ( 77.55425247552874168, 49.72899633274018782, 14.94892306696621631 ) ) ;
#4817 = CARTESIAN_POINT ( 'NONE',  ( 182.2606358067372412, 295.0231671335754982, 4.761058120652655212 ) ) ;
#4818 = CARTESIAN_POINT ( 'NONE',  ( 69.81003220229767692, 70.90474864260643528, 1.346364422161295815 ) ) ;
#4819 = CARTESIAN_POINT ( 'NONE',  ( 148.6181070846184866, 274.7356907660122260, -7.901608801242418600 ) ) ;
#4820 = ORIENTED_EDGE ( 'NONE', *, *, #24292, .T. ) ;
#4821 = EDGE_CURVE ( 'NONE', #92014, #20280, #94267, .T. ) ;
#4822 = FACE_OUTER_BOUND ( 'NONE', #53550, .T. ) ;
#4823 = CARTESIAN_POINT ( 'NONE',  ( 9.667034506031535912, 13.78052372038638218, -10.00000000000000355 ) ) ;
#4824 = CYLINDRICAL_SURFACE ( 'NONE', #62737, 10.00000000000010658 ) ;
#4825 = ORIENTED_EDGE ( 'NONE', *, *, #6143, .F. ) ;
#4826 = CARTESIAN_POINT ( 'NONE',  ( 66.10228174255657052, 68.64626758096548542, 4.271897712742703135 ) ) ;
#4827 = CARTESIAN_POINT ( 'NONE',  ( 86.28449982416978514, 46.95005333036156969, -10.54182221192812818 ) ) ;
#4828 = CARTESIAN_POINT ( 'NONE',  ( 158.7054080432568526, 263.5240239109023150, -17.05492894054507147 ) ) ;
#4829 = ORIENTED_EDGE ( 'NONE', *, *, #29214, .T. ) ;
#4830 = VECTOR ( 'NONE', #48570, 1000.000000000000227 ) ;
#4831 = DIRECTION ( 'NONE',  ( -0.8261602328994366307, 0.5634352399127593447, 0.000000000000000000 ) ) ;
#4832 = CARTESIAN_POINT ( 'NONE',  ( 184.9393937902272853, 291.8736057701431719, 12.09585067037464690 ) ) ;
#4833 = CARTESIAN_POINT ( 'NONE',  ( 204.3276935076901850, 276.7410487817560920, 13.46217427333259309 ) ) ;
#4834 = CARTESIAN_POINT ( 'NONE',  ( 74.73487060833782891, 53.69418506457893869, 16.08953207461605928 ) ) ;
#4835 = EDGE_LOOP ( 'NONE', ( #60725, #46809, #97039, #22506 ) ) ;
#4836 = CARTESIAN_POINT ( 'NONE',  ( 81.52757139778736928, 224.0024278399161233, 9.188101187500095079 ) ) ;
#4837 = AXIS2_PLACEMENT_3D ( 'NONE', #12393, #43258, #25589 ) ;
#4838 = CARTESIAN_POINT ( 'NONE',  ( 203.4656741260425861, 278.2341101478789369, 15.04751411186255794 ) ) ;
#4839 = B_SPLINE_CURVE_WITH_KNOTS ( 'NONE', 3,
 ( #43033, #87743, #80614, #88727, #17781, #34465, #41046, #57254, #25888, #11191, #3585, #89232, #4559, #18284, #49178, #10677 ),
 .UNSPECIFIED., .F., .F.,
 ( 4, 1, 2, 2, 2, 1, 2, 2, 4 ),
 ( 0.000000000000000000, 0.1250000000000006661, 0.1875000000000011102, 0.2500000000000015543, 0.5000000000000035527, 0.6250000000000026645, 0.6875000000000022204, 0.7500000000000017764, 1.000000000000000000 ),
 .UNSPECIFIED. ) ;
#4840 = CARTESIAN_POINT ( 'NONE',  ( 84.75777273949843504, 49.85283236070215196, -13.16649314506352475 ) ) ;
#4841 = CARTESIAN_POINT ( 'NONE',  ( 185.0661581905127946, 259.9867678767801067, -5.962180284922311557 ) ) ;
#4842 = ORIENTED_EDGE ( 'NONE', *, *, #83291, .T. ) ;
#4843 = ADVANCED_FACE ( 'NONE', ( #98367, #90798 ), #22832, .F. ) ;
#4844 = VERTEX_POINT ( 'NONE', #38524 ) ;
#4845 = CARTESIAN_POINT ( 'NONE',  ( 88.46339282683516103, 43.84930607083626342, 0.06358566718628017034 ) ) ;
#4846 = ORIENTED_EDGE ( 'NONE', *, *, #78162, .F. ) ;
#4847 = DIRECTION ( 'NONE',  ( 0.8660254037844387076, 0.4999999999999998890, 0.000000000000000000 ) ) ;
#4848 = ORIENTED_EDGE ( 'NONE', *, *, #72790, .T. ) ;
#4849 = DIRECTION ( 'NONE',  ( 0.000000000000000000, -0.000000000000000000, -1.000000000000000000 ) ) ;
#4850 = CARTESIAN_POINT ( 'NONE',  ( 155.0619429961492983, 262.0718317407570339, -17.08853361476647592 ) ) ;
#4851 = ORIENTED_EDGE ( 'NONE', *, *, #47272, .F. ) ;
#4852 = CARTESIAN_POINT ( 'NONE',  ( 166.1309782654906257, 249.2029336093187339, -9.347746458946922132 ) ) ;
#4853 = FACE_OUTER_BOUND ( 'NONE', #2335, .T. ) ;
#4854 = CARTESIAN_POINT ( 'NONE',  ( 152.0427391285763008, 268.8460936103824679, 15.18634991826209379 ) ) ;
#4855 = DIRECTION ( 'NONE',  ( -0.5906904945688551400, 0.000000000000000000, 0.8068982213550859317 ) ) ;
#4856 = CARTESIAN_POINT ( 'NONE',  ( 194.3708539535661259, 293.9868007723104029, -16.01585187499628304 ) ) ;
#4857 = CARTESIAN_POINT ( 'NONE',  ( 133.1643360984345179, 253.8149278399160949, 9.188101187500093303 ) ) ;
#4858 = CARTESIAN_POINT ( 'NONE',  ( 168.2960286251776836, 267.1807326767980157, -17.13187780290563822 ) ) ;
#4859 = ORIENTED_EDGE ( 'NONE', *, *, #65273, .T. ) ;
#4860 = CARTESIAN_POINT ( 'NONE',  ( 77.05881501368067177, 62.08228305079084919, 15.47689417538831869 ) ) ;
#4861 = CARTESIAN_POINT ( 'NONE',  ( 12.18311320154372801, 9.960047579820882291, -5.678558825948276656 ) ) ;
#4862 = EDGE_CURVE ( 'NONE', #74723, #66013, #40873, .T. ) ;
#4863 = ORIENTED_EDGE ( 'NONE', *, *, #15300, .T. ) ;
#4864 = VECTOR ( 'NONE', #2325, 1000.000000000000000 ) ;
#4865 = CARTESIAN_POINT ( 'NONE',  ( 167.4640555680685452, 284.2325975850394570, 9.238334356205527342 ) ) ;
#4867 = ORIENTED_EDGE ( 'NONE', *, *, #61947, .T. ) ;
#4866 = CARTESIAN_POINT ( 'NONE',  ( 82.41933087055697627, 40.38430946167127900, -0.8419157719606891188 ) ) ;
#4868 = CARTESIAN_POINT ( 'NONE',  ( 78.13885432066443570, 47.60678095579073243, -13.89854567155110665 ) ) ;
#4869 = CARTESIAN_POINT ( 'NONE',  ( 76.18015836404990182, 65.31175638499995273, -14.08199309598906801 ) ) ;
#4870 = CARTESIAN_POINT ( 'NONE',  ( 159.4915328267279904, 280.5121072581201247, -6.654986942288538820 ) ) ;
#4871 = CARTESIAN_POINT ( 'NONE',  ( 77.49342303783743091, 51.34850931301296839, -15.95500110091012047 ) ) ;
#4872 = CARTESIAN_POINT ( 'NONE',  ( -58.62427208439002158, 70.56504152958493137, 60.00000000000000000 ) ) ;
#4873 = DIRECTION ( 'NONE',  ( -1.000000000000000000, -0.000000000000000000, 5.984665299743594308E-16 ) ) ;
#4874 = DIRECTION ( 'NONE',  ( 0.000000000000000000, 1.000000000000000000, 0.000000000000000000 ) ) ;
#4875 = ORIENTED_EDGE ( 'NONE', *, *, #50491, .T. ) ;
#4876 = CARTESIAN_POINT ( 'NONE',  ( 182.2370137474378282, 271.6850240291627188, -16.00081368563178330 ) ) ;
#4877 = CARTESIAN_POINT ( 'NONE',  ( 66.42665093650496999, 68.92825192741007356, 0.05375612720383066145 ) ) ;
#4878 = ORIENTED_EDGE ( 'NONE', *, *, #87099, .T. ) ;
#4879 = CARTESIAN_POINT ( 'NONE',  ( 161.4789001435202636, 276.1860666989730362, 12.81388631890260932 ) ) ;
#4880 = CARTESIAN_POINT ( 'NONE',  ( 174.2334270921930113, 280.9505671044033761, -14.19419622416070048 ) ) ;
#4881 = CARTESIAN_POINT ( 'NONE',  ( -44.49648453423614569, 28.96346851210257967, -10.00000000000000000 ) ) ;
#4882 = CARTESIAN_POINT ( 'NONE',  ( 149.4539134692060145, 271.7852238117696402, 12.95627816374690688 ) ) ;
#4883 = CARTESIAN_POINT ( 'NONE',  ( 163.3241744239597040, 273.7201536836278706, 14.82517280019972361 ) ) ;
#4885 = CARTESIAN_POINT ( 'NONE',  ( 88.47356364199694667, 43.97712956045978672, 1.870819122003379187 ) ) ;
#4884 = DIRECTION ( 'NONE',  ( 0.000000000000000000, 0.000000000000000000, 1.000000000000000000 ) ) ;
#4886 = CARTESIAN_POINT ( 'NONE',  ( -62.83817737799399339, 37.97373922903764765, -10.00000000000000000 ) ) ;
#4887 = ORIENTED_EDGE ( 'NONE', *, *, #66450, .T. ) ;
#4889 = ORIENTED_EDGE ( 'NONE', *, *, #78442, .T. ) ;
#4888 = B_SPLINE_CURVE_WITH_KNOTS ( 'NONE', 3,
 ( #51577, #90629, #13585, #75391, #36870, #43958, #59144, #73395, #27290, #27786, #5973, #34867, #73889, #43465, #12598, #51063, #35871, #20688, #82534, #13097, #67776, #19211, #50569, #96724, #88647, #74408, #58172, #65766, #20193, #42950, #50083, #81039, #66284, #89157, #11602, #35371, #83015, #81519, #90114, #59657, #89631, #19703, #4994, #12088, #74896, #4479 ),
 .UNSPECIFIED., .F., .F.,
 ( 4, 2, 2, 2, 2, 2, 2, 2, 2, 2, 2, 2, 2, 2, 2, 2, 2, 2, 2, 2, 2, 2, 4 ),
 ( 0.001330336800848096928, 0.001796201410264788162, 0.002262066019681479179, 0.002494998324389811895, 0.002611464476743977168, 0.002727930629098142441, 0.002844396781452308148, 0.002960862933806473855, 0.003193795238514659553, 0.003659659847931111612, 0.004125524457347563671, 0.005057253676180531975, 0.005988982895013501145, 0.006454847504429985297, 0.006920712113846468581, 0.007037178266200548420, 0.007095411342377589206, 0.007153644418554628258, 0.007270110570908708963, 0.007386576723262788802, 0.007852441332679101216, 0.008318305942095415365, 0.008784170551511727779 ),
 .UNSPECIFIED. ) ;
#4890 = CARTESIAN_POINT ( 'NONE',  ( 22.61461015039527922, 36.55466486950700755, 7.012934429366973338E-14 ) ) ;
#4891 = CARTESIAN_POINT ( 'NONE',  ( 79.90415527835997977, 58.06450031769458775, 16.26805976162004441 ) ) ;
#4892 = DIRECTION ( 'NONE',  ( -0.000000000000000000, 0.000000000000000000, 1.000000000000000000 ) ) ;
#4893 = CARTESIAN_POINT ( 'NONE',  ( 173.4201897355620474, 289.8359727321131913, 2.578270883801049518 ) ) ;
#4894 = CARTESIAN_POINT ( 'NONE',  ( 152.8134625983922490, 265.9663140294953791, 17.57333028169644251 ) ) ;
#4895 = CARTESIAN_POINT ( 'NONE',  ( 80.68090781023890656, 43.23449616528987605, -9.208455255847814769 ) ) ;
#4896 = CARTESIAN_POINT ( 'NONE',  ( 41.75918455503629190, 206.4637435831424739, 2.679491924311251605 ) ) ;
#4897 = CARTESIAN_POINT ( 'NONE',  ( 5.155129649429669669, 173.7833772461660828, -9.188101187500095079 ) ) ;
#4898 = CARTESIAN_POINT ( 'NONE',  ( 97.41363812451689341, 236.2369531367911009, -4.594050593750048428 ) ) ;
#4899 = CARTESIAN_POINT ( 'NONE',  ( 87.64597162258272078, 44.36656289597981839, -4.061167644325248460 ) ) ;
#4900 = CARTESIAN_POINT ( 'NONE',  ( 180.4454643261772731, 254.9133515654937696, -2.466473243201257937 ) ) ;
#4902 = CARTESIAN_POINT ( 'NONE',  ( 78.88416877887701162, 55.54717536121699339, 16.10259716625749249 ) ) ;
#4901 = AXIS2_PLACEMENT_3D ( 'NONE', #25113, #76823, #92566 ) ;
#4903 = DIRECTION ( 'NONE',  ( -0.5000000000000011102, -0.8660254037844380415, -0.000000000000000000 ) ) ;
#4904 = CARTESIAN_POINT ( 'NONE',  ( 155.0898745997320134, 262.0234527842152374, 17.05457557403769542 ) ) ;
#4905 = CARTESIAN_POINT ( 'NONE',  ( 194.2389208611690492, 294.2153155915419802, -15.75132567904764791 ) ) ;
#4906 = CARTESIAN_POINT ( 'NONE',  ( 84.61344793860607183, 50.61789989419376212, 13.66347863740807078 ) ) ;
#4907 = CARTESIAN_POINT ( 'NONE',  ( 187.3930124382416693, 298.9285105704863668, -0.5915368864456632680 ) ) ;
#4908 = EDGE_CURVE ( 'NONE', #9648, #3492, #58643, .T. ) ;
#4909 = CARTESIAN_POINT ( 'NONE',  ( 200.1294354126899009, 267.3366221627135246, -6.812218948514619399 ) ) ;
#4910 = CARTESIAN_POINT ( 'NONE',  ( 162.3094458652978744, 251.7674390756731668, -12.89874854057887354 ) ) ;
#4911 = CARTESIAN_POINT ( 'NONE',  ( 176.5750811079351763, 290.0661888821730372, -9.631901365267058424 ) ) ;
#4912 = ADVANCED_FACE ( 'NONE', ( #17225 ), #93268, .F. ) ;
#4913 = AXIS2_PLACEMENT_3D ( 'NONE', #28402, #73530, #59282 ) ;
#4915 = EDGE_CURVE ( 'NONE', #47930, #93599, #83277, .T. ) ;
#4914 = DIRECTION ( 'NONE',  ( 0.5000000000000014433, -0.8660254037844378194, 0.000000000000000000 ) ) ;
#4916 = EDGE_CURVE ( 'NONE', #9076, #7688, #31192, .T. ) ;
#4917 = CARTESIAN_POINT ( 'NONE',  ( 82.14994038281616895, 227.4244531367911293, -4.594050593750046652 ) ) ;
#4918 = CARTESIAN_POINT ( 'NONE',  ( 13.89351337401799391, 10.94754757982087945, 5.678558825948272215 ) ) ;
#4919 = CARTESIAN_POINT ( 'NONE',  ( 67.88638817726504726, 65.66482337939683589, 10.84849054539563440 ) ) ;
#4920 = CARTESIAN_POINT ( 'NONE',  ( -13.86269525828469895, 104.2312461070084879, 10.61543114587583148 ) ) ;
#4922 = CARTESIAN_POINT ( 'NONE',  ( 152.2859909530489517, 266.8799217187815884, 16.93598397993736882 ) ) ;
#4921 = CARTESIAN_POINT ( 'NONE',  ( 157.6286460899086137, 257.6261715744221306, 18.25526781158026779 ) ) ;
#4923 = B_SPLINE_CURVE_WITH_KNOTS ( 'NONE', 3,
 ( #74458, #66331, #26839, #5038, #50132, #41522, #57715, #4525, #58707, #81084, #19265, #58222, #4030, #72465, #64335, #73446, #89201, #42028, #11650, #42510, #34918, #18745, #96776, #97264, #80583, #89681, #20242, #95295, #64842, #95789, #25854, #3070, #56730, #26344, #87713, #33956, #57220, #49142, #88195, #53120, #84076, #7016, #75439, #68809, #99237, #92178, #28833, #74945 ),
 .UNSPECIFIED., .F., .F.,
 ( 4, 2, 2, 2, 2, 2, 2, 2, 2, 2, 2, 2, 2, 2, 2, 2, 2, 2, 2, 2, 2, 2, 2, 4 ),
 ( 0.0008144580099773583498, 0.001301468210863030231, 0.001788478411748702004, 0.002031983512191493438, 0.002275488612634284872, 0.002397241162855693383, 0.002518993713077101460, 0.002640746263298509536, 0.002762498813519918047, 0.003006003913962740706, 0.003249509014405562932, 0.003736519215291275037, 0.004710539617062700982, 0.005684560018834127794, 0.006171570219719800868, 0.006658580420605473074, 0.006780332970826863370, 0.006841209245937644387, 0.006902085521048426271, 0.007145590621491398550, 0.007632600822377442855, 0.008119611023263488894, 0.008363116123706508878, 0.008606621224149532332 ),
 .UNSPECIFIED. ) ;
#4924 = CARTESIAN_POINT ( 'NONE',  ( 197.0943835026307056, 289.2695092174155889, 17.13247302375833669 ) ) ;
#4925 = CARTESIAN_POINT ( 'NONE',  ( 75.59751354683669433, 65.29851079375914935, 14.32525510856801709 ) ) ;
#4926 = DIRECTION ( 'NONE',  ( -0.8614378286617561109, 0.5078630399532132467, 0.000000000000000000 ) ) ;
#4927 = CARTESIAN_POINT ( 'NONE',  ( 35.39919958817179690, 22.29860640527294535, -2.839279412974138328 ) ) ;
#4928 = CARTESIAN_POINT ( 'NONE',  ( 193.1649355862271591, 296.0755126543221536, -12.21556774862162698 ) ) ;
#4929 = CARTESIAN_POINT ( 'NONE',  ( 75.09434506655878749, 58.72130435028955731, 16.35444582053638740 ) ) ;
#4930 = ORIENTED_EDGE ( 'NONE', *, *, #25360, .F. ) ;
#4931 = CARTESIAN_POINT ( 'NONE',  ( 22.39019813391814751, 21.43085787977763701, -9.188101187500008038 ) ) ;
#4932 = LINE ( 'NONE', #97159, #57192 ) ;
#4933 = CARTESIAN_POINT ( 'NONE',  ( 193.1569697810063531, 296.0893098336876506, -13.02398914535779539 ) ) ;
#4934 = DIRECTION ( 'NONE',  ( 0.000000000000000000, 0.000000000000000000, 1.000000000000000000 ) ) ;
#4935 = ORIENTED_EDGE ( 'NONE', *, *, #76767, .F. ) ;
#4936 =( BOUNDED_CURVE ( )  B_SPLINE_CURVE ( 2, ( #9777, #2673, #1164, #41134, #55336, #33052, #18368, #86312, #23944, #64458, #1675, #16847, #78672 ),
 .UNSPECIFIED., .F., .T. ) 
 B_SPLINE_CURVE_WITH_KNOTS ( ( 3, 2, 2, 2, 2, 2, 3 ),
 ( 0.01250000000000000069, 0.01499999999999999944, 0.02000000000000000042, 0.02500000000000000139, 0.02999999999999999889, 0.03500000000000000333, 0.03750000000000000555 ),
 .UNSPECIFIED. ) 
 CURVE ( )  GEOMETRIC_REPRESENTATION_ITEM ( )  RATIONAL_B_SPLINE_CURVE ( ( 0.9755282581475768211, 0.9755282581475768211, 1.000000000000000000, 0.9510565162951535312, 1.000000000000000000, 0.9510565162951535312, 1.000000000000000000, 0.9510565162951535312, 1.000000000000000000, 0.9510565162951535312, 1.000000000000000000, 0.9755282581475767101, 0.9755282581475768211 ) ) 
 REPRESENTATION_ITEM ( '' )  );
#4937 = CARTESIAN_POINT ( 'NONE',  ( 70.99470838923255656, 61.07944878815018086, 14.50894906648577631 ) ) ;
#4938 = CARTESIAN_POINT ( 'NONE',  ( 198.0006249058153003, 287.6998530631771587, 18.31850453277666801 ) ) ;
#4939 = CARTESIAN_POINT ( 'NONE',  ( 157.8154903851704205, 268.3609324989079710, 16.38998070839103249 ) ) ;
#4940 = PLANE ( 'NONE',  #16114 ) ;
#4941 = CARTESIAN_POINT ( 'NONE',  ( 136.1324508756439400, 242.7365022471902307, 10.00000000000009592 ) ) ;
#4942 = DIRECTION ( 'NONE',  ( 0.5000000000000012212, -0.8660254037844379305, -0.000000000000000000 ) ) ;
#4943 = ORIENTED_EDGE ( 'NONE', *, *, #20110, .F. ) ;
#4944 = CARTESIAN_POINT ( 'NONE',  ( 86.53615271802112829, 45.81344646433711887, -9.028428416148619462 ) ) ;
#4945 = CARTESIAN_POINT ( 'NONE',  ( 165.5459811318285972, 246.9046815158575328, -1.768130512343973226 ) ) ;
#4946 = EDGE_LOOP ( 'NONE', ( #84609, #14073, #50650, #71398 ) ) ;
#4947 = LINE ( 'NONE', #28729, #87156 ) ;
#4948 = CARTESIAN_POINT ( 'NONE',  ( 81.46395823134524505, 41.91769605856590886, -7.572882635748096725 ) ) ;
#4949 = ORIENTED_EDGE ( 'NONE', *, *, #10768, .T. ) ;
#4950 = CARTESIAN_POINT ( 'NONE',  ( 66.90909321525144549, 68.17756947874360662, -6.600776075497404527 ) ) ;
#4951 = ORIENTED_EDGE ( 'NONE', *, *, #55441, .T. ) ;
#4952 = CARTESIAN_POINT ( 'NONE',  ( 189.3510599963105960, 290.0131996961930554, 14.40846774032805300 ) ) ;
#4953 = CARTESIAN_POINT ( 'NONE',  ( 158.5534433844464104, 256.0243756735802094, 16.12506798773286221 ) ) ;
#4954 = CARTESIAN_POINT ( 'NONE',  ( 147.0210896547505399, 249.5643266524160140, 9.188101187500095079 ) ) ;
#4955 = CARTESIAN_POINT ( 'NONE',  ( 88.19523698511710563, 44.46804064255652378, -4.670053027270651747 ) ) ;
#4956 = CARTESIAN_POINT ( 'NONE',  ( 192.2836406301186685, 296.5693283646611462, -11.72525413493355373 ) ) ;
#4957 = CARTESIAN_POINT ( 'NONE',  ( 36.57375671714491006, 36.51421378149921537, -9.188101187500004485 ) ) ;
#4958 = CARTESIAN_POINT ( 'NONE',  ( 75.60606471573575504, 59.79559749501326849, -15.76384363349462525 ) ) ;
#4959 = CARTESIAN_POINT ( 'NONE',  ( 164.9592205905213973, 274.6244470290632194, 14.74651761685257512 ) ) ;
#4960 = PLANE ( 'NONE',  #88631 ) ;
#4961 = VERTEX_POINT ( 'NONE', #42512 ) ;
#4962 = ORIENTED_EDGE ( 'NONE', *, *, #29227, .F. ) ;
#4963 = CARTESIAN_POINT ( 'NONE',  ( 81.13608137687064925, 42.60696278352305200, 7.988320930663086905 ) ) ;
#4965 = CARTESIAN_POINT ( 'NONE',  ( 194.3442947553755005, 294.0328026529847421, -15.97648891113594871 ) ) ;
#4964 = CARTESIAN_POINT ( 'NONE',  ( 68.35176054198142026, 65.66817991788700226, 10.38336397426687974 ) ) ;
#4966 = CARTESIAN_POINT ( 'NONE',  ( 85.85757975920050455, 48.54684933318403495, 12.22929488966399880 ) ) ;
#4967 = LINE ( 'NONE', #13073, #27917 ) ;
#4968 = CARTESIAN_POINT ( 'NONE',  ( 158.7507817778773074, 280.7662553832301455, -8.161742422992587009 ) ) ;
#4969 = CARTESIAN_POINT ( 'NONE',  ( 147.6121581866023007, 274.9752375363476631, 8.700660424766859080 ) ) ;
#4970 = DIRECTION ( 'NONE',  ( 0.000000000000000000, -0.5906904945688906672, 0.8068982213550599525 ) ) ;
#4971 = LINE ( 'NONE', #65258, #66283 ) ;
#4972 = EDGE_CURVE ( 'NONE', #38611, #37700, #26531, .T. ) ;
#4973 = CARTESIAN_POINT ( 'NONE',  ( 78.96564777457507489, 59.77152385746119023, 16.49451479044646973 ) ) ;
#4974 = CARTESIAN_POINT ( 'NONE',  ( 96.30395630197683943, 238.6589784336661637, -6.496448406907675876E-16 ) ) ;
#4975 = EDGE_LOOP ( 'NONE', ( #44909, #6067, #30840, #99599 ) ) ;
#4976 = CARTESIAN_POINT ( 'NONE',  ( 171.7154418923348942, 259.3365693118849435, -15.26938553599716641 ) ) ;
#4977 = CYLINDRICAL_SURFACE ( 'NONE', #57701, 10.00000000000001066 ) ;
#4978 = CARTESIAN_POINT ( 'NONE',  ( 164.8623370068202689, 277.1737403023538491, -13.48993746920329073 ) ) ;
#4979 = EDGE_CURVE ( 'NONE', #83740, #81604, #80585, .T. ) ;
#4980 = ORIENTED_EDGE ( 'NONE', *, *, #23312, .F. ) ;
#4981 = ORIENTED_EDGE ( 'NONE', *, *, #97350, .F. ) ;
#4982 = FACE_OUTER_BOUND ( 'NONE', #28219, .T. ) ;
#4983 = CARTESIAN_POINT ( 'NONE',  ( 72.04273812837081437, 59.28583566120335746, 15.34548535902080246 ) ) ;
#4984 = CARTESIAN_POINT ( 'NONE',  ( 157.7529601300917363, 257.4108533407307959, 16.91445305439664892 ) ) ;
#4985 = CARTESIAN_POINT ( 'NONE',  ( 17.84779077618757626, 10.70852965304478843, 1.583844403245364907 ) ) ;
#4986 = CARTESIAN_POINT ( 'NONE',  ( 208.1583869480885483, 270.1060931147653719, 3.025867354224990979 ) ) ;
#4987 = ORIENTED_EDGE ( 'NONE', *, *, #85853, .T. ) ;
#4988 = AXIS2_PLACEMENT_3D ( 'NONE', #91943, #14883, #84338 ) ;
#4989 = DIRECTION ( 'NONE',  ( 0.9291732088853837945, -0.3696446237802449297, 0.000000000000000000 ) ) ;
#4990 = CARTESIAN_POINT ( 'NONE',  ( 162.8223739550644211, 248.6303710312858186, -11.16939803179192658 ) ) ;
#4991 = ORIENTED_EDGE ( 'NONE', *, *, #22539, .F. ) ;
#4992 = EDGE_CURVE ( 'NONE', #35225, #15906, #23827, .T. ) ;
#4993 = B_SPLINE_CURVE_WITH_KNOTS ( 'NONE', 3,
 ( #55173, #85652, #54167, #76985 ),
 .UNSPECIFIED., .F., .F.,
 ( 4, 4 ),
 ( 0.000000000000000000, 0.001252170427096359296 ),
 .UNSPECIFIED. ) ;
#4994 = CARTESIAN_POINT ( 'NONE',  ( 194.8450826448002715, 266.1639313023655973, -8.766057580558177520 ) ) ;
#4995 = LINE ( 'NONE', #28269, #80233 ) ;
#4996 = CARTESIAN_POINT ( 'NONE',  ( 82.54497950703030540, 45.20829423347827714, 10.29466844316771734 ) ) ;
#4998 = CARTESIAN_POINT ( 'NONE',  ( 69.60866448817320418, 62.38574252042192114, -13.47313703376398664 ) ) ;
#4997 = CARTESIAN_POINT ( 'NONE',  ( 123.3944002380500677, 251.2369531367911293, -4.594050593750048428 ) ) ;
#4999 = CARTESIAN_POINT ( 'NONE',  ( -62.95439910331221256, 68.06504152958493137, -20.00000000000000355 ) ) ;
#5000 = ORIENTED_EDGE ( 'NONE', *, *, #27630, .F. ) ;
#5001 = CARTESIAN_POINT ( 'NONE',  ( 147.3154503175461514, 275.4891506405583073, 3.671329888160011823 ) ) ;
#5002 = CARTESIAN_POINT ( 'NONE',  ( 60.78824074639776143, 199.2365022471902307, 10.00000000000009948 ) ) ;
#5003 = CARTESIAN_POINT ( 'NONE',  ( 159.9470087484377814, 253.6106496594791508, -16.54933891566789939 ) ) ;
#5004 = CARTESIAN_POINT ( 'NONE',  ( 192.4273719102352800, 271.7576443049806585, 14.08159452427905300 ) ) ;
#5005 = CARTESIAN_POINT ( 'NONE',  ( 178.2382707639212356, 285.7843550335422833, 14.43266090959460435 ) ) ;
#5006 = PLANE ( 'NONE',  #7937 ) ;
#5007 = CARTESIAN_POINT ( 'NONE',  ( 198.9728866542080823, 282.1116337930695295, -16.69484273823314879 ) ) ;
#5008 = CARTESIAN_POINT ( 'NONE',  ( -38.61298035630893111, 26.97617139035147460, -10.00000000000000000 ) ) ;
#5009 = CARTESIAN_POINT ( 'NONE',  ( 79.83603558536034939, 49.47464228346785831, 14.36412132351409454 ) ) ;
#5010 = CARTESIAN_POINT ( 'NONE',  ( 67.81775003199867058, 69.65792968701072141, -1.625205651952876362 ) ) ;
#5011 = CARTESIAN_POINT ( 'NONE',  ( 61.98804677278346986, 206.5958772461660828, -9.188101187500095079 ) ) ;
#5012 = CARTESIAN_POINT ( 'NONE',  ( 206.1408608592916494, 273.6005508061571732, -10.42739367433323494 ) ) ;
#5013 = CARTESIAN_POINT ( 'NONE',  ( -22.42236680055709641, 157.8615022471902591, 0.000000000000000000 ) ) ;
#5014 = CARTESIAN_POINT ( 'NONE',  ( 207.9328781051891042, 270.4966858882232259, -0.8820402142964423042 ) ) ;
#5015 = LINE ( 'NONE', #6000, #85432 ) ;
#5017 = CYLINDRICAL_SURFACE ( 'NONE', #67393, 16.60714546451156792 ) ;
#5016 = CARTESIAN_POINT ( 'NONE',  ( 73.62324627567660684, 69.69863374744915063, -9.485613227022392735 ) ) ;
#5018 = CARTESIAN_POINT ( 'NONE',  ( 185.8639835793372583, 267.1203966262607992, -15.06692291552070273 ) ) ;
#5019 = CARTESIAN_POINT ( 'NONE',  ( 31.53257425345116260, 33.90829794293883026, 10.00000000000000355 ) ) ;
#5020 = DIRECTION ( 'NONE',  ( 0.000000000000000000, 0.000000000000000000, 1.000000000000000000 ) ) ;
#5021 = FACE_OUTER_BOUND ( 'NONE', #87155, .T. ) ;
#5022 = CARTESIAN_POINT ( 'NONE',  ( 205.9652721086518739, 272.7100367737629085, -9.293361325695892461 ) ) ;
#5023 = CARTESIAN_POINT ( 'NONE',  ( 24.28913873611587348, 175.6423013555409796, -4.594050593750043987 ) ) ;
#5024 = CARTESIAN_POINT ( 'NONE',  ( 68.19623763041657583, 68.89888936764938876, 6.646214744952141373 ) ) ;
#5025 = VERTEX_POINT ( 'NONE', #96782 ) ;
#5026 = EDGE_CURVE ( 'NONE', #52618, #83827, #17955, .T. ) ;
#5027 = CARTESIAN_POINT ( 'NONE',  ( 86.72622664077024979, 46.44337019134223965, 9.089705772931038652 ) ) ;
#5028 = CARTESIAN_POINT ( 'NONE',  ( 50.13870555935886841, 87.67061469898740711, 10.00000000000000000 ) ) ;
#5029 = CARTESIAN_POINT ( 'NONE',  ( 71.88488839165290756, 72.57896392602057745, -1.213109508826733407 ) ) ;
#5030 = CARTESIAN_POINT ( 'NONE',  ( 53.65289935712326042, 189.5327760586659167, 1.948934522072302763E-15 ) ) ;
#5031 = CARTESIAN_POINT ( 'NONE',  ( 200.9110265982630779, 282.6588894614233141, 17.52479721249226685 ) ) ;
#5032 = CARTESIAN_POINT ( 'NONE',  ( 171.2443824779643080, 286.7566234589221494, 7.224323052557026337 ) ) ;
#5033 = CARTESIAN_POINT ( 'NONE',  ( 147.4317198359019301, 275.2877659273946733, 3.797273160043843188 ) ) ;
#5034 = CARTESIAN_POINT ( 'NONE',  ( 44.94038342867872871, 31.11029122506298705, -8.090169943749478065 ) ) ;
#5035 = CARTESIAN_POINT ( 'NONE',  ( 202.9457411048790618, 270.0800994776229800, -6.926181921767012639 ) ) ;
#5036 = CARTESIAN_POINT ( 'NONE',  ( 178.7320898300308727, 293.3905527527083450, 2.643181550327659668 ) ) ;
#5037 = CARTESIAN_POINT ( 'NONE',  ( 176.5744236666108691, 275.1798363790605322, 17.44874769457867458 ) ) ;
#5038 = CARTESIAN_POINT ( 'NONE',  ( 179.6882155687777356, 278.8364783109157088, -17.29851916968328140 ) ) ;
#5039 = CARTESIAN_POINT ( 'NONE',  ( 72.04713214249291298, 67.71874806291776849, -10.56511915099177301 ) ) ;
#5040 = CARTESIAN_POINT ( 'NONE',  ( 167.1114647352963232, 257.9194854303543138, -15.52048492569388038 ) ) ;
#5041 = ADVANCED_FACE ( 'NONE', ( #46375 ), #24590, .T. ) ;
#5042 = VECTOR ( 'NONE', #77082, 1000.000000000000000 ) ;
#5043 = CARTESIAN_POINT ( 'NONE',  ( 149.0710170770012724, 245.3262482093457777, 3.021315404115420679E-15 ) ) ;
#5044 = CARTESIAN_POINT ( 'NONE',  ( 91.45997379709655206, 233.6115022471902876, -5.000000000000047962 ) ) ;
#5045 = DIRECTION ( 'NONE',  ( 0.5607300124661794838, -0.8279987035736700030, 0.000000000000000000 ) ) ;
#5046 = CARTESIAN_POINT ( 'NONE',  ( 165.2187654623328683, 269.8677273813709121, -16.27684390681923432 ) ) ;
#5047 = ORIENTED_EDGE ( 'NONE', *, *, #52016, .T. ) ;
#5048 = CARTESIAN_POINT ( 'NONE',  ( 60.33744616864313315, 196.4548013555410080, -4.594050593750042211 ) ) ;
#5049 = EDGE_LOOP ( 'NONE', ( #58869, #15624, #55007, #64286, #86903, #68242, #98636, #58129, #90068, #85847, #45803, #93430, #43793, #27597, #77616, #11333, #80130, #85501, #94732, #86887, #63105, #49953, #7048, #32473, #18175, #3012, #61368, #41291, #41332, #44445, #2987, #6249, #53388, #61150, #57126, #46852, #86351, #63422, #35026, #97672, #85968, #36179, #77643, #93211, #86414, #97596, #47092, #44156, #18159, #84786, #47947, #30373, #98782, #38835, #91106, #42666, #69576, #70660, #17799, #87660, #58903, #77066, #42670, #39040, #80089, #61255, #65096, #88362, #2078, #17053, #71113, #35367, #83210, #29392, #46160, #30103, #70263, #91549, #11976, #26677, #62257, #4848, #22370, #16521, #56477, #2957, #94570, #62755, #40026, #15631, #5555, #35242, #20533, #59528, #24128, #18786, #72152, #5842, #69227, #37495, #3359, #68323, #48970, #26879, #32118, #71984, #10946, #73522, #92940, #96534, #17960, #15418, #16627, #22465, #92339, #79532, #14303, #64292, #37804, #31203, #28758, #63599, #81469, #88773, #9834, #65501, #78203, #86331, #53738, #11320, #96670, #53141, #35098, #43915, #74995, #28221, #4272, #25915, #10815, #2578, #95581, #19916, #77730, #92936, #39438, #49531, #43694, #44669, #2070, #16907, #41415, #27990, #65868, #48319, #15672, #20295, #6578, #13156, #89616, #51405, #67267, #38478, #86479, #39633, #69490, #88384, #60995, #33243, #20694, #38413, #69828, #4842, #71861, #38066, #39455, #77951, #82820, #16498, #81107, #38579, #24241, #89135, #706, #15393, #12149, #59601, #96220, #20050, #42411, #63513, #90855, #46289, #12394, #72729, #41700, #50520, #55494, #50307, #70607, #60758, #75018, #6321, #55114, #12732, #67862, #97072, #34576, #60626, #64323, #77977, #6320, #4431, #56890, #12834, #73873, #40430, #52902, #90073, #14904, #676, #561, #70603, #45313, #75606, #4044, #21011, #85348, #47908, #72130, #59404, #57601, #52279, #19690, #15060, #77075, #66665, #56995, #68377, #2964, #18190, #33218, #57881, #20794, #97488, #11917, #97157, #65043, #47157, #85238, #44783, #58854, #18659, #83121, #96426, #43296, #47077, #14026, #34970, #84761, #26174, #88728, #95014, #97806, #93088, #95489, #79350, #69592, #40567, #71116, #4344, #21145, #55149, #2393, #43471, #86977, #45290, #14183, #72901, #64397, #94548, #67648, #30882, #47817, #3724, #97216, #87796, #21541, #17878, #60715, #31320, #37801, #13317, #8548, #65342, #8791, #48807, #32369, #83075, #23132, #78712, #35254, #30008, #14209, #66963, #97212, #35463, #16757, #58644, #84892, #99400, #88865, #48043, #76384, #43109, #17949, #97407, #60774, #9878, #32242, #52842, #35842, #34953, #4346, #99004, #56250, #49572, #87019, #22936, #3839, #92980, #22138, #85378, #8431, #16296, #12562, #83401, #67138, #74892, #71250, #37726, #31710, #53146, #52759, #11224, #46087, #94352, #30237, #16648, #91493, #32474, #54198, #91759, #41213, #71891, #43230, #83092, #24622, #37579, #12049, #35504, #75453, #58033, #63625, #56143, #16193, #20790, #87885, #91297, #91970, #85120, #51562, #25639, #29614, #7254, #72129, #64348, #61001, #39408, #64744, #70857, #61466, #60231, #56903, #21977, #12125, #32095, #47302, #65621, #70091, #797, #35092, #68360, #47789, #65134, #36132, #58508, #16513, #26067, #28209, #58772, #55120, #42767, #97757, #42589 ) ) ;
#5050 = DIRECTION ( 'NONE',  ( -0.4999999999999987788, 0.8660254037844392627, 0.000000000000000000 ) ) ;
#5051 = CARTESIAN_POINT ( 'NONE',  ( 146.7845206192450007, 276.4087478532630939, 4.443586170796542945 ) ) ;
#5052 = CARTESIAN_POINT ( 'NONE',  ( 67.36095123383401528, 66.69455278167134793, -8.467567626117057600 ) ) ;
#5053 = VERTEX_POINT ( 'NONE', #54471 ) ;
#5054 = CARTESIAN_POINT ( 'NONE',  ( 71.01270533261738649, 200.2592609112379591, 2.679491924311254714 ) ) ;
#5055 = CARTESIAN_POINT ( 'NONE',  ( 164.2953672501826929, 246.0790718049323687, -2.576662677987826111 ) ) ;
#5056 = CARTESIAN_POINT ( 'NONE',  ( 77.38344707992527560, 49.10671604805792612, -15.27628165681131200 ) ) ;
#5057 = CARTESIAN_POINT ( 'NONE',  ( 36.43182450750798296, 23.96004757982092315, -5.678558825948276656 ) ) ;
#5058 = CARTESIAN_POINT ( 'NONE',  ( 185.7415151600560819, 263.1377994056483089, 11.14276090414980480 ) ) ;
#5059 = CARTESIAN_POINT ( 'NONE',  ( 149.1004267900891307, 272.3974806997987343, -12.86882154300063341 ) ) ;
#5060 = CARTESIAN_POINT ( 'NONE',  ( 156.8296764551412537, 259.0100275755436883, 18.25869368615038013 ) ) ;
#5061 = ORIENTED_EDGE ( 'NONE', *, *, #98017, .F. ) ;
#5062 = CARTESIAN_POINT ( 'NONE',  ( 14.44441505419593064, 16.84335787977761711, 9.188101187500006262 ) ) ;
#5063 = CARTESIAN_POINT ( 'NONE',  ( 31.19757978783344399, 18.41603393254327514, -1.583844403245396437 ) ) ;
#5064 = CARTESIAN_POINT ( 'NONE',  ( 66.99161703481539121, 69.18407532166969531, -1.591805497166421945 ) ) ;
#5065 = CARTESIAN_POINT ( 'NONE',  ( 20.60277255440211164, 12.86426979415089278, -3.090169943749474069 ) ) ;
#5066 = EDGE_LOOP ( 'NONE', ( #50417, #33111 ) ) ;
#5067 = FACE_OUTER_BOUND ( 'NONE', #46254, .T. ) ;
#5068 = LINE ( 'NONE', #82110, #66204 ) ;
#5069 = CARTESIAN_POINT ( 'NONE',  ( 159.3586121662929713, 254.6297824347537642, -15.50090345830412630 ) ) ;
#5070 = ORIENTED_EDGE ( 'NONE', *, *, #24480, .T. ) ;
#5071 = ORIENTED_EDGE ( 'NONE', *, *, #58498, .F. ) ;
#5073 = CARTESIAN_POINT ( 'NONE',  ( -43.51495119940489786, 40.26192753957666071, 59.99999999999999289 ) ) ;
#5072 = CARTESIAN_POINT ( 'NONE',  ( 207.3874697692679945, 271.4413608369101780, -6.809237722377445401 ) ) ;
#5074 = CARTESIAN_POINT ( 'NONE',  ( 182.3700640764176342, 263.2847133751610045, -13.94439451147478337 ) ) ;
#5075 = ORIENTED_EDGE ( 'NONE', *, *, #18319, .T. ) ;
#5076 = CARTESIAN_POINT ( 'NONE',  ( 66.53579232977513414, 68.81352912635834684, -2.225901204553964785 ) ) ;
#5077 = CARTESIAN_POINT ( 'NONE',  ( 159.3767386493506137, 254.5983864451355032, 15.47015898230477760 ) ) ;
#5078 = CARTESIAN_POINT ( 'NONE',  ( 182.6784043417008263, 256.7666309132076776, 5.682484670743590094 ) ) ;
#5079 = CARTESIAN_POINT ( 'NONE',  ( 78.30540700459937398, 61.08339965263432703, -15.90943835942215046 ) ) ;
#5080 = CARTESIAN_POINT ( 'NONE',  ( 137.4948102131217240, 244.0643266524160424, -9.188101187500093303 ) ) ;
#5081 = DIRECTION ( 'NONE',  ( 1.000000000000000000, 0.000000000000000000, 0.000000000000000000 ) ) ;
#5082 = CARTESIAN_POINT ( 'NONE',  ( -22.42236680055709641, 157.8615022471902591, 0.000000000000000000 ) ) ;
#5083 = EDGE_CURVE ( 'NONE', #42705, #26065, #44511, .T. ) ;
#5084 = EDGE_LOOP ( 'NONE', ( #74785, #58142, #55551, #51440, #84394, #91008, #53504, #361, #23654, #60146, #29901, #3223, #97416, #15997, #95497, #76627, #21383, #28632, #92804, #28886, #85462, #84718, #77866, #34111, #37819, #44393, #51263, #95450, #94208, #85865, #42078, #72803, #47076, #98970, #17943, #96689, #19077, #57033, #66177, #56161, #81298, #65066, #5120, #81849 ) ) ;
#5085 = FACE_OUTER_BOUND ( 'NONE', #8579, .T. ) ;
#5086 = VERTEX_POINT ( 'NONE', #70184 ) ;
#5087 = ORIENTED_EDGE ( 'NONE', *, *, #12355, .T. ) ;
#5088 = CARTESIAN_POINT ( 'NONE',  ( 159.5573297132660002, 254.2855935470410031, 16.91607698584599007 ) ) ;
#5089 = DIRECTION ( 'NONE',  ( 0.8660254037844385966, 0.5000000000000001110, -0.000000000000000000 ) ) ;
#5090 = CARTESIAN_POINT ( 'NONE',  ( 77.90126356732251622, 215.7833772461660544, -9.188101187500095079 ) ) ;
#5091 = DIRECTION ( 'NONE',  ( -0.9292718480896766664, -0.3693965786901617365, 0.000000000000000000 ) ) ;
#5092 = CARTESIAN_POINT ( 'NONE',  ( 81.80121988122709809, 55.57996685460995678, 16.31202477726384004 ) ) ;
#5093 = CARTESIAN_POINT ( 'NONE',  ( 198.2860450010354043, 287.2054909567549430, 18.54284983329501557 ) ) ;
#5094 = DIRECTION ( 'NONE',  ( -0.6123724356957859216, -0.3535533905932690124, 0.7071067811865573427 ) ) ;
#5095 = CARTESIAN_POINT ( 'NONE',  ( 182.3414255478350299, 257.1538671092444588, -6.203902589603837114 ) ) ;
#5096 = ORIENTED_EDGE ( 'NONE', *, *, #92773, .F. ) ;
#5097 = CARTESIAN_POINT ( 'NONE',  ( 76.66170733860469966, 62.40948344195681585, -15.31146014519883991 ) ) ;
#5098 = CARTESIAN_POINT ( 'NONE',  ( 87.25031752591065981, 43.70243236605378456, -1.741586274254640188 ) ) ;
#5099 = CARTESIAN_POINT ( 'NONE',  ( 153.2283961777204695, 265.2476279883323400, -17.66880461074566000 ) ) ;
#5100 = DIRECTION ( 'NONE',  ( 0.9331105242498740626, -0.3595896960900372696, 0.000000000000000000 ) ) ;
#5101 = ORIENTED_EDGE ( 'NONE', *, *, #85291, .F. ) ;
#5102 = CARTESIAN_POINT ( 'NONE',  ( 206.8217325168575371, 270.0045844243117017, 3.350393751014514532 ) ) ;
#5103 = EDGE_CURVE ( 'NONE', #29135, #35604, #72326, .T. ) ;
#5104 = CARTESIAN_POINT ( 'NONE',  ( 76.12675507841289857, 51.10280720933135967, -16.07849684238113497 ) ) ;
#5105 = CARTESIAN_POINT ( 'NONE',  ( 165.1399196574946018, 246.6162641258139843, 5.603258891903981187 ) ) ;
#5106 = LINE ( 'NONE', #90246, #57535 ) ;
#5107 = CARTESIAN_POINT ( 'NONE',  ( 176.9050207115652711, 269.9844065969573990, 16.88525275472998288 ) ) ;
#5108 = CARTESIAN_POINT ( 'NONE',  ( 148.9322735291567597, 272.6887306911919495, -12.40988026045598858 ) ) ;
#5109 = CARTESIAN_POINT ( 'NONE',  ( 199.0131399161024035, 281.1222020366274137, 17.22481283254653306 ) ) ;
#5110 = CARTESIAN_POINT ( 'NONE',  ( 207.5792673731680793, 271.1091576421853233, 2.359198794924813214 ) ) ;
#5111 = CARTESIAN_POINT ( 'NONE',  ( 116.3579438323015012, 247.1744531367911293, 4.594050593750047540 ) ) ;
#5112 = ORIENTED_EDGE ( 'NONE', *, *, #70437, .F. ) ;
#5113 = CARTESIAN_POINT ( 'NONE',  ( 88.03035862218379748, 44.39407565500617636, 4.731894665149351198 ) ) ;
#5114 = CARTESIAN_POINT ( 'NONE',  ( 69.82040969387803386, 67.81765696479247651, -9.721210921651175951 ) ) ;
#5115 = CARTESIAN_POINT ( 'NONE',  ( 79.95816027405184911, 44.45915948752763569, -10.97504526610144993 ) ) ;
#5116 = CARTESIAN_POINT ( 'NONE',  ( 204.9427641582406636, 275.6757151647582305, 14.40446820030680897 ) ) ;
#5117 = CARTESIAN_POINT ( 'NONE',  ( 74.95033118751130985, 62.00148963258062906, 15.10603149014151647 ) ) ;
#5118 = AXIS2_PLACEMENT_3D ( 'NONE', #2065, #16250, #78065 ) ;
#5119 = CARTESIAN_POINT ( 'NONE',  ( 178.6379759496232111, 254.3921254701204759, 4.464154310029138983 ) ) ;
#5120 = ORIENTED_EDGE ( 'NONE', *, *, #93977, .T. ) ;
#5121 = CARTESIAN_POINT ( 'NONE',  ( 77.34464417660132085, 59.58687695751251567, 16.02097068141453562 ) ) ;
#5122 = LINE ( 'NONE', #90768, #6948 ) ;
#5123 = LINE ( 'NONE', #19356, #38137 ) ;
#5124 = LINE ( 'NONE', #4625, #21708 ) ;
#5125 = CARTESIAN_POINT ( 'NONE',  ( 201.2290932460805948, 267.4596528866035783, 0.8384362464926046199 ) ) ;
#5126 = CARTESIAN_POINT ( 'NONE',  ( 199.0733432591706276, 265.2368624245646060, 0.1624720798152879120 ) ) ;
#5127 = CARTESIAN_POINT ( 'NONE',  ( 190.1693911629507738, 301.2639477917662703, -5.112716700269980485 ) ) ;
#5128 = CARTESIAN_POINT ( 'NONE',  ( 70.30735548187293205, 71.13048692529430639, 1.811214889704019226 ) ) ;
#5129 = CARTESIAN_POINT ( 'NONE',  ( 193.3516273516660533, 268.9799088949432075, 12.17662679305565909 ) ) ;
#5130 = ADVANCED_FACE ( 'NONE', ( #10411 ), #18514, .F. ) ;
#5131 = EDGE_CURVE ( 'NONE', #93052, #53210, #64100, .T. ) ;
#5132 = CARTESIAN_POINT ( 'NONE',  ( 12.79584618246493477, 29.16126292948894516, -6.180339887498951690 ) ) ;
#5133 = CARTESIAN_POINT ( 'NONE',  ( 190.5477107455830321, 300.6086790531491033, 3.126266616601216963 ) ) ;
#5134 = CARTESIAN_POINT ( 'NONE',  ( 82.10990542498430500, 41.84899041517284957, 5.504228460268151046 ) ) ;
#5135 = CARTESIAN_POINT ( 'NONE',  ( -27.42236680055714260, 166.5217562850347406, 1.224646799147364892E-15 ) ) ;
#5136 = CARTESIAN_POINT ( 'NONE',  ( 201.3911183001464451, 266.9640362439821502, -3.754059931952923534 ) ) ;
#5137 = CARTESIAN_POINT ( 'NONE',  ( 161.2966333957525933, 251.2730311991824408, 13.85068866972710744 ) ) ;
#5138 = EDGE_CURVE ( 'NONE', #71477, #84728, #71726, .T. ) ;
#5139 = CARTESIAN_POINT ( 'NONE',  ( 142.4652616372697480, 246.3927522451418497, 10.00000000000009592 ) ) ;
#5140 = CARTESIAN_POINT ( 'NONE',  ( 182.7403103768833432, 278.7531403573107127, 17.53058794496005390 ) ) ;
#5141 = ORIENTED_EDGE ( 'NONE', *, *, #41856, .F. ) ;
#5142 = EDGE_CURVE ( 'NONE', #63156, #86521, #95046, .T. ) ;
#5143 = CARTESIAN_POINT ( 'NONE',  ( 157.5042325173297684, 257.8416622032797818, 16.70595240278738203 ) ) ;
#5144 = CARTESIAN_POINT ( 'NONE',  ( 150.6815632051821581, 269.6588720951601772, -14.68790257316217307 ) ) ;
#5145 = CARTESIAN_POINT ( 'NONE',  ( -13.87062626178347813, 171.9869531367911293, 4.594050593750046652 ) ) ;
#5146 = CARTESIAN_POINT ( 'NONE',  ( 61.77188751760236585, 194.2202760586659736, -5.415160957724236172E-17 ) ) ;
#5147 = CARTESIAN_POINT ( 'NONE',  ( 84.74286529925647926, 43.14323271637052670, 6.350952207087867230 ) ) ;
#5148 = CARTESIAN_POINT ( 'NONE',  ( 30.99507739981537213, 18.86426979415090699, -3.090169943749474069 ) ) ;
#5149 = CARTESIAN_POINT ( 'NONE',  ( 68.11396990072297797, 66.09066184265174115, -10.54551009852403354 ) ) ;
#5150 = FACE_OUTER_BOUND ( 'NONE', #96864, .T. ) ;
#5151 = CARTESIAN_POINT ( 'NONE',  ( 72.05747908138206981, 72.41062208079183904, -3.017343731799825512 ) ) ;
#5152 = CARTESIAN_POINT ( 'NONE',  ( 74.18348328006130998, 55.49302420257691892, -16.11862618869125896 ) ) ;
#5153 = EDGE_CURVE ( 'NONE', #48577, #62465, #95325, .T. ) ;
#5155 = CARTESIAN_POINT ( 'NONE',  ( 67.91490812815924016, 210.0177522451418497, -10.00000000000009592 ) ) ;
#5154 = CARTESIAN_POINT ( 'NONE',  ( 171.4364880475070265, 258.3207074781752794, 14.28679915105377241 ) ) ;
#5156 = EDGE_CURVE ( 'NONE', #2331, #55485, #27122, .T. ) ;
#5157 = CARTESIAN_POINT ( 'NONE',  ( 74.67374711520119490, 67.12383300063542890, 12.47279688402123199 ) ) ;
#5158 = CARTESIAN_POINT ( 'NONE',  ( 150.3737790450080354, 270.1919698983467697, 15.09624067603409969 ) ) ;
#5159 = CARTESIAN_POINT ( 'NONE',  ( 55.08690683815017763, 202.6115022471902591, 10.00000000000009592 ) ) ;
#5160 = CARTESIAN_POINT ( 'NONE',  ( 181.8512048739169700, 291.6361654578719254, 9.308531600642181658 ) ) ;
#5161 = CARTESIAN_POINT ( 'NONE',  ( 202.9216520459657147, 279.1763840310111391, 15.75371595331685803 ) ) ;
#5162 = CARTESIAN_POINT ( 'NONE',  ( 18.84898279888859918, 187.8149278399161233, 9.188101187500093303 ) ) ;
#5163 = CARTESIAN_POINT ( 'NONE',  ( 72.87252120309180725, 71.00776288696197014, -7.711505026642229588 ) ) ;
#5164 = CARTESIAN_POINT ( 'NONE',  ( 2.788041384736548611, 183.9637435831425307, 2.679491924311251605 ) ) ;
#5165 = CARTESIAN_POINT ( 'NONE',  ( 45.79150443358504674, 28.29860640527296667, -2.839279412974138328 ) ) ;
#5166 = CARTESIAN_POINT ( 'NONE',  ( 201.2846070193694175, 280.3231637734562582, -16.68660556726656807 ) ) ;
#5167 = CARTESIAN_POINT ( 'NONE',  ( 179.3828213106868077, 277.5311947685291329, 17.51078081574469536 ) ) ;
#5168 = CARTESIAN_POINT ( 'NONE',  ( 22.92804849793282784, 21.43677371833801715, -10.00000000000000355 ) ) ;
#5169 = CARTESIAN_POINT ( 'NONE',  ( 153.4176784699686777, 265.3156473403554969, -16.22513339788883968 ) ) ;
#5170 = DIRECTION ( 'NONE',  ( 1.000000000000000000, 0.000000000000000000, 0.000000000000000000 ) ) ;
#5171 = DIRECTION ( 'NONE',  ( 1.000000000000000000, 0.000000000000000000, 0.000000000000000000 ) ) ;
#5172 = CARTESIAN_POINT ( 'NONE',  ( 15.46319120177094142, 20.87878583063840665, -9.188101187500006262 ) ) ;
#5173 = CARTESIAN_POINT ( 'NONE',  ( 71.66539077729501628, 72.47145342129384460, 0.9585255015204100504 ) ) ;
#5174 = CARTESIAN_POINT ( 'NONE',  ( 82.22659455697501585, 54.23696157584255673, 15.63556931923067239 ) ) ;
#5175 = DIRECTION ( 'NONE',  ( -0.3400251696390411693, 0.9404163354663408469, 0.000000000000000000 ) ) ;
#5176 = CARTESIAN_POINT ( 'NONE',  ( 194.0672051292551430, 294.5127359636757660, 15.53337744471869364 ) ) ;
#5177 = ORIENTED_EDGE ( 'NONE', *, *, #25032, .F. ) ;
#5178 = CYLINDRICAL_SURFACE ( 'NONE', #33397, 70.00000000000002842 ) ;
#5179 = CARTESIAN_POINT ( 'NONE',  ( 103.9969882237314351, 242.3967562850347122, -4.648177544792955347E-16 ) ) ;
#5180 = APPLICATION_CONTEXT ( 'automotive_design' ) ;
#5181 = CARTESIAN_POINT ( 'NONE',  ( 81.11262804297332707, 42.45350992371406562, 7.766723531211875198 ) ) ;
#5182 = DIRECTION ( 'NONE',  ( 0.5076330711061761702, -0.8615733660689098850, 0.000000000000000000 ) ) ;
#5183 = ORIENTED_EDGE ( 'NONE', *, *, #20011, .F. ) ;
#5184 = LINE ( 'NONE', #99385, #95961 ) ;
#5185 = CARTESIAN_POINT ( 'NONE',  ( 67.96380970210620376, 69.83446729340751347, 0.3907781913280385377 ) ) ;
#5186 = CARTESIAN_POINT ( 'NONE',  ( 201.5931001570695571, 271.8169877960688723, -11.84458199429158931 ) ) ;
#5187 = CARTESIAN_POINT ( 'NONE',  ( 203.1526193585190470, 278.7763369107815379, -16.67658907091021447 ) ) ;
#5188 = ORIENTED_EDGE ( 'NONE', *, *, #40157, .F. ) ;
#5190 = CARTESIAN_POINT ( 'NONE',  ( 164.4990934228277411, 245.7262077230798809, 6.470820838822735510 ) ) ;
#5189 = CARTESIAN_POINT ( 'NONE',  ( 164.4077444581934060, 246.8171098232803047, -5.536143951676388397 ) ) ;
#5191 = CARTESIAN_POINT ( 'NONE',  ( 192.7693357657653053, 296.7607116428271183, 12.22606306887835714 ) ) ;
#5192 = ORIENTED_EDGE ( 'NONE', *, *, #4721, .T. ) ;
#5193 = CARTESIAN_POINT ( 'NONE',  ( 88.14497077207560949, 43.82233299356100531, -2.120619512623201253 ) ) ;
#5194 = CARTESIAN_POINT ( 'NONE',  ( 80.26984573713558291, 57.41310870600725025, -16.58958131739138508 ) ) ;
#5195 = CARTESIAN_POINT ( 'NONE',  ( 174.5400248142499890, 262.3018208131371125, 14.37995792819177154 ) ) ;
#5196 = VERTEX_POINT ( 'NONE', #47878 ) ;
#5197 = LINE ( 'NONE', #75598, #96114 ) ;
#5198 = CARTESIAN_POINT ( 'NONE',  ( 81.17457202243787151, 43.12509331780193378, 9.545365352588273566 ) ) ;
#5199 = EDGE_CURVE ( 'NONE', #98479, #69834, #1810, .T. ) ;
#5200 = ORIENTED_EDGE ( 'NONE', *, *, #4454, .T. ) ;
#5201 = CARTESIAN_POINT ( 'NONE',  ( 206.4229368915142686, 273.1119807867502800, 10.31819530520674810 ) ) ;
#5202 = CARTESIAN_POINT ( 'NONE',  ( 151.0534475874070779, 275.6857711074018766, -8.249277203261174307 ) ) ;
#5203 = ORIENTED_EDGE ( 'NONE', *, *, #58316, .T. ) ;
#5204 = CARTESIAN_POINT ( 'NONE',  ( 177.4590209526847389, 279.3686772430251608, -16.70803785899330762 ) ) ;
#5205 = DIRECTION ( 'NONE',  ( 0.4999999999999992784, -0.8660254037844390407, 0.000000000000000000 ) ) ;
#5206 = EDGE_CURVE ( 'NONE', #94561, #86855, #57060, .T. ) ;
#5207 = ORIENTED_EDGE ( 'NONE', *, *, #93109, .F. ) ;
#5208 = CARTESIAN_POINT ( 'NONE',  ( 90.04477061917849312, 44.76220097505219542, 0.000000000000000000 ) ) ;
#5209 = CARTESIAN_POINT ( 'NONE',  ( 193.2053309019613891, 296.0055459150826778, -12.79465285318189061 ) ) ;
#5210 = ORIENTED_EDGE ( 'NONE', *, *, #44566, .F. ) ;
#5211 = CARTESIAN_POINT ( 'NONE',  ( 157.3127155075455050, 269.2413269589708307, 15.61457394689876388 ) ) ;
#5212 = ORIENTED_EDGE ( 'NONE', *, *, #56220, .F. ) ;
#5213 =( BOUNDED_CURVE ( )  B_SPLINE_CURVE ( 2, ( #58570, #64189, #17592, #71813, #95138, #10494, #11516, #64699, #73304 ),
 .UNSPECIFIED., .F., .T. ) 
 B_SPLINE_CURVE_WITH_KNOTS ( ( 3, 2, 2, 2, 3 ),
 ( 0.03629032258064516375, 0.03763440860215053890, 0.04032258064516128920, 0.04301075268817204644, 0.04435483870967742159 ),
 .UNSPECIFIED. ) 
 CURVE ( )  GEOMETRIC_REPRESENTATION_ITEM ( )  RATIONAL_B_SPLINE_CURVE ( ( 0.9330127018922194093, 0.9330127018922195203, 1.000000000000000000, 0.8660254037844387076, 1.000000000000000000, 0.8660254037844387076, 1.000000000000000000, 0.9330127018922194093, 0.9330127018922194093 ) ) 
 REPRESENTATION_ITEM ( '' )  );
#5214 = CARTESIAN_POINT ( 'NONE',  ( 156.5650439790640860, 266.5144819405009571, -16.22741892766980953 ) ) ;
#5215 = CARTESIAN_POINT ( 'NONE',  ( 169.0688750560406675, 272.3726058702321779, 16.94514216011815932 ) ) ;
#5216 = CARTESIAN_POINT ( 'NONE',  ( 190.2236813008869660, 301.1699145145108218, -5.401374690107298093 ) ) ;
#5217 = CARTESIAN_POINT ( 'NONE',  ( 50.27371054362191671, 89.86549102125590593, 177.5919119679930134 ) ) ;
#5218 = CARTESIAN_POINT ( 'NONE',  ( 148.9228818358559749, 272.7049975811580680, 12.13823097167056275 ) ) ;
#5219 = CARTESIAN_POINT ( 'NONE',  ( 192.3401793061076717, 297.5040324353506094, 12.56432540404525611 ) ) ;
#5220 = EDGE_CURVE ( 'NONE', #63028, #67404, #8246, .T. ) ;
#5221 = CARTESIAN_POINT ( 'NONE',  ( 177.2398528310001495, 290.8784864842746174, 6.085034101453419275 ) ) ;
#5222 = CARTESIAN_POINT ( 'NONE',  ( 146.5095091551180815, 276.8850816817948726, 0.1418322875769769398 ) ) ;
#5223 = EDGE_LOOP ( 'NONE', ( #62211, #68488, #6769, #86872 ) ) ;
#5224 = CARTESIAN_POINT ( 'NONE',  ( 74.46886260449439021, 57.89172860934509401, -15.95710879220658995 ) ) ;
#5225 = AXIS2_PLACEMENT_3D ( 'NONE', #7540, #98778, #60719 ) ;
#5227 = CARTESIAN_POINT ( 'NONE',  ( 164.9356397357043704, 244.9700873293209042, 2.799217332519396972 ) ) ;
#5226 = CARTESIAN_POINT ( 'NONE',  ( 149.6230451358742926, 271.4922791719315001, -12.72565967355361671 ) ) ;
#5228 = CARTESIAN_POINT ( 'NONE',  ( 198.5966822647444587, 286.6674514332866579, 17.25284514431582750 ) ) ;
#5229 = CARTESIAN_POINT ( 'NONE',  ( 171.2304119843477963, 289.1496298482710472, 4.331491222947584596 ) ) ;
#5230 = LINE ( 'NONE', #51308, #85225 ) ;
#5231 = ORIENTED_EDGE ( 'NONE', *, *, #15630, .F. ) ;
#5232 = CARTESIAN_POINT ( 'NONE',  ( 72.06483804294512652, 69.71054388629096366, 8.252314821295385627 ) ) ;
#5233 = CARTESIAN_POINT ( 'NONE',  ( 83.36864264039709838, 41.16137561131296962, 2.770299137610701123 ) ) ;
#5234 = ADVANCED_FACE ( 'NONE', ( #75210 ), #43779, .T. ) ;
#5235 = CARTESIAN_POINT ( 'NONE',  ( 20.67738335769525904, 35.85097175740956743, -10.00000000000000000 ) ) ;
#5236 = EDGE_CURVE ( 'NONE', #30076, #24137, #68083, .T. ) ;
#5237 = CARTESIAN_POINT ( 'NONE',  ( 199.0619536713871582, 285.8615777176725032, -18.61677200412056976 ) ) ;
#5238 = ORIENTED_EDGE ( 'NONE', *, *, #35698, .F. ) ;
#5239 = CARTESIAN_POINT ( 'NONE',  ( 207.9328781051891042, 270.4966858882232259, -0.8820402142964423042 ) ) ;
#5240 = CARTESIAN_POINT ( 'NONE',  ( 85.27608704655584404, 46.23732751045460532, 10.40392852235657450 ) ) ;
#5241 = CARTESIAN_POINT ( 'NONE',  ( 201.0468719883840265, 282.4235983437597497, -16.59631526626950659 ) ) ;
#5242 = CARTESIAN_POINT ( 'NONE',  ( 165.0532575723395041, 244.7663672603923715, -2.144843157699870773 ) ) ;
#5243 = CARTESIAN_POINT ( 'NONE',  ( 27.64472685218285264, 186.7677522451418497, 10.00000000000009592 ) ) ;
#5244 = CARTESIAN_POINT ( 'NONE',  ( 117.4951228184160783, 229.4548013555409796, -4.594050593750042211 ) ) ;
#5245 = B_SPLINE_CURVE_WITH_KNOTS ( 'NONE', 3,
 ( #15012, #23605, #54002, #15506, #76352, #23111, #68221, #14541, #31215, #29733, #30734, #822, #68721, #37321, #84962, #39297, #8427, #22633, #7420, #46925, #7941, #84471, #22133, #38313, #99145, #54499, #60607, #69222, #53519, #77332, #62103 ),
 .UNSPECIFIED., .F., .F.,
 ( 4, 3, 3, 3, 3, 3, 3, 3, 3, 3, 4 ),
 ( 0.000000000000000000, 0.1333490885032332374, 0.3007194338854220494, 0.4699862290245090390, 0.5844252810809320575, 0.6686540514502788968, 0.7354980260655487045, 0.8028463152565534777, 0.8633854507757111607, 0.9437142632667073761, 1.000000000000000000 ),
 .UNSPECIFIED. ) ;
#5246 = CARTESIAN_POINT ( 'NONE',  ( 180.8047931442907270, 294.0922736414096903, -2.692425206983429131 ) ) ;
#5247 = CARTESIAN_POINT ( 'NONE',  ( 162.8839686824157127, 249.6387011324054015, -11.33670648097108113 ) ) ;
#5248 = CARTESIAN_POINT ( 'NONE',  ( 84.62367088353330757, 50.61169820936780184, 13.65639662624268702 ) ) ;
#5249 = CARTESIAN_POINT ( 'NONE',  ( 163.1177074157340030, 248.1188384722309195, 11.53923137679231026 ) ) ;
#5250 = CARTESIAN_POINT ( 'NONE',  ( 30.81113223654366706, 188.5958772461660544, -9.188101187500095079 ) ) ;
#5251 = CARTESIAN_POINT ( 'NONE',  ( -1.087500518889665591, 25.57194971796827332, 10.00000000000000000 ) ) ;
#5252 = ORIENTED_EDGE ( 'NONE', *, *, #63640, .T. ) ;
#5253 = CYLINDRICAL_SURFACE ( 'NONE', #52742, 10.00000000000010658 ) ;
#5254 = CARTESIAN_POINT ( 'NONE',  ( 74.29176946830207839, 67.89628765651626452, -11.69942945965017422 ) ) ;
#5255 = EDGE_CURVE ( 'NONE', #1997, #61284, #67583, .T. ) ;
#5256 = DIRECTION ( 'NONE',  ( 0.4999999999999992784, -0.8660254037844390407, 0.000000000000000000 ) ) ;
#5257 = CARTESIAN_POINT ( 'NONE',  ( 81.67837127500261829, 41.48712589271562479, -5.236831772534292107 ) ) ;
#5258 = CARTESIAN_POINT ( 'NONE',  ( 8.995063969029878592, 17.14441083166259006, 10.00000000000000533 ) ) ;
#5259 = CARTESIAN_POINT ( 'NONE',  ( 179.0026682949594488, 287.9522070891227941, -12.87249257965389759 ) ) ;
#5260 = DIRECTION ( 'NONE',  ( -6.123233995736786990E-17, 1.060575238724905929E-16, 1.000000000000000000 ) ) ;
#5261 = EDGE_CURVE ( 'NONE', #53287, #82871, #57996, .T. ) ;
#5262 = B_SPLINE_CURVE_WITH_KNOTS ( 'NONE', 3,
 ( #60180, #6514, #28298, #91144, #84054, #66802, #52591, #21706, #99219, #20224, #14110, #37392, #59175, #90664, #60676, #36899, #90148, #12629, #44991, #75936, #68296, #98227, #91637, #35902 ),
 .UNSPECIFIED., .F., .F.,
 ( 4, 2, 2, 2, 2, 2, 2, 2, 2, 2, 2, 4 ),
 ( 0.000000000000000000, 0.1249999999999811262, 0.2499999999999622524, 0.3749999999999433786, 0.4374999999999501510, 0.4999999999999569233, 0.5624999999999636957, 0.6249999999999704681, 0.6874999999999772404, 0.7499999999999840128, 0.8749999999999916733, 1.000000000000000000 ),
 .UNSPECIFIED. ) ;
#5263 = CARTESIAN_POINT ( 'NONE',  ( 95.19470834736912934, 215.7677522451417929, -5.000000000000041744 ) ) ;
#5264 = ORIENTED_EDGE ( 'NONE', *, *, #71455, .F. ) ;
#5265 = CARTESIAN_POINT ( 'NONE',  ( 79.05300200689269730, 59.41537015362478513, -16.53193985632129426 ) ) ;
#5266 = ADVANCED_FACE ( 'NONE', ( #30083 ), #8781, .T. ) ;
#5267 = EDGE_CURVE ( 'NONE', #34753, #63230, #62581, .T. ) ;
#5268 = CARTESIAN_POINT ( 'NONE',  ( 202.4943568615953779, 279.9164810001701085, 17.09064351659286984 ) ) ;
#5269 = CARTESIAN_POINT ( 'NONE',  ( 208.0006710756887287, 270.3792650189220126, -0.8737665032493013850 ) ) ;
#5270 = CARTESIAN_POINT ( 'NONE',  ( 9.403806464923315289, 185.4244531367911293, -4.594050593750046652 ) ) ;
#5271 = ADVANCED_FACE ( 'NONE', ( #77703 ), #29589, .T. ) ;
#5272 = CARTESIAN_POINT ( 'NONE',  ( 66.81631347157465939, 68.63490661804873127, -5.506013109174251241 ) ) ;
#5273 = DIRECTION ( 'NONE',  ( 0.8325133752583725455, -0.5540049458406594018, 0.000000000000000000 ) ) ;
#5274 = CARTESIAN_POINT ( 'NONE',  ( 71.55076955509966297, 59.02864663040953275, -15.83821917523768619 ) ) ;
#5275 = CARTESIAN_POINT ( 'NONE',  ( 73.57121657643290291, 69.82745460598127352, 9.896087309288359890 ) ) ;
#5276 = CARTESIAN_POINT ( 'NONE',  ( 56.95444766116892055, 197.5643266524159856, -9.188101187500093303 ) ) ;
#5277 = CARTESIAN_POINT ( 'NONE',  ( 163.7595992360150490, 247.0070492265414828, -6.976205010573520049 ) ) ;
#5278 = CARTESIAN_POINT ( 'NONE',  ( 203.6731738038005517, 276.2319078309685096, 13.32647105319332326 ) ) ;
#5279 = CARTESIAN_POINT ( 'NONE',  ( 68.35978272809893497, 66.81434282768250910, 9.109814194020067646 ) ) ;
#5280 = CARTESIAN_POINT ( 'NONE',  ( 66.16222611801360642, 68.48874123133123248, -4.854165969021398297 ) ) ;
#5281 = ORIENTED_EDGE ( 'NONE', *, *, #98009, .T. ) ;
#5282 = B_SPLINE_CURVE_WITH_KNOTS ( 'NONE', 3,
 ( #18556, #87522, #18054, #79884 ),
 .UNSPECIFIED., .F., .F.,
 ( 4, 4 ),
 ( 0.009818966555397349791, 0.01814036154117733973 ),
 .UNSPECIFIED. ) ;
#5283 = CARTESIAN_POINT ( 'NONE',  ( 16.11576366785043746, 180.1115022471902591, 10.00000000000009592 ) ) ;
#5284 = DIRECTION ( 'NONE',  ( 0.000000000000000000, 1.000000000000000000, 0.000000000000000000 ) ) ;
#5285 = CARTESIAN_POINT ( 'NONE',  ( 146.3987206697217403, 246.1423013555409796, -4.594050593750043987 ) ) ;
#5286 = CARTESIAN_POINT ( 'NONE',  ( 22.53213034355506750, 33.98502408145593279, -5.678558825948271327 ) ) ;
#5287 = CARTESIAN_POINT ( 'NONE',  ( 188.7923053583308217, 259.7687708077174307, -4.103412599247693748 ) ) ;
#5288 = CARTESIAN_POINT ( 'NONE',  ( -27.42236680055714260, 166.5217562850347406, 1.224646799147364892E-15 ) ) ;
#5289 = CARTESIAN_POINT ( 'NONE',  ( 197.3711752247862705, 281.8738618512871881, -17.64585401704185941 ) ) ;
#5291 = CARTESIAN_POINT ( 'NONE',  ( 74.70353909524752112, 67.05423462026553239, 12.97237599094835758 ) ) ;
#5290 = LINE ( 'NONE', #92902, #43565 ) ;
#5292 = CARTESIAN_POINT ( 'NONE',  ( 68.89885689118237622, 64.10311179774262769, 12.05621680499958082 ) ) ;
#5293 = ORIENTED_EDGE ( 'NONE', *, *, #21840, .F. ) ;
#5294 = CARTESIAN_POINT ( 'NONE',  ( 191.4922467593309250, 298.9726946877590876, 7.604184559945784017 ) ) ;
#5295 = CARTESIAN_POINT ( 'NONE',  ( 208.1052924987534425, 270.1980553986139171, -0.2554279711716039847 ) ) ;
#5296 = CARTESIAN_POINT ( 'NONE',  ( 152.2397443934144690, 268.7033665454236484, -15.42800614587808461 ) ) ;
#5297 = VECTOR ( 'NONE', #57094, 1000.000000000000114 ) ;
#5298 = CARTESIAN_POINT ( 'NONE',  ( 170.6178593158246315, 266.5408558992322696, -17.65857870869936974 ) ) ;
#5299 = LINE ( 'NONE', #91928, #66907 ) ;
#5300 = ORIENTED_EDGE ( 'NONE', *, *, #14158, .F. ) ;
#5301 = CARTESIAN_POINT ( 'NONE',  ( 70.99214648936349192, 70.33938369507340838, 5.954994780460230785 ) ) ;
#5302 = AXIS2_PLACEMENT_3D ( 'NONE', #96695, #34356, #90092 ) ;
#5303 = CARTESIAN_POINT ( 'NONE',  ( 168.7064118984686161, 282.3780792379856166, -10.92572408344284440 ) ) ;
#5304 = B_SPLINE_SURFACE_WITH_KNOTS ( 'NONE', 3, 1, ( 
 ( #58821, #73558 ),
 ( #12260, #82198 ),
 ( #49751, #18868 ),
 ( #57838, #43118 ),
 ( #90294, #96390 ),
 ( #74572, #97373 ),
 ( #4142, #65942 ),
 ( #81687, #13262 ),
 ( #26954, #36031 ),
 ( #19865, #50732 ),
 ( #96895, #44122 ),
 ( #80703, #88818 ),
 ( #11279, #51229 ),
 ( #74063, #66931 ),
 ( #27939, #19384 ),
 ( #89783, #88314 ),
 ( #81197, #28432 ),
 ( #59314, #11766 ),
 ( #26464, #20359 ),
 ( #35037, #20863 ),
 ( #4651, #73071 ),
 ( #51754, #27465 ),
 ( #82696, #75059 ),
 ( #66445, #12768 ),
 ( #43633, #3669 ),
 ( #5636, #36529 ),
 ( #95906, #57340 ),
 ( #98862, #46110 ),
 ( #30431, #90793 ),
 ( #38521, #67941 ),
 ( #54208, #7630 ),
 ( #68922, #14242 ),
 ( #13736, #29932 ),
 ( #99354, #92765 ) ),
 .UNSPECIFIED., .T., .F., .F.,
 ( 4, 2, 2, 2, 2, 2, 2, 2, 2, 2, 2, 2, 2, 2, 2, 2, 4 ),
 ( 2, 2 ),
 ( 0.000000000000000000, 0.06250000000000000000, 0.1250000000000000000, 0.1875000000000000000, 0.2500000000000000000, 0.3125000000000000000, 0.3750000000000000000, 0.4375000000000000000, 0.5000000000000000000, 0.5625000000000000000, 0.6250000000000000000, 0.6875000000000000000, 0.7500000000000000000, 0.8125000000000000000, 0.8750000000000000000, 0.9375000000000000000, 1.000000000000000000 ),
 ( 0.000000000000000000, 1.000000000000000000 ),
 .UNSPECIFIED. ) ;
#5305 = CARTESIAN_POINT ( 'NONE',  ( 77.71268576465143951, 49.44357064982640537, 15.32985931323573325 ) ) ;
#5306 = CARTESIAN_POINT ( 'NONE',  ( 84.99999999999998579, 14.99999999999999467, 59.99999999999999289 ) ) ;
#5307 = CARTESIAN_POINT ( 'NONE',  ( 181.8596306508903524, 295.2094889523889378, 4.865735665145750843 ) ) ;
#5308 = CARTESIAN_POINT ( 'NONE',  ( 146.5247557210571756, 248.7365022471902023, 10.00000000000009948 ) ) ;
#5309 = PLANE ( 'NONE',  #88938 ) ;
#5310 = CARTESIAN_POINT ( 'NONE',  ( 138.1418008908465822, 79.75620593067000641, 17.47570218321536473 ) ) ;
#5311 = ORIENTED_EDGE ( 'NONE', *, *, #87580, .F. ) ;
#5312 = CARTESIAN_POINT ( 'NONE',  ( 159.1344352748853055, 279.7114264697810313, -10.00621538743078354 ) ) ;
#5313 = CARTESIAN_POINT ( 'NONE',  ( 12.29152061481545566, 25.83478043621387243, -8.090169943749479842 ) ) ;
#5314 = PLANE ( 'NONE',  #82263 ) ;
#5315 = ORIENTED_EDGE ( 'NONE', *, *, #29918, .T. ) ;
#5316 = CARTESIAN_POINT ( 'NONE',  ( 74.24569808078352651, 55.17391705787447620, 16.60426680768635421 ) ) ;
#5317 = CARTESIAN_POINT ( 'NONE',  ( 22.96769398916923421, 37.53608102203548214, 177.5919119679930134 ) ) ;
#5318 = CARTESIAN_POINT ( 'NONE',  ( 159.3149481673140144, 263.8852099524119126, -17.20139123423869520 ) ) ;
#5319 = VERTEX_POINT ( 'NONE', #99005 ) ;
#5320 = CARTESIAN_POINT ( 'NONE',  ( 146.7818291168261453, 276.4134096722012828, -0.7617065417431535534 ) ) ;
#5321 = CARTESIAN_POINT ( 'NONE',  ( 186.0392071921917534, 291.3832317854910343, 12.18629431491837600 ) ) ;
#5322 = VECTOR ( 'NONE', #87299, 1000.000000000000000 ) ;
#5323 = CARTESIAN_POINT ( 'NONE',  ( 204.8523313866422484, 275.8323493198358847, 14.65426965484541100 ) ) ;
#5324 = CARTESIAN_POINT ( 'NONE',  ( 51.11762373747147592, 206.9865022471902876, -10.00000000000009592 ) ) ;
#5325 = ORIENTED_EDGE ( 'NONE', *, *, #20648, .T. ) ;
#5326 = CARTESIAN_POINT ( 'NONE',  ( 88.45577462806285496, 228.0024278399160949, -9.188101187500093303 ) ) ;
#5327 = CARTESIAN_POINT ( 'NONE',  ( 155.3184171719837252, 261.6276054373827833, 18.58354126389791361 ) ) ;
#5328 = LINE ( 'NONE', #21043, #11674 ) ;
#5329 = CARTESIAN_POINT ( 'NONE',  ( 185.1433062948085251, 259.8750339556800100, -6.566076700648285858 ) ) ;
#5330 = ORIENTED_EDGE ( 'NONE', *, *, #25246, .T. ) ;
#5331 = ORIENTED_EDGE ( 'NONE', *, *, #32346, .T. ) ;
#5332 = CARTESIAN_POINT ( 'NONE',  ( 192.9672696936424074, 283.3911346215554659, -17.79517654261226767 ) ) ;
#5333 = VERTEX_POINT ( 'NONE', #7784 ) ;
#5334 = CARTESIAN_POINT ( 'NONE',  ( 81.86540518833783153, 52.37565918963163369, 15.11782163349261410 ) ) ;
#5335 = VERTEX_POINT ( 'NONE', #185 ) ;
#5336 = CARTESIAN_POINT ( 'NONE',  ( 75.09907887158918527, 59.19784231363958327, 15.80952553784205428 ) ) ;
#5337 = CARTESIAN_POINT ( 'NONE',  ( 203.1705638993064156, 278.7452560544191442, -15.08126533799095093 ) ) ;
#5338 = ORIENTED_EDGE ( 'NONE', *, *, #13491, .F. ) ;
#5339 = CARTESIAN_POINT ( 'NONE',  ( 182.7224642469025468, 280.1677561527186526, -16.13469908156701393 ) ) ;
#5340 = FACE_OUTER_BOUND ( 'NONE', #3268, .T. ) ;
#5341 = CARTESIAN_POINT ( 'NONE',  ( 81.75096066047075283, 229.5530062829863027, -4.648177544792955347E-16 ) ) ;
#5342 = EDGE_CURVE ( 'NONE', #20462, #79982, #38157, .T. ) ;
#5343 = CARTESIAN_POINT ( 'NONE',  ( 71.78973387874195566, 68.32824629913071135, -9.790379935438130232 ) ) ;
#5344 = CARTESIAN_POINT ( 'NONE',  ( 168.2829851573790165, 267.1582986060611802, -17.45266922015316879 ) ) ;
#5345 = VERTEX_POINT ( 'NONE', #78193 ) ;
#5346 = CARTESIAN_POINT ( 'NONE',  ( 75.95060373600504988, 56.00093423504673495, 16.15035647359714588 ) ) ;
#5347 = CARTESIAN_POINT ( 'NONE',  ( 4.685401460390529849, 24.74646525600388003, 2.839279412974139660 ) ) ;
#5348 = VERTEX_POINT ( 'NONE', #14395 ) ;
#5349 = CARTESIAN_POINT ( 'NONE',  ( 167.2946170330464497, 284.3018367931351804, 9.330332355628671692 ) ) ;
#5351 = ORIENTED_EDGE ( 'NONE', *, *, #54261, .T. ) ;
#5350 = CARTESIAN_POINT ( 'NONE',  ( 203.9579186766783891, 271.6971408411359334, 9.704203457501737518 ) ) ;
#5352 = CARTESIAN_POINT ( 'NONE',  ( -14.46602979551751389, 105.4129113170957481, 10.54689744722228006 ) ) ;
#5353 = CARTESIAN_POINT ( 'NONE',  ( 163.1008115941903895, 248.1481028935802442, 11.25332017433677834 ) ) ;
#5354 = CARTESIAN_POINT ( 'NONE',  ( 188.9068162171112419, 259.6246725331779999, 2.484684062397731097 ) ) ;
#5355 = CARTESIAN_POINT ( 'NONE',  ( 160.7119030392097727, 282.6337468314966372, -6.452778162566800368 ) ) ;
#5356 = ADVANCED_FACE ( 'NONE', ( #37668 ), #805, .F. ) ;
#5357 = CARTESIAN_POINT ( 'NONE',  ( 174.5432515410337544, 282.4104588529930311, -15.15290805577315680 ) ) ;
#5358 = CARTESIAN_POINT ( 'NONE',  ( -74.97640825042664403, 52.25402898078436920, 10.00000000000000000 ) ) ;
#5359 = ADVANCED_FACE ( 'NONE', ( #41665 ), #48796, .T. ) ;
#5360 = CARTESIAN_POINT ( 'NONE',  ( 84.97346864989049209, 42.47303927933469936, 1.910285522896328469 ) ) ;
#5361 = CARTESIAN_POINT ( 'NONE',  ( 88.43398120015881148, 44.08421024288151102, -2.684292198961160114 ) ) ;
#5362 = VERTEX_POINT ( 'NONE', #79727 ) ;
#5363 = CARTESIAN_POINT ( 'NONE',  ( 102.4216706764260465, 218.3932355074535678, -2.679491924311248496 ) ) ;
#5364 = CARTESIAN_POINT ( 'NONE',  ( 73.08335586614711588, 62.87131163969772274, -14.31063855017556286 ) ) ;
#5365 = ORIENTED_EDGE ( 'NONE', *, *, #96234, .F. ) ;
#5366 = CARTESIAN_POINT ( 'NONE',  ( 11.48900327905998431, 165.8932355074535678, -2.679491924311248496 ) ) ;
#5367 = CARTESIAN_POINT ( 'NONE',  ( 171.4037692059896472, 279.8853805441466420, -15.04371018346111377 ) ) ;
#5368 = LINE ( 'NONE', #67154, #61137 ) ;
#5369 = CARTESIAN_POINT ( 'NONE',  ( 83.36188103862497201, 44.67940999285032433, -9.129105138708005995 ) ) ;
#5370 = CARTESIAN_POINT ( 'NONE',  ( 162.5447505464307483, 273.3239273621815073, 14.91589735394761007 ) ) ;
#5372 = CARTESIAN_POINT ( 'NONE',  ( 88.38522318935277156, 43.99954571450756191, 2.365518284841155783 ) ) ;
#5371 = CARTESIAN_POINT ( 'NONE',  ( -16.90171517502901466, 170.2369531367911293, -4.594050593750048428 ) ) ;
#5373 = CARTESIAN_POINT ( 'NONE',  ( 188.3993081743329014, 296.6400551805262467, 8.121699605044829795 ) ) ;
#5374 = VERTEX_POINT ( 'NONE', #10791 ) ;
#5375 = ORIENTED_EDGE ( 'NONE', *, *, #4862, .T. ) ;
#5376 = FACE_OUTER_BOUND ( 'NONE', #49831, .T. ) ;
#5377 = CARTESIAN_POINT ( 'NONE',  ( 189.8395658503075367, 274.1636632147208843, -15.63209073522486214 ) ) ;
#5378 = AXIS2_PLACEMENT_3D ( 'NONE', #72081, #16858, #72592 ) ;
#5379 = CARTESIAN_POINT ( 'NONE',  ( 85.74702290878657607, 48.70847181056628727, -12.40582123554878891 ) ) ;
#5380 = CARTESIAN_POINT ( 'NONE',  ( 171.6531670106267029, 289.5256590595021748, 2.674700294240007103 ) ) ;
#5381 = DIRECTION ( 'NONE',  ( 0.1237105541964823863, -0.9923183454821336014, 0.000000000000000000 ) ) ;
#5382 = CARTESIAN_POINT ( 'NONE',  ( 84.16162000085680006, 46.04706940539106341, 10.25047128361154058 ) ) ;
#5383 = DIRECTION ( 'NONE',  ( 0.000000000000000000, 0.000000000000000000, 1.000000000000000000 ) ) ;
#5384 = EDGE_CURVE ( 'NONE', #72718, #30899, #63974, .T. ) ;
#5385 = CARTESIAN_POINT ( 'NONE',  ( 0.4998960083233069396, 183.3464784336661637, 1.353441290958777525E-15 ) ) ;
#5386 = CARTESIAN_POINT ( 'NONE',  ( 100.9591899430832029, 229.0958772461660260, -9.188101187500095079 ) ) ;
#5387 = CARTESIAN_POINT ( 'NONE',  ( 44.53222222597941027, 196.5177522451418781, -10.00000000000009592 ) ) ;
#5388 = CARTESIAN_POINT ( 'NONE',  ( 186.7556369116643680, 295.8656198945773781, -7.669303673011643063 ) ) ;
#5389 = CARTESIAN_POINT ( 'NONE',  ( 78.92796571603908262, 55.80079471467821861, 16.12519358965519345 ) ) ;
#5390 = VECTOR ( 'NONE', #56746, 1000.000000000000114 ) ;
#5391 = ADVANCED_FACE ( 'NONE', ( #94917 ), #95931, .F. ) ;
#5392 = CARTESIAN_POINT ( 'NONE',  ( 177.4587666978972322, 282.9167551205503628, -14.35547426222066925 ) ) ;
#5393 = CARTESIAN_POINT ( 'NONE',  ( 78.16852457591994607, 54.24206277777997798, -15.97971777959419271 ) ) ;
#5394 = CARTESIAN_POINT ( 'NONE',  ( 193.8603219414924013, 294.8710681561126989, 15.36476279452078586 ) ) ;
#5395 = CARTESIAN_POINT ( 'NONE',  ( 183.2664581031647231, 274.6986942775652665, 16.36951637877005084 ) ) ;
#5396 = CARTESIAN_POINT ( 'NONE',  ( 147.8819534105757043, 274.5079385007862811, -9.338341377131436971 ) ) ;
#5397 = EDGE_CURVE ( 'NONE', #79979, #87041, #68336, .T. ) ;
#5398 = CARTESIAN_POINT ( 'NONE',  ( 84.14828671478454680, 50.48813722287673045, 13.74412682973423649 ) ) ;
#5399 = CARTESIAN_POINT ( 'NONE',  ( 193.1215250612204102, 265.4992790482471605, 7.789832503989316592 ) ) ;
#5400 = CARTESIAN_POINT ( 'NONE',  ( -19.51131409799570093, 93.06655697632794499, 59.99999999999999289 ) ) ;
#5401 = CARTESIAN_POINT ( 'NONE',  ( 184.4954910655095546, 268.6554621394339506, -15.49256567782061467 ) ) ;
#5402 = B_SPLINE_CURVE_WITH_KNOTS ( 'NONE', 3,
 ( #72318, #11016, #19120, #60805, #91765, #84669, #37259, #13001, #60047, #50967, #4376, #13974, #98598, #5380, #51975, #51470, #52960, #81919, #21575, #6376, #82915, #11994, #60543, #29180, #4893, #13489, #68157, #91012, #66182, #52459, #27693, #12495, #82438, #67668, #43860, #74802, #35775, #66670, #44359, #90015, #97606, #43362, #28173, #99084, #29666, #75292, #36266, #59045, #83404, #91498, #22061, #42851 ),
 .UNSPECIFIED., .F., .F.,
 ( 4, 2, 2, 2, 2, 2, 2, 2, 2, 2, 2, 2, 2, 2, 2, 2, 2, 2, 2, 2, 2, 2, 2, 2, 2, 4 ),
 ( 0.0007237080175806911249, 0.001215060144269388548, 0.001706412270958085863, 0.001952088334302373371, 0.002197764397646660879, 0.002320602429318732209, 0.002443440460990803538, 0.002566278492662874867, 0.002689116524334946197, 0.002934792587679060667, 0.003180468651023176004, 0.003671820777711521169, 0.004654525031088134306, 0.005637229284464748309, 0.006128581411153092608, 0.006374257474497301186, 0.006619933537841508897, 0.006681352553677620022, 0.006742771569513730280, 0.006804190585349841405, 0.006865609601185951663, 0.007111285664530410909, 0.007602637791219313788, 0.008093989917908217535, 0.008339665981252667240, 0.008585342044597118680 ),
 .UNSPECIFIED. ) ;
#5403 = CARTESIAN_POINT ( 'NONE',  ( -36.83782344121361518, 37.72751643289125667, 59.99999999999999289 ) ) ;
#5404 = CARTESIAN_POINT ( 'NONE',  ( 157.7632566947985708, 282.3764601569879460, -1.694678876849560645 ) ) ;
#5405 = CARTESIAN_POINT ( 'NONE',  ( 85.85769841670953895, 226.5024278399160664, -9.188101187500093303 ) ) ;
#5406 = FACE_OUTER_BOUND ( 'NONE', #3133, .T. ) ;
#5407 = CARTESIAN_POINT ( 'NONE',  ( 190.8264243556038195, 300.1259329198319961, 8.466983560044813117 ) ) ;
#5408 = CARTESIAN_POINT ( 'NONE',  ( 47.74604483422196921, 186.8262482093457777, 3.021315404115420679E-15 ) ) ;
#5410 = CARTESIAN_POINT ( 'NONE',  ( 152.4958592292019830, 266.5164192015877234, 16.46101990066986431 ) ) ;
#5409 = CARTESIAN_POINT ( 'NONE',  ( 157.6673516573649181, 257.5591315650518141, 16.79781451397666103 ) ) ;
#5411 = CARTESIAN_POINT ( 'NONE',  ( 149.0651262117185354, 272.4586230950732784, 12.81403047969042319 ) ) ;
#5412 = CARTESIAN_POINT ( 'NONE',  ( 199.2205425252482200, 285.5868937652708155, -18.05012564782189344 ) ) ;
#5413 = CARTESIAN_POINT ( 'NONE',  ( 80.52908760376209329, 44.46502938403837391, 11.36794461543396473 ) ) ;
#5414 = CARTESIAN_POINT ( 'NONE',  ( 34.45502471548058310, 41.93396525600392977, 2.839279412974139660 ) ) ;
#5415 = CARTESIAN_POINT ( 'NONE',  ( 147.3236643320416022, 275.4749235501183193, -5.185334239426818037 ) ) ;
#5416 = CARTESIAN_POINT ( 'NONE',  ( 176.8917175299031896, 289.5346434493817469, -10.53293604869262978 ) ) ;
#5417 = ORIENTED_EDGE ( 'NONE', *, *, #92946, .F. ) ;
#5418 = CARTESIAN_POINT ( 'NONE',  ( 28.84566271970979301, 17.44966523072494979, -2.296566073217252530E-15 ) ) ;
#5419 = DIRECTION ( 'NONE',  ( 0.8660254037844377084, 0.5000000000000015543, 0.000000000000000000 ) ) ;
#5420 = CARTESIAN_POINT ( 'NONE',  ( 147.3715240516018810, 275.3920280842035595, -3.728968767617475866 ) ) ;
#5421 = CARTESIAN_POINT ( 'NONE',  ( 191.1350110915517462, 287.5662594520668449, -15.83302594719356371 ) ) ;
#5422 = ORIENTED_EDGE ( 'NONE', *, *, #34996, .F. ) ;
#5423 = LINE ( 'NONE', #36305, #59896 ) ;
#5424 = CARTESIAN_POINT ( 'NONE',  ( 76.00688113039353766, 65.27918228371470377, -14.45284717766215721 ) ) ;
#5426 = EDGE_CURVE ( 'NONE', #91683, #85466, #47798, .T. ) ;
#5425 = CARTESIAN_POINT ( 'NONE',  ( 157.5967295993894481, 268.7214701990851609, 15.68487696739332193 ) ) ;
#5427 = CARTESIAN_POINT ( 'NONE',  ( -22.85267942241863537, 23.13820207187275457, 177.5919119679930134 ) ) ;
#5428 = CARTESIAN_POINT ( 'NONE',  ( 147.2464435575442110, 242.4865022471901455, 1.119607411625061291E-15 ) ) ;
#5429 = CARTESIAN_POINT ( 'NONE',  ( 88.27857211938396631, 44.33912310488177866, -2.307176908786845893 ) ) ;
#5430 = VERTEX_POINT ( 'NONE', #64987 ) ;
#5431 = CARTESIAN_POINT ( 'NONE',  ( 190.5496216836923224, 298.9665820173917155, -8.014846329333149555 ) ) ;
#5432 = ORIENTED_EDGE ( 'NONE', *, *, #7896, .F. ) ;
#5433 = CARTESIAN_POINT ( 'NONE',  ( 196.7937303734090904, 265.3195474433538266, -4.517652853299265026 ) ) ;
#5434 = CARTESIAN_POINT ( 'NONE',  ( 83.28320137151804659, 41.40174392785183954, 0.7055483525344276030 ) ) ;
#5435 = EDGE_CURVE ( 'NONE', #79763, #15038, #57746, .T. ) ;
#5436 = ORIENTED_EDGE ( 'NONE', *, *, #15521, .T. ) ;
#5437 = CARTESIAN_POINT ( 'NONE',  ( 181.8097039409798299, 290.8543075322054392, -10.92870535220637684 ) ) ;
#5438 = ORIENTED_EDGE ( 'NONE', *, *, #93934, .F. ) ;
#5439 = CARTESIAN_POINT ( 'NONE',  ( 41.59134429584264581, 201.4865022471903160, 10.00000000000009415 ) ) ;
#5440 = CARTESIAN_POINT ( 'NONE',  ( 12.91273316327571052, 9.583808731787851087, 6.180339887498953466 ) ) ;
#5441 = CARTESIAN_POINT ( 'NONE',  ( 157.6621077668482087, 257.9721149867314125, -16.69158026131348294 ) ) ;
#5442 = CARTESIAN_POINT ( 'NONE',  ( 87.81919554331292943, 44.17710153608190637, -4.445631852975250098 ) ) ;
#5443 = FACE_OUTER_BOUND ( 'NONE', #92756, .T. ) ;
#5444 = AXIS2_PLACEMENT_3D ( 'NONE', #29706, #59589, #36800 ) ;
#5445 = CARTESIAN_POINT ( 'NONE',  ( 33.80247542503471436, 34.91421378149921395, 9.188101187500008038 ) ) ;
#5446 = CARTESIAN_POINT ( 'NONE',  ( 73.05987329793948959, 60.57830585426727055, -15.15309607717232687 ) ) ;
#5447 = CARTESIAN_POINT ( 'NONE',  ( -65.03992292888628413, 39.77302590755693501, 10.00000000000000000 ) ) ;
#5448 = CARTESIAN_POINT ( 'NONE',  ( 87.63520241360411944, 45.47292483007888109, 6.761783866543302324 ) ) ;
#5449 = VERTEX_POINT ( 'NONE', #50269 ) ;
#5450 = ORIENTED_EDGE ( 'NONE', *, *, #20114, .T. ) ;
#5451 = CARTESIAN_POINT ( 'NONE',  ( 87.14453225490829880, 46.27907944775106586, -9.173786573548373013 ) ) ;
#5453 = CARTESIAN_POINT ( 'NONE',  ( 162.4144876147732077, 272.5436428348735944, -16.23799951425711185 ) ) ;
#5452 = DIRECTION ( 'NONE',  ( 0.4556638457577371626, 0.000000000000000000, -0.8901519306664841258 ) ) ;
#5454 = CYLINDRICAL_SURFACE ( 'NONE', #82197, 10.00000000000010658 ) ;
#5455 = CARTESIAN_POINT ( 'NONE',  ( 43.53831125515428369, 65.97156238185917232, -10.00000000000000000 ) ) ;
#5456 = AXIS2_PLACEMENT_3D ( 'NONE', #15973, #45855, #54449 ) ;
#5457 = CARTESIAN_POINT ( 'NONE',  ( 71.03830642738165579, 61.94422969780909938, -14.15059485863699607 ) ) ;
#5458 = CARTESIAN_POINT ( 'NONE',  ( 82.16240693639510084, 40.80627634428258688, 1.120954036452832980 ) ) ;
#5459 = CARTESIAN_POINT ( 'NONE',  ( 167.5902884827328023, 286.2268049185996688, -4.744512013060059097 ) ) ;
#5460 = CARTESIAN_POINT ( 'NONE',  ( 77.02134436793002692, 63.41470467299149760, -15.46275534251473438 ) ) ;
#5461 = VECTOR ( 'NONE', #57892, 1000.000000000000114 ) ;
#5462 = CARTESIAN_POINT ( 'NONE',  ( 78.86219776201926379, 59.55369065033505649, 16.50996775951927020 ) ) ;
#5463 = CARTESIAN_POINT ( 'NONE',  ( 98.52331994705694740, 233.8149278399160949, -9.188101187500095079 ) ) ;
#5464 = ORIENTED_EDGE ( 'NONE', *, *, #26433, .T. ) ;
#5465 = CARTESIAN_POINT ( 'NONE',  ( 148.5272680744187141, 275.3902207161408455, -7.185975151065171929 ) ) ;
#5466 = CARTESIAN_POINT ( 'NONE',  ( 191.7774707643941667, 275.0877732711670092, 16.73782656324233642 ) ) ;
#5467 = VERTEX_POINT ( 'NONE', #89811 ) ;
#5468 = ORIENTED_EDGE ( 'NONE', *, *, #67897, .F. ) ;
#5469 = CARTESIAN_POINT ( 'NONE',  ( 87.17064494550572817, 46.10325694261842244, -8.264880744854202987 ) ) ;
#5470 = CARTESIAN_POINT ( 'NONE',  ( 196.5452668095620368, 286.2544686769650752, -17.73926526098317069 ) ) ;
#5471 = CARTESIAN_POINT ( 'NONE',  ( 157.5042325173297684, 257.8416622032797818, 16.70595240278738203 ) ) ;
#5472 = CARTESIAN_POINT ( 'NONE',  ( 68.26658298682237103, 69.66286806335898518, 4.977088283642358668 ) ) ;
#5473 = EDGE_CURVE ( 'NONE', #99839, #36195, #16670, .T. ) ;
#5474 = CARTESIAN_POINT ( 'NONE',  ( 73.91058561509676395, 55.40454524342042930, -16.11566030560718588 ) ) ;
#5475 = EDGE_LOOP ( 'NONE', ( #81507, #2444, #12685, #36000 ) ) ;
#5476 = ADVANCED_FACE ( 'NONE', ( #5664 ), #50761, .F. ) ;
#5477 = VERTEX_POINT ( 'NONE', #12795 ) ;
#5479 = ADVANCED_FACE ( 'NONE', ( #20384 ), #4680, .F. ) ;
#5478 = FACE_OUTER_BOUND ( 'NONE', #2583, .T. ) ;
#5480 = ORIENTED_EDGE ( 'NONE', *, *, #76353, .F. ) ;
#5481 = DIRECTION ( 'NONE',  ( -0.3297783986044530158, -0.8484238185761759921, -0.4140328874455538322 ) ) ;
#5482 = CARTESIAN_POINT ( 'NONE',  ( 153.3409266555433703, 265.4419702791891496, 16.17400560137409116 ) ) ;
#5483 = CARTESIAN_POINT ( 'NONE',  ( 40.70814378237798081, 60.14496435084704018, 10.00000000000000000 ) ) ;
#5485 = CARTESIAN_POINT ( 'NONE',  ( 199.2082368456953532, 284.5671209592410946, 17.30778797021233828 ) ) ;
#5484 = CARTESIAN_POINT ( 'NONE',  ( 139.7681268980558968, 245.3768266524160140, -9.188101187500091527 ) ) ;
#5486 = DIRECTION ( 'NONE',  ( -0.7061384650677096086, -0.7080737730998225565, 0.000000000000000000 ) ) ;
#5487 = ORIENTED_EDGE ( 'NONE', *, *, #80178, .F. ) ;
#5488 = CARTESIAN_POINT ( 'NONE',  ( -167.0327448629461742, 42.61639673982678289, -21.50000000000000000 ) ) ;
#5489 = FACE_OUTER_BOUND ( 'NONE', #68693, .T. ) ;
#5490 = CARTESIAN_POINT ( 'NONE',  ( 82.53374931873412379, 40.90496126830478829, -3.689593570638290743 ) ) ;
#5491 = CARTESIAN_POINT ( 'NONE',  ( 172.9708666340684999, 251.4732952470851615, -0.2584728925942609279 ) ) ;
#5492 = DIRECTION ( 'NONE',  ( 0.000000000000000000, 0.000000000000000000, 1.000000000000000000 ) ) ;
#5493 = CARTESIAN_POINT ( 'NONE',  ( 72.14269493036653103, 72.23228066185846785, 3.937576401637835843 ) ) ;
#5494 = CARTESIAN_POINT ( 'NONE',  ( 82.34150913319267318, 40.80060775105380344, -3.714726174206739895 ) ) ;
#5495 = DIRECTION ( 'NONE',  ( 0.4999999999999992784, -0.8660254037844390407, 0.000000000000000000 ) ) ;
#5496 = CARTESIAN_POINT ( 'NONE',  ( 79.04312205966233762, 46.85810355056803900, 13.20029221486031368 ) ) ;
#5497 = ADVANCED_FACE ( 'NONE', ( #12287 ), #73103, .F. ) ;
#5498 = CARTESIAN_POINT ( 'NONE',  ( 68.82403863051547432, 70.06653083274885319, -2.813536757197747651 ) ) ;
#5499 = CARTESIAN_POINT ( 'NONE',  ( 61.44712799118319424, 194.0327760586659451, 1.948934522072303157E-15 ) ) ;
#5500 = CARTESIAN_POINT ( 'NONE',  ( 206.3454060440500086, 273.2462681537123785, -9.268083217908118954 ) ) ;
#5501 = CYLINDRICAL_SURFACE ( 'NONE', #49922, 70.00000000000002842 ) ;
#5502 = CARTESIAN_POINT ( 'NONE',  ( 208.3226489551340990, 269.8215829728092103, -1.240262689467544366 ) ) ;
#5503 = APPLICATION_CONTEXT ( 'automotive_design' ) ;
#5504 = CARTESIAN_POINT ( 'NONE',  ( 66.35881563399601646, 68.82796675089451810, 1.446283243008493313 ) ) ;
#5506 = DIRECTION ( 'NONE',  ( -0.000000000000000000, 0.000000000000000000, -1.000000000000000000 ) ) ;
#5505 = CARTESIAN_POINT ( 'NONE',  ( 73.27328646083024921, 70.16270934360545652, -9.274526489422589393 ) ) ;
#5507 = CARTESIAN_POINT ( 'NONE',  ( 79.94359230559648211, 205.4155109091896065, 2.679491924311254714 ) ) ;
#5508 = CARTESIAN_POINT ( 'NONE',  ( 80.86586985908986946, 155.7185146834693512, 0.000000000000000000 ) ) ;
#5509 = CARTESIAN_POINT ( 'NONE',  ( 71.71174882302005926, 58.93038559421764688, -15.88944412480316259 ) ) ;
#5510 =( BOUNDED_CURVE ( )  B_SPLINE_CURVE ( 2, ( #68750, #67769, #90107, #52064, #53548, #60142, #45935, #7449, #91104, #83007, #29763, #84013, #20680 ),
 .UNSPECIFIED., .F., .T. ) 
 B_SPLINE_CURVE_WITH_KNOTS ( ( 3, 2, 2, 2, 2, 2, 3 ),
 ( 0.6375000000000000666, 0.6400000000000000133, 0.6450000000000000178, 0.6500000000000000222, 0.6550000000000000266, 0.6600000000000000311, 0.6625000000000000888 ),
 .UNSPECIFIED. ) 
 CURVE ( )  GEOMETRIC_REPRESENTATION_ITEM ( )  RATIONAL_B_SPLINE_CURVE ( ( 0.9755282581475767101, 0.9755282581475772652, 1.000000000000000000, 0.9510565162951535312, 1.000000000000000000, 0.9510565162951535312, 1.000000000000000000, 0.9510565162951535312, 1.000000000000000000, 0.9510565162951535312, 1.000000000000000000, 0.9755282581475761550, 0.9755282581475767101 ) ) 
 REPRESENTATION_ITEM ( '' )  );
#5511 = CARTESIAN_POINT ( 'NONE',  ( 157.6831565925140239, 270.7739412695440819, -15.91244755415583612 ) ) ;
#5512 = CARTESIAN_POINT ( 'NONE',  ( 72.28940563590052193, 72.06213100273473060, 3.327866248218421585 ) ) ;
#5513 = AXIS2_PLACEMENT_3D ( 'NONE', #83597, #74495, #67864 ) ;
#5514 = CARTESIAN_POINT ( 'NONE',  ( 24.99226373304320958, 194.4244531367911293, -4.594050593750046652 ) ) ;
#5515 = CARTESIAN_POINT ( 'NONE',  ( 196.0727848089514964, 291.0389700598140621, 17.56388901715066808 ) ) ;
#5517 = LINE ( 'NONE', #29319, #62180 ) ;
#5516 = VECTOR ( 'NONE', #51919, 1000.000000000000000 ) ;
#5518 = CARTESIAN_POINT ( 'NONE',  ( 80.95490552855073929, 50.32613945632080288, -14.46254378829325660 ) ) ;
#5519 = CARTESIAN_POINT ( 'NONE',  ( 71.91886814437489761, 72.60555707853946217, -1.127020781340661193 ) ) ;
#5520 = CARTESIAN_POINT ( 'NONE',  ( 53.16558651961199899, 195.3768266524160140, 9.188101187500096856 ) ) ;
#5521 = EDGE_CURVE ( 'NONE', #36208, #25628, #92677, .T. ) ;
#5522 = CARTESIAN_POINT ( 'NONE',  ( 20.05074681235918277, 34.68290643055188127, 3.479690158560446702E-15 ) ) ;
#5523 = CARTESIAN_POINT ( 'NONE',  ( 199.0756812798354645, 285.8378008023734083, -18.45377816087746936 ) ) ;
#5524 = CARTESIAN_POINT ( 'NONE',  ( 196.9098758191317700, 289.5890858996224324, -16.54412079817003800 ) ) ;
#5525 = CARTESIAN_POINT ( 'NONE',  ( 7.453652514893187586, 19.70171378149916919, -9.188101187500004485 ) ) ;
#5526 = CARTESIAN_POINT ( 'NONE',  ( 202.9510194980842641, 270.0555581978532587, -6.495183321546498689 ) ) ;
#5527 = CARTESIAN_POINT ( 'NONE',  ( 174.9787010148468767, 292.1454046610912769, 2.108760379847960387 ) ) ;
#5528 = CARTESIAN_POINT ( 'NONE',  ( 179.7724920804510873, 276.7831429704333459, 16.31391713246987862 ) ) ;
#5529 = CARTESIAN_POINT ( 'NONE',  ( 73.12786766706317110, 63.39850902397307664, 14.05984965185791502 ) ) ;
#5530 = CARTESIAN_POINT ( 'NONE',  ( 86.30977306730703447, 47.58285218899635538, -10.62438056216880611 ) ) ;
#5531 = B_SPLINE_SURFACE_WITH_KNOTS ( 'NONE', 3, 1, ( 
 ( #48658, #79591 ),
 ( #74350, #10155 ),
 ( #88205, #63344 ),
 ( #78562, #33968 ),
 ( #64853, #24837 ),
 ( #4938, #40022 ),
 ( #41021, #70962 ),
 ( #41531, #1563 ),
 ( #49153, #71959 ),
 ( #80088, #33446 ),
 ( #55711, #17235 ),
 ( #48142, #64343 ),
 ( #79086, #95307 ),
 ( #40529, #71464 ),
 ( #10655, #29712 ),
 ( #51513, #60588 ),
 ( #91544, #75334 ),
 ( #91057, #5917 ),
 ( #53498, #29225 ),
 ( #37794, #84452 ),
 ( #98135, #28720 ),
 ( #67211, #22112 ),
 ( #53005, #83956 ),
 ( #90571, #43904 ),
 ( #68697, #99628 ),
 ( #36806, #45881 ),
 ( #97646, #36306 ),
 ( #13532, #37302 ),
 ( #82479, #60093 ),
 ( #22612, #75838 ),
 ( #13043, #14993 ),
 ( #21622, #59594 ),
 ( #67718, #44898 ),
 ( #38291, #21139 ) ),
 .UNSPECIFIED., .T., .F., .F.,
 ( 4, 2, 2, 2, 2, 2, 2, 2, 2, 2, 2, 2, 2, 2, 2, 2, 4 ),
 ( 2, 2 ),
 ( 0.000000000000000000, 0.06250000000000000000, 0.1250000000000000000, 0.1875000000000000000, 0.2500000000000000000, 0.3125000000000000000, 0.3750000000000000000, 0.4375000000000000000, 0.5000000000000000000, 0.5625000000000000000, 0.6250000000000000000, 0.6875000000000000000, 0.7500000000000000000, 0.8125000000000000000, 0.8750000000000000000, 0.9375000000000000000, 1.000000000000000000 ),
 ( 0.000000000000000000, 1.000000000000000000 ),
 .UNSPECIFIED. ) ;
#5532 = CARTESIAN_POINT ( 'NONE',  ( 163.2883354864554519, 256.0504063331084694, -14.91619366091854282 ) ) ;
#5533 = LINE ( 'NONE', #28837, #72022 ) ;
#5534 = CARTESIAN_POINT ( 'NONE',  ( 90.16093569141993669, 222.8615022471902591, -10.00000000000009592 ) ) ;
#5535 = CARTESIAN_POINT ( 'NONE',  ( 184.6894110187365641, 293.7322318964822330, -10.88359728165448814 ) ) ;
#5536 = CARTESIAN_POINT ( 'NONE',  ( 163.5869523275859763, 268.7237500424058680, -16.42576965565886482 ) ) ;
#5537 = VERTEX_POINT ( 'NONE', #35571 ) ;
#5538 = CARTESIAN_POINT ( 'NONE',  ( 59.90443346675090908, 196.2048013555409796, 4.594050593750051981 ) ) ;
#5539 = ORIENTED_EDGE ( 'NONE', *, *, #75864, .F. ) ;
#5540 = DIRECTION ( 'NONE',  ( 0.4635919272833914917, -0.8029647720336136052, 0.3746065934159158450 ) ) ;
#5541 = CARTESIAN_POINT ( 'NONE',  ( 147.0538900202505488, 275.9421863647172017, 5.192507380313251986 ) ) ;
#5542 = LINE ( 'NONE', #59727, #4602 ) ;
#5543 = ORIENTED_EDGE ( 'NONE', *, *, #98251, .F. ) ;
#5544 = DIRECTION ( 'NONE',  ( 0.2649596321166021728, -0.4589235447807153423, -0.8480480961564252906 ) ) ;
#5545 = CARTESIAN_POINT ( 'NONE',  ( 79.16669127013743434, 45.83075451395571775, -13.07232462202737366 ) ) ;
#5546 = CARTESIAN_POINT ( 'NONE',  ( 47.92671612011951510, 80.40884667711614497, 10.00000000000000000 ) ) ;
#5547 = CARTESIAN_POINT ( 'NONE',  ( 186.3306027636789679, 263.0363486839914913, 11.47262423782134277 ) ) ;
#5548 = CARTESIAN_POINT ( 'NONE',  ( 86.51323263660401608, 47.18218208451981610, -10.10578519018193333 ) ) ;
#5549 = CARTESIAN_POINT ( 'NONE',  ( 205.0722772166587902, 275.4513919673344731, 14.18415804594472185 ) ) ;
#5550 = EDGE_LOOP ( 'NONE', ( #85454, #64015, #22018, #26631 ) ) ;
#5551 = CARTESIAN_POINT ( 'NONE',  ( 22.77687932801360660, 15.01110640527292261, 2.839279412974134775 ) ) ;
#5552 = CARTESIAN_POINT ( 'NONE',  ( 68.94535929113044403, 64.35437313888181166, 12.52085547237679286 ) ) ;
#5553 = CARTESIAN_POINT ( 'NONE',  ( 71.72726194589085935, 70.29524283496927239, -6.982538226112097846 ) ) ;
#5554 = CARTESIAN_POINT ( 'NONE',  ( 7.816353548249534100, 181.9865022471903160, 10.00000000000009415 ) ) ;
#5555 = ORIENTED_EDGE ( 'NONE', *, *, #82689, .T. ) ;
#5556 = CARTESIAN_POINT ( 'NONE',  ( 181.5631808996132008, 283.6781476641766631, 14.96027398286517496 ) ) ;
#5557 = CARTESIAN_POINT ( 'NONE',  ( 167.6885389621171782, 262.0286974587709210, 16.15245462749480154 ) ) ;
#5558 = CARTESIAN_POINT ( 'NONE',  ( 206.4484807199597753, 273.0677375780628608, -9.220527398138528952 ) ) ;
#5559 = ORIENTED_EDGE ( 'NONE', *, *, #81366, .T. ) ;
#5561 = DIRECTION ( 'NONE',  ( 0.000000000000000000, 0.000000000000000000, 1.000000000000000000 ) ) ;
#5560 = CARTESIAN_POINT ( 'NONE',  ( 162.1541172097854826, 283.1473020987244809, -3.122785026967457966 ) ) ;
#5562 = CARTESIAN_POINT ( 'NONE',  ( 181.7882433779857081, 293.0516533115879270, -9.677455024747617429 ) ) ;
#5563 = CARTESIAN_POINT ( 'NONE',  ( 66.08237217692345666, 68.53364664378331383, -2.343639106938055328 ) ) ;
#5564 = CARTESIAN_POINT ( 'NONE',  ( 159.8416255366773839, 253.7931787365127434, 16.77980437810719394 ) ) ;
#5565 = CARTESIAN_POINT ( 'NONE',  ( -22.42236680055709641, 157.8615022471902591, 0.000000000000000000 ) ) ;
#5566 = CARTESIAN_POINT ( 'NONE',  ( -22.42236680055709641, 157.8615022471902591, 0.000000000000000000 ) ) ;
#5567 = CARTESIAN_POINT ( 'NONE',  ( 118.5230073417626073, 248.4244531367911293, -4.594050593750046652 ) ) ;
#5568 = CYLINDRICAL_SURFACE ( 'NONE', #58572, 10.00000000000001066 ) ;
#5569 = ORIENTED_EDGE ( 'NONE', *, *, #23704, .T. ) ;
#5570 = CARTESIAN_POINT ( 'NONE',  ( 173.3549678798564742, 265.3355617639286379, 16.05511268515816781 ) ) ;
#5571 = DIRECTION ( 'NONE',  ( -0.9762722099447388446, -0.2165469281463391626, 0.000000000000000000 ) ) ;
#5572 = ORIENTED_EDGE ( 'NONE', *, *, #25630, .F. ) ;
#5573 = CARTESIAN_POINT ( 'NONE',  ( 82.39721099668476256, 40.42262220707492304, 1.474573639734337860 ) ) ;
#5574 = VERTEX_POINT ( 'NONE', #36552 ) ;
#5575 = ORIENTED_EDGE ( 'NONE', *, *, #14158, .T. ) ;
#5576 = CARTESIAN_POINT ( 'NONE',  ( 159.7897726928491409, 253.8829904965402875, 16.83923858130328810 ) ) ;
#5577 = CARTESIAN_POINT ( 'NONE',  ( -32.04500338604974985, 25.44370296803430520, -10.00000000000000000 ) ) ;
#5578 = CARTESIAN_POINT ( 'NONE',  ( 68.04987750350953490, 222.3464784336661637, 1.353441290958777525E-15 ) ) ;
#5579 = CARTESIAN_POINT ( 'NONE',  ( 16.74724052122864393, 187.1427522451419350, 10.00000000000009415 ) ) ;
#5580 = CARTESIAN_POINT ( 'NONE',  ( 81.86683804372771078, 55.45883585039843666, 16.28524382593451136 ) ) ;
#5581 = CARTESIAN_POINT ( 'NONE',  ( 155.6126298223767890, 261.1180141786725244, 18.15400560664037855 ) ) ;
#5582 = EDGE_CURVE ( 'NONE', #6163, #74234, #97394, .T. ) ;
#5583 = CARTESIAN_POINT ( 'NONE',  ( 171.9941656342203089, 276.8346263436580443, 16.42768944293989719 ) ) ;
#5584 = ORIENTED_EDGE ( 'NONE', *, *, #60442, .T. ) ;
#5585 = VECTOR ( 'NONE', #94859, 1000.000000000000000 ) ;
#5586 = EDGE_CURVE ( 'NONE', #88849, #19800, #34782, .T. ) ;
#5587 = FACE_OUTER_BOUND ( 'NONE', #47590, .T. ) ;
#5588 = CARTESIAN_POINT ( 'NONE',  ( 152.8328714238065515, 265.9326969577624027, -16.29536156676786263 ) ) ;
#5589 = CARTESIAN_POINT ( 'NONE',  ( 155.1865148098964937, 261.8560670301561686, -16.99758927948949605 ) ) ;
#5590 = VERTEX_POINT ( 'NONE', #27962 ) ;
#5591 = CARTESIAN_POINT ( 'NONE',  ( 73.23646752216983202, 69.77611894600212850, -9.099901738753176872 ) ) ;
#5592 = CARTESIAN_POINT ( 'NONE',  ( 76.17161704303337899, 51.04481688019111374, -15.56989386545701848 ) ) ;
#5593 = ADVANCED_FACE ( 'NONE', ( #3695 ), #78121, .F. ) ;
#5594 = CARTESIAN_POINT ( 'NONE',  ( 174.2386054419784784, 253.2136311291264690, -7.745944249412784366 ) ) ;
#5595 = CIRCLE ( 'NONE', #20150, 60.00000000000001421 ) ;
#5596 = CARTESIAN_POINT ( 'NONE',  ( 174.8696466734779449, 292.3029143586743430, -1.153856708368909967 ) ) ;
#5597 = CARTESIAN_POINT ( 'NONE',  ( -78.71521058394759507, 57.86724000996476747, 10.00000000000000000 ) ) ;
#5598 = CARTESIAN_POINT ( 'NONE',  ( -29.38832164612380637, 94.71097215053278262, 44.55472784766640615 ) ) ;
#5599 = CARTESIAN_POINT ( 'NONE',  ( 81.62374368218522136, 41.76230689378201788, 5.959470817902202455 ) ) ;
#5600 = ORIENTED_EDGE ( 'NONE', *, *, #29657, .T. ) ;
#5601 = CARTESIAN_POINT ( 'NONE',  ( 164.4963285489318991, 245.7309966251440301, -6.672251175510283794 ) ) ;
#5602 = CARTESIAN_POINT ( 'NONE',  ( 147.5084024922618084, 243.7202760586659736, -5.415160957724236172E-17 ) ) ;
#5603 = ORIENTED_EDGE ( 'NONE', *, *, #97462, .T. ) ;
#5604 = LINE ( 'NONE', #53195, #83752 ) ;
#5605 = CARTESIAN_POINT ( 'NONE',  ( 182.0573489978566215, 257.5803797228366534, 6.639334650236212276 ) ) ;
#5606 = CARTESIAN_POINT ( 'NONE',  ( -4.300976545156382613, 36.43331849613671380, 59.99999999999999289 ) ) ;
#5607 = CARTESIAN_POINT ( 'NONE',  ( 72.73213343415878285, 70.95121167556251862, 7.670646158728287922 ) ) ;
#5608 = LINE ( 'NONE', #43603, #56674 ) ;
#5609 = EDGE_LOOP ( 'NONE', ( #17454, #71606, #16795, #31414 ) ) ;
#5610 = DIRECTION ( 'NONE',  ( 0.000000000000000000, -0.000000000000000000, -1.000000000000000000 ) ) ;
#5611 = CARTESIAN_POINT ( 'NONE',  ( 182.4299782848027291, 275.0440474321702595, -17.09684782076308807 ) ) ;
#5612 = CARTESIAN_POINT ( 'NONE',  ( 167.5444266783159435, 249.1640122146770011, -5.486574941136140637 ) ) ;
#5613 = CARTESIAN_POINT ( 'NONE',  ( 80.78918961562681034, 43.20779693872438543, -9.098606657379765039 ) ) ;
#5614 = CARTESIAN_POINT ( 'NONE',  ( 73.72378779666912862, 69.49084951233950846, -9.812509676730275743 ) ) ;
#5615 = CARTESIAN_POINT ( 'NONE',  ( 198.3653284636346541, 266.1659536649856932, 0.8111552996551663064 ) ) ;
#5616 = CARTESIAN_POINT ( 'NONE',  ( 147.5492216329511166, 275.0842468449245644, 4.751613690710122739 ) ) ;
#5617 = CARTESIAN_POINT ( 'NONE',  ( 182.8710648154623186, 280.6231348432476125, 16.78699077144874252 ) ) ;
#5618 = DIRECTION ( 'NONE',  ( 1.000000000000000000, 0.000000000000000000, 0.000000000000000000 ) ) ;
#5619 = CARTESIAN_POINT ( 'NONE',  ( 17.57657260583443559, 33.08080186712592763, -3.090169943749475845 ) ) ;
#5620 = LINE ( 'NONE', #14717, #59644 ) ;
#5621 = CARTESIAN_POINT ( 'NONE',  ( -19.65312891409030271, 93.06504152958497400, 10.00000000000000888 ) ) ;
#5622 = CARTESIAN_POINT ( 'NONE',  ( 178.7600897929267774, 254.1784503161647706, 4.743017227330367014 ) ) ;
#5623 = CARTESIAN_POINT ( 'NONE',  ( 159.6978881494930249, 254.0421391940632532, 15.34888828951022610 ) ) ;
#5624 = CARTESIAN_POINT ( 'NONE',  ( 76.28872632190459058, 51.00282802105012081, -16.03419075268624994 ) ) ;
#5625 = CARTESIAN_POINT ( 'NONE',  ( 135.5370584069941060, 262.3927522451419350, 2.944929066748280225E-16 ) ) ;
#5626 = B_SPLINE_CURVE_WITH_KNOTS ( 'NONE', 3,
 ( #52457, #82913, #257, #99574 ),
 .UNSPECIFIED., .F., .F.,
 ( 4, 4 ),
 ( 0.008863162062248396492, 0.01509767807619737633 ),
 .UNSPECIFIED. ) ;
#5627 = CARTESIAN_POINT ( 'NONE',  ( 174.4421927399967842, 284.4761513374891706, -12.08263559617888916 ) ) ;
#5628 = ORIENTED_EDGE ( 'NONE', *, *, #46192, .F. ) ;
#5629 = CARTESIAN_POINT ( 'NONE',  ( 66.80351077683091887, 68.15053363805938602, -6.532535086774335475 ) ) ;
#5630 = CARTESIAN_POINT ( 'NONE',  ( 150.6386650955079176, 269.7331738006648720, -15.06054658539322766 ) ) ;
#5631 = CARTESIAN_POINT ( 'NONE',  ( 3.531332017333847606, 172.8458772461660828, 9.188101187500095079 ) ) ;
#5632 = ADVANCED_FACE ( 'NONE', ( #98387 ), #85815, .T. ) ;
#5633 = CARTESIAN_POINT ( 'NONE',  ( 178.5281950170523544, 259.0983513684005288, -10.32239201220430225 ) ) ;
#5634 = CARTESIAN_POINT ( 'NONE',  ( 20.35638218401011912, 30.49103043416549497, -8.090169943749479842 ) ) ;
#5635 = DIRECTION ( 'NONE',  ( 0.4635919272833914917, -0.8029647720336136052, 0.3746065934159158450 ) ) ;
#5636 = CARTESIAN_POINT ( 'NONE',  ( 204.7242223814549504, 276.0542406257275161, -13.93608974681376189 ) ) ;
#5637 = FACE_OUTER_BOUND ( 'NONE', #49533, .T. ) ;
#5638 = LINE ( 'NONE', #28952, #88035 ) ;
#5640 = CARTESIAN_POINT ( 'NONE',  ( 66.11068853694163749, 215.6427522451419065, 10.00000000000009237 ) ) ;
#5639 = CARTESIAN_POINT ( 'NONE',  ( 196.2956918591910664, 269.5555983294441376, -10.79850100103040944 ) ) ;
#5641 = CARTESIAN_POINT ( 'NONE',  ( 75.58345210230092448, 53.75839974157640455, 16.53437228110026780 ) ) ;
#5642 = CARTESIAN_POINT ( 'NONE',  ( 150.8613910702043768, 269.3474010963252567, 15.19517615056406612 ) ) ;
#5643 = VECTOR ( 'NONE', #31115, 1000.000000000000114 ) ;
#5644 = EDGE_CURVE ( 'NONE', #1734, #46146, #23341, .T. ) ;
#5645 = CARTESIAN_POINT ( 'NONE',  ( 179.5028650301413791, 294.0833190536570214, 1.038326004487517551 ) ) ;
#5646 = CARTESIAN_POINT ( 'NONE',  ( 63.38631695775107033, 200.7365022471902023, 10.00000000000009592 ) ) ;
#5647 = DIRECTION ( 'NONE',  ( -0.000000000000000000, -0.000000000000000000, -1.000000000000000000 ) ) ;
#5648 = CARTESIAN_POINT ( 'NONE',  ( 181.7815785431583038, 276.1505370498239813, -17.81783396216490445 ) ) ;
#5649 = CARTESIAN_POINT ( 'NONE',  ( 17.27983239817682559, 168.5327760586659736, 1.948934522072303157E-15 ) ) ;
#5650 = CARTESIAN_POINT ( 'NONE',  ( 164.2838888460686064, 285.0926974262010276, 4.322335904415723462 ) ) ;
#5651 = EDGE_CURVE ( 'NONE', #82532, #52858, #64690, .T. ) ;
#5652 = CARTESIAN_POINT ( 'NONE',  ( 11.42479273068475010, 170.7365022471902307, 10.00000000000009948 ) ) ;
#5653 = CARTESIAN_POINT ( 'NONE',  ( 36.18707552304946518, 42.93396525600392977, 2.839279412974139660 ) ) ;
#5654 = CARTESIAN_POINT ( 'NONE',  ( 201.9062777989876452, 280.4778359209939254, -15.96862433567465622 ) ) ;
#5655 = CARTESIAN_POINT ( 'NONE',  ( 206.9408877595175511, 272.2148635675444552, 6.707071080545934372 ) ) ;
#5656 = CARTESIAN_POINT ( 'NONE',  ( 193.9401685343300699, 294.7327698005063326, 14.01047396938887069 ) ) ;
#5657 = CARTESIAN_POINT ( 'NONE',  ( 188.3428823685774489, 267.3304898084075489, 14.27533445868386508 ) ) ;
#5658 = LINE ( 'NONE', #83193, #78425 ) ;
#5659 = PLANE ( 'NONE',  #13232 ) ;
#5660 = CARTESIAN_POINT ( 'NONE',  ( 0.000000000000000000, 0.000000000000000000, 0.000000000000000000 ) ) ;
#5661 = CARTESIAN_POINT ( 'NONE',  ( 13.01786573420820226, 22.91421378149917842, 9.188101187500008038 ) ) ;
#5662 = CARTESIAN_POINT ( 'NONE',  ( 165.2720705891711930, 285.9514678962245853, -0.2691863636319293818 ) ) ;
#5663 = CARTESIAN_POINT ( 'NONE',  ( 82.79017490736518425, 53.74338802490922973, 15.39689667775746251 ) ) ;
#5664 = FACE_OUTER_BOUND ( 'NONE', #8960, .T. ) ;
#5665 = CARTESIAN_POINT ( 'NONE',  ( 194.3562588153086779, 294.0120802933159325, 14.11474987148825200 ) ) ;
#5666 = VERTEX_POINT ( 'NONE', #10167 ) ;
#5667 = FACE_OUTER_BOUND ( 'NONE', #21316, .T. ) ;
#5668 = CARTESIAN_POINT ( 'NONE',  ( 80.53812798300913300, 46.07492565378247207, -12.69342001902709072 ) ) ;
#5669 = CARTESIAN_POINT ( 'NONE',  ( 81.38935016679909040, 42.00105843850820975, 7.782619590129813858 ) ) ;
#5670 = CARTESIAN_POINT ( 'NONE',  ( 155.5995420464182644, 262.6346450740109617, -17.48312782858739567 ) ) ;
#5671 = VERTEX_POINT ( 'NONE', #47143 ) ;
#5672 = DIRECTION ( 'NONE',  ( 1.000000000000000000, -9.773927698932179522E-14, 0.000000000000000000 ) ) ;
#5673 = CARTESIAN_POINT ( 'NONE',  ( 71.10837680816226225, 221.8615022471903160, 5.000000000000046185 ) ) ;
#5674 = CARTESIAN_POINT ( 'NONE',  ( 66.45324346747356969, 68.19700524679973341, 4.520682066448438619 ) ) ;
#5675 = CARTESIAN_POINT ( 'NONE',  ( 202.9881971861223917, 279.0611244672630278, -15.16231470264511927 ) ) ;
#5676 = ORIENTED_EDGE ( 'NONE', *, *, #71364, .F. ) ;
#5677 = ORIENTED_EDGE ( 'NONE', *, *, #59489, .F. ) ;
#5679 = CARTESIAN_POINT ( 'NONE',  ( 204.5831314780710954, 276.2986172388744421, 13.28075685133257089 ) ) ;
#5678 = CARTESIAN_POINT ( 'NONE',  ( 44.10470679282203577, 121.9603419428074460, 177.5919119679930134 ) ) ;
#5680 = CARTESIAN_POINT ( 'NONE',  ( 192.5712965840290849, 297.1037255674836501, 11.03742858512898906 ) ) ;
#5681 = ORIENTED_EDGE ( 'NONE', *, *, #55658, .F. ) ;
#5682 = CARTESIAN_POINT ( 'NONE',  ( 190.9061255863007318, 299.9878863388391892, 7.497146773253707153 ) ) ;
#5683 = CARTESIAN_POINT ( 'NONE',  ( 80.46835216585913031, 57.85139773374410055, -16.60023610630909019 ) ) ;
#5684 = ORIENTED_EDGE ( 'NONE', *, *, #3217, .F. ) ;
#5685 = DIRECTION ( 'NONE',  ( -0.8614378286617615510, 0.5078630399532038098, 0.000000000000000000 ) ) ;
#5686 = CARTESIAN_POINT ( 'NONE',  ( 149.6890529486499872, 271.3779502865075983, -12.51465682618088593 ) ) ;
#5687 = AXIS2_PLACEMENT_3D ( 'NONE', #53264, #85208, #91307 ) ;
#5688 = ORIENTED_EDGE ( 'NONE', *, *, #59691, .T. ) ;
#5689 = CARTESIAN_POINT ( 'NONE',  ( 164.3493441216711517, 245.9855811210807417, 1.722120810491653664 ) ) ;
#5690 = CARTESIAN_POINT ( 'NONE',  ( 74.54230909194660626, 63.39697481222554387, 14.46401092357988638 ) ) ;
#5691 = ORIENTED_EDGE ( 'NONE', *, *, #71320, .F. ) ;
#5692 = ADVANCED_FACE ( 'NONE', ( #8655 ), #44410, .F. ) ;
#5693 = CARTESIAN_POINT ( 'NONE',  ( 174.6178695879432041, 276.7332269073218072, -16.18563341224413676 ) ) ;
#5694 = CARTESIAN_POINT ( 'NONE',  ( 172.3630404188492662, 263.8283741867592198, -15.51507169348583304 ) ) ;
#5695 = VERTEX_POINT ( 'NONE', #11181 ) ;
#5696 = CARTESIAN_POINT ( 'NONE',  ( 161.4666507344003605, 276.8280471058072294, -12.69379384225013219 ) ) ;
#5697 = LINE ( 'NONE', #4723, #48288 ) ;
#5698 = CARTESIAN_POINT ( 'NONE',  ( 192.8301672656986341, 296.6553483942417415, -13.40355799340913556 ) ) ;
#5699 = EDGE_LOOP ( 'NONE', ( #1337, #34998 ) ) ;
#5700 = VERTEX_POINT ( 'NONE', #98265 ) ;
#5701 = B_SPLINE_CURVE_WITH_KNOTS ( 'NONE', 3,
 ( #47796, #16410, #93957, #78231 ),
 .UNSPECIFIED., .F., .F.,
 ( 4, 4 ),
 ( 0.01771268258920854696, 0.02667042995983895728 ),
 .UNSPECIFIED. ) ;
#5702 = CARTESIAN_POINT ( 'NONE',  ( 73.34397377724333467, 69.83796661625983404, 9.136125499330086441 ) ) ;
#5703 = CARTESIAN_POINT ( 'NONE',  ( 190.5653282632609091, 300.5781646174276602, -5.775635208185608604 ) ) ;
#5704 = CARTESIAN_POINT ( 'NONE',  ( 82.59507288524608271, 53.86809943430368719, 15.83774089001703800 ) ) ;
#5705 = FACE_OUTER_BOUND ( 'NONE', #26331, .T. ) ;
#5706 = CARTESIAN_POINT ( 'NONE',  ( 192.1883190596398094, 297.7670620978826150, 12.41391288785556668 ) ) ;
#5707 = EDGE_CURVE ( 'NONE', #98408, #58918, #92961, .T. ) ;
#5708 = CARTESIAN_POINT ( 'NONE',  ( 146.6344723850759522, 276.6686390184297579, -0.5903044561608344898 ) ) ;
#5709 = EDGE_CURVE ( 'NONE', #38470, #53225, #43211, .T. ) ;
#5710 = CARTESIAN_POINT ( 'NONE',  ( 191.3413020738616410, 299.2341385521244774, -8.295023558158421295 ) ) ;
#5711 = ORIENTED_EDGE ( 'NONE', *, *, #4513, .T. ) ;
#5712 = CARTESIAN_POINT ( 'NONE',  ( 80.93527952113549873, 55.40317981316568563, -16.00817129638969760 ) ) ;
#5713 = CARTESIAN_POINT ( 'NONE',  ( 164.9171241593586217, 245.0021572482830550, 1.622680932994367220 ) ) ;
#5714 = CARTESIAN_POINT ( 'NONE',  ( 206.5117639185820906, 272.9581278627833285, 11.28485531511759099 ) ) ;
#5715 = CARTESIAN_POINT ( 'NONE',  ( 67.14930737951127071, 66.86624931644598746, 8.959152673661975541 ) ) ;
#5716 = CARTESIAN_POINT ( 'NONE',  ( 171.4584946453171597, 288.7452855169624399, 4.212295942657065417 ) ) ;
#5717 = CARTESIAN_POINT ( 'NONE',  ( 203.9648368022151601, 269.0477214045654364, 5.644613064108824574 ) ) ;
#5718 = CARTESIAN_POINT ( 'NONE',  ( 99.22679203974932705, 240.3464784336661637, 1.353441290958777327E-15 ) ) ;
#5719 = VERTEX_POINT ( 'NONE', #42534 ) ;
#5720 = CARTESIAN_POINT ( 'NONE',  ( 149.1807793072240997, 272.2583060576048979, -11.58584517200773867 ) ) ;
#5721 = CARTESIAN_POINT ( 'NONE',  ( 70.66892005943768140, 66.34497638887206961, 11.09326023022040530 ) ) ;
#5722 = CARTESIAN_POINT ( 'NONE',  ( 85.39557543340885104, 43.32749037753681165, 5.933140306914251205 ) ) ;
#5723 = CARTESIAN_POINT ( 'NONE',  ( 79.25911175516624496, 45.79062382720663749, 13.00842035693561272 ) ) ;
#5724 = CARTESIAN_POINT ( 'NONE',  ( 179.5668846297247683, 282.8373499615596529, -15.68793421486103945 ) ) ;
#5725 = CARTESIAN_POINT ( 'NONE',  ( 76.81923273335645774, 55.69533986730546360, -16.60453251139683317 ) ) ;
#5726 = VERTEX_POINT ( 'NONE', #88716 ) ;
#5727 = CARTESIAN_POINT ( 'NONE',  ( 163.4055107321044318, 247.6203485056908846, -10.24153090796238530 ) ) ;
#5728 = CYLINDRICAL_SURFACE ( 'NONE', #17698, 49.99999999999999289 ) ;
#5729 = CARTESIAN_POINT ( 'NONE',  ( 164.6460902696047128, 245.4716017159096566, -3.036414139157908476 ) ) ;
#5730 = CARTESIAN_POINT ( 'NONE',  ( 55.79055247517715799, 193.0177522451417929, 5.000000000000051514 ) ) ;
#5731 = CARTESIAN_POINT ( 'NONE',  ( 118.6048046409561465, 227.0327760586659451, 1.948934522072302763E-15 ) ) ;
#5732 = AXIS2_PLACEMENT_3D ( 'NONE', #5660, #50757, #73099 ) ;
#5733 = CARTESIAN_POINT ( 'NONE',  ( 151.3898985249405200, 268.4319993325432847, -14.65018536945715510 ) ) ;
#5734 = CARTESIAN_POINT ( 'NONE',  ( -19.65312891409030271, 93.06504152958497400, -10.00000000000000888 ) ) ;
#5735 = DIRECTION ( 'NONE',  ( -0.8660254037844387076, -0.4999999999999998890, -0.000000000000000000 ) ) ;
#5736 = CARTESIAN_POINT ( 'NONE',  ( 81.56753329430793542, 59.44520672954722329, 0.3596699001693225983 ) ) ;
#5737 = CARTESIAN_POINT ( 'NONE',  ( 27.26558041797736465, 195.7369531367911293, -4.594050593750048428 ) ) ;
#5738 = CARTESIAN_POINT ( 'NONE',  ( -14.65312891409034535, 84.40478749174073414, 0.000000000000000000 ) ) ;
#5740 = ORIENTED_EDGE ( 'NONE', *, *, #17098, .T. ) ;
#5739 = B_SPLINE_CURVE_WITH_KNOTS ( 'NONE', 3,
 ( #55637, #78480, #94696, #3486 ),
 .UNSPECIFIED., .F., .F.,
 ( 4, 4 ),
 ( 0.008210304326597597790, 0.01330689658320593181 ),
 .UNSPECIFIED. ) ;
#5741 = B_SPLINE_CURVE_WITH_KNOTS ( 'NONE', 3,
 ( #22597, #70178, #292, #91043 ),
 .UNSPECIFIED., .F., .F.,
 ( 4, 4 ),
 ( 0.01080220131554398416, 0.01688746497888054740 ),
 .UNSPECIFIED. ) ;
#5742 = CARTESIAN_POINT ( 'NONE',  ( 37.30626620713776731, 103.7037781670604204, 59.99999999999999289 ) ) ;
#5743 = CARTESIAN_POINT ( 'NONE',  ( 70.08719291027311726, 71.11346239110757494, -0.2046584118080456149 ) ) ;
#5744 = CARTESIAN_POINT ( 'NONE',  ( 76.54006514935311145, 51.19995672389920571, 16.04627313578386705 ) ) ;
#5745 = CYLINDRICAL_SURFACE ( 'NONE', #91974, 16.60714546451156792 ) ;
#5746 = CARTESIAN_POINT ( 'NONE',  ( -22.42236680055709641, 157.8615022471902591, 0.000000000000000000 ) ) ;
#5747 = CARTESIAN_POINT ( 'NONE',  ( 179.0788045520370702, 287.9706957157609963, -12.84865443290734888 ) ) ;
#5748 = CARTESIAN_POINT ( 'NONE',  ( 182.0889153921933143, 262.8220885373254418, 12.61422020207666073 ) ) ;
#5749 = CARTESIAN_POINT ( 'NONE',  ( 95.19470834736908671, 225.7677522451418497, 10.00000000000009592 ) ) ;
#5750 = EDGE_LOOP ( 'NONE', ( #75965, #64656, #12072, #53852 ) ) ;
#5751 = CARTESIAN_POINT ( 'NONE',  ( 198.6608371149412733, 267.8789152959208195, -8.090336142662009067 ) ) ;
#5752 = CARTESIAN_POINT ( 'NONE',  ( 155.4640109849479472, 279.7078215382471171, -1.643371934387127808 ) ) ;
#5753 = CARTESIAN_POINT ( 'NONE',  ( 155.0568450317760494, 264.0806616740677555, 17.52241723436104337 ) ) ;
#5755 = EDGE_CURVE ( 'NONE', #30892, #35128, #35448, .T. ) ;
#5754 = AXIS2_PLACEMENT_3D ( 'NONE', #66039, #73164, #88407 ) ;
#5756 = CARTESIAN_POINT ( 'NONE',  ( 12.78715206816254302, 172.0643266524160140, -9.188101187500093303 ) ) ;
#5757 = CARTESIAN_POINT ( 'NONE',  ( 12.91273316327571052, 9.583808731787852864, 6.180339887498953466 ) ) ;
#5758 = CARTESIAN_POINT ( 'NONE',  ( 195.8612935349768520, 273.6653920451291242, 14.68105839524987744 ) ) ;
#5759 = CARTESIAN_POINT ( 'NONE',  ( 71.66596873478475516, 59.16830023791868598, -15.31655212997402060 ) ) ;
#5760 = CARTESIAN_POINT ( 'NONE',  ( 73.11654091825437263, 69.80299609433679109, 9.611781565164262631 ) ) ;
#5761 = CARTESIAN_POINT ( 'NONE',  ( 52.86797706100236383, 192.1423013555410080, -4.594050593750043987 ) ) ;
#5762 = EDGE_CURVE ( 'NONE', #77711, #94602, #73467, .T. ) ;
#5763 = CARTESIAN_POINT ( 'NONE',  ( 207.5290616128274337, 271.1961165699281651, 2.604679844609484984 ) ) ;
#5764 = FACE_OUTER_BOUND ( 'NONE', #34174, .T. ) ;
#5765 = DIRECTION ( 'NONE',  ( -1.000000000000000000, 0.000000000000000000, 0.000000000000000000 ) ) ;
#5766 = CARTESIAN_POINT ( 'NONE',  ( 165.0532575723395041, 244.7663672603923715, -2.144843157699870773 ) ) ;
#5767 = ORIENTED_EDGE ( 'NONE', *, *, #1944, .F. ) ;
#5768 = VECTOR ( 'NONE', #99056, 1000.000000000000000 ) ;
#5769 = CARTESIAN_POINT ( 'NONE',  ( 15.61058218230948036, 186.4865022471903160, 10.00000000000009237 ) ) ;
#5770 = CARTESIAN_POINT ( 'NONE',  ( 208.3057440179679531, 269.8508631828800617, 2.969924427282375046 ) ) ;
#5771 = CARTESIAN_POINT ( 'NONE',  ( 138.6044920356617922, 241.6423013555409796, -4.594050593750043987 ) ) ;
#5772 = CARTESIAN_POINT ( 'NONE',  ( 20.80007953598619963, 32.98502408145593279, -5.678558825948271327 ) ) ;
#5774 = EDGE_CURVE ( 'NONE', #37486, #92061, #84354, .T. ) ;
#5773 = CARTESIAN_POINT ( 'NONE',  ( 164.3075360873267527, 246.0579947607303097, 1.438421213066341187 ) ) ;
#5775 = CARTESIAN_POINT ( 'NONE',  ( 83.55324616867257248, 51.62071861895685743, -14.85649312488210860 ) ) ;
#5776 = LINE ( 'NONE', #67572, #51309 ) ;
#5778 = CARTESIAN_POINT ( 'NONE',  ( 185.9978760885800853, 288.1611571412556714, 14.69368409826119404 ) ) ;
#5777 = CARTESIAN_POINT ( 'NONE',  ( 157.6286460899086137, 257.6261715744221306, 18.25526781158026779 ) ) ;
#5779 = CARTESIAN_POINT ( 'NONE',  ( 68.86387196620182749, 64.09141771346156702, 12.04978999048449850 ) ) ;
#5780 = EDGE_LOOP ( 'NONE', ( #15528, #40462, #67662, #74007 ) ) ;
#5781 = CARTESIAN_POINT ( 'NONE',  ( 150.8888667059421209, 269.2998118992572927, 15.79021133717968617 ) ) ;
#5782 = CARTESIAN_POINT ( 'NONE',  ( 208.2011561505922828, 270.0320146830300132, -1.742225264168492771 ) ) ;
#5783 = CARTESIAN_POINT ( 'NONE',  ( 181.6780919045320672, 288.0220715738037711, 13.83910407665415931 ) ) ;
#5784 = CARTESIAN_POINT ( 'NONE',  ( 170.4610070438220930, 266.6194390815376210, -16.58348635212187361 ) ) ;
#5785 = CARTESIAN_POINT ( 'NONE',  ( 197.2730491841539617, 273.3678195921213501, -13.56865045505698575 ) ) ;
#5786 = ORIENTED_EDGE ( 'NONE', *, *, #15936, .T. ) ;
#5787 = CARTESIAN_POINT ( 'NONE',  ( 72.08189555467076559, 71.77589625233247261, 3.913479549830300108 ) ) ;
#5788 = CARTESIAN_POINT ( 'NONE',  ( 84.27190106046026585, 41.73435386644143819, -2.959663762035162460 ) ) ;
#5789 = VECTOR ( 'NONE', #57061, 1000.000000000000000 ) ;
#5790 = ADVANCED_FACE ( 'NONE', ( #58728 ), #88216, .F. ) ;
#5791 = EDGE_CURVE ( 'NONE', #55615, #92124, #97769, .T. ) ;
#5792 = CARTESIAN_POINT ( 'NONE',  ( 200.7867161642997758, 282.5082135784035131, -16.60672201385608204 ) ) ;
#5793 = CARTESIAN_POINT ( 'NONE',  ( 196.2709069678370497, 270.8137320491818514, 13.18132365197871358 ) ) ;
#5794 = VECTOR ( 'NONE', #58198, 1000.000000000000000 ) ;
#5795 = DIRECTION ( 'NONE',  ( -0.4999999999999987788, 0.8660254037844392627, 0.000000000000000000 ) ) ;
#5796 = CARTESIAN_POINT ( 'NONE',  ( 208.3829315663354862, 269.7171704273955015, -1.768817828503133072 ) ) ;
#5797 = CARTESIAN_POINT ( 'NONE',  ( 72.59661365748412720, 57.20633740541691736, -16.35330217628511207 ) ) ;
#5798 =( BOUNDED_CURVE ( )  B_SPLINE_CURVE ( 2, ( #26099, #87472, #25597, #19014, #2308, #57983, #12400, #88455, #42271 ),
 .UNSPECIFIED., .F., .T. ) 
 B_SPLINE_CURVE_WITH_KNOTS ( ( 3, 2, 2, 2, 3 ),
 ( 0.3266129032258064391, 0.3279569892473118142, 0.3306451612903225645, 0.3333333333333333148, 0.3346774193548386900 ),
 .UNSPECIFIED. ) 
 CURVE ( )  GEOMETRIC_REPRESENTATION_ITEM ( )  RATIONAL_B_SPLINE_CURVE ( ( 0.9330127018922194093, 0.9330127018922194093, 1.000000000000000000, 0.8660254037844387076, 1.000000000000000000, 0.8660254037844387076, 1.000000000000000000, 0.9330127018922194093, 0.9330127018922194093 ) ) 
 REPRESENTATION_ITEM ( '' )  );
#5799 = ORIENTED_EDGE ( 'NONE', *, *, #94947, .F. ) ;
#5800 = FACE_OUTER_BOUND ( 'NONE', #65592, .T. ) ;
#5801 = CARTESIAN_POINT ( 'NONE',  ( 14.35886136108867994, 13.45404122711132011, -8.090169943749478065 ) ) ;
#5802 = CARTESIAN_POINT ( 'NONE',  ( 85.23541620384800410, 230.0177522451419350, 5.000000000000046185 ) ) ;
#5803 = ORIENTED_EDGE ( 'NONE', *, *, #42310, .T. ) ;
#5804 = DIRECTION ( 'NONE',  ( 0.8660254037844382635, 0.5000000000000004441, 0.000000000000000000 ) ) ;
#5805 = CARTESIAN_POINT ( 'NONE',  ( 50.23025173566475132, 97.10399052176643409, -10.00000000000000000 ) ) ;
#5806 = CARTESIAN_POINT ( 'NONE',  ( 86.53256316603656728, 45.00470303126988370, -7.040634408676482714 ) ) ;
#5807 = EDGE_LOOP ( 'NONE', ( #34590, #16460, #13308, #46550 ) ) ;
#5808 = DIRECTION ( 'NONE',  ( -0.000000000000000000, -0.000000000000000000, -1.000000000000000000 ) ) ;
#5809 = CARTESIAN_POINT ( 'NONE',  ( 205.8889072768004951, 273.5716727396786041, -9.812782715980612025 ) ) ;
#5810 = CARTESIAN_POINT ( 'NONE',  ( 204.2133777088835700, 276.9390495533970693, 13.75768580338462144 ) ) ;
#5811 = CARTESIAN_POINT ( 'NONE',  ( 58.13834967963523326, 192.8262482093458061, 3.021315404115420679E-15 ) ) ;
#5812 = VERTEX_POINT ( 'NONE', #7038 ) ;
#5813 = CARTESIAN_POINT ( 'NONE',  ( 90.35072584248885619, 210.7202760586659167, -5.415160957724236172E-17 ) ) ;
#5814 = CARTESIAN_POINT ( 'NONE',  ( 203.4046850588284485, 278.3397463110001695, 14.99647135965170897 ) ) ;
#5815 = CARTESIAN_POINT ( 'NONE',  ( 177.8917589780327546, 269.0032800508485593, -16.65457745387491073 ) ) ;
#5816 = CARTESIAN_POINT ( 'NONE',  ( 81.63469519429038712, 42.65045104992751845, -7.594666505242645194 ) ) ;
#5817 = ORIENTED_EDGE ( 'NONE', *, *, #73326, .F. ) ;
#5818 = ADVANCED_FACE ( 'NONE', ( #68831 ), #30341, .T. ) ;
#5819 = ORIENTED_EDGE ( 'NONE', *, *, #61708, .T. ) ;
#5820 = CARTESIAN_POINT ( 'NONE',  ( 88.33060278926279807, 43.77373715677852317, 0.1867717842524382055 ) ) ;
#5821 = VERTEX_POINT ( 'NONE', #76932 ) ;
#5822 = LINE ( 'NONE', #13927, #36916 ) ;
#5823 = ORIENTED_EDGE ( 'NONE', *, *, #86339, .F. ) ;
#5824 = CARTESIAN_POINT ( 'NONE',  ( 173.4026771546767804, 273.2456497557084845, -17.70700034978624515 ) ) ;
#5825 = ORIENTED_EDGE ( 'NONE', *, *, #66008, .T. ) ;
#5826 = ADVANCED_FACE ( 'NONE', ( #69339 ), #75978, .T. ) ;
#5827 = LINE ( 'NONE', #3844, #18476 ) ;
#5828 = B_SPLINE_CURVE_WITH_KNOTS ( 'NONE', 3,
 ( #16096, #71316, #39868, #1413 ),
 .UNSPECIFIED., .F., .F.,
 ( 4, 4 ),
 ( 0.008174317677677851723, 0.01411586822901593832 ),
 .UNSPECIFIED. ) ;
#5829 = CARTESIAN_POINT ( 'NONE',  ( 41.47569090598248920, 209.1868197944957899, -17.47570218321533631 ) ) ;
#5830 = CARTESIAN_POINT ( 'NONE',  ( -23.41475416096364981, 99.76909336696888886, 45.19938842315524852 ) ) ;
#5831 = CARTESIAN_POINT ( 'NONE',  ( 67.94274346924396468, 68.32429110883670376, -6.362094354891789649 ) ) ;
#5832 = EDGE_CURVE ( 'NONE', #82529, #85923, #53139, .T. ) ;
#5833 = CARTESIAN_POINT ( 'NONE',  ( 164.7649989079121156, 265.0053717114169558, -16.62870243764915656 ) ) ;
#5834 = ORIENTED_EDGE ( 'NONE', *, *, #9246, .F. ) ;
#5835 = CARTESIAN_POINT ( 'NONE',  ( 65.97757591540607791, 68.67073303864405887, -0.1440890505035684610 ) ) ;
#5836 = CARTESIAN_POINT ( 'NONE',  ( 13.56875384759882763, 10.76004757982087767, 5.678558825948272215 ) ) ;
#5837 = ORIENTED_EDGE ( 'NONE', *, *, #81547, .T. ) ;
#5839 = EDGE_CURVE ( 'NONE', #83863, #59100, #84583, .T. ) ;
#5838 = VECTOR ( 'NONE', #91720, 1000.000000000000114 ) ;
#5840 = CARTESIAN_POINT ( 'NONE',  ( -29.41917662106829212, 23.74964416229699893, 177.5919119679930134 ) ) ;
#5842 = ORIENTED_EDGE ( 'NONE', *, *, #4555, .T. ) ;
#5841 = FACE_OUTER_BOUND ( 'NONE', #91048, .T. ) ;
#5843 = ADVANCED_FACE ( 'NONE', ( #15623 ), #91676, .T. ) ;
#5844 = CARTESIAN_POINT ( 'NONE',  ( -16.76269525828470464, 104.2312461070085021, 12.63376007436041171 ) ) ;
#5845 = CARTESIAN_POINT ( 'NONE',  ( 202.2773826701151165, 280.2922913237452462, 16.62862787739668846 ) ) ;
#5846 = ADVANCED_FACE ( 'NONE', ( #90701 ), #92195, .T. ) ;
#5847 = CARTESIAN_POINT ( 'NONE',  ( 188.0130000780826265, 260.6906737763359274, 2.852620083407500395 ) ) ;
#5848 = CARTESIAN_POINT ( 'NONE',  ( 161.0174131639706161, 281.2532803613611918, -6.597337978638083911 ) ) ;
#5849 = CARTESIAN_POINT ( 'NONE',  ( 77.56105267981614304, 49.72783448595330924, -15.46007777815280981 ) ) ;
#5850 = CIRCLE ( 'NONE', #33324, 16.10714546451156082 ) ;
#5851 = DIRECTION ( 'NONE',  ( -0.000000000000000000, -0.000000000000000000, 1.000000000000000000 ) ) ;
#5852 = CARTESIAN_POINT ( 'NONE',  ( 168.4162858537046645, 252.9027699456641187, 12.03307035579989126 ) ) ;
#5853 = CARTESIAN_POINT ( 'NONE',  ( 158.1077839419051827, 281.0782939731791998, 2.063989399413418191 ) ) ;
#5854 = VERTEX_POINT ( 'NONE', #29844 ) ;
#5855 = CARTESIAN_POINT ( 'NONE',  ( 155.3935616475962149, 261.4974513877137952, -18.59422973016237890 ) ) ;
#5856 = CARTESIAN_POINT ( 'NONE',  ( 71.92239571885137650, 63.18146859836171103, -13.81142053453491059 ) ) ;
#5857 = ORIENTED_EDGE ( 'NONE', *, *, #89622, .F. ) ;
#5858 = CARTESIAN_POINT ( 'NONE',  ( 160.6427889144519554, 275.7530518071173447, 12.78665216319188858 ) ) ;
#5859 = CARTESIAN_POINT ( 'NONE',  ( -7.429302001086912632, 166.5177522451418781, -10.00000000000009592 ) ) ;
#5860 = CARTESIAN_POINT ( 'NONE',  ( 196.1510318622376872, 269.5623502998935805, -10.89412449686265560 ) ) ;
#5861 = CARTESIAN_POINT ( 'NONE',  ( 47.39496755818312579, 108.2889530649357681, -10.00000000000000000 ) ) ;
#5862 = CARTESIAN_POINT ( 'NONE',  ( 169.3092427493755281, 280.4792478331783059, -14.38416588291234000 ) ) ;
#5863 = CARTESIAN_POINT ( 'NONE',  ( 87.43898003897845683, 44.70913447485149561, -5.303997024264144322 ) ) ;
#5864 = CARTESIAN_POINT ( 'NONE',  ( 160.8606767143015759, 272.6466877113235228, 15.42252470312289248 ) ) ;
#5866 = CARTESIAN_POINT ( 'NONE',  ( 30.45164419685804447, 25.78052372038641948, -10.00000000000000355 ) ) ;
#5865 = CARTESIAN_POINT ( 'NONE',  ( 0.1486806056246424423, 161.7048013555410080, 4.594050593750051981 ) ) ;
#5867 = CARTESIAN_POINT ( 'NONE',  ( 185.0971745880719936, 295.3200165845683500, 8.402215535322445916 ) ) ;
#5868 = ORIENTED_EDGE ( 'NONE', *, *, #64011, .F. ) ;
#5869 = VECTOR ( 'NONE', #31768, 1000.000000000000000 ) ;
#5870 = ORIENTED_EDGE ( 'NONE', *, *, #20040, .T. ) ;
#5871 = PLANE ( 'NONE',  #22534 ) ;
#5872 = FACE_OUTER_BOUND ( 'NONE', #81594, .T. ) ;
#5873 = VECTOR ( 'NONE', #53819, 1000.000000000000000 ) ;
#5874 = CARTESIAN_POINT ( 'NONE',  ( 84.93582513569069192, 42.31612956156499195, 0.5963448692699542253 ) ) ;
#5875 = CARTESIAN_POINT ( 'NONE',  ( -19.64547786486492598, 92.92342514603942050, 59.99999999999999289 ) ) ;
#5876 = CARTESIAN_POINT ( 'NONE',  ( 68.38018342861622045, 66.23482706493213357, 10.56038378207740358 ) ) ;
#5877 = CARTESIAN_POINT ( 'NONE',  ( 153.2507058676394536, 279.2988129818712650, 3.890835714306057458 ) ) ;
#5878 = CARTESIAN_POINT ( 'NONE',  ( 17.11727908708474288, 174.5643266524160424, 9.188101187500095079 ) ) ;
#5879 = CARTESIAN_POINT ( 'NONE',  ( 120.0931990297694085, 230.9548013555409796, -4.594050593750042211 ) ) ;
#5880 = CARTESIAN_POINT ( 'NONE',  ( 87.67819772848358184, 44.37415200095301770, -4.027115429479418474 ) ) ;
#5881 = CARTESIAN_POINT ( 'NONE',  ( 183.1420952819525780, 257.7645371039402562, -2.611028994885449261 ) ) ;
#5882 = CARTESIAN_POINT ( 'NONE',  ( 206.2084181172874651, 271.6286034143743677, -8.104356745948360086 ) ) ;
#5883 = CARTESIAN_POINT ( 'NONE',  ( 178.5070354113733231, 283.8968948738306608, -14.91322718153175053 ) ) ;
#5884 = CARTESIAN_POINT ( 'NONE',  ( 82.21058008569970355, 52.79855391407854626, -15.17934502883119308 ) ) ;
#5885 = CARTESIAN_POINT ( 'NONE',  ( 166.2015897840689149, 251.7888940817747425, -12.22707897765162599 ) ) ;
#5886 = CARTESIAN_POINT ( 'NONE',  ( 183.8863552858182118, 275.0393761356287996, 16.36257040815191388 ) ) ;
#5887 = CARTESIAN_POINT ( 'NONE',  ( 147.7785919239399846, 274.6869658471848652, -7.924750738206837397 ) ) ;
#5888 = DIRECTION ( 'NONE',  ( 0.8435938723211464652, 0.5369817302126890235, 0.000000000000000000 ) ) ;
#5889 = CARTESIAN_POINT ( 'NONE',  ( 84.49887294678060812, 50.66939116110540908, 13.73193151845090831 ) ) ;
#5890 = CARTESIAN_POINT ( 'NONE',  ( 196.3622566498499111, 266.7229801469659947, 8.086874854287275483 ) ) ;
#5891 = CARTESIAN_POINT ( 'NONE',  ( -22.42236680055709641, 157.8615022471902591, 0.000000000000000000 ) ) ;
#5892 = CARTESIAN_POINT ( 'NONE',  ( 183.6708288585361686, 268.4310204149097103, -15.04327638771743381 ) ) ;
#5893 = CARTESIAN_POINT ( 'NONE',  ( -49.85285084787511067, 106.9394001011715574, -10.00000000000000000 ) ) ;
#5894 = CARTESIAN_POINT ( 'NONE',  ( 174.0300771628572818, 264.6284561815462553, -15.49364447767913866 ) ) ;
#5895 = CARTESIAN_POINT ( 'NONE',  ( 96.25000326212280299, 232.5024278399160664, -9.188101187500093303 ) ) ;
#5896 = ADVANCED_FACE ( 'NONE', ( #7535 ), #53628, .F. ) ;
#5897 = CARTESIAN_POINT ( 'NONE',  ( -19.65312891409030271, 93.06504152958497400, -10.00000000000000888 ) ) ;
#5899 = CARTESIAN_POINT ( 'NONE',  ( 152.3887669668241074, 266.7019084411238623, 16.79563195480379534 ) ) ;
#5898 = CARTESIAN_POINT ( 'NONE',  ( 157.5520850189458884, 257.7587792392113215, 16.71892742266126319 ) ) ;
#5900 = CARTESIAN_POINT ( 'NONE',  ( 201.3105023133114173, 270.3128416713978481, -10.18795719577549796 ) ) ;
#5901 = CARTESIAN_POINT ( 'NONE',  ( 198.8533049117289977, 286.2229679703367538, -18.60939981449148561 ) ) ;
#5902 = CARTESIAN_POINT ( 'NONE',  ( 80.02025975469349817, 44.34820518763979180, 11.52912450659341381 ) ) ;
#5903 = AXIS2_PLACEMENT_3D ( 'NONE', #2724, #63500, #26020 ) ;
#5904 = CARTESIAN_POINT ( 'NONE',  ( 38.30461122658549300, 34.06628583063844928, -9.188101187500006262 ) ) ;
#5905 = DIRECTION ( 'NONE',  ( 0.2126238682951520631, -0.9771341211068242938, 0.000000000000000000 ) ) ;
#5906 = CARTESIAN_POINT ( 'NONE',  ( 81.74119788692269140, 59.14441083166271795, 0.000000000000000000 ) ) ;
#5907 = ORIENTED_EDGE ( 'NONE', *, *, #47331, .T. ) ;
#5908 = CARTESIAN_POINT ( 'NONE',  ( 20.27082849090286487, 27.10171378149918908, 9.188101187500008038 ) ) ;
#5909 = DIRECTION ( 'NONE',  ( 0.001368469433193631119, -0.9999990636452669168, 0.000000000000000000 ) ) ;
#5910 = CIRCLE ( 'NONE', #22031, 15.50000000000000000 ) ;
#5911 = CARTESIAN_POINT ( 'NONE',  ( 193.1169444172380167, 296.1586357973259283, -13.13373377033755318 ) ) ;
#5912 = CARTESIAN_POINT ( 'NONE',  ( 82.30224259357629535, 41.51585266698759114, -5.837696018585297075 ) ) ;
#5914 = ORIENTED_EDGE ( 'NONE', *, *, #17435, .T. ) ;
#5913 = EDGE_CURVE ( 'NONE', #82593, #22789, #38424, .T. ) ;
#5915 = EDGE_CURVE ( 'NONE', #74024, #95321, #27211, .T. ) ;
#5916 = CARTESIAN_POINT ( 'NONE',  ( 70.80077772051866702, 60.95163764393168293, 15.04332542951107676 ) ) ;
#5917 = CARTESIAN_POINT ( 'NONE',  ( 159.7608930362198407, 253.9330115291272421, 15.38895778945778581 ) ) ;
#5918 = CARTESIAN_POINT ( 'NONE',  ( 154.3836164983932804, 267.1724063083494229, 16.08677479740975969 ) ) ;
#5919 = CARTESIAN_POINT ( 'NONE',  ( -51.02451589650411989, 104.0357803128446506, -10.00000000000000000 ) ) ;
#5920 = CARTESIAN_POINT ( 'NONE',  ( 140.3904091109174317, 241.8615022471902023, 5.000000000000051514 ) ) ;
#5921 = EDGE_LOOP ( 'NONE', ( #85265, #71901, #35711, #55489 ) ) ;
#5922 = CARTESIAN_POINT ( 'NONE',  ( 190.4606495512497304, 299.4734402352337383, -6.528258444144710460 ) ) ;
#5923 = ORIENTED_EDGE ( 'NONE', *, *, #44335, .T. ) ;
#5924 = CARTESIAN_POINT ( 'NONE',  ( 197.0096825693687776, 265.1139848888072379, -4.595851537931033626 ) ) ;
#5925 = CYLINDRICAL_SURFACE ( 'NONE', #87042, 70.00000000000002842 ) ;
#5926 = VERTEX_POINT ( 'NONE', #28854 ) ;
#5927 = CARTESIAN_POINT ( 'NONE',  ( 185.2453734934235570, 292.5319340899530971, -10.69469963830730919 ) ) ;
#5928 = ORIENTED_EDGE ( 'NONE', *, *, #80627, .T. ) ;
#5929 = CARTESIAN_POINT ( 'NONE',  ( 86.39040197603725346, 47.55452816739963140, -10.55219518323342243 ) ) ;
#5930 = CARTESIAN_POINT ( 'NONE',  ( 205.8843284829576987, 274.0448779157541708, 10.73475218247099683 ) ) ;
#5931 = CARTESIAN_POINT ( 'NONE',  ( 84.85964987685913741, 50.19146562821751445, 13.75030272624154470 ) ) ;
#5932 = CARTESIAN_POINT ( 'NONE',  ( 204.1793134244172734, 273.0455815889928886, 10.99258542199709154 ) ) ;
#5933 = LINE ( 'NONE', #43922, #98454 ) ;
#5934 = VECTOR ( 'NONE', #44733, 1000.000000000000114 ) ;
#5935 = CARTESIAN_POINT ( 'NONE',  ( 30.11829213135327166, 40.49540643055188838, 3.479690158560446702E-15 ) ) ;
#5936 = AXIS2_PLACEMENT_3D ( 'NONE', #79896, #94094, #78876 ) ;
#5937 = CARTESIAN_POINT ( 'NONE',  ( 72.14715343843565165, 60.82528180842287924, -14.87966352528053449 ) ) ;
#5938 = B_SPLINE_CURVE_WITH_KNOTS ( 'NONE', 3,
 ( #23528, #76747, #53922, #24540 ),
 .UNSPECIFIED., .F., .F.,
 ( 4, 4 ),
 ( 0.000000000000000000, 0.003871553614270288081 ),
 .UNSPECIFIED. ) ;
#5939 = FACE_OUTER_BOUND ( 'NONE', #87722, .T. ) ;
#5940 = CARTESIAN_POINT ( 'NONE',  ( 73.72680694775513643, 201.8262482093457777, 3.021315404115420679E-15 ) ) ;
#5941 = VECTOR ( 'NONE', #2668, 1000.000000000000000 ) ;
#5942 = ORIENTED_EDGE ( 'NONE', *, *, #40283, .T. ) ;
#5943 = ORIENTED_EDGE ( 'NONE', *, *, #51314, .T. ) ;
#5944 = CARTESIAN_POINT ( 'NONE',  ( 87.24292777721575476, 46.11748857515735267, -8.882011181227387198 ) ) ;
#5945 = EDGE_CURVE ( 'NONE', #60977, #25883, #2151, .T. ) ;
#5947 = CARTESIAN_POINT ( 'NONE',  ( 165.4717973444044503, 273.8037661123966586, -15.20093003926469066 ) ) ;
#5946 = CARTESIAN_POINT ( 'NONE',  ( 174.4157552818196848, 257.3257494145293549, -11.97941750818477757 ) ) ;
#5948 = CARTESIAN_POINT ( 'NONE',  ( 206.6829130365991034, 272.6616888947074244, -10.15488415123734001 ) ) ;
#5949 = LINE ( 'NONE', #337, #2035 ) ;
#5950 = CARTESIAN_POINT ( 'NONE',  ( 73.76765479342118681, 61.19218300593534821, -15.11731574097786712 ) ) ;
#5951 = CARTESIAN_POINT ( 'NONE',  ( 82.32489299410643468, 40.36065608818346107, 1.262906813034385456 ) ) ;
#5952 = CARTESIAN_POINT ( 'NONE',  ( 167.0625938901047789, 286.3493216121294154, -4.853271414194278321 ) ) ;
#5953 = CARTESIAN_POINT ( 'NONE',  ( 77.28356520717616718, 63.39747816212522480, -15.14739555479249589 ) ) ;
#5954 = EDGE_CURVE ( 'NONE', #31208, #97695, #66196, .T. ) ;
#5955 = CARTESIAN_POINT ( 'NONE',  ( 178.1108306389469647, 255.4780320608604995, 4.908464522874967706 ) ) ;
#5956 = EDGE_CURVE ( 'NONE', #44657, #62092, #20388, .T. ) ;
#5957 = CARTESIAN_POINT ( 'NONE',  ( 109.7816501962546454, 240.3149278399160949, 9.188101187500093303 ) ) ;
#5958 = ORIENTED_EDGE ( 'NONE', *, *, #16226, .T. ) ;
#5959 = CARTESIAN_POINT ( 'NONE',  ( 148.1162654905123190, 275.3898513388497804, -5.688393309263520159 ) ) ;
#5960 = CARTESIAN_POINT ( 'NONE',  ( 34.18979426048110781, 28.24335787977765122, -9.188101187500008038 ) ) ;
#5961 = CARTESIAN_POINT ( 'NONE',  ( 191.9772060522040533, 275.3178886761277226, 16.43916042812731249 ) ) ;
#5962 = ORIENTED_EDGE ( 'NONE', *, *, #1186, .F. ) ;
#5963 = CARTESIAN_POINT ( 'NONE',  ( 74.20878020607858616, 68.72316200637693839, -11.41572480156362879 ) ) ;
#5964 = EDGE_CURVE ( 'NONE', #51310, #49046, #25092, .T. ) ;
#5965 = DIRECTION ( 'NONE',  ( -0.6123724356958019088, -0.3535533905932806698, -0.7071067811865376918 ) ) ;
#5966 = CARTESIAN_POINT ( 'NONE',  ( 164.3720776498103646, 249.6648944244760173, 9.933307626539082946 ) ) ;
#5967 = CARTESIAN_POINT ( 'NONE',  ( 206.1408608592916494, 273.6005508061571732, -10.42739367433323494 ) ) ;
#5968 = CARTESIAN_POINT ( 'NONE',  ( 97.22551825371941447, 215.3932355074535394, -2.679491924311248496 ) ) ;
#5969 = ORIENTED_EDGE ( 'NONE', *, *, #7524, .T. ) ;
#5970 = ORIENTED_EDGE ( 'NONE', *, *, #29773, .T. ) ;
#5971 = CARTESIAN_POINT ( 'NONE',  ( 199.7327534409123189, 266.0852835921289170, -4.070366225034659280 ) ) ;
#5972 = ORIENTED_EDGE ( 'NONE', *, *, #42937, .F. ) ;
#5973 = CARTESIAN_POINT ( 'NONE',  ( 191.4684674121631076, 263.6719838314244271, -8.116905096791009910 ) ) ;
#5974 = CARTESIAN_POINT ( 'NONE',  ( 174.1019790828183034, 269.4634721183348915, -17.75005378496514297 ) ) ;
#5975 = AXIS2_PLACEMENT_3D ( 'NONE', #18174, #69859, #471 ) ;
#5976 = CARTESIAN_POINT ( 'NONE',  ( 83.38724336809534066, 47.38832907623395840, 11.89773227219856899 ) ) ;
#5978 = DIRECTION ( 'NONE',  ( -0.6835488936653838499, -0.7299047266382302501, 0.000000000000000000 ) ) ;
#5977 = CARTESIAN_POINT ( 'NONE',  ( 30.34687108590969373, 93.06504152958497400, 20.00000000000000355 ) ) ;
#5979 = DIRECTION ( 'NONE',  ( -0.8660254037844387076, -0.4999999999999998890, -0.000000000000000000 ) ) ;
#5980 = VERTEX_POINT ( 'NONE', #94678 ) ;
#5982 = CARTESIAN_POINT ( 'NONE',  ( 147.4317198359019301, 275.2877659273946733, 3.797273160043843188 ) ) ;
#5981 = AXIS2_PLACEMENT_3D ( 'NONE', #51156, #82120, #50173 ) ;
#5983 = CARTESIAN_POINT ( 'NONE',  ( 52.03546399666511491, 212.3967562850347122, -4.648177544792955347E-16 ) ) ;
#5984 = CARTESIAN_POINT ( 'NONE',  ( 82.44254630377066917, 40.85897994371414654, -3.714870737426086755 ) ) ;
#5985 = CARTESIAN_POINT ( 'NONE',  ( 172.1240434037265743, 250.9065000376095043, -0.2557444706756556996 ) ) ;
#5986 = CARTESIAN_POINT ( 'NONE',  ( 189.3359066111170534, 270.2222636373566047, -14.08322114487687848 ) ) ;
#5987 = CARTESIAN_POINT ( 'NONE',  ( 26.69679556076013327, 57.08553156527587902, 59.99999999999999289 ) ) ;
#5988 = ADVANCED_FACE ( 'NONE', ( #946 ), #24246, .F. ) ;
#5989 = CARTESIAN_POINT ( 'NONE',  ( 84.14612687645852418, 44.79878194911968592, 8.715766578047444924 ) ) ;
#5990 = CARTESIAN_POINT ( 'NONE',  ( -22.42236680055709641, 157.8615022471902591, 0.000000000000000000 ) ) ;
#5991 = AXIS2_PLACEMENT_3D ( 'NONE', #32252, #79900, #41341 ) ;
#5992 = CARTESIAN_POINT ( 'NONE',  ( 70.81316579126399802, 61.41551742065354347, -14.85192641751565468 ) ) ;
#5993 = CARTESIAN_POINT ( 'NONE',  ( 75.14063404487711750, 220.3149278399160664, -9.188101187500095079 ) ) ;
#5994 = CARTESIAN_POINT ( 'NONE',  ( 159.2536436069973718, 254.8115933126508992, -15.76697951715411250 ) ) ;
#5995 = CARTESIAN_POINT ( 'NONE',  ( 197.0121621852902933, 287.4119207165142029, 17.64812647472269092 ) ) ;
#5996 = DIRECTION ( 'NONE',  ( -0.000000000000000000, 0.000000000000000000, -1.000000000000000000 ) ) ;
#5997 = EDGE_CURVE ( 'NONE', #11925, #26012, #56122, .T. ) ;
#5998 = CARTESIAN_POINT ( 'NONE',  ( 197.3665944960539491, 288.3056451486161222, -16.78855881086668234 ) ) ;
#5999 = CARTESIAN_POINT ( 'NONE',  ( 161.2977680094314223, 251.2710659906439616, -13.03191437619249982 ) ) ;
#6000 = CARTESIAN_POINT ( 'NONE',  ( 45.86253193465722688, 68.41350641406140198, 177.5919119679930134 ) ) ;
#6001 = CIRCLE ( 'NONE', #59342, 17.82106496071138935 ) ;
#6002 = CARTESIAN_POINT ( 'NONE',  ( 81.95770423786879633, 58.76941083166271795, 0.2500000000000019984 ) ) ;
#6003 = FILL_AREA_STYLE_COLOUR ( '', #95152 ) ;
#6004 = CARTESIAN_POINT ( 'NONE',  ( 35.31250668086032363, 42.16126292948897714, -6.180339887498951690 ) ) ;
#6005 = LINE ( 'NONE', #28297, #67671 ) ;
#6006 = CARTESIAN_POINT ( 'NONE',  ( 46.60452734134890562, 70.48356709729735314, 10.00000000000000000 ) ) ;
#6007 = CARTESIAN_POINT ( 'NONE',  ( 72.00818181938288376, 72.30390281540809383, 3.363530094501230305 ) ) ;
#6008 = CARTESIAN_POINT ( 'NONE',  ( 20.90579313287664576, 189.0024278399160949, -9.188101187500093303 ) ) ;
#6009 = CARTESIAN_POINT ( 'NONE',  ( 157.8763546842245376, 257.1971277035954699, 17.68444922773363004 ) ) ;
#6011 = ADVANCED_FACE ( 'NONE', ( #16141 ), #77956, .F. ) ;
#6010 = DIRECTION ( 'NONE',  ( -1.000000000000000000, 0.000000000000000000, 0.000000000000000000 ) ) ;
#6012 = CARTESIAN_POINT ( 'NONE',  ( 77.35960201006287207, 51.36102757442933608, -15.48319045058203791 ) ) ;
#6013 = CARTESIAN_POINT ( 'NONE',  ( 71.47791206682282450, 72.34364865201938244, -1.216664393387148380 ) ) ;
#6014 = CARTESIAN_POINT ( 'NONE',  ( 45.88512659934279014, 206.4869531367911009, 4.594050593750046652 ) ) ;
#6015 = CARTESIAN_POINT ( 'NONE',  ( 16.58664519722142927, 32.68290643055186706, 3.479690158560446702E-15 ) ) ;
#6016 = CARTESIAN_POINT ( 'NONE',  ( 170.7424494536428483, 287.6183357598478665, 7.193943569343137057 ) ) ;
#6017 = CARTESIAN_POINT ( 'NONE',  ( -17.99656830608997993, 171.9637435831424739, 2.679491924311252049 ) ) ;
#6018 = CARTESIAN_POINT ( 'NONE',  ( 12.50787272796288896, 10.14754757982087874, -5.678558825948276656 ) ) ;
#6019 = CARTESIAN_POINT ( 'NONE',  ( 203.1504851873393136, 269.7283529643794395, -7.434428718697961180 ) ) ;
#6020 = CARTESIAN_POINT ( 'NONE',  ( 175.6726996453791685, 291.0189004104380501, 2.504403466513535736 ) ) ;
#6021 = ORIENTED_EDGE ( 'NONE', *, *, #63552, .F. ) ;
#6022 = CARTESIAN_POINT ( 'NONE',  ( 157.1614910081131882, 264.8482722167576071, 17.59091970785239667 ) ) ;
#6023 = CARTESIAN_POINT ( 'NONE',  ( 69.96286275937281118, 67.88719041800112564, -8.946398746998555751 ) ) ;
#6024 = CARTESIAN_POINT ( 'NONE',  ( 163.4107516284163637, 256.1401433533470708, -14.91842279323626030 ) ) ;
#6025 = EDGE_CURVE ( 'NONE', #63549, #77820, #88730, .T. ) ;
#6026 = EDGE_CURVE ( 'NONE', #2734, #60148, #55618, .T. ) ;
#6027 = CARTESIAN_POINT ( 'NONE',  ( 81.92111866118570163, 41.12818642295167848, 3.752801100571455883 ) ) ;
#6028 = CARTESIAN_POINT ( 'NONE',  ( 101.8522786425099156, 219.6115022471901739, -5.000000000000041744 ) ) ;
#6029 = CARTESIAN_POINT ( 'NONE',  ( -22.42236680055709641, 157.8615022471902591, 0.000000000000000000 ) ) ;
#6030 = CARTESIAN_POINT ( 'NONE',  ( 165.1531489442545535, 269.9894434971714077, -16.29722773533296731 ) ) ;
#6031 = ORIENTED_EDGE ( 'NONE', *, *, #32862, .F. ) ;
#6032 = CARTESIAN_POINT ( 'NONE',  ( 61.44712799118319424, 194.0327760586659451, 1.948934522072303157E-15 ) ) ;
#6033 = ORIENTED_EDGE ( 'NONE', *, *, #82743, .T. ) ;
#6034 = CARTESIAN_POINT ( 'NONE',  ( 166.1405104867327793, 265.3397484891177101, 16.55385694601057978 ) ) ;
#6035 = B_SPLINE_CURVE_WITH_KNOTS ( 'NONE', 3,
 ( #88827, #49760, #81205, #65453 ),
 .UNSPECIFIED., .F., .F.,
 ( 4, 4 ),
 ( 0.006807249740348602328, 0.01254308171105925247 ),
 .UNSPECIFIED. ) ;
#6036 = CARTESIAN_POINT ( 'NONE',  ( 147.1199024702499969, 275.8278494473859723, 5.224467159276165340 ) ) ;
#6037 = DIRECTION ( 'NONE',  ( -0.4330127018922203530, 0.7500000000000046629, 0.4999999999999919509 ) ) ;
#6038 = VERTEX_POINT ( 'NONE', #64241 ) ;
#6039 = LINE ( 'NONE', #91672, #29731 ) ;
#6040 = CARTESIAN_POINT ( 'NONE',  ( 79.18083756185062327, 46.29419887370401909, -12.77432615883756206 ) ) ;
#6041 = CARTESIAN_POINT ( 'NONE',  ( 157.8444045675000496, 264.5910462210627543, -17.67892232388873097 ) ) ;
#6042 = CARTESIAN_POINT ( 'NONE',  ( 175.3129199032210295, 273.6512861356621329, -16.42196374976860440 ) ) ;
#6043 = CIRCLE ( 'NONE', #38353, 0.1418229129681557177 ) ;
#6044 = CARTESIAN_POINT ( 'NONE',  ( 12.00096474099108512, 32.03863464977598596, -10.00000000000000000 ) ) ;
#6045 = VERTEX_POINT ( 'NONE', #54617 ) ;
#6046 = AXIS2_PLACEMENT_3D ( 'NONE', #26463, #11765, #65940 ) ;
#6047 = CARTESIAN_POINT ( 'NONE',  ( 24.83671989960918935, 22.84335787977763488, 9.188101187500006262 ) ) ;
#6048 = CARTESIAN_POINT ( 'NONE',  ( 79.96701105519208852, 44.50246225239077091, 11.69262897647518962 ) ) ;
#6049 = CARTESIAN_POINT ( 'NONE',  ( 72.00092472038465985, 70.29460662667155191, -7.277950757834694251 ) ) ;
#6050 = FACE_OUTER_BOUND ( 'NONE', #46410, .T. ) ;
#6051 = VERTEX_POINT ( 'NONE', #31336 ) ;
#6052 = CARTESIAN_POINT ( 'NONE',  ( 48.38981961164311940, 109.5014996615669105, -10.00000000000000000 ) ) ;
#6053 = DIRECTION ( 'NONE',  ( -0.9055221650797523614, -0.4242989612870595728, 0.000000000000000000 ) ) ;
#6054 = ORIENTED_EDGE ( 'NONE', *, *, #88067, .T. ) ;
#6055 = EDGE_LOOP ( 'NONE', ( #61402, #24511, #21152, #90923 ) ) ;
#6056 = VECTOR ( 'NONE', #74434, 1000.000000000000114 ) ;
#6057 = EDGE_CURVE ( 'NONE', #52772, #56685, #69882, .T. ) ;
#6059 = DIRECTION ( 'NONE',  ( -0.8660254037844387076, -0.4999999999999998890, -0.000000000000000000 ) ) ;
#6058 = CARTESIAN_POINT ( 'NONE',  ( 159.3180704616806906, 282.3194142970525604, -3.259201431328204723 ) ) ;
#6060 = CARTESIAN_POINT ( 'NONE',  ( 207.7837159184916231, 270.7550423741513441, -2.369602332675663448 ) ) ;
#6061 = CARTESIAN_POINT ( 'NONE',  ( 163.8147431267737204, 246.9115372060205118, 7.125417796469586840 ) ) ;
#6062 = CARTESIAN_POINT ( 'NONE',  ( 159.6898930778639283, 254.0559870643349143, 16.90891900388599822 ) ) ;
#6063 = CARTESIAN_POINT ( 'NONE',  ( 81.71596569511639530, 55.69046771286013353, 16.33797717450969955 ) ) ;
#6064 = CARTESIAN_POINT ( 'NONE',  ( 164.4177597422757060, 265.5742877017660817, -16.83945066787966383 ) ) ;
#6065 = CARTESIAN_POINT ( 'NONE',  ( 128.8345561752773278, 239.0643266524160424, 9.188101187500095079 ) ) ;
#6066 = CARTESIAN_POINT ( 'NONE',  ( 73.32782722540972031, 203.9548013555409796, -4.594050593750042211 ) ) ;
#6067 = ORIENTED_EDGE ( 'NONE', *, *, #24192, .F. ) ;
#6068 = CARTESIAN_POINT ( 'NONE',  ( 170.3588773579726308, 263.8410958083132982, 15.88277590726158017 ) ) ;
#6069 = CARTESIAN_POINT ( 'NONE',  ( 70.62955678152276562, 60.80479719363771807, -15.06269029744276011 ) ) ;
#6070 = LINE ( 'NONE', #52657, #28606 ) ;
#6071 = ORIENTED_EDGE ( 'NONE', *, *, #85123, .T. ) ;
#6072 = VECTOR ( 'NONE', #7591, 1000.000000000000114 ) ;
#6073 = B_SPLINE_CURVE_WITH_KNOTS ( 'NONE', 3,
 ( #81995, #12568, #4968, #74386 ),
 .UNSPECIFIED., .F., .F.,
 ( 4, 4 ),
 ( 0.006379106832508525497, 0.01446904724182691837 ),
 .UNSPECIFIED. ) ;
#6074 = CARTESIAN_POINT ( 'NONE',  ( 160.6481820402849792, 253.1006006086905984, 14.59193497169809284 ) ) ;
#6075 = ORIENTED_EDGE ( 'NONE', *, *, #73317, .T. ) ;
#6076 = VERTEX_POINT ( 'NONE', #11062 ) ;
#6077 = CARTESIAN_POINT ( 'NONE',  ( 76.22741562560636908, 65.24129761985034293, 14.53304928680089603 ) ) ;
#6078 = CARTESIAN_POINT ( 'NONE',  ( 74.91863663735624357, 66.38413888100485849, -13.07019282884167843 ) ) ;
#6079 = CARTESIAN_POINT ( 'NONE',  ( 34.61729389309891758, 20.39040679176985549, -6.890680421881970419E-14 ) ) ;
#6080 = CARTESIAN_POINT ( 'NONE',  ( 191.8210230231139803, 298.4032374945642232, -8.800268167321144475 ) ) ;
#6081 = CARTESIAN_POINT ( 'NONE',  ( 81.83839218517164227, 55.52280113860526711, 16.29901351018851230 ) ) ;
#6082 = CARTESIAN_POINT ( 'NONE',  ( 155.0197698005585494, 262.1448778582381465, 18.42918111182112284 ) ) ;
#6083 = CARTESIAN_POINT ( 'NONE',  ( 72.62665088832551419, 69.64092492267511147, 8.780471156129905808 ) ) ;
#6084 = CARTESIAN_POINT ( 'NONE',  ( 87.54989630752690744, 45.07147448993673322, 6.930566558073853578 ) ) ;
#6085 = VERTEX_POINT ( 'NONE', #73847 ) ;
#6086 =( BOUNDED_CURVE ( )  B_SPLINE_CURVE ( 2, ( #98590, #45347, #60041, #6852, #76752, #5866, #21569, #37738, #77252, #91490, #75282, #38228, #61036 ),
 .UNSPECIFIED., .F., .T. ) 
 B_SPLINE_CURVE_WITH_KNOTS ( ( 3, 2, 2, 2, 2, 2, 3 ),
 ( 0.6375000000000000666, 0.6400000000000000133, 0.6450000000000000178, 0.6500000000000000222, 0.6550000000000000266, 0.6600000000000000311, 0.6625000000000000888 ),
 .UNSPECIFIED. ) 
 CURVE ( )  GEOMETRIC_REPRESENTATION_ITEM ( )  RATIONAL_B_SPLINE_CURVE ( ( 0.9755282581475767101, 0.9755282581475772652, 1.000000000000000000, 0.9510565162951535312, 1.000000000000000000, 0.9510565162951535312, 1.000000000000000000, 0.9510565162951535312, 1.000000000000000000, 0.9510565162951535312, 1.000000000000000000, 0.9755282581475761550, 0.9755282581475767101 ) ) 
 REPRESENTATION_ITEM ( '' )  );
#6087 = CARTESIAN_POINT ( 'NONE',  ( 200.8251833487811666, 282.8075743310126882, -16.74393672780000131 ) ) ;
#6088 = CARTESIAN_POINT ( 'NONE',  ( 201.0740630776729745, 282.3765019955979483, -17.86148837378524590 ) ) ;
#6089 = ORIENTED_EDGE ( 'NONE', *, *, #6261, .T. ) ;
#6090 = LINE ( 'NONE', #96843, #6545 ) ;
#6091 = CARTESIAN_POINT ( 'NONE',  ( 76.09996437315240314, 51.13569808109860304, -15.59936768269888852 ) ) ;
#6092 = CARTESIAN_POINT ( 'NONE',  ( 174.1320578672132626, 253.2284290848832313, -7.713315856054966169 ) ) ;
#6093 = EDGE_CURVE ( 'NONE', #11051, #69971, #88085, .T. ) ;
#6094 = CARTESIAN_POINT ( 'NONE',  ( 164.9617201910520237, 244.9249146555742414, 2.745022583679548767 ) ) ;
#6095 = CARTESIAN_POINT ( 'NONE',  ( 47.63001943043753528, 186.7592609112380160, 2.679491924311254714 ) ) ;
#6096 = CARTESIAN_POINT ( 'NONE',  ( 159.3282873775263795, 259.5781396707945987, 16.68337382483777276 ) ) ;
#6097 = CARTESIAN_POINT ( 'NONE',  ( 138.6852480475602931, 257.0024278399161517, 9.188101187500095079 ) ) ;
#6098 = ORIENTED_EDGE ( 'NONE', *, *, #36457, .F. ) ;
#6099 = CARTESIAN_POINT ( 'NONE',  ( 88.10887562929657690, 44.41668309952778060, 4.665177569529614487 ) ) ;
#6100 = CARTESIAN_POINT ( 'NONE',  ( 86.69825349856462537, 45.38628583907267000, 7.498776714496921514 ) ) ;
#6101 = CARTESIAN_POINT ( 'NONE',  ( 87.90374476427271588, 44.03065798963926625, -1.770940394083930780 ) ) ;
#6102 =( BOUNDED_CURVE ( )  B_SPLINE_CURVE ( 2, ( #69220, #7419, #31214, #93048, #30733, #23604, #39296, #24617, #821 ),
 .UNSPECIFIED., .F., .F. ) 
 B_SPLINE_CURVE_WITH_KNOTS ( ( 3, 2, 2, 2, 3 ),
 ( 0.7943548387096773800, 0.7956989247311827551, 0.7983870967741935054, 0.8010752688172042557, 0.8024193548387096309 ),
 .UNSPECIFIED. ) 
 CURVE ( )  GEOMETRIC_REPRESENTATION_ITEM ( )  RATIONAL_B_SPLINE_CURVE ( ( 0.9330127018922194093, 0.9330127018922194093, 1.000000000000000000, 0.8660254037844387076, 1.000000000000000000, 0.8660254037844387076, 1.000000000000000000, 0.9330127018922194093, 0.9330127018922194093 ) ) 
 REPRESENTATION_ITEM ( '' )  );
#6103 = CARTESIAN_POINT ( 'NONE',  ( 28.75210520338636044, 111.3165232727998415, 59.99999999999999289 ) ) ;
#6104 = CARTESIAN_POINT ( 'NONE',  ( 74.91863663735624357, 66.38413888100485849, -13.07019282884167843 ) ) ;
#6105 = EDGE_LOOP ( 'NONE', ( #98707, #48806, #30843, #99519 ) ) ;
#6106 = CARTESIAN_POINT ( 'NONE',  ( 77.10620603181371280, 57.94243604226648614, 16.15307470803915635 ) ) ;
#6107 = CARTESIAN_POINT ( 'NONE',  ( 184.0420290590031414, 276.8802109191442469, -16.58438063308576105 ) ) ;
#6108 = CARTESIAN_POINT ( 'NONE',  ( 72.58826525418655251, 71.51553178166663827, -5.516888840409344574 ) ) ;
#6109 = VECTOR ( 'NONE', #40967, 1000.000000000000000 ) ;
#6110 = CARTESIAN_POINT ( 'NONE',  ( 79.86290868560162437, 47.38898415025740718, 13.23194629791669463 ) ) ;
#6111 = CARTESIAN_POINT ( 'NONE',  ( 73.30483403957811106, 69.17932697374328654, -9.895411455429695025 ) ) ;
#6112 = CARTESIAN_POINT ( 'NONE',  ( 196.3062046258999658, 264.8785121205631299, 0.8257428584848626185 ) ) ;
#6113 = CARTESIAN_POINT ( 'NONE',  ( 190.9498149295421570, 299.9122141765958531, -5.138500224925297566 ) ) ;
#6114 = CARTESIAN_POINT ( 'NONE',  ( 186.7005128325694727, 282.3869391950191812, 16.28400853260290759 ) ) ;
#6115 = VECTOR ( 'NONE', #20375, 1000.000000000000114 ) ;
#6116 = CARTESIAN_POINT ( 'NONE',  ( 196.6791268423878307, 270.0974108068855344, 11.84491577176450861 ) ) ;
#6117 = B_SPLINE_SURFACE_WITH_KNOTS ( 'NONE', 3, 1, ( 
 ( #29536, #92369 ),
 ( #21928, #51848 ),
 ( #84768, #44219 ),
 ( #60909, #60409 ),
 ( #45710, #91365 ),
 ( #59921, #36620 ),
 ( #99449, #7726 ),
 ( #30025, #38615 ),
 ( #91874, #69016 ),
 ( #22429, #76634 ),
 ( #30529, #5733 ),
 ( #7219, #53803 ),
 ( #15304, #69521 ),
 ( #59411, #90391 ),
 ( #82789, #13354 ),
 ( #75156, #67529 ),
 ( #86285, #1650 ),
 ( #78141, #47219 ),
 ( #8728, #93872 ),
 ( #71547, #2142 ),
 ( #40108, #63429 ),
 ( #16821, #92858 ),
 ( #8234, #23918 ),
 ( #39600, #61909 ),
 ( #17322, #33024 ),
 ( #54302, #55305 ),
 ( #55796, #47708 ),
 ( #24921, #70520 ),
 ( #9753, #23412 ),
 ( #62922, #39101 ),
 ( #56314, #17843 ),
 ( #40613, #86788 ),
 ( #78646, #54816 ),
 ( #79676, #1135 ) ),
 .UNSPECIFIED., .T., .F., .F.,
 ( 4, 2, 2, 2, 2, 2, 2, 2, 2, 2, 2, 2, 2, 2, 2, 2, 4 ),
 ( 2, 2 ),
 ( 0.000000000000000000, 0.06250000000000000000, 0.1250000000000000000, 0.1875000000000000000, 0.2500000000000000000, 0.3125000000000000000, 0.3750000000000000000, 0.4375000000000000000, 0.5000000000000000000, 0.5625000000000000000, 0.6250000000000000000, 0.6875000000000000000, 0.7500000000000000000, 0.8125000000000000000, 0.8750000000000000000, 0.9375000000000000000, 1.000000000000000000 ),
 ( 0.000000000000000000, 1.000000000000000000 ),
 .UNSPECIFIED. ) ;
#6118 = CARTESIAN_POINT ( 'NONE',  ( 18.33840876668534037, 32.36126292948895866, 6.180339887498949913 ) ) ;
#6119 = CARTESIAN_POINT ( 'NONE',  ( 47.84007798744509898, 106.1754093786579318, -10.00000000000000000 ) ) ;
#6120 = CARTESIAN_POINT ( 'NONE',  ( 205.4948664586259497, 274.1576266782160474, 10.82119204727489326 ) ) ;
#6121 = CARTESIAN_POINT ( 'NONE',  ( 25.63248128490755562, 16.92755873383626408, 6.180339887498953466 ) ) ;
#6122 = CARTESIAN_POINT ( 'NONE',  ( 198.3075590527773784, 287.1682275260610027, 16.94807365630277118 ) ) ;
#6123 = CARTESIAN_POINT ( 'NONE',  ( 161.6043392661310065, 250.7400689978998685, 14.26332272462310691 ) ) ;
#6124 = CIRCLE ( 'NONE', #70862, 7.273499999999997634 ) ;
#6125 = CARTESIAN_POINT ( 'NONE',  ( -1.691623377417284635, 160.6423013555410080, -4.594050593750043987 ) ) ;
#6126 = CARTESIAN_POINT ( 'NONE',  ( 175.4155855648062357, 286.4771596746830937, -12.38400456956481577 ) ) ;
#6127 = VERTEX_POINT ( 'NONE', #27748 ) ;
#6128 = AXIS2_PLACEMENT_3D ( 'NONE', #11069, #70858, #80496 ) ;
#6129 = CARTESIAN_POINT ( 'NONE',  ( 177.9714937548455680, 255.7189482022137383, 8.882064279750110813 ) ) ;
#6130 = CARTESIAN_POINT ( 'NONE',  ( 72.99813893926936714, 70.38310088471868653, -8.105588444390599889 ) ) ;
#6131 = CARTESIAN_POINT ( 'NONE',  ( 199.1867231605587278, 285.6454706231928071, -17.41989184023605475 ) ) ;
#6132 = CARTESIAN_POINT ( 'NONE',  ( 4.830370123010505168, 173.5958772461660828, -9.188101187500095079 ) ) ;
#6133 = CARTESIAN_POINT ( 'NONE',  ( 181.9452575149977065, 275.8400803543989355, -16.44639771376654735 ) ) ;
#6134 = CARTESIAN_POINT ( 'NONE',  ( 22.93916872074224855, 35.01751292744056343, 6.180339887498949913 ) ) ;
#6135 = LINE ( 'NONE', #36528, #20600 ) ;
#6136 = CARTESIAN_POINT ( 'NONE',  ( -110.0000000000000000, 0.000000000000000000, 59.99999999999999289 ) ) ;
#6137 = CARTESIAN_POINT ( 'NONE',  ( 81.38451658133408273, 39.76220097505215278, 2.033788753608857291E-15 ) ) ;
#6138 = CARTESIAN_POINT ( 'NONE',  ( 171.3928239984006723, 250.3015599828365509, -5.796133048607560845 ) ) ;
#6139 = B_SPLINE_SURFACE_WITH_KNOTS ( 'NONE', 3, 1, ( 
 ( #40049, #32476 ),
 ( #94312, #79113 ),
 ( #12175, #19301 ),
 ( #26379, #74494 ),
 ( #43036, #89235 ),
 ( #26876, #96815 ),
 ( #57755, #50653 ),
 ( #81120, #88731 ),
 ( #57257, #90207 ),
 ( #27864, #59231 ),
 ( #18783, #73980 ),
 ( #19785, #4564 ),
 ( #41558, #64880 ),
 ( #49662, #49181 ),
 ( #34954, #12688 ),
 ( #33996, #80117 ),
 ( #66365, #88232 ),
 ( #95826, #11687 ),
 ( #80619, #73480 ),
 ( #35953, #20277 ),
 ( #28354, #81605 ),
 ( #11194, #35460 ),
 ( #3107, #50168 ),
 ( #10679, #42547 ),
 ( #97297, #43555 ),
 ( #5072, #65854 ),
 ( #58743, #51151 ),
 ( #89716, #82115 ),
 ( #4064, #27372 ),
 ( #58257, #66855 ),
 ( #97784, #72501 ),
 ( #42063, #72997 ),
 ( #3587, #34468 ),
 ( #65366, #96308 ) ),
 .UNSPECIFIED., .T., .F., .F.,
 ( 4, 2, 2, 2, 2, 2, 2, 2, 2, 2, 2, 2, 2, 2, 2, 2, 4 ),
 ( 2, 2 ),
 ( 0.000000000000000000, 0.06250000000000000000, 0.1250000000000000000, 0.1875000000000000000, 0.2500000000000000000, 0.3125000000000000000, 0.3750000000000000000, 0.4375000000000000000, 0.5000000000000000000, 0.5625000000000000000, 0.6250000000000000000, 0.6875000000000000000, 0.7500000000000000000, 0.8125000000000000000, 0.8750000000000000000, 0.9375000000000000000, 1.000000000000000000 ),
 ( 0.000000000000000000, 1.000000000000000000 ),
 .UNSPECIFIED. ) ;
#6140 = CARTESIAN_POINT ( 'NONE',  ( 177.5863610073459427, 254.6759042037001848, -3.887113448368675339 ) ) ;
#6141 = CARTESIAN_POINT ( 'NONE',  ( 150.8360166798673561, 269.3913508296000145, 13.81437070545826806 ) ) ;
#6142 = EDGE_CURVE ( 'NONE', #67236, #17408, #46923, .T. ) ;
#6143 = EDGE_CURVE ( 'NONE', #2866, #32378, #15387, .T. ) ;
#6144 = CARTESIAN_POINT ( 'NONE',  ( 57.68498304950345812, 214.1115022471903444, -5.000000000000047962 ) ) ;
#6145 = LINE ( 'NONE', #76076, #40922 ) ;
#6146 = CIRCLE ( 'NONE', #51428, 2.471954595299370006 ) ;
#6147 = CARTESIAN_POINT ( 'NONE',  ( 148.0427192501136062, 274.2294838985851015, 9.385226820296049155 ) ) ;
#6148 = EDGE_CURVE ( 'NONE', #36369, #79500, #25619, .T. ) ;
#6149 = CARTESIAN_POINT ( 'NONE',  ( 12.62459875707045143, 178.0958772461660544, -9.188101187500095079 ) ) ;
#6150 = CARTESIAN_POINT ( 'NONE',  ( 168.1939926483296972, 286.2578356360547218, 4.106630047314361320 ) ) ;
#6151 = EDGE_CURVE ( 'NONE', #96434, #77358, #82289, .T. ) ;
#6152 = FACE_OUTER_BOUND ( 'NONE', #19578, .T. ) ;
#6153 = PLANE ( 'NONE',  #48095 ) ;
#6154 = CARTESIAN_POINT ( 'NONE',  ( 50.15574305400770072, 101.0118721476823964, -10.00000000000000000 ) ) ;
#6155 = CARTESIAN_POINT ( 'NONE',  ( 207.6826438088389750, 270.9301044032979462, 7.252082088659585146 ) ) ;
#6156 = CARTESIAN_POINT ( 'NONE',  ( 185.3916143550522122, 266.4269361941668990, 14.53728910407776098 ) ) ;
#6157 = DIRECTION ( 'NONE',  ( 0.5607300124661794838, -0.8279987035736700030, 0.000000000000000000 ) ) ;
#6158 = CARTESIAN_POINT ( 'NONE',  ( 164.1824377412969511, 281.5202305190522338, 9.046750956103593921 ) ) ;
#6159 = CARTESIAN_POINT ( 'NONE',  ( 13.17245041747802148, 29.64646525600389637, -2.839279412974133887 ) ) ;
#6160 = CARTESIAN_POINT ( 'NONE',  ( 148.4016473149517594, 273.6078022540229426, 8.470066617688926769 ) ) ;
#6161 = CARTESIAN_POINT ( 'NONE',  ( 71.41401697283629346, 59.26550905095592725, 15.74935196026153150 ) ) ;
#6162 = CARTESIAN_POINT ( 'NONE',  ( 186.8624879592976811, 268.0158595129609580, -15.20275046462360713 ) ) ;
#6163 = VERTEX_POINT ( 'NONE', #89116 ) ;
#6164 = CARTESIAN_POINT ( 'NONE',  ( 185.3078095671113772, 290.9215328420979176, 12.16701217945218083 ) ) ;
#6165 = CARTESIAN_POINT ( 'NONE',  ( 177.5636530406916620, 258.7959717445368142, 12.62758304280528066 ) ) ;
#6166 = CARTESIAN_POINT ( 'NONE',  ( 74.96950070121518195, 53.51615853226594055, -16.54031916057799023 ) ) ;
#6167 = CARTESIAN_POINT ( 'NONE',  ( 81.30291217968080275, 42.41553967202970199, 7.523264834473000207 ) ) ;
#6168 = VERTEX_POINT ( 'NONE', #12054 ) ;
#6169 = DIRECTION ( 'NONE',  ( 0.9628097264997651505, -0.2701803667135113662, 0.000000000000000000 ) ) ;
#6170 = CARTESIAN_POINT ( 'NONE',  ( 68.61511293431414060, 70.22156159657447461, -0.4539256867429169451 ) ) ;
#6171 = CARTESIAN_POINT ( 'NONE',  ( 77.19265361661118163, 63.55806316509790577, 15.06964695689175926 ) ) ;
#6172 = CARTESIAN_POINT ( 'NONE',  ( 155.6328838216860220, 261.0829332228125850, -17.51014940606912518 ) ) ;
#6173 = ORIENTED_EDGE ( 'NONE', *, *, #4201, .T. ) ;
#6174 = ORIENTED_EDGE ( 'NONE', *, *, #21173, .T. ) ;
#6176 = CARTESIAN_POINT ( 'NONE',  ( 170.8054577101068219, 287.4915981561377976, 8.526299399445241178 ) ) ;
#6175 = CARTESIAN_POINT ( 'NONE',  ( 186.7746357155629084, 272.1319419735754082, -16.70060704968626553 ) ) ;
#6177 = VERTEX_POINT ( 'NONE', #96184 ) ;
#6178 = CARTESIAN_POINT ( 'NONE',  ( 88.32926345284593594, 43.93619003093853337, -2.170256470903187740 ) ) ;
#6179 = AXIS2_PLACEMENT_3D ( 'NONE', #59047, #88050, #34284 ) ;
#6180 = DIRECTION ( 'NONE',  ( -0.3613624741150673336, -0.7937185950816985081, -0.4893137583626402387 ) ) ;
#6181 = CARTESIAN_POINT ( 'NONE',  ( 80.42701765378497214, 57.95285881342197598, 16.25594651261488011 ) ) ;
#6182 = DIRECTION ( 'NONE',  ( -0.7909930170786233505, 0.6118251767726273771, 0.000000000000000000 ) ) ;
#6183 = ORIENTED_EDGE ( 'NONE', *, *, #87161, .F. ) ;
#6184 = CARTESIAN_POINT ( 'NONE',  ( 87.68484451513312194, 45.24243923569854786, -6.260370172860385551 ) ) ;
#6185 = CARTESIAN_POINT ( 'NONE',  ( 149.6191398986701415, 271.4990432411842676, -11.66821883946526839 ) ) ;
#6186 = VECTOR ( 'NONE', #3874, 1000.000000000000227 ) ;
#6187 = ORIENTED_EDGE ( 'NONE', *, *, #36829, .T. ) ;
#6188 = CARTESIAN_POINT ( 'NONE',  ( 164.5348324038273518, 245.6643059921780718, 1.473102934610569958 ) ) ;
#6189 = AXIS2_PLACEMENT_3D ( 'NONE', #64785, #95731, #79524 ) ;
#6190 = CARTESIAN_POINT ( 'NONE',  ( 150.1462219700033813, 275.7016199270512402, -8.305148579817409171 ) ) ;
#6191 = ORIENTED_EDGE ( 'NONE', *, *, #2725, .T. ) ;
#6192 = CARTESIAN_POINT ( 'NONE',  ( 190.2935937139882299, 301.0488226629397559, 4.649863831023156813 ) ) ;
#6193 = CARTESIAN_POINT ( 'NONE',  ( 172.2407488011533871, 263.6222815918252422, -15.46399472876365344 ) ) ;
#6194 = VERTEX_POINT ( 'NONE', #19665 ) ;
#6195 = CARTESIAN_POINT ( 'NONE',  ( 158.6969344861375077, 274.7767743472534221, -13.28740588576491533 ) ) ;
#6196 = CARTESIAN_POINT ( 'NONE',  ( 42.09650208215185074, 24.70852965304482396, 1.583844403245330712 ) ) ;
#6197 = CARTESIAN_POINT ( 'NONE',  ( 164.9280325499431115, 267.7146836723554202, 17.76834957580831187 ) ) ;
#6198 = CARTESIAN_POINT ( 'NONE',  ( 83.47960489914133575, 52.40473646238481820, 14.81961029483872494 ) ) ;
#6199 = ORIENTED_EDGE ( 'NONE', *, *, #83155, .T. ) ;
#6200 = ORIENTED_EDGE ( 'NONE', *, *, #85678, .F. ) ;
#6201 = AXIS2_PLACEMENT_3D ( 'NONE', #52779, #22394, #15272 ) ;
#6202 = CARTESIAN_POINT ( 'NONE',  ( 73.67141920324468174, 69.63945410956655735, 9.591121436403057032 ) ) ;
#6203 = CARTESIAN_POINT ( 'NONE',  ( 147.5177358149801421, 275.1387818813681179, 4.867883209065928085 ) ) ;
#6204 = CARTESIAN_POINT ( 'NONE',  ( 82.36618331495026268, 53.78214551141627453, 15.85029956610786428 ) ) ;
#6205 = CARTESIAN_POINT ( 'NONE',  ( 192.7507137768506880, 296.7929658737652971, 11.30364540927242345 ) ) ;
#6206 = CARTESIAN_POINT ( 'NONE',  ( 191.3292802282752803, 299.2549609994807724, 8.303257185644898897 ) ) ;
#6207 = CARTESIAN_POINT ( 'NONE',  ( 191.1747001918821525, 299.5227014763493116, -9.654804683100723040 ) ) ;
#6208 = VECTOR ( 'NONE', #6353, 1000.000000000000000 ) ;
#6209 = DIRECTION ( 'NONE',  ( 0.4145187862775202015, -0.7179675985244525771, -0.5591929034707450175 ) ) ;
#6210 = ADVANCED_FACE ( 'NONE', ( #42906 ), #83287, .F. ) ;
#6211 = CARTESIAN_POINT ( 'NONE',  ( 167.0957737472305666, 246.8272050136007749, 1.963998143010642128 ) ) ;
#6212 = CARTESIAN_POINT ( 'NONE',  ( 70.96339409936065579, 72.09815267950916962, -0.4058125698486632071 ) ) ;
#6213 = CARTESIAN_POINT ( 'NONE',  ( 171.4797962540974652, 288.7824835811317143, 4.217883281193715028 ) ) ;
#6214 = DIRECTION ( 'NONE',  ( 0.2237140788069379993, 0.9746548163034761680, 0.000000000000000000 ) ) ;
#6215 = EDGE_LOOP ( 'NONE', ( #59856, #62245, #86227, #58381 ) ) ;
#6216 = CARTESIAN_POINT ( 'NONE',  ( 149.7298672153112591, 271.3072579029764029, -11.96904942057522270 ) ) ;
#6217 = CARTESIAN_POINT ( 'NONE',  ( 75.46068616328098244, 54.40098703217916665, -16.11819300020396994 ) ) ;
#6218 = CARTESIAN_POINT ( 'NONE',  ( 202.7749754141538006, 277.6906214767087704, 15.33344055037920128 ) ) ;
#6219 = CARTESIAN_POINT ( 'NONE',  ( 36.38358746446922254, 51.11404133282110962, 177.5919119679930134 ) ) ;
#6220 = CARTESIAN_POINT ( 'NONE',  ( 180.9602365206295929, 283.3372604617935622, -15.11549797918817895 ) ) ;
#6221 = CARTESIAN_POINT ( 'NONE',  ( 147.9312304387540564, 274.4225881843351544, -9.820174179285407590 ) ) ;
#6222 = VERTEX_POINT ( 'NONE', #84469 ) ;
#6223 = CARTESIAN_POINT ( 'NONE',  ( 163.3473224498206093, 247.7211335670114352, -10.00320358166632850 ) ) ;
#6224 = CARTESIAN_POINT ( 'NONE',  ( 205.7544487159363769, 273.3880016642347073, 10.04406142612960728 ) ) ;
#6225 = VECTOR ( 'NONE', #82490, 1000.000000000000000 ) ;
#6227 = EDGE_CURVE ( 'NONE', #48184, #31958, #42076, .T. ) ;
#6226 = CARTESIAN_POINT ( 'NONE',  ( 72.24563128311258708, 71.52449707465140705, 5.035610742599487821 ) ) ;
#6228 = CARTESIAN_POINT ( 'NONE',  ( 40.12992642340848448, 200.6427522451419065, 10.00000000000009237 ) ) ;
#6229 = CARTESIAN_POINT ( 'NONE',  ( 117.8466853168797428, 238.8458772461660544, 9.188101187500095079 ) ) ;
#6230 = CARTESIAN_POINT ( 'NONE',  ( 180.5626108788783313, 294.4595582549500250, -3.477258678576252482 ) ) ;
#6231 = CARTESIAN_POINT ( 'NONE',  ( 193.9979983253333842, 262.2552985615510579, -0.8131695963413709816 ) ) ;
#6232 = CARTESIAN_POINT ( 'NONE',  ( 104.4503548538632316, 221.1115022471901739, -5.000000000000041744 ) ) ;
#6233 = CARTESIAN_POINT ( 'NONE',  ( 175.4310824030733613, 253.5328469009434684, -3.918382160889689381 ) ) ;
#6234 = B_SPLINE_CURVE_WITH_KNOTS ( 'NONE', 3,
 ( #71408, #32884, #39967, #24297, #38479, #23278, #23784, #1998, #69393, #69884, #39463, #78006, #47086, #31877, #16691, #78510, #47582, #63787, #92728, #79024, #25285, #84631, #8598, #85132, #9, #16194 ),
 .UNSPECIFIED., .F., .F.,
 ( 4, 2, 2, 2, 2, 2, 2, 2, 2, 2, 2, 2, 4 ),
 ( 0.003565812906164105359, 0.003712674125762171519, 0.003786104735561204599, 0.003859535345360237679, 0.004006396564958202358, 0.004153257784556166170, 0.004446980223752116344, 0.004740702662948066519, 0.005915592419731927065, 0.007090482176515788479, 0.007677927054907681889, 0.007971649494103592165, 0.008265371933299504176 ),
 .UNSPECIFIED. ) ;
#6235 = CARTESIAN_POINT ( 'NONE',  ( 25.10051690851626560, 194.4869531367911293, 4.594050593750046652 ) ) ;
#6236 = VECTOR ( 'NONE', #49109, 1000.000000000000114 ) ;
#6237 = CARTESIAN_POINT ( 'NONE',  ( 147.7638709860940764, 275.5540662940547350, -3.738940778976949098 ) ) ;
#6238 = ORIENTED_EDGE ( 'NONE', *, *, #100231, .F. ) ;
#6239 = CARTESIAN_POINT ( 'NONE',  ( 72.86041354566070538, 69.04060312456013548, 9.737600754264374103 ) ) ;
#6240 = CARTESIAN_POINT ( 'NONE',  ( 181.2586407163293813, 267.7608388338027225, 14.99160397322970972 ) ) ;
#6241 = CYLINDRICAL_SURFACE ( 'NONE', #14161, 10.00000000000010658 ) ;
#6242 = CARTESIAN_POINT ( 'NONE',  ( 146.8058449195592061, 276.3718130816831149, 4.181814292810413392 ) ) ;
#6243 = CARTESIAN_POINT ( 'NONE',  ( 81.69339766308513617, 41.48081229801229597, -5.200024030478571646 ) ) ;
#6244 = DIRECTION ( 'NONE',  ( 0.4999999999999992784, -0.8660254037844390407, 0.000000000000000000 ) ) ;
#6245 = CARTESIAN_POINT ( 'NONE',  ( 176.6906187182376300, 285.7386481342455795, -12.05608563264864763 ) ) ;
#6246 = CARTESIAN_POINT ( 'NONE',  ( 203.3286960320409094, 267.8359400968079171, 2.569349860321338941 ) ) ;
#6247 = CARTESIAN_POINT ( 'NONE',  ( 104.2158063034569579, 237.6427522451419065, -10.00000000000009415 ) ) ;
#6248 = VECTOR ( 'NONE', #46702, 1000.000000000000000 ) ;
#6249 = ORIENTED_EDGE ( 'NONE', *, *, #59634, .T. ) ;
#6250 = CARTESIAN_POINT ( 'NONE',  ( 79.13712759260107532, 59.42437504702359519, -16.53516983581164013 ) ) ;
#6251 = VECTOR ( 'NONE', #40125, 1000.000000000000114 ) ;
#6252 = CARTESIAN_POINT ( 'NONE',  ( 202.2576150004249200, 280.3265299319959354, 16.24828394350762295 ) ) ;
#6253 = CARTESIAN_POINT ( 'NONE',  ( -69.57603038520839789, 62.23413909710347980, 59.99999999999999289 ) ) ;
#6254 = AXIS2_PLACEMENT_3D ( 'NONE', #24289, #15673, #54664 ) ;
#6255 = CARTESIAN_POINT ( 'NONE',  ( 4.640666744108908226, 182.6744531367911577, 4.594050593750047540 ) ) ;
#6256 = VECTOR ( 'NONE', #22984, 1000.000000000000227 ) ;
#6257 = CARTESIAN_POINT ( 'NONE',  ( 5.618660645053492608, 25.01751292744054567, 6.180339887498949913 ) ) ;
#6258 = CARTESIAN_POINT ( 'NONE',  ( 192.1966557276483911, 272.1854317587748255, 14.40833446829215347 ) ) ;
#6259 = CARTESIAN_POINT ( 'NONE',  ( 71.68833228970933646, 59.19930892918411303, -15.31119584666944711 ) ) ;
#6260 = CARTESIAN_POINT ( 'NONE',  ( 81.65569285109127406, 59.29250989802573457, 0.4698463103929529372 ) ) ;
#6261 = EDGE_CURVE ( 'NONE', #33698, #27127, #94044, .T. ) ;
#6263 = CARTESIAN_POINT ( 'NONE',  ( 48.02338713675939630, 198.5333772461660828, 9.188101187500095079 ) ) ;
#6262 = CARTESIAN_POINT ( 'NONE',  ( 198.1602621822531773, 277.2937910998977600, -15.34043159284401092 ) ) ;
#6264 = CARTESIAN_POINT ( 'NONE',  ( -23.73952538801239598, 24.43184193311134678, -10.00000000000000000 ) ) ;
#6265 = CARTESIAN_POINT ( 'NONE',  ( 72.68142160263464291, 57.13787751540092330, 16.37077060121746541 ) ) ;
#6266 = CARTESIAN_POINT ( 'NONE',  ( -32.97299853046111195, 95.39863959553431982, 43.99458562601660816 ) ) ;
#6267 = CARTESIAN_POINT ( 'NONE',  ( 207.3502731283117555, 271.5057873089173768, 6.280625384230454245 ) ) ;
#6268 = ORIENTED_EDGE ( 'NONE', *, *, #92878, .T. ) ;
#6269 = AXIS2_PLACEMENT_3D ( 'NONE', #92824, #77613, #84732 ) ;
#6270 = CARTESIAN_POINT ( 'NONE',  ( 165.3402721949960892, 269.3030652250268417, 17.34759000155790432 ) ) ;
#6271 = CARTESIAN_POINT ( 'NONE',  ( 5.723458822437122784, 184.1115022471903160, -5.000000000000047962 ) ) ;
#6272 = CARTESIAN_POINT ( 'NONE',  ( 163.7012083107868534, 247.1081852757374975, -6.544933039329257518 ) ) ;
#6273 = CARTESIAN_POINT ( 'NONE',  ( 138.9560545341254851, 251.0333772461660260, 9.188101187500095079 ) ) ;
#6274 = CARTESIAN_POINT ( 'NONE',  ( 23.04210978301307122, 28.70171378149919406, -9.188101187500004485 ) ) ;
#6275 = CARTESIAN_POINT ( 'NONE',  ( -9.517469918280088592, 23.54023200771947799, -10.00000000000000000 ) ) ;
#6276 = EDGE_CURVE ( 'NONE', #63506, #91070, #5933, .T. ) ;
#6277 = CARTESIAN_POINT ( 'NONE',  ( 83.65902391768069890, 51.64235791857056768, -14.83937710116058639 ) ) ;
#6278 = CARTESIAN_POINT ( 'NONE',  ( 76.62156306105930526, 63.43458379359962152, 15.37592086074862685 ) ) ;
#6280 = CARTESIAN_POINT ( 'NONE',  ( 75.03253579078814539, 67.12707870640632279, 13.05283704309126236 ) ) ;
#6279 = CARTESIAN_POINT ( 'NONE',  ( 88.05378287308985819, 43.82556038557745381, 2.467578420128289540 ) ) ;
#6281 = CARTESIAN_POINT ( 'NONE',  ( 170.0812506307862009, 258.7503018971702318, -15.45556229382616031 ) ) ;
#6282 = ORIENTED_EDGE ( 'NONE', *, *, #46472, .T. ) ;
#6283 = B_SPLINE_CURVE_WITH_KNOTS ( 'NONE', 3,
 ( #49577, #19704, #58660, #74409, #12089, #4480, #73396, #89632, #67269, #5482, #66285, #3507, #27787, #57667, #72916, #50570, #3982, #18695, #80530, #27291 ),
 .UNSPECIFIED., .F., .F.,
 ( 4, 2, 2, 2, 2, 2, 2, 2, 2, 4 ),
 ( 3.403994264753323137E-15, 0.0003780139803775907554, 0.0007560279607517774413, 0.001134041941125964181, 0.001512055921500150921, 0.001701062911687225643, 0.001890069901874300799, 0.002268083882248450676, 0.002646097862622600987, 0.003024111842996750864 ),
 .UNSPECIFIED. ) ;
#6284 = CARTESIAN_POINT ( 'NONE',  ( 154.1583213311439238, 272.3229918181682478, 14.15140380722988667 ) ) ;
#6285 = CARTESIAN_POINT ( 'NONE',  ( 189.9686529740312153, 299.6116365339944423, 6.575253125843024016 ) ) ;
#6286 = CARTESIAN_POINT ( 'NONE',  ( 74.41171749419693526, 66.31585784636642700, -13.36723480910198170 ) ) ;
#6287 = CARTESIAN_POINT ( 'NONE',  ( 169.7674466671218738, 266.1787835990222106, -16.83623305646149149 ) ) ;
#6288 = CARTESIAN_POINT ( 'NONE',  ( 3.825981621811214151, 23.18502408145589300, 5.678558825948276656 ) ) ;
#6290 = ORIENTED_EDGE ( 'NONE', *, *, #14645, .F. ) ;
#6289 = AXIS2_PLACEMENT_3D ( 'NONE', #43508, #51103, #19741 ) ;
#6291 = DIRECTION ( 'NONE',  ( -2.816764622163176999E-16, -1.626259812849726945E-16, 1.000000000000000000 ) ) ;
#6292 = CARTESIAN_POINT ( 'NONE',  ( 85.92832551797569351, 42.38550953085665896, -0.9154095918151041733 ) ) ;
#6293 = CARTESIAN_POINT ( 'NONE',  ( 75.42612112994180507, 53.21573441260188275, 16.48906790374613962 ) ) ;
#6294 = CARTESIAN_POINT ( 'NONE',  ( 71.64550269418319317, 72.08018802489503685, 0.6977335431020577072 ) ) ;
#6295 = CARTESIAN_POINT ( 'NONE',  ( 148.8368245119552284, 273.2444610639298617, -9.231145687738527172 ) ) ;
#6296 = CARTESIAN_POINT ( 'NONE',  ( 32.04156216231763210, 177.7592609112380444, 2.679491924311254714 ) ) ;
#6297 = CARTESIAN_POINT ( 'NONE',  ( 9.837252142675987798, 71.98620320469845524, 1.836970198720989751E-15 ) ) ;
#6298 = CARTESIAN_POINT ( 'NONE',  ( 68.25873685495425036, 69.52711191031835369, 3.726232860363765109 ) ) ;
#6299 = CARTESIAN_POINT ( 'NONE',  ( 153.3506059258413643, 265.0359544954067132, -16.39100908615009899 ) ) ;
#6300 = CARTESIAN_POINT ( 'NONE',  ( 195.4625579292164161, 281.9119700028093689, -17.76036160681684350 ) ) ;
#6301 = CARTESIAN_POINT ( 'NONE',  ( 8.827418999677703937, 23.83478043621386178, -8.090169943749479842 ) ) ;
#6302 = FACE_OUTER_BOUND ( 'NONE', #74654, .T. ) ;
#6303 = VERTEX_POINT ( 'NONE', #30731 ) ;
#6304 = CARTESIAN_POINT ( 'NONE',  ( 190.4249800432324662, 300.8212548652687133, 3.085047376053959400 ) ) ;
#6305 = PLANE ( 'NONE',  #27315 ) ;
#6306 = CARTESIAN_POINT ( 'NONE',  ( 189.1071431715656104, 297.0811097836661361, 8.130666790968703594 ) ) ;
#6308 = EDGE_LOOP ( 'NONE', ( #44167, #47915, #87686, #32478 ) ) ;
#6307 = B_SPLINE_CURVE_WITH_KNOTS ( 'NONE', 3,
 ( #62557, #76781, #53960, #93007 ),
 .UNSPECIFIED., .F., .F.,
 ( 4, 4 ),
 ( 0.04511453035517336979, 0.04887066958154941826 ),
 .UNSPECIFIED. ) ;
#6309 = DIRECTION ( 'NONE',  ( -0.5634352399127593447, -0.8261602328994366307, 0.000000000000000000 ) ) ;
#6310 = DIRECTION ( 'NONE',  ( -0.000000000000000000, -0.000000000000000000, -1.000000000000000000 ) ) ;
#6311 = CARTESIAN_POINT ( 'NONE',  ( 163.7707306762541748, 246.9877690064858484, 7.021959502997312086 ) ) ;
#6312 = CARTESIAN_POINT ( 'NONE',  ( 84.56954683517940907, 47.31801974212991979, -11.83040963924886135 ) ) ;
#6313 = CARTESIAN_POINT ( 'NONE',  ( 88.05624235485146301, 44.55787864911079765, -5.145732200269208967 ) ) ;
#6314 = ORIENTED_EDGE ( 'NONE', *, *, #48937, .F. ) ;
#6315 = CARTESIAN_POINT ( 'NONE',  ( 91.91987624320061911, 230.0024278399160949, 9.188101187500095079 ) ) ;
#6316 = DIRECTION ( 'NONE',  ( 0.000000000000000000, 0.000000000000000000, 1.000000000000000000 ) ) ;
#6317 = CARTESIAN_POINT ( 'NONE',  ( 178.0062659503225859, 269.1087611653143199, -16.50835682451741349 ) ) ;
#6318 = CARTESIAN_POINT ( 'NONE',  ( 81.29786749816629765, 42.48536220638202110, -7.641147779553272734 ) ) ;
#6319 = B_SPLINE_CURVE_WITH_KNOTS ( 'NONE', 3,
 ( #68142, #82422, #29164, #59029 ),
 .UNSPECIFIED., .F., .F.,
 ( 4, 4 ),
 ( 0.008739769553074294359, 0.01698173572311750812 ),
 .UNSPECIFIED. ) ;
#6320 = ORIENTED_EDGE ( 'NONE', *, *, #29714, .T. ) ;
#6321 = ORIENTED_EDGE ( 'NONE', *, *, #17732, .T. ) ;
#6322 = ORIENTED_EDGE ( 'NONE', *, *, #78793, .T. ) ;
#6323 = CARTESIAN_POINT ( 'NONE',  ( 160.6734846709049691, 282.6943762970620924, -6.583290857611773461 ) ) ;
#6324 = ORIENTED_EDGE ( 'NONE', *, *, #7725, .T. ) ;
#6325 = CARTESIAN_POINT ( 'NONE',  ( 151.1998204792857052, 278.0139405208182097, -4.510343437356565843 ) ) ;
#6326 = DIRECTION ( 'NONE',  ( -1.000000000000000000, 0.000000000000000000, 0.000000000000000000 ) ) ;
#6327 = ORIENTED_EDGE ( 'NONE', *, *, #85853, .F. ) ;
#6328 = CARTESIAN_POINT ( 'NONE',  ( 207.9622466093905189, 270.4458181468041289, 3.586592550214158681 ) ) ;
#6329 = CARTESIAN_POINT ( 'NONE',  ( -13.79761285583127872, 128.9229902121449811, 8.559299291603829198E-14 ) ) ;
#6330 = CARTESIAN_POINT ( 'NONE',  ( 153.1627746953036535, 265.3612877299463548, -17.72069958822647351 ) ) ;
#6331 = CARTESIAN_POINT ( 'NONE',  ( -23.56828086056981064, 99.64628362023964314, 45.19937630303414977 ) ) ;
#6333 = CARTESIAN_POINT ( 'NONE',  ( 82.69413518930780072, 53.98739327922660891, -15.48440177962634223 ) ) ;
#6332 = AXIS2_PLACEMENT_3D ( 'NONE', #71612, #71109, #24980 ) ;
#6334 = LINE ( 'NONE', #29633, #12246 ) ;
#6335 = ORIENTED_EDGE ( 'NONE', *, *, #69634, .T. ) ;
#6336 = DIRECTION ( 'NONE',  ( 0.4999999999999992784, -0.8660254037844390407, 0.000000000000000000 ) ) ;
#6337 = CARTESIAN_POINT ( 'NONE',  ( 9.991594722369004700, 23.95586893147753926, 7.433330006724141015 ) ) ;
#6338 = AXIS2_PLACEMENT_3D ( 'NONE', #79925, #49983, #80429 ) ;
#6339 = ORIENTED_EDGE ( 'NONE', *, *, #94964, .F. ) ;
#6340 = ADVANCED_FACE ( 'NONE', ( #5443 ), #98155, .F. ) ;
#6341 = CARTESIAN_POINT ( 'NONE',  ( 164.0584767703456066, 281.7763263192914565, 8.638174457797754613 ) ) ;
#6342 = DIRECTION ( 'NONE',  ( -0.9874733399847794857, -0.1577859398657057433, 0.000000000000000000 ) ) ;
#6343 = CIRCLE ( 'NONE', #51604, 70.00000000000001421 ) ;
#6345 = VERTEX_POINT ( 'NONE', #70718 ) ;
#6344 = CARTESIAN_POINT ( 'NONE',  ( 177.5337925685473408, 280.1858537220425092, 16.79564202278857721 ) ) ;
#6346 = CARTESIAN_POINT ( 'NONE',  ( 163.3543347837650686, 247.7089878483399730, 10.92686688779373405 ) ) ;
#6347 = EDGE_CURVE ( 'NONE', #70099, #22001, #39787, .T. ) ;
#6348 = CARTESIAN_POINT ( 'NONE',  ( 185.0156182622852441, 258.0389674772235935, 3.001315489709461382 ) ) ;
#6349 = CARTESIAN_POINT ( 'NONE',  ( 159.2202160840655552, 280.3973568208431288, -6.670942047025803845 ) ) ;
#6350 = DIRECTION ( 'NONE',  ( -0.000000000000000000, 0.000000000000000000, -1.000000000000000000 ) ) ;
#6351 = FACE_OUTER_BOUND ( 'NONE', #68131, .T. ) ;
#6352 = CARTESIAN_POINT ( 'NONE',  ( 169.5542383065973695, 254.4246916622037133, 11.34482188162280636 ) ) ;
#6353 = DIRECTION ( 'NONE',  ( -0.2649596321165964552, 0.4589235447807054058, -0.8480480961564325071 ) ) ;
#6354 = AXIS2_PLACEMENT_3D ( 'NONE', #78714, #55373, #24494 ) ;
#6355 = EDGE_LOOP ( 'NONE', ( #98084, #4556, #76845, #81766, #17453 ) ) ;
#6356 = CARTESIAN_POINT ( 'NONE',  ( 181.6129181475825760, 270.8901633951155077, -15.97990793206353821 ) ) ;
#6357 = CARTESIAN_POINT ( 'NONE',  ( 70.16720293958557875, 63.56956892108868118, -12.96925824068795130 ) ) ;
#6359 = EDGE_CURVE ( 'NONE', #50322, #83565, #57934, .T. ) ;
#6358 = CARTESIAN_POINT ( 'NONE',  ( 193.7547917776226427, 294.1291474128820482, -14.15125599393966205 ) ) ;
#6360 = CARTESIAN_POINT ( 'NONE',  ( -3.532187684056978583, 178.7677522451419350, -5.000000000000047962 ) ) ;
#6361 = CARTESIAN_POINT ( 'NONE',  ( -52.57320609282758994, 32.70376883311633520, -10.00000000000000000 ) ) ;
#6362 = B_SPLINE_CURVE_WITH_KNOTS ( 'NONE', 3,
 ( #90244, #43590, #21304, #52674, #52180, #20816, #5594, #6092, #23640, #46959, #83129, #51708, #60268, #77879, #74525, #13215, #54531, #13700, #44074, #14197, #36483, #45083, #77368, #7973, #85512, #39828, #88028, #49456, #71781, #41346, #64160, #78884, #33260, #63657, #9976, #48969, #17052, #32753, #17560, #47943, #2891, #3389, #24161, #72288, #72799, #10469, #64672, #55536, #79904, #33787, #95110, #70759 ),
 .UNSPECIFIED., .F., .F.,
 ( 4, 2, 2, 2, 2, 2, 2, 2, 2, 2, 2, 2, 2, 2, 2, 2, 2, 2, 2, 2, 2, 2, 2, 2, 2, 4 ),
 ( 0.0004385394321953336636, 0.0008914911018940902855, 0.001117966936743468569, 0.001344442771592846853, 0.001457680689017575894, 0.001570918606442304718, 0.001684156523867033758, 0.001797394441291762799, 0.002023870276141257959, 0.002250346110990753771, 0.003156249450389033220, 0.004062152789787312236, 0.004968056129185591252, 0.005421007798884741602, 0.005647483633734396574, 0.005760721551159234469, 0.005817340509871571884, 0.005873959468583910166, 0.005930578427296248449, 0.005987197386008586732, 0.006100435303433209520, 0.006326911138282458567, 0.006779862807980959263, 0.007232814477679459959, 0.007459290312528710741, 0.007685766147377961523 ),
 .UNSPECIFIED. ) ;
#6363 = LINE ( 'NONE', #5861, #79431 ) ;
#6364 = CARTESIAN_POINT ( 'NONE',  ( 203.4701571373468028, 278.2263453445292498, -15.29907731156314377 ) ) ;
#6365 = CARTESIAN_POINT ( 'NONE',  ( 72.10582633461223168, 72.29069366366150007, 1.276487819798711065 ) ) ;
#6366 = PLANE ( 'NONE',  #61347 ) ;
#6368 = CARTESIAN_POINT ( 'NONE',  ( 76.15850628665211275, 65.36065209603508208, 14.05241843883173125 ) ) ;
#6367 = CARTESIAN_POINT ( 'NONE',  ( 3.179769518870181777, 163.4548013555410080, -4.594050593750042211 ) ) ;
#6369 = AXIS2_PLACEMENT_3D ( 'NONE', #31175, #15470, #94030 ) ;
#6370 = CARTESIAN_POINT ( 'NONE',  ( 185.9351731181741059, 295.4263767797440892, 8.222620372872301076 ) ) ;
#6371 = ORIENTED_EDGE ( 'NONE', *, *, #34742, .F. ) ;
#6372 = VERTEX_POINT ( 'NONE', #1333 ) ;
#6373 = FACE_OUTER_BOUND ( 'NONE', #33608, .T. ) ;
#6374 = FACE_OUTER_BOUND ( 'NONE', #43332, .T. ) ;
#6375 = ADVANCED_FACE ( 'NONE', ( #54494 ), #23602, .T. ) ;
#6376 = CARTESIAN_POINT ( 'NONE',  ( 172.1580654244187087, 289.4298437067981240, 2.621979037154522629 ) ) ;
#6377 = CARTESIAN_POINT ( 'NONE',  ( 86.03398505837640187, 43.07944667279475226, 2.211680798076963494 ) ) ;
#6378 = CARTESIAN_POINT ( 'NONE',  ( 202.5254408350308495, 279.8626419788790827, -17.32378363213250694 ) ) ;
#6379 = CARTESIAN_POINT ( 'NONE',  ( 84.08331625476169791, 45.85772664244242947, 10.09099698929909827 ) ) ;
#6380 = CARTESIAN_POINT ( 'NONE',  ( 150.5904159330389405, 276.7600202670964791, 3.696576208654118290 ) ) ;
#6381 = CARTESIAN_POINT ( 'NONE',  ( 17.98330449086917682, 175.0643266524160140, -9.188101187500093303 ) ) ;
#6382 = CARTESIAN_POINT ( 'NONE',  ( 118.6312605172356598, 248.4869531367911293, 4.594050593750046652 ) ) ;
#6383 = CARTESIAN_POINT ( 'NONE',  ( 181.5281128488287834, 294.6324445685692126, -6.595065418016686110 ) ) ;
#6384 = CARTESIAN_POINT ( 'NONE',  ( 66.04530551455397358, 69.02646038902410908, 2.576574233892690469 ) ) ;
#6385 = CARTESIAN_POINT ( 'NONE',  ( 206.6548133100257587, 272.3286174528128072, -7.213596576582502529 ) ) ;
#6386 = LINE ( 'NONE', #45364, #45312 ) ;
#6387 = CARTESIAN_POINT ( 'NONE',  ( 69.78333826775208593, 199.5494855054051868, -2.679491924311248496 ) ) ;
#6388 = CARTESIAN_POINT ( 'NONE',  ( 193.8365934467825298, 294.9121671145370556, 14.14845633038902584 ) ) ;
#6389 = CARTESIAN_POINT ( 'NONE',  ( 161.4143265314674522, 251.0691807084224365, -12.94469757303959234 ) ) ;
#6390 = CARTESIAN_POINT ( 'NONE',  ( 81.73819839763727657, 45.44352528469654118, 11.62212099951958244 ) ) ;
#6391 = EDGE_CURVE ( 'NONE', #63506, #35869, #40800, .T. ) ;
#6392 = EDGE_CURVE ( 'NONE', #31723, #71916, #63120, .T. ) ;
#6393 = CARTESIAN_POINT ( 'NONE',  ( 164.8175787598647162, 249.8649966127220807, -10.54131631236613664 ) ) ;
#6394 = CARTESIAN_POINT ( 'NONE',  ( 194.4774025889061591, 266.1532203706993869, 7.847259440529423813 ) ) ;
#6395 = CARTESIAN_POINT ( 'NONE',  ( 55.54027346828191725, 191.3262482093457777, 3.021315404115420679E-15 ) ) ;
#6396 = CARTESIAN_POINT ( 'NONE',  ( 66.18285732059042914, 199.0177522451417929, 5.000000000000051514 ) ) ;
#6397 = EDGE_CURVE ( 'NONE', #39676, #31611, #24010, .T. ) ;
#6398 =( BOUNDED_CURVE ( )  B_SPLINE_CURVE ( 2, ( #77425, #1423, #86080, #9008, #16603, #25202, #33306, #64207, #93647 ),
 .UNSPECIFIED., .F., .T. ) 
 B_SPLINE_CURVE_WITH_KNOTS ( ( 3, 2, 2, 2, 3 ),
 ( 0.7137096774193548709, 0.7150537634408602461, 0.7177419354838709964, 0.7204301075268817467, 0.7217741935483871218 ),
 .UNSPECIFIED. ) 
 CURVE ( )  GEOMETRIC_REPRESENTATION_ITEM ( )  RATIONAL_B_SPLINE_CURVE ( ( 0.9330127018922194093, 0.9330127018922194093, 1.000000000000000000, 0.8660254037844387076, 1.000000000000000000, 0.8660254037844387076, 1.000000000000000000, 0.9330127018922194093, 0.9330127018922194093 ) ) 
 REPRESENTATION_ITEM ( '' )  );
#6399 = CARTESIAN_POINT ( 'NONE',  ( 181.4945938287030742, 267.9359334561378887, 15.00701915070772507 ) ) ;
#6400 = CARTESIAN_POINT ( 'NONE',  ( 95.57333414147498729, 235.1744531367911293, 4.594050593750047540 ) ) ;
#6401 = EDGE_CURVE ( 'NONE', #78746, #28265, #28686, .T. ) ;
#6402 = CARTESIAN_POINT ( 'NONE',  ( 11.38685760444945672, 12.28920272979924988, -7.433330006724141015 ) ) ;
#6403 = CARTESIAN_POINT ( 'NONE',  ( 190.7851866479434761, 300.1973587246873194, 7.931162401707728016 ) ) ;
#6404 = VECTOR ( 'NONE', #98362, 1000.000000000000000 ) ;
#6405 = EDGE_CURVE ( 'NONE', #18290, #20047, #79522, .T. ) ;
#6406 = DIRECTION ( 'NONE',  ( 0.9619696745371175695, -0.2731562652969027893, 0.000000000000000000 ) ) ;
#6408 = CARTESIAN_POINT ( 'NONE',  ( 84.64900121116050968, 42.46421430546889297, -2.907483025300086510 ) ) ;
#6407 = CARTESIAN_POINT ( 'NONE',  ( 18.70427805463205218, 12.92755873383625520, 6.180339887498953466 ) ) ;
#6409 = CARTESIAN_POINT ( 'NONE',  ( 203.9678271304799750, 272.5810641093525533, -9.740920016785768354 ) ) ;
#6410 = CARTESIAN_POINT ( 'NONE',  ( 150.6438662863770332, 269.7241650738195631, -14.92510732909997628 ) ) ;
#6411 = DIRECTION ( 'NONE',  ( -0.9820299053580098247, -0.1887253692075822886, 0.000000000000000000 ) ) ;
#6412 = CARTESIAN_POINT ( 'NONE',  ( 39.09967052555147404, 28.28920272979929962, -7.433330006724141015 ) ) ;
#6413 = CARTESIAN_POINT ( 'NONE',  ( 193.1569697810063531, 296.0893098336876506, -13.02398914535779539 ) ) ;
#6414 = CYLINDRICAL_SURFACE ( 'NONE', #58792, 16.60714546451156792 ) ;
#6415 = ORIENTED_EDGE ( 'NONE', *, *, #27524, .T. ) ;
#6416 = CARTESIAN_POINT ( 'NONE',  ( 30.20304716546516133, 19.29860640527293469, -2.839279412974138328 ) ) ;
#6417 = VECTOR ( 'NONE', #8640, 1000.000000000000114 ) ;
#6418 = CARTESIAN_POINT ( 'NONE',  ( 154.8238461974347615, 274.8835241144952874, -12.48494116114558672 ) ) ;
#6419 = CARTESIAN_POINT ( 'NONE',  ( 146.8868584395697781, 276.2314935489248455, -3.891417269505058396 ) ) ;
#6420 = CARTESIAN_POINT ( 'NONE',  ( 65.81655290991075447, 197.2592609112379876, 2.679491924311254714 ) ) ;
#6421 = EDGE_CURVE ( 'NONE', #74992, #58510, #40103, .T. ) ;
#6422 = EDGE_CURVE ( 'NONE', #51335, #15648, #995, .T. ) ;
#6423 = VERTEX_POINT ( 'NONE', #43678 ) ;
#6424 = CARTESIAN_POINT ( 'NONE',  ( 70.73318623536759731, 60.92596017579931811, 15.03791421717386001 ) ) ;
#6425 = CARTESIAN_POINT ( 'NONE',  ( 39.95181620016202118, 182.3262482093457493, 3.021315404115420679E-15 ) ) ;
#6426 = CARTESIAN_POINT ( 'NONE',  ( 156.5742463479611786, 268.2652725409449204, 15.70701561319111406 ) ) ;
#6427 = CARTESIAN_POINT ( 'NONE',  ( 173.2415407040283242, 253.7903840043475441, -9.089862982380825684 ) ) ;
#6428 = CONICAL_SURFACE ( 'NONE', #56528, 7.298499999999999766, 0.7853981633976494514 ) ;
#6429 = CARTESIAN_POINT ( 'NONE',  ( 132.5240116932087062, 253.9865022471903160, 10.00000000000009237 ) ) ;
#6430 = ORIENTED_EDGE ( 'NONE', *, *, #62643, .F. ) ;
#6431 = CARTESIAN_POINT ( 'NONE',  ( 73.28147120125912295, 69.89235501152899133, 9.618937042358501444 ) ) ;
#6432 = ORIENTED_EDGE ( 'NONE', *, *, #57621, .F. ) ;
#6433 = CARTESIAN_POINT ( 'NONE',  ( 86.60633125366983620, 44.49099921560663518, 5.921673564571794834 ) ) ;
#6434 = CARTESIAN_POINT ( 'NONE',  ( 181.4091070389452511, 290.9398227325178823, -11.15856678108262123 ) ) ;
#6435 = ORIENTED_EDGE ( 'NONE', *, *, #88569, .F. ) ;
#6436 = CARTESIAN_POINT ( 'NONE',  ( 86.37020013017546205, 47.54260244662367541, -11.08968936411753781 ) ) ;
#6437 = CARTESIAN_POINT ( 'NONE',  ( 158.7169418325966888, 256.1484519720124240, 16.12901909612147477 ) ) ;
#6438 = CARTESIAN_POINT ( 'NONE',  ( 190.5500686693750083, 278.8001826294041621, -16.51372018954678111 ) ) ;
#6439 = FACE_OUTER_BOUND ( 'NONE', #76343, .T. ) ;
#6440 = CARTESIAN_POINT ( 'NONE',  ( 152.8721808860877616, 265.8646109718731623, -17.65676496037632504 ) ) ;
#6441 = CARTESIAN_POINT ( 'NONE',  ( 33.95706010830453181, 41.64646525600393545, -2.839279412974133887 ) ) ;
#6442 = LINE ( 'NONE', #69719, #28418 ) ;
#6443 = VECTOR ( 'NONE', #20342, 1000.000000000000000 ) ;
#6444 = CARTESIAN_POINT ( 'NONE',  ( 184.7157775894015117, 297.3647472220100099, -4.497232409310948142 ) ) ;
#6445 = CARTESIAN_POINT ( 'NONE',  ( 87.59596448155561177, 45.49737888473278247, 6.855467717104687608 ) ) ;
#6446 = ORIENTED_EDGE ( 'NONE', *, *, #78162, .T. ) ;
#6447 = VERTEX_POINT ( 'NONE', #97413 ) ;
#6448 = CARTESIAN_POINT ( 'NONE',  ( 72.07457202599672996, 72.29788378598240683, -0.9408228227147766853 ) ) ;
#6449 = DIRECTION ( 'NONE',  ( 1.000000000000000000, 0.000000000000000000, 0.000000000000000000 ) ) ;
#6450 = CARTESIAN_POINT ( 'NONE',  ( 79.70163802149302512, 56.48321831271363180, 16.19055457390075503 ) ) ;
#6452 = CARTESIAN_POINT ( 'NONE',  ( 163.3721123024899100, 272.7106123632322578, -15.45002922943936952 ) ) ;
#6451 = CARTESIAN_POINT ( 'NONE',  ( 204.9103773355753617, 275.7318107871104189, 13.62808820451859937 ) ) ;
#6453 = LINE ( 'NONE', #91572, #48156 ) ;
#6454 = CARTESIAN_POINT ( 'NONE',  ( 69.33396002066325536, 69.83223954795549560, 6.100251480823068562 ) ) ;
#6455 = CARTESIAN_POINT ( 'NONE',  ( 76.44872654795528888, 60.25863428232945296, -15.81057438280002536 ) ) ;
#6456 = CARTESIAN_POINT ( 'NONE',  ( 190.4744901378711290, 300.7355008658671522, 0.04566709859947504224 ) ) ;
#6457 = CARTESIAN_POINT ( 'NONE',  ( 185.6331528164076019, 275.1493494416136514, -17.66137984873601496 ) ) ;
#6458 = CARTESIAN_POINT ( 'NONE',  ( 77.14345524627998429, 62.92765389764069539, -15.28297779662353761 ) ) ;
#6459 = CARTESIAN_POINT ( 'NONE',  ( 178.4479938518580866, 254.7379757184021685, 5.915197645450990471 ) ) ;
#6460 = CARTESIAN_POINT ( 'NONE',  ( 113.0020953926368037, 245.2369531367911009, -4.594050593750048428 ) ) ;
#6461 = ORIENTED_EDGE ( 'NONE', *, *, #14894, .T. ) ;
#6462 = CARTESIAN_POINT ( 'NONE',  ( 183.3861558808938810, 260.1507132443945238, -9.436288690551128511 ) ) ;
#6463 = CARTESIAN_POINT ( 'NONE',  ( 37.70440764347101492, 39.95586893147758900, 7.433330006724141015 ) ) ;
#6464 = CARTESIAN_POINT ( 'NONE',  ( 187.8353234249231321, 291.6460669958726157, -14.22777192653921041 ) ) ;
#6465 = ORIENTED_EDGE ( 'NONE', *, *, #31210, .F. ) ;
#6466 = ADVANCED_FACE ( 'NONE', ( #51274 ), #55001, .F. ) ;
#6467 = CARTESIAN_POINT ( 'NONE',  ( 163.1192251533336162, 248.6989372057958576, -9.692595118822335820 ) ) ;
#6468 = ADVANCED_FACE ( 'NONE', ( #77593 ), #97815, .F. ) ;
#6469 = DIRECTION ( 'NONE',  ( 0.5011331959107268030, 0.8653701635463872943, 0.000000000000000000 ) ) ;
#6470 = CARTESIAN_POINT ( 'NONE',  ( 196.0355168007595523, 291.1035201434990540, 17.55377893960077884 ) ) ;
#6471 = CARTESIAN_POINT ( 'NONE',  ( 69.02410329663756272, 70.46522642847207862, 3.828157181349015392 ) ) ;
#6472 = CARTESIAN_POINT ( 'NONE',  ( 95.42925689777531773, 219.2365022471902023, -10.00000000000009237 ) ) ;
#6473 = EDGE_LOOP ( 'NONE', ( #27778, #75629, #27689, #63250 ) ) ;
#6474 = CARTESIAN_POINT ( 'NONE',  ( 148.6802791471854448, 273.1251977639880693, 9.299514254131516111 ) ) ;
#6475 = ORIENTED_EDGE ( 'NONE', *, *, #66651, .F. ) ;
#6476 = LINE ( 'NONE', #84018, #31696 ) ;
#6477 = VERTEX_POINT ( 'NONE', #11198 ) ;
#6479 = EDGE_CURVE ( 'NONE', #75209, #26122, #47658, .T. ) ;
#6478 = CARTESIAN_POINT ( 'NONE',  ( 152.3360070569975449, 270.2436951681156643, -14.78697292633622951 ) ) ;
#6480 = AXIS2_PLACEMENT_3D ( 'NONE', #55516, #94577, #16040 ) ;
#6481 = CARTESIAN_POINT ( 'NONE',  ( 196.2834844919150612, 264.3817122522384579, 3.934541318863804094 ) ) ;
#6482 = FACE_OUTER_BOUND ( 'NONE', #37960, .T. ) ;
#6483 = CARTESIAN_POINT ( 'NONE',  ( 82.63223242006407077, 45.40567870588363064, 10.45052338476836873 ) ) ;
#6485 = CARTESIAN_POINT ( 'NONE',  ( 157.0825463324651707, 280.7710845550788576, 6.027187208097937621 ) ) ;
#6484 = LINE ( 'NONE', #99190, #32228 ) ;
#6486 = CARTESIAN_POINT ( 'NONE',  ( 201.3505934466285510, 281.8975373467312693, -16.83770227898004279 ) ) ;
#6487 = ORIENTED_EDGE ( 'NONE', *, *, #37774, .F. ) ;
#6488 = CARTESIAN_POINT ( 'NONE',  ( 157.4729130248890954, 257.8959091554543761, 17.83439074639795052 ) ) ;
#6489 = FACE_OUTER_BOUND ( 'NONE', #87749, .T. ) ;
#6490 = CARTESIAN_POINT ( 'NONE',  ( 190.6636931378345992, 264.2239263948314374, -9.507720587469599138 ) ) ;
#6491 = CARTESIAN_POINT ( 'NONE',  ( 171.6851387733911167, 250.5862967750797736, -0.2559814552254628395 ) ) ;
#6493 = EDGE_CURVE ( 'NONE', #15032, #95607, #95796, .T. ) ;
#6492 = CARTESIAN_POINT ( 'NONE',  ( 189.1666306803385282, 269.6788385675433233, -13.95880351805504382 ) ) ;
#6494 = CARTESIAN_POINT ( 'NONE',  ( 71.81276634784433099, 72.21619144530795609, 3.256612196116187352 ) ) ;
#6495 = ADVANCED_FACE ( 'NONE', ( #56262 ), #8093, .T. ) ;
#6496 = CARTESIAN_POINT ( 'NONE',  ( 84.58839726686360905, 45.66716180150288551, 9.521216735525740660 ) ) ;
#6497 = CARTESIAN_POINT ( 'NONE',  ( 68.10039974585599509, 65.18542567973287305, -10.72853162865224519 ) ) ;
#6498 = AXIS2_PLACEMENT_3D ( 'NONE', #73295, #80430, #11003 ) ;
#6499 = CARTESIAN_POINT ( 'NONE',  ( 29.10614472461701752, 187.6115022471902591, 10.00000000000009592 ) ) ;
#6500 = CARTESIAN_POINT ( 'NONE',  ( 82.53793375827495993, 54.22719885510827709, -15.94096427280454087 ) ) ;
#6501 = CARTESIAN_POINT ( 'NONE',  ( 82.77265646360999085, 218.5958772461660544, -9.188101187500095079 ) ) ;
#6502 = CARTESIAN_POINT ( 'NONE',  ( 159.9770824720811220, 253.5585604421560788, -16.42166711341322483 ) ) ;
#6503 = CARTESIAN_POINT ( 'NONE',  ( 77.59577977556848793, 61.80410179206373300, 15.66623212455446890 ) ) ;
#6504 = CARTESIAN_POINT ( 'NONE',  ( 163.3020905273760093, 247.7994775548095845, -11.05431316445765155 ) ) ;
#6505 = B_SPLINE_CURVE_WITH_KNOTS ( 'NONE', 3,
 ( #53653, #98800, #52659, #92226 ),
 .UNSPECIFIED., .F., .F.,
 ( 4, 4 ),
 ( 0.03592842450685154038, 0.04464100137491056747 ),
 .UNSPECIFIED. ) ;
#6506 = CARTESIAN_POINT ( 'NONE',  ( 196.9526636073363477, 287.5149752765084941, -17.63101726665603053 ) ) ;
#6507 = CARTESIAN_POINT ( 'NONE',  ( 207.3874697692679945, 271.4413608369101780, -6.809237722377445401 ) ) ;
#6508 = CYLINDRICAL_SURFACE ( 'NONE', #69176, 17.82106496071139645 ) ;
#6510 = CARTESIAN_POINT ( 'NONE',  ( 185.9530610298360216, 265.4397761326690670, 13.93956406728625375 ) ) ;
#6509 = CARTESIAN_POINT ( 'NONE',  ( 108.1850894041357094, 223.2677522451417929, -5.000000000000041744 ) ) ;
#6511 = CARTESIAN_POINT ( 'NONE',  ( 188.1065894726285990, 258.8392727029177536, -0.5366119281032075694 ) ) ;
#6512 = CARTESIAN_POINT ( 'NONE',  ( 41.88317952681261858, 32.38052372038644933, 10.00000000000000533 ) ) ;
#6513 = CARTESIAN_POINT ( 'NONE',  ( -19.65312891409030271, 93.06504152958497400, -10.00000000000000888 ) ) ;
#6514 = CARTESIAN_POINT ( 'NONE',  ( 82.78960406368588565, 53.73890389198745510, 15.39558355803757728 ) ) ;
#6515 = CARTESIAN_POINT ( 'NONE',  ( 71.92161918111298746, 71.97213927130549393, 2.836694015421989956 ) ) ;
#6516 = ADVANCED_FACE ( 'NONE', ( #3591 ), #59235, .T. ) ;
#6517 = CARTESIAN_POINT ( 'NONE',  ( 29.83685365728618066, 188.0333772461660544, 9.188101187500095079 ) ) ;
#6518 = CARTESIAN_POINT ( 'NONE',  ( 157.7365441389748923, 257.4392866714015895, 18.13124212464487073 ) ) ;
#6519 = CARTESIAN_POINT ( 'NONE',  ( 199.3165775953382024, 277.8358694028592595, 15.47252840930216067 ) ) ;
#6520 = ADVANCED_FACE ( 'NONE', ( #19788 ), #39615, .F. ) ;
#6521 = CARTESIAN_POINT ( 'NONE',  ( 81.19178922867995141, 50.25691689511806004, -14.37495122601996655 ) ) ;
#6522 = CARTESIAN_POINT ( 'NONE',  ( 72.02678134044498393, 72.22633079433387593, -1.610807377262633899 ) ) ;
#6523 = CARTESIAN_POINT ( 'NONE',  ( 39.14627965220388006, 205.6589784336661637, -6.496448406907676862E-16 ) ) ;
#6524 = CARTESIAN_POINT ( 'NONE',  ( 25.16147942602835030, 23.03085787977763843, 9.188101187500006262 ) ) ;
#6525 = CARTESIAN_POINT ( 'NONE',  ( 151.1451503555562113, 268.8559155969762742, -15.81507177720227553 ) ) ;
#6526 = CARTESIAN_POINT ( 'NONE',  ( 196.9976074755333286, 289.4371302133026802, -16.79549473444794216 ) ) ;
#6527 = CARTESIAN_POINT ( 'NONE',  ( 44.85148386036637191, 26.86426979415093541, -3.090169943749474069 ) ) ;
#6528 = CARTESIAN_POINT ( 'NONE',  ( 157.4893260420801653, 257.8674809757739013, -18.30842125257398223 ) ) ;
#6529 = CARTESIAN_POINT ( 'NONE',  ( 202.9014212808193918, 270.0062346898790793, -6.438034076772497727 ) ) ;
#6530 = CARTESIAN_POINT ( 'NONE',  ( 174.9358745049650565, 292.2217799751211942, 2.235529367806339263 ) ) ;
#6531 = ADVANCED_FACE ( 'NONE', ( #57618 ), #61434, .F. ) ;
#6532 = CARTESIAN_POINT ( 'NONE',  ( 179.2582380156520401, 276.5659109761746777, 16.30564618147165845 ) ) ;
#6533 = CARTESIAN_POINT ( 'NONE',  ( 72.34119125645204917, 60.41698090225992956, 15.06063977213209881 ) ) ;
#6534 = CARTESIAN_POINT ( 'NONE',  ( 153.3384820949992502, 276.8128241755385943, 7.236455069745591828 ) ) ;
#6535 = B_SPLINE_CURVE_WITH_KNOTS ( 'NONE', 3,
 ( #36354, #88635, #3971, #50558, #34853, #19201, #96212, #12585, #89623, #80517, #11591, #28260, #51051, #35363, #65757, #96711, #95730, #27279, #89142, #81509, #59134, #26281, #20184, #82011, #43457, #11093, #65269, #12079, #42938, #73877, #45446, #76379, #99174, #37347, #45933, #36857, #67259, #6954, #21183, #90619, #91589, #92114, #22160, #7966, #61141, #44950, #30256, #75890 ),
 .UNSPECIFIED., .F., .F.,
 ( 4, 2, 2, 2, 2, 2, 2, 2, 2, 2, 2, 2, 2, 2, 2, 2, 2, 2, 2, 2, 2, 2, 2, 4 ),
 ( 0.001614394524384737788, 0.002072026746786071599, 0.002529658969187404977, 0.002758475080388071883, 0.002872883135988325322, 0.002987291191588578761, 0.003101699247188831766, 0.003216107302789084771, 0.003444923413989510116, 0.003902555636390277975, 0.004360187858791046700, 0.005275452303592720327, 0.006190716748394393953, 0.006648348970795231634, 0.007105981193196068448, 0.007220389248796255967, 0.007277593276596350594, 0.007334797304396444353, 0.007449205359996691721, 0.007563613415596938221, 0.008021245637998029171, 0.008478877860399122723, 0.008707693971599577559, 0.008936510082800030660 ),
 .UNSPECIFIED. ) ;
#6536 = LINE ( 'NONE', #51121, #16956 ) ;
#6537 = CARTESIAN_POINT ( 'NONE',  ( 103.2234855318352373, 223.7365022471902023, -10.00000000000009059 ) ) ;
#6538 = DIRECTION ( 'NONE',  ( -0.3535533905933014309, 0.6123724356957908066, -0.7071067811865369146 ) ) ;
#6539 = DIRECTION ( 'NONE',  ( -0.8660254037844382635, -0.5000000000000004441, 0.000000000000000000 ) ) ;
#6540 = ORIENTED_EDGE ( 'NONE', *, *, #15936, .F. ) ;
#6541 = CARTESIAN_POINT ( 'NONE',  ( 60.95981515367195414, 199.8768266524160140, 9.188101187500098632 ) ) ;
#6542 = ORIENTED_EDGE ( 'NONE', *, *, #92994, .T. ) ;
#6543 = CARTESIAN_POINT ( 'NONE',  ( 166.1065669591089886, 265.3346322838461333, 16.55527594901084854 ) ) ;
#6544 = CARTESIAN_POINT ( 'NONE',  ( 162.7414887829580721, 250.5555091418873985, 12.74047579032432687 ) ) ;
#6546 = DIRECTION ( 'NONE',  ( -0.8660254037844387076, -0.4999999999999998890, -0.000000000000000000 ) ) ;
#6545 = VECTOR ( 'NONE', #4599, 1000.000000000000000 ) ;
#6547 = EDGE_LOOP ( 'NONE', ( #90408, #59140, #77188, #91238 ) ) ;
#6548 = DIRECTION ( 'NONE',  ( 1.000000000000000000, 1.855658484016332714E-13, 0.000000000000000000 ) ) ;
#6549 = CARTESIAN_POINT ( 'NONE',  ( 79.30106977174941107, 46.37009440408895244, -12.77856967582355985 ) ) ;
#6550 = CARTESIAN_POINT ( 'NONE',  ( 71.41016749218992743, 59.45273978182970609, 15.69346469599747174 ) ) ;
#6551 = CARTESIAN_POINT ( 'NONE',  ( 84.83882459461941039, 41.93430961319199213, 2.331212101531141112 ) ) ;
#6552 = CARTESIAN_POINT ( 'NONE',  ( -3.376183997657045133, 64.08949848310733444, -10.00000000000000000 ) ) ;
#6553 = CARTESIAN_POINT ( 'NONE',  ( 204.3227106360847927, 276.7496793685443208, 13.60086062244164573 ) ) ;
#6554 = ORIENTED_EDGE ( 'NONE', *, *, #7512, .F. ) ;
#6555 = CARTESIAN_POINT ( 'NONE',  ( 23.10466909204031083, 21.84335787977763133, 9.188101187500006262 ) ) ;
#6556 = CARTESIAN_POINT ( 'NONE',  ( 75.52901062100019658, 57.36030880927751952, 16.09556828531399120 ) ) ;
#6557 = CARTESIAN_POINT ( 'NONE',  ( 69.50278484786903732, 70.03302840163392773, -4.514860484484302994 ) ) ;
#6558 = DIRECTION ( 'NONE',  ( 0.4270171210482451851, -0.9042435392811322137, 0.000000000000000000 ) ) ;
#6559 = ORIENTED_EDGE ( 'NONE', *, *, #13796, .F. ) ;
#6560 = CARTESIAN_POINT ( 'NONE',  ( 47.05668214639808156, 76.45164061169337799, 10.00000000000000000 ) ) ;
#6561 = CARTESIAN_POINT ( 'NONE',  ( 206.3018347371251195, 273.3217358710584790, -9.309724106897926177 ) ) ;
#6562 = ORIENTED_EDGE ( 'NONE', *, *, #77355, .F. ) ;
#6563 = VECTOR ( 'NONE', #69889, 1000.000000000000114 ) ;
#6564 = ORIENTED_EDGE ( 'NONE', *, *, #23596, .F. ) ;
#6565 = CARTESIAN_POINT ( 'NONE',  ( 78.96783115249304785, 50.21060704042795209, -14.86080133530415992 ) ) ;
#6567 = DIRECTION ( 'NONE',  ( -1.000000000000000000, 0.000000000000000000, 0.000000000000000000 ) ) ;
#6566 = CARTESIAN_POINT ( 'NONE',  ( 161.3004582353723322, 282.7615572226706604, -3.141450372068092634 ) ) ;
#6568 = CARTESIAN_POINT ( 'NONE',  ( 189.7726967107949747, 264.4065126852114531, 11.24316165915873000 ) ) ;
#6569 = CARTESIAN_POINT ( 'NONE',  ( 163.7707306762541748, 246.9877690064858484, 7.021959502997312086 ) ) ;
#6570 = DIRECTION ( 'NONE',  ( -0.6857383512133925496, -0.7278481391575704063, 0.000000000000000000 ) ) ;
#6571 = CARTESIAN_POINT ( 'NONE',  ( 81.22503698233943226, 55.71330003141861198, 16.38398667929945773 ) ) ;
#6572 = CARTESIAN_POINT ( 'NONE',  ( 161.2003520097632929, 263.0782596298864178, -17.28377924258164455 ) ) ;
#6573 = EDGE_CURVE ( 'NONE', #73457, #24730, #91065, .T. ) ;
#6574 = CARTESIAN_POINT ( 'NONE',  ( 135.5734031224162663, 239.8923013555409796, 4.594050593750050204 ) ) ;
#6575 = CARTESIAN_POINT ( 'NONE',  ( 198.2505066714982149, 285.2670451491296149, 0.000000000000000000 ) ) ;
#6576 = CARTESIAN_POINT ( 'NONE',  ( 195.7755322585767317, 290.7755156195648851, -16.12766413607943150 ) ) ;
#6577 = CARTESIAN_POINT ( 'NONE',  ( 78.09096694622414248, 206.7048013555409796, 4.594050593750051981 ) ) ;
#6578 = ORIENTED_EDGE ( 'NONE', *, *, #73874, .T. ) ;
#6579 = CARTESIAN_POINT ( 'NONE',  ( 170.2456429460595757, 264.0157069346884668, 17.14554996422683431 ) ) ;
#6580 = CARTESIAN_POINT ( 'NONE',  ( 72.27760156895793386, 60.37162225583013253, -15.57713023393894147 ) ) ;
#6581 = CARTESIAN_POINT ( 'NONE',  ( -6.542761065016642341, 25.57183462804972507, -10.00000000000000000 ) ) ;
#6582 = VERTEX_POINT ( 'NONE', #14024 ) ;
#6583 = CARTESIAN_POINT ( 'NONE',  ( 160.2064895855051248, 253.7921695486214446, 15.02796977922756838 ) ) ;
#6584 = ORIENTED_EDGE ( 'NONE', *, *, #82033, .F. ) ;
#6585 = ORIENTED_EDGE ( 'NONE', *, *, #1126, .T. ) ;
#6586 = DIRECTION ( 'NONE',  ( -1.000000000000000000, 0.000000000000000000, 0.000000000000000000 ) ) ;
#6587 = CARTESIAN_POINT ( 'NONE',  ( 67.11284809570460652, 67.67925989217837923, 6.627993865167674414 ) ) ;
#6588 = CARTESIAN_POINT ( 'NONE',  ( 190.0667283601964357, 259.9641452334862493, -5.090329199819447104E-14 ) ) ;
#6589 = CARTESIAN_POINT ( 'NONE',  ( 81.53115339410010165, 41.92267797703283350, -7.515177224638171616 ) ) ;
#6590 = CARTESIAN_POINT ( 'NONE',  ( 81.50373498261929228, 55.81176558511297969, 16.37496158676513858 ) ) ;
#6591 = CARTESIAN_POINT ( 'NONE',  ( 193.0512205562391159, 275.6825563886401369, -16.88465587640301280 ) ) ;
#6592 = CARTESIAN_POINT ( 'NONE',  ( 71.24781679453236904, 66.22908028783459145, 11.48236923496973461 ) ) ;
#6593 = CARTESIAN_POINT ( 'NONE',  ( 87.52489256634972037, 45.06004022996453529, 6.936227203615889181 ) ) ;
#6594 = ORIENTED_EDGE ( 'NONE', *, *, #97048, .F. ) ;
#6595 = CARTESIAN_POINT ( 'NONE',  ( 206.8711744556208885, 269.6661967102621702, -5.660351959544826712E-12 ) ) ;
#6596 = ORIENTED_EDGE ( 'NONE', *, *, #1496, .F. ) ;
#6597 = CARTESIAN_POINT ( 'NONE',  ( 76.18516340950158394, 51.05281452121147368, -16.05953048902229341 ) ) ;
#6598 = EDGE_CURVE ( 'NONE', #66853, #49704, #40122, .T. ) ;
#6599 = CARTESIAN_POINT ( 'NONE',  ( 183.7168947869212161, 275.6071481288901168, 16.66324111737131730 ) ) ;
#6600 = CARTESIAN_POINT ( 'NONE',  ( 206.5318754762992910, 272.9232936229979032, 10.63244694018452741 ) ) ;
#6601 = CARTESIAN_POINT ( 'NONE',  ( 169.5608680270499917, 283.3855602016760713, -12.49222823364715040 ) ) ;
#6602 = DIRECTION ( 'NONE',  ( -0.7510153523339188064, 0.6602847420308604054, 0.000000000000000000 ) ) ;
#6603 = CARTESIAN_POINT ( 'NONE',  ( 162.8296681715975467, 261.5150638136722137, 17.10512620579534726 ) ) ;
#6604 = CARTESIAN_POINT ( 'NONE',  ( 145.9657079678295020, 245.8923013555409511, 4.594050593750050204 ) ) ;
#6605 = ORIENTED_EDGE ( 'NONE', *, *, #77001, .F. ) ;
#6606 = DIRECTION ( 'NONE',  ( 0.5866775868892262213, 0.8098206029991052990, 0.000000000000000000 ) ) ;
#6607 = CARTESIAN_POINT ( 'NONE',  ( 86.99715697556658256, 45.94190566429735867, 8.138834009077100973 ) ) ;
#6608 = CARTESIAN_POINT ( 'NONE',  ( 166.5303610463213602, 284.3444823442944767, -9.543174262395664798 ) ) ;
#6609 = EDGE_CURVE ( 'NONE', #29494, #48939, #74160, .T. ) ;
#6610 = CARTESIAN_POINT ( 'NONE',  ( 72.91771958014867039, 70.92947700147982459, 7.881516594485344918 ) ) ;
#6611 = EDGE_CURVE ( 'NONE', #96074, #69981, #4947, .T. ) ;
#6612 = CARTESIAN_POINT ( 'NONE',  ( 68.70919837959567644, 67.43310744183247607, -8.574709995985422495 ) ) ;
#6613 = EDGE_LOOP ( 'NONE', ( #62285, #28371, #75099, #89383 ) ) ;
#6614 = CARTESIAN_POINT ( 'NONE',  ( 199.5606914717536711, 266.8596729079026204, 4.600230128018988118 ) ) ;
#6615 = CARTESIAN_POINT ( 'NONE',  ( 204.0884846259506276, 275.1553707185394728, 13.46337290381501717 ) ) ;
#6616 = CARTESIAN_POINT ( 'NONE',  ( 72.26490814316112221, 71.11794692069462087, -6.031233613558444340 ) ) ;
#6617 = CARTESIAN_POINT ( 'NONE',  ( 185.1897086401880586, 263.6483258020415974, -12.64245034936682721 ) ) ;
#6618 = CARTESIAN_POINT ( 'NONE',  ( 73.72239016385701404, 69.47467296629645261, -9.830903513004800587 ) ) ;
#6619 = CARTESIAN_POINT ( 'NONE',  ( 195.1395877695788670, 263.6489633415297931, 0.8500072188313321231 ) ) ;
#6620 = B_SPLINE_CURVE_WITH_KNOTS ( 'NONE', 3,
 ( #31688, #23101, #15496, #54488 ),
 .UNSPECIFIED., .F., .F.,
 ( 4, 4 ),
 ( 0.008185375094193318019, 0.01430533136218472591 ),
 .UNSPECIFIED. ) ;
#6621 = VERTEX_POINT ( 'NONE', #90582 ) ;
#6622 = FACE_BOUND ( 'NONE', #64006, .T. ) ;
#6623 = CARTESIAN_POINT ( 'NONE',  ( 186.4575292785845022, 282.5265642665722794, 16.18250184841760841 ) ) ;
#6624 = CARTESIAN_POINT ( 'NONE',  ( 207.1122325394003951, 271.9180857031755636, 7.794245785756032774 ) ) ;
#6626 = CARTESIAN_POINT ( 'NONE',  ( 196.2721503905644056, 270.7675346716773106, 11.95883742778919157 ) ) ;
#6625 = CARTESIAN_POINT ( 'NONE',  ( 155.0197698005585494, 262.1448778582381465, 18.42918111182112284 ) ) ;
#6627 = CARTESIAN_POINT ( 'NONE',  ( 27.36453209247643414, 17.92755873383626408, 6.180339887498953466 ) ) ;
#6628 = DIRECTION ( 'NONE',  ( 0.9995565931350004485, 0.02977611660964677581, 0.000000000000000000 ) ) ;
#6629 = FACE_OUTER_BOUND ( 'NONE', #37555, .T. ) ;
#6630 = CARTESIAN_POINT ( 'NONE',  ( 24.23155096423127475, 19.15404122711133894, 8.090169943749479842 ) ) ;
#6631 = CARTESIAN_POINT ( 'NONE',  ( 160.0072461633487535, 253.5063153963366744, 16.23938890643736244 ) ) ;
#6632 = VECTOR ( 'NONE', #76579, 1000.000000000000000 ) ;
#6633 = CARTESIAN_POINT ( 'NONE',  ( 36.81131572470497559, 77.10862815663108449, 59.99999999999999289 ) ) ;
#6634 = EDGE_CURVE ( 'NONE', #37194, #94538, #27738, .T. ) ;
#6635 = CARTESIAN_POINT ( 'NONE',  ( 150.9811781078167598, 244.6427522451417360, 1.119607411625061291E-15 ) ) ;
#6636 = LINE ( 'NONE', #525, #80880 ) ;
#6637 = ORIENTED_EDGE ( 'NONE', *, *, #81998, .T. ) ;
#6638 = CARTESIAN_POINT ( 'NONE',  ( 67.08288010347953900, 67.73116597731298327, -6.493375440012594701 ) ) ;
#6639 = CARTESIAN_POINT ( 'NONE',  ( 72.97800438629489861, 70.36521761891982862, -8.115508188870068196 ) ) ;
#6640 = CARTESIAN_POINT ( 'NONE',  ( 202.5477177782173897, 274.2023237505306383, -12.92955543092264215 ) ) ;
#6641 = CARTESIAN_POINT ( 'NONE',  ( 198.9590707264871412, 286.0397762054715827, -17.05306195936250191 ) ) ;
#6642 = CARTESIAN_POINT ( 'NONE',  ( 1.717831006336420607, 180.9869531367911293, 4.594050593750046652 ) ) ;
#6643 = CARTESIAN_POINT ( 'NONE',  ( 178.4244581223062767, 273.6332221299129515, -17.11712909880773736 ) ) ;
#6644 = CARTESIAN_POINT ( 'NONE',  ( 32.72712820738424000, 19.86426979415091054, -3.090169943749474069 ) ) ;
#6645 = CARTESIAN_POINT ( 'NONE',  ( 85.31730801475342219, 49.09321715058120361, 12.43107433435324616 ) ) ;
#6646 = CARTESIAN_POINT ( 'NONE',  ( 70.58515312316130519, 204.8927522451418213, -10.00000000000009237 ) ) ;
#6647 = DIRECTION ( 'NONE',  ( -0.7492053821869066876, -0.6623377501714446947, 0.000000000000000000 ) ) ;
#6648 = DIRECTION ( 'NONE',  ( -0.8917477921037005872, -0.4525327339300165286, 0.000000000000000000 ) ) ;
#6649 = EDGE_CURVE ( 'NONE', #53961, #70584, #21148, .T. ) ;
#6650 = CARTESIAN_POINT ( 'NONE',  ( 175.5929596258776542, 253.6151216998191558, -3.855483475996990705 ) ) ;
#6651 = CARTESIAN_POINT ( 'NONE',  ( 198.6416989287814943, 286.5894802839873137, 18.33538993684147300 ) ) ;
#6652 = CARTESIAN_POINT ( 'NONE',  ( 48.66388509341553714, 212.2365022471903444, 2.944929066748280225E-16 ) ) ;
#6653 = CARTESIAN_POINT ( 'NONE',  ( 37.35766167792363746, 103.4248275259887748, 59.99999999999999289 ) ) ;
#6654 = CARTESIAN_POINT ( 'NONE',  ( 190.6071113721798156, 300.5057941498820924, -0.4754021072632813594 ) ) ;
#6655 = CARTESIAN_POINT ( 'NONE',  ( 21.71786549680706102, 183.3458772461660544, 9.188101187500095079 ) ) ;
#6656 = LINE ( 'NONE', #68932, #81233 ) ;
#6657 = CARTESIAN_POINT ( 'NONE',  ( 39.32338737416051089, 38.10171378149922106, 9.188101187500008038 ) ) ;
#6658 = CARTESIAN_POINT ( 'NONE',  ( 201.3991315993686158, 280.4374122447417790, -16.53561221323570862 ) ) ;
#6659 = DIRECTION ( 'NONE',  ( -0.8660254037844387076, -0.4999999999999998890, -0.000000000000000000 ) ) ;
#6660 = CARTESIAN_POINT ( 'NONE',  ( 188.9655998164360824, 267.8375115036470220, 14.10301077631414302 ) ) ;
#6661 = CARTESIAN_POINT ( 'NONE',  ( 153.7843434526567989, 265.0750476961756590, -16.54915785148878271 ) ) ;
#6662 = CARTESIAN_POINT ( 'NONE',  ( 164.0803995805677573, 281.7114191920252892, 9.860144147819550398 ) ) ;
#6663 = CONTEXT_DEPENDENT_SHAPE_REPRESENTATION ( #28549, #41011 ) ;
#6664 = CARTESIAN_POINT ( 'NONE',  ( 15.73863525846626032, 14.80170272979925272, 7.433330006724137462 ) ) ;
#6665 = CARTESIAN_POINT ( 'NONE',  ( 190.5726849661229210, 300.5654224342945326, -0.2192718484028965964 ) ) ;
#6666 = CARTESIAN_POINT ( 'NONE',  ( 71.91139111156488184, 59.09947579900738646, 15.37520130739997803 ) ) ;
#6667 = CARTESIAN_POINT ( 'NONE',  ( 154.9683083969241011, 262.2340116239618055, 18.33261662430134109 ) ) ;
#6668 = ORIENTED_EDGE ( 'NONE', *, *, #37258, .F. ) ;
#6669 = CARTESIAN_POINT ( 'NONE',  ( 184.2544554321892747, 290.3215093552799999, 12.16168713926963996 ) ) ;
#6670 = CARTESIAN_POINT ( 'NONE',  ( 85.59433769663435498, 45.42763512727970010, -9.231865596844450295 ) ) ;
#6671 = CARTESIAN_POINT ( 'NONE',  ( 0.3649266329730349034, 171.0177522451418781, -10.00000000000009592 ) ) ;
#6672 = ORIENTED_EDGE ( 'NONE', *, *, #87563, .T. ) ;
#6673 = CARTESIAN_POINT ( 'NONE',  ( 6.396987757676564357, 15.64441083166258295, -10.00000000000000533 ) ) ;
#6674 = CARTESIAN_POINT ( 'NONE',  ( 66.84604957904534217, 69.05321346016246764, 1.856603427880919366 ) ) ;
#6675 = DIRECTION ( 'NONE',  ( 0.000000000000000000, 0.000000000000000000, 1.000000000000000000 ) ) ;
#6676 = CARTESIAN_POINT ( 'NONE',  ( 203.3684377202211522, 278.4025285431072803, -16.56116267537666076 ) ) ;
#6677 = ADVANCED_FACE ( 'NONE', ( #35826 ), #58607, .T. ) ;
#6678 =( BOUNDED_CURVE ( )  B_SPLINE_CURVE ( 2, ( #78273, #2793, #8857, #17458, #78777, #55930, #72695, #9362, #16948 ),
 .UNSPECIFIED., .F., .F. ) 
 B_SPLINE_CURVE_WITH_KNOTS ( ( 3, 2, 2, 2, 3 ),
 ( 0.3185483870967741882, 0.3198924731182795633, 0.3225806451612903136, 0.3252688172043010639, 0.3266129032258064391 ),
 .UNSPECIFIED. ) 
 CURVE ( )  GEOMETRIC_REPRESENTATION_ITEM ( )  RATIONAL_B_SPLINE_CURVE ( ( 0.9330127018922194093, 0.9330127018922194093, 1.000000000000000000, 0.8660254037844387076, 1.000000000000000000, 0.8660254037844387076, 1.000000000000000000, 0.9330127018922194093, 0.9330127018922194093 ) ) 
 REPRESENTATION_ITEM ( '' )  );
#6679 = ORIENTED_EDGE ( 'NONE', *, *, #59058, .F. ) ;
#6681 = CYLINDRICAL_SURFACE ( 'NONE', #76667, 70.00000000000002842 ) ;
#6680 = CARTESIAN_POINT ( 'NONE',  ( 67.62392126478502519, 221.3967562850346837, -4.648177544792955347E-16 ) ) ;
#6682 = ORIENTED_EDGE ( 'NONE', *, *, #31600, .F. ) ;
#6683 = CARTESIAN_POINT ( 'NONE',  ( 191.4941427383744781, 298.9694107557253346, 8.584406880462095657 ) ) ;
#6684 = DIRECTION ( 'NONE',  ( -0.8660254037844387076, -0.4999999999999998890, -0.000000000000000000 ) ) ;
#6685 = CARTESIAN_POINT ( 'NONE',  ( 80.38256674825400694, 58.04436476229781761, -16.60504034864360179 ) ) ;
#6686 = CARTESIAN_POINT ( 'NONE',  ( 135.1739027599712131, 260.3967562850347122, -4.648177544792955347E-16 ) ) ;
#6688 = VERTEX_POINT ( 'NONE', #2792 ) ;
#6687 = EDGE_CURVE ( 'NONE', #26873, #85118, #74658, .T. ) ;
#6689 = CARTESIAN_POINT ( 'NONE',  ( 87.66785150117509318, 45.41448820971019984, -6.605137624362326321 ) ) ;
#6690 = EDGE_LOOP ( 'NONE', ( #89887, #38743, #67976, #1636 ) ) ;
#6691 = CARTESIAN_POINT ( 'NONE',  ( 164.4494343874829099, 245.8122196953522121, 2.922779519406129456 ) ) ;
#6692 = CARTESIAN_POINT ( 'NONE',  ( 74.72968269109679795, 64.25080327513990142, 14.13526639238711979 ) ) ;
#6693 = VERTEX_POINT ( 'NONE', #26071 ) ;
#6694 = CARTESIAN_POINT ( 'NONE',  ( 190.1190668544949460, 301.3511120508678118, 4.410340539513557090 ) ) ;
#6695 = CARTESIAN_POINT ( 'NONE',  ( 78.34563248601955365, 47.34227125466418329, -14.25321530020122118 ) ) ;
#6696 = EDGE_LOOP ( 'NONE', ( #24877, #24488, #66344, #65999 ) ) ;
#6697 = CARTESIAN_POINT ( 'NONE',  ( -16.74804229723488191, 74.64713832601701426, 13.42402697601097117 ) ) ;
#6698 =( BOUNDED_CURVE ( )  B_SPLINE_CURVE ( 2, ( #54420, #77769, #85397, #70130, #39223, #93487, #24045, #2642, #43093 ),
 .UNSPECIFIED., .F., .F. ) 
 B_SPLINE_CURVE_WITH_KNOTS ( ( 3, 2, 2, 2, 3 ),
 ( 0.1088709677419354843, 0.1102150537634408595, 0.1129032258064516098, 0.1155913978494623601, 0.1169354838709677491 ),
 .UNSPECIFIED. ) 
 CURVE ( )  GEOMETRIC_REPRESENTATION_ITEM ( )  RATIONAL_B_SPLINE_CURVE ( ( 0.9330127018922194093, 0.9330127018922194093, 1.000000000000000000, 0.8660254037844387076, 1.000000000000000000, 0.8660254037844387076, 1.000000000000000000, 0.9330127018922189652, 0.9330127018922192983 ) ) 
 REPRESENTATION_ITEM ( '' )  );
#6699 = CARTESIAN_POINT ( 'NONE',  ( 149.0247308281161622, 274.5285899518638075, 9.115861392502811356 ) ) ;
#6700 = CARTESIAN_POINT ( 'NONE',  ( -19.72006729068866804, 93.19007349502240345, 59.99999999999999289 ) ) ;
#6701 = DIRECTION ( 'NONE',  ( 0.5000000000000012212, -0.8660254037844380415, -0.000000000000000000 ) ) ;
#6702 = VERTEX_POINT ( 'NONE', #57953 ) ;
#6703 = AXIS2_PLACEMENT_3D ( 'NONE', #84323, #45273, #77174 ) ;
#6704 = ORIENTED_EDGE ( 'NONE', *, *, #76526, .F. ) ;
#6705 = CARTESIAN_POINT ( 'NONE',  ( 156.2256614230932428, 267.4609830032940181, -16.82359569179483216 ) ) ;
#6706 = CARTESIAN_POINT ( 'NONE',  ( 146.8358616138309571, 276.3198226421291679, 4.054088818585255716 ) ) ;
#6707 = CARTESIAN_POINT ( 'NONE',  ( 148.4016473149517594, 273.6078022540229426, 8.470066617688926769 ) ) ;
#6708 = CARTESIAN_POINT ( 'NONE',  ( 149.1856130393175306, 272.2499337880290682, 11.44243872309708188 ) ) ;
#6709 = CARTESIAN_POINT ( 'NONE',  ( 157.4500450658088937, 258.5180226767713521, -16.88753703094210579 ) ) ;
#6710 = CARTESIAN_POINT ( 'NONE',  ( 191.7833554288250184, 298.4684796816713970, 8.633437946248736949 ) ) ;
#6711 = CARTESIAN_POINT ( 'NONE',  ( 146.6647111637776106, 276.6162639173599587, -0.6373001129109082674 ) ) ;
#6712 = CARTESIAN_POINT ( 'NONE',  ( 148.9498507103374152, 272.6582861203333437, 11.90061892622094852 ) ) ;
#6713 = CARTESIAN_POINT ( 'NONE',  ( 71.12867290548950905, 69.85259973772616604, 7.111628047231884686 ) ) ;
#6715 = DIRECTION ( 'NONE',  ( -0.5143720371616018472, -0.8575671445351807920, 0.000000000000000000 ) ) ;
#6714 = CARTESIAN_POINT ( 'NONE',  ( 149.7109319212262051, 271.3400547943878109, -12.38605961032017433 ) ) ;
#6716 = CARTESIAN_POINT ( 'NONE',  ( 45.88188149789386472, 72.29567966924399514, -10.00000000000000000 ) ) ;
#6717 = CARTESIAN_POINT ( 'NONE',  ( 168.2645477972932326, 286.3693708646730443, 3.929190110370803790 ) ) ;
#6718 = CARTESIAN_POINT ( 'NONE',  ( 78.26124923612431417, 47.74493931943022318, 13.93016830306222964 ) ) ;
#6719 = CARTESIAN_POINT ( 'NONE',  ( 99.71410487726056715, 234.5024278399160949, 9.188101187500095079 ) ) ;
#6720 = ORIENTED_EDGE ( 'NONE', *, *, #37203, .F. ) ;
#6721 = CARTESIAN_POINT ( 'NONE',  ( 190.2890464677749662, 301.0566987244154120, -4.760511403740203207 ) ) ;
#6722 = CARTESIAN_POINT ( 'NONE',  ( 77.64951034529184426, 53.68749555020726660, -15.94746932111433857 ) ) ;
#6723 = CARTESIAN_POINT ( 'NONE',  ( 82.89880969010835088, 40.77920605493923034, 2.125336176704005542 ) ) ;
#6724 = CARTESIAN_POINT ( 'NONE',  ( 78.88804580972617941, 46.40278381930198037, 12.96229758350466810 ) ) ;
#6725 = ADVANCED_FACE ( 'NONE', ( #50351 ), #87933, .T. ) ;
#6726 = CARTESIAN_POINT ( 'NONE',  ( 180.4782130350719171, 283.6118113979034661, -16.15436706920364074 ) ) ;
#6727 = ADVANCED_FACE ( 'NONE', ( #49362 ), #72694, .F. ) ;
#6728 = CARTESIAN_POINT ( 'NONE',  ( 79.14312167556931854, 57.64441083166269664, 0.000000000000000000 ) ) ;
#6729 = CARTESIAN_POINT ( 'NONE',  ( 166.3623252550682423, 283.7353191977674101, -8.107535353489314645 ) ) ;
#6730 = ORIENTED_EDGE ( 'NONE', *, *, #65631, .T. ) ;
#6731 = CARTESIAN_POINT ( 'NONE',  ( 170.5698107352472732, 255.6068603507982289, -11.67185973913825769 ) ) ;
#6732 = CARTESIAN_POINT ( 'NONE',  ( 159.2186641046529303, 254.8721795879351646, -15.96198087403305443 ) ) ;
#6733 = EDGE_CURVE ( 'NONE', #87881, #36461, #26570, .T. ) ;
#6734 = DIRECTION ( 'NONE',  ( -0.9689225787001356505, 0.2473641778533817170, 0.000000000000000000 ) ) ;
#6735 = ADVANCED_FACE ( 'NONE', ( #4770 ), #48874, .T. ) ;
#6736 = CARTESIAN_POINT ( 'NONE',  ( 47.20246722098145398, 191.3927522451417929, -10.00000000000009059 ) ) ;
#6737 = CARTESIAN_POINT ( 'NONE',  ( 108.9156247924702114, 239.8149278399160949, -9.188101187500095079 ) ) ;
#6738 = CARTESIAN_POINT ( 'NONE',  ( 174.3575034883137391, 273.0034624690363216, 17.77573060583294762 ) ) ;
#6739 = LINE ( 'NONE', #52819, #73963 ) ;
#6740 = FACE_OUTER_BOUND ( 'NONE', #57022, .T. ) ;
#6741 = CARTESIAN_POINT ( 'NONE',  ( 175.3489461370708398, 253.4744944187259819, -3.884895130763601490 ) ) ;
#6742 = CARTESIAN_POINT ( 'NONE',  ( 41.71789998727770410, 185.7048013555409796, 4.594050593750051981 ) ) ;
#6743 = CARTESIAN_POINT ( 'NONE',  ( 78.99848661620950452, 60.24637179098724005, -16.44349368446546222 ) ) ;
#6744 = ORIENTED_EDGE ( 'NONE', *, *, #457, .T. ) ;
#6745 = CARTESIAN_POINT ( 'NONE',  ( 72.62975712138512563, 68.37227089251233281, 10.30573641387579364 ) ) ;
#6746 = PLANE ( 'NONE',  #33489 ) ;
#6747 = B_SPLINE_SURFACE_WITH_KNOTS ( 'NONE', 3, 1, ( 
 ( #35362, #89621 ),
 ( #35861, #66759 ),
 ( #11589, #67257 ),
 ( #98183, #90104 ),
 ( #83002, #27772 ),
 ( #97690, #74885 ),
 ( #28258, #41967 ),
 ( #66272, #82524 ),
 ( #59646, #58646 ),
 ( #34852, #20183 ),
 ( #42448, #34370 ),
 ( #65756, #5469 ),
 ( #3494, #73383 ),
 ( #19692, #88634 ),
 ( #65267, #3969 ),
 ( #96211, #51050 ),
 ( #28764, #59133 ),
 ( #27278, #20675 ),
 ( #96710, #58160 ),
 ( #42936, #81508 ),
 ( #90617, #12078 ),
 ( #82009, #19200 ),
 ( #51564, #12583 ),
 ( #26774, #73875 ),
 ( #43456, #57655 ),
 ( #14569, #69246 ),
 ( #31240, #15530 ),
 ( #91588, #92590 ),
 ( #60633, #29760 ),
 ( #22159, #23134 ),
 ( #100174, #29270 ) ),
 .UNSPECIFIED., .F., .F., .F.,
 ( 4, 3, 3, 3, 3, 3, 3, 3, 3, 3, 4 ),
 ( 2, 2 ),
 ( 0.000000000000000000, 0.1333490885032394824, 0.3007194338854430882, 0.4699862290245251373, 0.5844252810809388299, 0.6686540514502711252, 0.7354980260655488156, 0.8028463152565757932, 0.8633854507757249275, 0.9437142632667384623, 1.000000000000000000 ),
 ( 0.000000000000000000, 1.000000000000000000 ),
 .UNSPECIFIED. ) ;
#6748 = LINE ( 'NONE', #38113, #80524 ) ;
#6749 = CARTESIAN_POINT ( 'NONE',  ( 190.1696443193688708, 301.2635093119881162, -4.804312979389741223 ) ) ;
#6750 = FACE_OUTER_BOUND ( 'NONE', #53772, .T. ) ;
#6751 = DIRECTION ( 'NONE',  ( -0.000000000000000000, 0.000000000000000000, -1.000000000000000000 ) ) ;
#6752 = CARTESIAN_POINT ( 'NONE',  ( 88.49573251350186354, 44.44521367694441949, 1.972556413651489717E-15 ) ) ;
#6753 = CARTESIAN_POINT ( 'NONE',  ( 105.5870131927823508, 231.7677522451418497, 10.00000000000009592 ) ) ;
#6754 = ORIENTED_EDGE ( 'NONE', *, *, #48077, .T. ) ;
#6755 = FACE_OUTER_BOUND ( 'NONE', #56232, .T. ) ;
#6756 = CARTESIAN_POINT ( 'NONE',  ( 155.4495112628364097, 279.7055087804715754, -1.752144325060382535 ) ) ;
#6757 = CARTESIAN_POINT ( 'NONE',  ( 162.9383752892161397, 248.4294508267893491, -11.25953730674605957 ) ) ;
#6758 = CARTESIAN_POINT ( 'NONE',  ( 22.80074434730262567, 171.7202760586659736, -5.415160957724236172E-17 ) ) ;
#6759 = CARTESIAN_POINT ( 'NONE',  ( 13.67456932412660997, 8.864269794150878568, -3.090169943749474069 ) ) ;
#6760 = CARTESIAN_POINT ( 'NONE',  ( 196.1615410976813507, 273.7113085403182140, 14.86458732197895216 ) ) ;
#6761 = CARTESIAN_POINT ( 'NONE',  ( -2.073866539663252073, 26.60322154129611505, -10.00000000000000000 ) ) ;
#6762 = CARTESIAN_POINT ( 'NONE',  ( 73.15133419349439237, 69.74273237385936852, 9.116647530793477117 ) ) ;
#6764 = CARTESIAN_POINT ( 'NONE',  ( 73.65258675182887771, 204.1423013555409796, -4.594050593750043987 ) ) ;
#6763 = CARTESIAN_POINT ( 'NONE',  ( 174.7229882116660065, 286.3465783895868526, 10.42342695070571601 ) ) ;
#6765 = CARTESIAN_POINT ( 'NONE',  ( 164.1821508476733698, 246.2751683663292397, -7.347745041495428175 ) ) ;
#6766 = CARTESIAN_POINT ( 'NONE',  ( 72.94198659864277090, 57.16943012042473526, 15.90410001130455164 ) ) ;
#6767 = CARTESIAN_POINT ( 'NONE',  ( 70.18403142648233484, 67.22621705619883414, 10.62750587675546576 ) ) ;
#6768 = CARTESIAN_POINT ( 'NONE',  ( 66.45987627312771906, 68.25526039504281073, -4.355395359899360663 ) ) ;
#6769 = ORIENTED_EDGE ( 'NONE', *, *, #34632, .F. ) ;
#6770 = AXIS2_PLACEMENT_3D ( 'NONE', #94788, #87233, #39523 ) ;
#6771 = CARTESIAN_POINT ( 'NONE',  ( 12.29081813446918758, 171.2365022471902023, -10.00000000000009059 ) ) ;
#6772 = CARTESIAN_POINT ( 'NONE',  ( 208.3135187673106543, 269.8373969220020285, 2.829653198597726682 ) ) ;
#6773 = CARTESIAN_POINT ( 'NONE',  ( 135.0589402170954827, 248.7833772461660544, -9.188101187500095079 ) ) ;
#6774 = CARTESIAN_POINT ( 'NONE',  ( 20.59861825492957621, 33.93396525600390845, 2.839279412974139660 ) ) ;
#6775 = CARTESIAN_POINT ( 'NONE',  ( 207.5551753531803172, 271.1508862448613399, -7.290975649195053698 ) ) ;
#6776 = CARTESIAN_POINT ( 'NONE',  ( 83.74768966023471251, 52.21580090503303495, -15.05827679895701898 ) ) ;
#6777 = DIRECTION ( 'NONE',  ( -0.6793907169778456989, 0.000000000000000000, 0.7337767056021393675 ) ) ;
#6779 = CARTESIAN_POINT ( 'NONE',  ( -17.26243516413818924, 24.35187462261283997, -10.00000000000000000 ) ) ;
#6778 = CARTESIAN_POINT ( 'NONE',  ( 69.23475887354902625, 68.83203394105711936, 7.846736462262181355 ) ) ;
#6780 = CARTESIAN_POINT ( 'NONE',  ( 68.72575050907364869, 64.26090759019037080, 12.49566804605334447 ) ) ;
#6781 = ORIENTED_EDGE ( 'NONE', *, *, #59421, .F. ) ;
#6782 = CARTESIAN_POINT ( 'NONE',  ( 64.01779381112933720, 197.7677522451418213, -5.000000000000041744 ) ) ;
#6783 = EDGE_CURVE ( 'NONE', #22179, #73260, #9411, .T. ) ;
#6784 = CARTESIAN_POINT ( 'NONE',  ( 71.98645284171395531, 66.88534893327906161, -11.90698704647148531 ) ) ;
#6785 = CARTESIAN_POINT ( 'NONE',  ( 196.6039295022987972, 289.7324168733214833, 16.35530466314298437 ) ) ;
#6786 = CARTESIAN_POINT ( 'NONE',  ( 196.9474029239601975, 272.9819407449171536, -13.37321390883489691 ) ) ;
#6787 = ORIENTED_EDGE ( 'NONE', *, *, #11107, .T. ) ;
#6788 = CARTESIAN_POINT ( 'NONE',  ( 206.5002523963886176, 272.9780664040949318, 9.017141309861059995 ) ) ;
#6789 = CARTESIAN_POINT ( 'NONE',  ( -78.94662368502558536, 55.85910816071121587, -10.00000000000000000 ) ) ;
#6790 = CARTESIAN_POINT ( 'NONE',  ( 71.80217098314240332, 72.17902961906311532, 0.5796836128640239227 ) ) ;
#6791 = CARTESIAN_POINT ( 'NONE',  ( 148.8112445470583225, 273.2837754581220793, -9.153596929589264519 ) ) ;
#6792 = CARTESIAN_POINT ( 'NONE',  ( 196.3844087422174596, 270.6169231452851704, 13.31990624255254474 ) ) ;
#6793 = CARTESIAN_POINT ( 'NONE',  ( -38.61298035630893111, 26.97617139035147460, 10.00000000000000000 ) ) ;
#6794 = CARTESIAN_POINT ( 'NONE',  ( 208.1912724900461740, 270.0491336852600170, -0.9856800448607289100 ) ) ;
#6795 = CARTESIAN_POINT ( 'NONE',  ( 200.9812045408918380, 282.5373376992193926, -16.61165062382494284 ) ) ;
#6796 = VERTEX_POINT ( 'NONE', #58443 ) ;
#6797 = CARTESIAN_POINT ( 'NONE',  ( 190.6828093349753317, 281.2089909899326585, 16.73330534773390710 ) ) ;
#6798 = CARTESIAN_POINT ( 'NONE',  ( 17.30334773395576775, 15.15404122711132651, 8.090169943749479842 ) ) ;
#6799 = CARTESIAN_POINT ( 'NONE',  ( -19.65312891409030271, 93.06504152958497400, 177.5919119679930134 ) ) ;
#6800 = ORIENTED_EDGE ( 'NONE', *, *, #72412, .F. ) ;
#6801 = CARTESIAN_POINT ( 'NONE',  ( -69.85371643402891095, 44.28081239092799848, 10.00000000000000000 ) ) ;
#6802 = DIRECTION ( 'NONE',  ( 0.000000000000000000, 1.000000000000000000, 0.000000000000000000 ) ) ;
#6803 = CARTESIAN_POINT ( 'NONE',  ( 86.11128617339311120, 45.02157760453157920, -7.471804814321710175 ) ) ;
#6804 = VERTEX_POINT ( 'NONE', #49856 ) ;
#6805 = CARTESIAN_POINT ( 'NONE',  ( 191.3041230083617563, 299.2985345825480863, -9.819045872446528378 ) ) ;
#6806 = PLANE ( 'NONE',  #89668 ) ;
#6807 = CARTESIAN_POINT ( 'NONE',  ( 164.4294002498235159, 245.8469198396639399, 6.098783631055905374 ) ) ;
#6809 = AXIS2_PLACEMENT_3D ( 'NONE', #78960, #63728, #94664 ) ;
#6808 = CARTESIAN_POINT ( 'NONE',  ( 69.40462582020063564, 62.82854907067461880, 13.14331805213147319 ) ) ;
#6810 = VERTEX_POINT ( 'NONE', #43237 ) ;
#6811 = CARTESIAN_POINT ( 'NONE',  ( 106.3178956768819319, 226.0643266524159856, -9.188101187500093303 ) ) ;
#6812 = CARTESIAN_POINT ( 'NONE',  ( -13.11024591527723615, 6.000000000000000000, -32.50000000000017053 ) ) ;
#6813 = CARTESIAN_POINT ( 'NONE',  ( 180.5397319334442159, 270.7127871342991625, -15.99547242021038329 ) ) ;
#6814 = CARTESIAN_POINT ( 'NONE',  ( 81.58540180393886487, 42.27212079091695784, -8.035051867169045181 ) ) ;
#6815 = ORIENTED_EDGE ( 'NONE', *, *, #62143, .F. ) ;
#6816 = VERTEX_POINT ( 'NONE', #4251 ) ;
#6817 = ORIENTED_EDGE ( 'NONE', *, *, #8245, .T. ) ;
#6818 = CARTESIAN_POINT ( 'NONE',  ( 157.4991920912938497, 281.1666361535517353, -5.886997319559604591 ) ) ;
#6819 = ORIENTED_EDGE ( 'NONE', *, *, #99531, .T. ) ;
#6820 = CARTESIAN_POINT ( 'NONE',  ( 159.5903462228227738, 257.4064654884239758, -17.16338673343565446 ) ) ;
#6821 = EDGE_LOOP ( 'NONE', ( #4200, #1217, #85881, #89360 ) ) ;
#6822 = CARTESIAN_POINT ( 'NONE',  ( 163.8111161534324935, 246.9178193081252743, -7.110480325054721717 ) ) ;
#6823 = CYLINDRICAL_SURFACE ( 'NONE', #12371, 17.82106496071139645 ) ;
#6824 = CYLINDRICAL_SURFACE ( 'NONE', #3251, 70.00000000000002842 ) ;
#6825 = CARTESIAN_POINT ( 'NONE',  ( 82.86632025040690053, 53.49705537725820648, -15.32442982359594730 ) ) ;
#6826 = EDGE_LOOP ( 'NONE', ( #36094, #31480, #84349, #19910 ) ) ;
#6827 = CARTESIAN_POINT ( 'NONE',  ( 66.46320885748656337, 68.94986384069261476, 0.01364106734875079018 ) ) ;
#6828 = CARTESIAN_POINT ( 'NONE',  ( 20.84336723938811176, 14.96004757982089828, -5.678558825948276656 ) ) ;
#6829 = CARTESIAN_POINT ( 'NONE',  ( 198.7242481644049121, 277.5995992023655958, -15.36478769293520941 ) ) ;
#6830 = CARTESIAN_POINT ( 'NONE',  ( 80.65095556854913639, 57.57228308630150337, 16.58706730796346918 ) ) ;
#6832 = ORIENTED_EDGE ( 'NONE', *, *, #55561, .T. ) ;
#6831 = DIRECTION ( 'NONE',  ( 0.000000000000000000, 0.000000000000000000, 1.000000000000000000 ) ) ;
#6833 = CARTESIAN_POINT ( 'NONE',  ( 162.9796882977680639, 248.3578945969637743, 9.683801903336119565 ) ) ;
#6834 = CARTESIAN_POINT ( 'NONE',  ( 185.0543536129055155, 258.0163728256403033, 3.008362416367333925 ) ) ;
#6835 = CARTESIAN_POINT ( 'NONE',  ( 74.56414817410228579, 187.8759306620403322, -18.47570218321542868 ) ) ;
#6836 = DIRECTION ( 'NONE',  ( -0.5000000000000006661, 0.8660254037844382635, -1.877843081442121204E-16 ) ) ;
#6837 = CARTESIAN_POINT ( 'NONE',  ( 171.8532966785767258, 254.8378052108570273, 11.04733308641842804 ) ) ;
#6838 = EDGE_CURVE ( 'NONE', #21034, #5053, #41243, .T. ) ;
#6839 = CARTESIAN_POINT ( 'NONE',  ( 157.7886504734048003, 281.3435236914132815, 1.490504832958681636 ) ) ;
#6840 = ORIENTED_EDGE ( 'NONE', *, *, #99780, .F. ) ;
#6841 = CARTESIAN_POINT ( 'NONE',  ( 97.95516432547988472, 227.3615022471902591, -10.00000000000009592 ) ) ;
#6842 = CARTESIAN_POINT ( 'NONE',  ( 70.11758659987526698, 63.57919021067856846, -12.94399158718550069 ) ) ;
#6843 = DIRECTION ( 'NONE',  ( -0.1032265479692960342, 0.9946578707245736783, 0.000000000000000000 ) ) ;
#6844 = EDGE_CURVE ( 'NONE', #73983, #2236, #33669, .T. ) ;
#6845 = CARTESIAN_POINT ( 'NONE',  ( 4.262040950003053830, 163.2677522451418213, -5.000000000000041744 ) ) ;
#6846 = CARTESIAN_POINT ( 'NONE',  ( 195.7350119871117329, 269.2567921979494372, -10.80356350091597761 ) ) ;
#6847 = CARTESIAN_POINT ( 'NONE',  ( 175.0457569121529389, 281.4923175861599134, -14.14130193385072154 ) ) ;
#6848 = CARTESIAN_POINT ( 'NONE',  ( 203.4748520814800088, 278.2182134627518053, -14.85237232639370575 ) ) ;
#6849 = CARTESIAN_POINT ( 'NONE',  ( 87.93887446415499198, 44.76116579897428238, -4.704258403839747693 ) ) ;
#6850 = CARTESIAN_POINT ( 'NONE',  ( 72.98735915780690675, 70.85324004147126686, 8.065790162528026386 ) ) ;
#6852 = CARTESIAN_POINT ( 'NONE',  ( 32.90709467669683619, 21.12755873383627758, -6.180339887498949025 ) ) ;
#6851 = CARTESIAN_POINT ( 'NONE',  ( -11.27255005043015856, 173.4869531367911293, 4.594050593750046652 ) ) ;
#6853 = CARTESIAN_POINT ( 'NONE',  ( 186.3020778951789111, 295.5636472136135922, 8.187152758880353431 ) ) ;
#6854 = VERTEX_POINT ( 'NONE', #50845 ) ;
#6855 = ORIENTED_EDGE ( 'NONE', *, *, #45141, .F. ) ;
#6856 = CARTESIAN_POINT ( 'NONE',  ( -30.95603806669010538, 23.98360954755322183, -10.00000000000000000 ) ) ;
#6857 = CARTESIAN_POINT ( 'NONE',  ( -75.18208942163934694, 50.44421862632483311, -10.00000000000000000 ) ) ;
#6858 = CARTESIAN_POINT ( 'NONE',  ( 86.76444126019433156, 45.86660341771495553, -8.261827951889216592 ) ) ;
#6859 = CYLINDRICAL_SURFACE ( 'NONE', #77663, 17.82106496071139645 ) ;
#6860 = CARTESIAN_POINT ( 'NONE',  ( 202.1549692867851888, 280.5043175231993473, -17.32512590000773045 ) ) ;
#6861 = CARTESIAN_POINT ( 'NONE',  ( 83.81086367703072426, 45.25070890705758586, 9.560661162256756995 ) ) ;
#6862 = CARTESIAN_POINT ( 'NONE',  ( 149.9300743764016488, 276.9001158938398817, 3.155267742367139139 ) ) ;
#6863 = CARTESIAN_POINT ( 'NONE',  ( 25.77753312492912841, 179.5643266524160140, -9.188101187500093303 ) ) ;
#6864 = CARTESIAN_POINT ( 'NONE',  ( 110.8370318831756975, 243.9869531367911009, 4.594050593750046652 ) ) ;
#6865 = DIRECTION ( 'NONE',  ( -2.168404344971021440E-16, 3.755786496842916807E-16, 1.000000000000000000 ) ) ;
#6866 = CARTESIAN_POINT ( 'NONE',  ( 65.88310562893973099, 69.02589174555536999, 1.996831191813060347 ) ) ;
#6867 = CARTESIAN_POINT ( 'NONE',  ( 78.58136487301973716, 53.95277478616699796, 15.90687120791058007 ) ) ;
#6868 = DIRECTION ( 'NONE',  ( -0.8660254037844387076, -0.4999999999999998890, -0.000000000000000000 ) ) ;
#6869 = VECTOR ( 'NONE', #99259, 1000.000000000000227 ) ;
#6870 = CARTESIAN_POINT ( 'NONE',  ( 62.64658692180388755, 213.6427522451419065, -10.00000000000009592 ) ) ;
#6871 = CARTESIAN_POINT ( 'NONE',  ( 195.6974783896144174, 291.6890198465123945, 16.70600479393688431 ) ) ;
#6872 = CARTESIAN_POINT ( 'NONE',  ( 74.06414817410220053, 188.7419560658248656, 18.47570218321542868 ) ) ;
#6873 = CARTESIAN_POINT ( 'NONE',  ( 184.3718295276511583, 274.4586611926505952, 17.53799969959756311 ) ) ;
#6874 = CARTESIAN_POINT ( 'NONE',  ( -19.65312891409030271, 93.06504152958497400, 177.5919119679930134 ) ) ;
#6875 = VECTOR ( 'NONE', #30591, 1000.000000000000000 ) ;
#6876 = CARTESIAN_POINT ( 'NONE',  ( 171.1613143928009606, 279.7166738654231040, 13.89588308401470051 ) ) ;
#6877 = CARTESIAN_POINT ( 'NONE',  ( 186.9944938751388861, 298.8788464850996434, -0.5967753998689386830 ) ) ;
#6878 = CARTESIAN_POINT ( 'NONE',  ( 68.85610678100678683, 68.65685376360768544, 6.741963133850092049 ) ) ;
#6879 = CARTESIAN_POINT ( 'NONE',  ( 67.00187114335926708, 67.08813303282481399, 8.529924657355552498 ) ) ;
#6880 = CARTESIAN_POINT ( 'NONE',  ( 79.42866338260434134, 59.50128377535573776, 16.18467811310512872 ) ) ;
#6881 = ORIENTED_EDGE ( 'NONE', *, *, #68874, .F. ) ;
#6882 = LINE ( 'NONE', #83429, #44861 ) ;
#6883 = B_SPLINE_CURVE_WITH_KNOTS ( 'NONE', 3,
 ( #42848, #35273, #43858, #98086, #88046, #96623, #66179, #88540, #74799, #41875, #74310, #3404, #97123, #58562, #12493, #34278, #80938, #43360, #96125, #19103, #4891, #27188, #35772, #26679 ),
 .UNSPECIFIED., .F., .F.,
 ( 4, 2, 2, 2, 2, 2, 2, 2, 2, 2, 2, 4 ),
 ( 0.000000000000000000, 0.1249999999999770461, 0.2499999999999540923, 0.3749999999999311662, 0.4374999999999368283, 0.4999999999999424904, 0.5624999999999481526, 0.6249999999999537037, 0.6874999999999593658, 0.7499999999999649170, 0.8749999999999825695, 1.000000000000000000 ),
 .UNSPECIFIED. ) ;
#6884 = CARTESIAN_POINT ( 'NONE',  ( 184.2750561946413654, 269.3830903805491630, 15.28138810499674349 ) ) ;
#6885 = CARTESIAN_POINT ( 'NONE',  ( 94.03063961704269502, 237.3464784336661637, 1.353441290958777327E-15 ) ) ;
#6886 = CARTESIAN_POINT ( 'NONE',  ( 7.993722094130166766, 16.56628583063838533, 9.188101187500006262 ) ) ;
#6887 = CARTESIAN_POINT ( 'NONE',  ( 80.20857538925844210, 44.21345027839176112, -11.30608575764589752 ) ) ;
#6888 = DIRECTION ( 'NONE',  ( 0.5000000000000013323, -0.8660254037844378194, 0.000000000000000000 ) ) ;
#6890 = CARTESIAN_POINT ( 'NONE',  ( 85.58122159723554034, 42.79555190012898436, -1.803223411638267493 ) ) ;
#6889 = CARTESIAN_POINT ( 'NONE',  ( 196.0034224882197975, 291.1591091234520263, 17.53794140922627776 ) ) ;
#6891 = CARTESIAN_POINT ( 'NONE',  ( 149.5742366896305668, 271.5768178806638957, 12.98651753098913098 ) ) ;
#6892 = CARTESIAN_POINT ( 'NONE',  ( 150.9584389135710865, 269.1793093008492406, -15.82751450793727699 ) ) ;
#6893 = CARTESIAN_POINT ( 'NONE',  ( 149.8928472635447804, 271.6201905152058771, -11.69094866835029656 ) ) ;
#6894 = ADVANCED_FACE ( 'NONE', ( #12880 ), #5745, .T. ) ;
#6895 = CARTESIAN_POINT ( 'NONE',  ( 44.05945362601616466, 27.29860640527295956, -2.839279412974138328 ) ) ;
#6896 = CARTESIAN_POINT ( 'NONE',  ( 123.2041546383393751, 253.4860189848785126, -2.679491924311252493 ) ) ;
#6897 = FACE_BOUND ( 'NONE', #58603, .T. ) ;
#6898 = ORIENTED_EDGE ( 'NONE', *, *, #46398, .F. ) ;
#6899 = CARTESIAN_POINT ( 'NONE',  ( 31.56043161122053320, 21.14754757982091249, -5.678558825948276656 ) ) ;
#6900 = CARTESIAN_POINT ( 'NONE',  ( 73.85177649559180679, 63.65451359222425509, -14.63794785187609371 ) ) ;
#6901 = CARTESIAN_POINT ( 'NONE',  ( 193.1977289678065404, 296.0187128512746995, -12.37159405312863925 ) ) ;
#6902 = CARTESIAN_POINT ( 'NONE',  ( 149.7200635338602410, 271.3242383773507527, -12.12223662813266500 ) ) ;
#6903 = VERTEX_POINT ( 'NONE', #67541 ) ;
#6904 = CARTESIAN_POINT ( 'NONE',  ( 70.88562338225854376, 61.01594546643109851, 15.03711900572700877 ) ) ;
#6905 = CARTESIAN_POINT ( 'NONE',  ( 75.97482311634344398, 65.22733265193998875, -14.46914695647701343 ) ) ;
#6907 = EDGE_CURVE ( 'NONE', #63624, #98201, #37138, .T. ) ;
#6906 = CARTESIAN_POINT ( 'NONE',  ( 182.0647779265614190, 264.0180564602412119, -12.95455995337640864 ) ) ;
#6908 = CARTESIAN_POINT ( 'NONE',  ( 173.1578642404289496, 253.8352349280846738, -9.039979433292165467 ) ) ;
#6909 = CARTESIAN_POINT ( 'NONE',  ( 192.0963028965829551, 297.9264387674147656, 11.34530024772836754 ) ) ;
#6910 = ORIENTED_EDGE ( 'NONE', *, *, #53077, .F. ) ;
#6911 = CARTESIAN_POINT ( 'NONE',  ( 187.3516457461684297, 278.8611292493811789, 17.07296404786917066 ) ) ;
#6912 = CARTESIAN_POINT ( 'NONE',  ( 30.25658917092484756, 35.65586893147758474, -7.433330006724137462 ) ) ;
#6913 = EDGE_LOOP ( 'NONE', ( #95348, #93355, #43011, #21885 ) ) ;
#6914 = CARTESIAN_POINT ( 'NONE',  ( 167.7292734088323130, 249.7294130688958376, 6.677680936074735563 ) ) ;
#6915 = EDGE_CURVE ( 'NONE', #88465, #45893, #41290, .T. ) ;
#6916 = CARTESIAN_POINT ( 'NONE',  ( 185.2856931816752990, 292.6844727045286731, -10.59087788492901971 ) ) ;
#6917 = ORIENTED_EDGE ( 'NONE', *, *, #45891, .T. ) ;
#6918 = CARTESIAN_POINT ( 'NONE',  ( 166.1321135059490359, 260.4694391397057416, 16.98093069965871038 ) ) ;
#6919 = DIRECTION ( 'NONE',  ( -0.8951289669282589401, 0.4458072818673421422, 0.000000000000000000 ) ) ;
#6920 = CARTESIAN_POINT ( 'NONE',  ( 191.0757748809261045, 279.1147246841564993, -16.54284077524308927 ) ) ;
#6921 = CARTESIAN_POINT ( 'NONE',  ( 192.6674894974040058, 296.9371145541902592, -12.11795536761400882 ) ) ;
#6922 = CARTESIAN_POINT ( 'NONE',  ( 153.2513309553138470, 265.2079037882803618, -16.24091495603130397 ) ) ;
#6923 = CARTESIAN_POINT ( 'NONE',  ( 36.96107555259132482, 29.84335787977765619, 9.188101187500006262 ) ) ;
#6924 = CARTESIAN_POINT ( 'NONE',  ( 80.32771389996757705, 57.94408260071153194, -16.24746918486169633 ) ) ;
#6925 = FACE_OUTER_BOUND ( 'NONE', #70462, .T. ) ;
#6926 = ORIENTED_EDGE ( 'NONE', *, *, #12641, .T. ) ;
#6927 = CARTESIAN_POINT ( 'NONE',  ( 198.8683739244561082, 276.4215138120039796, -15.93986209720707414 ) ) ;
#6928 = ORIENTED_EDGE ( 'NONE', *, *, #28905, .F. ) ;
#6929 = ORIENTED_EDGE ( 'NONE', *, *, #34268, .F. ) ;
#6930 = CARTESIAN_POINT ( 'NONE',  ( 205.0520875136525376, 275.4863615587311756, -14.16385635411862509 ) ) ;
#6931 = CARTESIAN_POINT ( 'NONE',  ( 169.4094010280188911, 269.1046630455843456, 17.13746518211817360 ) ) ;
#6932 = CARTESIAN_POINT ( 'NONE',  ( 79.76444659671797410, 57.08246710002341473, 16.23159459986195330 ) ) ;
#6934 = DIRECTION ( 'NONE',  ( -0.6857383512134002101, -0.7278481391575631898, 0.000000000000000000 ) ) ;
#6933 = CARTESIAN_POINT ( 'NONE',  ( 174.0704149835363808, 256.6406572203894711, -12.38982705157956410 ) ) ;
#6935 = DIRECTION ( 'NONE',  ( -0.9795703749556662343, 0.2011016670970565412, 0.000000000000000000 ) ) ;
#6936 = CARTESIAN_POINT ( 'NONE',  ( 70.44156110210124666, 71.15467463549107663, 4.264815030697374887 ) ) ;
#6937 = CARTESIAN_POINT ( 'NONE',  ( 76.73198439572453822, 60.14737954539558018, -15.86720150413332675 ) ) ;
#6938 = CARTESIAN_POINT ( 'NONE',  ( 190.1730848958311810, 301.2575500587478814, 0.2415986433272204748 ) ) ;
#6939 = CARTESIAN_POINT ( 'NONE',  ( 170.4449418037447970, 288.8185950528904300, -4.219811512460142744 ) ) ;
#6940 = CARTESIAN_POINT ( 'NONE',  ( 77.07812270435945834, 63.66946605146480209, -15.38604565157081794 ) ) ;
#6941 = CARTESIAN_POINT ( 'NONE',  ( 178.6026051973306323, 254.4708812555809345, 5.813106864979912913 ) ) ;
#6942 = CARTESIAN_POINT ( 'NONE',  ( 117.0621101165238542, 229.2048013555409796, 4.594050593750051981 ) ) ;
#6943 = ORIENTED_EDGE ( 'NONE', *, *, #58563, .F. ) ;
#6944 = LINE ( 'NONE', #61134, #41479 ) ;
#6945 = CARTESIAN_POINT ( 'NONE',  ( 43.97106342183892735, 31.10170272979931028, -7.433330006724141015 ) ) ;
#6946 = CARTESIAN_POINT ( 'NONE',  ( 191.8258794905848674, 275.2947431816082258, 16.27196167175203811 ) ) ;
#6947 = ORIENTED_EDGE ( 'NONE', *, *, #75984, .T. ) ;
#6948 = VECTOR ( 'NONE', #7990, 1000.000000000000000 ) ;
#6949 = ORIENTED_EDGE ( 'NONE', *, *, #21767, .T. ) ;
#6950 = ADVANCED_FACE ( 'NONE', ( #6750 ), #24286, .T. ) ;
#6951 = CARTESIAN_POINT ( 'NONE',  ( 73.84430631328980610, 68.30184443197676103, -11.60545323109705507 ) ) ;
#6952 = EDGE_CURVE ( 'NONE', #60043, #79260, #9243, .T. ) ;
#6953 = CIRCLE ( 'NONE', #60370, 70.00000000000001421 ) ;
#6954 = CARTESIAN_POINT ( 'NONE',  ( 180.7266824466902904, 294.1535421663213015, -2.386762920861517312 ) ) ;
#6955 = FACE_OUTER_BOUND ( 'NONE', #85981, .T. ) ;
#6956 = CARTESIAN_POINT ( 'NONE',  ( 190.3528479301325262, 300.4287509476951641, -0.1680789796435935290 ) ) ;
#6957 = CARTESIAN_POINT ( 'NONE',  ( 13.93250452138409479, 29.81751292744056059, -6.180339887498951690 ) ) ;
#6958 = ORIENTED_EDGE ( 'NONE', *, *, #24976, .T. ) ;
#6959 = CARTESIAN_POINT ( 'NONE',  ( 147.9323189423145664, 274.4207028408641804, 9.430423372208688093 ) ) ;
#6960 = ORIENTED_EDGE ( 'NONE', *, *, #89379, .T. ) ;
#6961 = B_SPLINE_CURVE_WITH_KNOTS ( 'NONE', 3,
 ( #202, #83344, #76702, #13910 ),
 .UNSPECIFIED., .F., .F.,
 ( 4, 4 ),
 ( 0.009355697899887138388, 0.01532099559381962239 ),
 .UNSPECIFIED. ) ;
#6962 = PLANE ( 'NONE',  #26949 ) ;
#6963 = EDGE_LOOP ( 'NONE', ( #62124, #48302, #96931, #83288 ) ) ;
#6964 = CARTESIAN_POINT ( 'NONE',  ( 191.8890130564416552, 267.7039900243542547, -12.47167058615804258 ) ) ;
#6965 = EDGE_CURVE ( 'NONE', #39921, #50534, #32024, .T. ) ;
#6966 = AXIS2_PLACEMENT_3D ( 'NONE', #61474, #53859, #96287 ) ;
#6967 = EDGE_CURVE ( 'NONE', #56880, #78230, #38628, .T. ) ;
#6968 = CARTESIAN_POINT ( 'NONE',  ( 192.4683202118899885, 263.0335775797599922, 4.534414443811968454 ) ) ;
#6969 = CARTESIAN_POINT ( 'NONE',  ( 204.6209114679778338, 273.0706743954793296, -9.999413212032170151 ) ) ;
#6971 = CARTESIAN_POINT ( 'NONE',  ( 159.8157848413643762, 281.0678040903168267, 5.628117109850034439 ) ) ;
#6970 = CARTESIAN_POINT ( 'NONE',  ( 184.2825131821604430, 288.8156619643899035, -13.20009111789595480 ) ) ;
#6972 = CARTESIAN_POINT ( 'NONE',  ( 153.3544108199959908, 265.0293642254135307, -17.49105661178601423 ) ) ;
#6973 = VERTEX_POINT ( 'NONE', #40118 ) ;
#6974 = CARTESIAN_POINT ( 'NONE',  ( 146.9709166616330549, 276.0859004375172390, 3.755270622130282732 ) ) ;
#6976 = CARTESIAN_POINT ( 'NONE',  ( 73.30406195733340269, 68.46761453276084808, 10.59438808196635762 ) ) ;
#6975 = B_SPLINE_SURFACE_WITH_KNOTS ( 'NONE', 3, 1, ( 
 ( #85711, #31433 ),
 ( #79089, #63347 ),
 ( #9672, #94285 ),
 ( #70445, #93280 ),
 ( #16746, #40533 ),
 ( #47634, #2058 ),
 ( #71467, #16246 ),
 ( #78567, #3566 ),
 ( #34446, #18262 ),
 ( #96793, #65345 ),
 ( #42526, #34933 ),
 ( #27353, #20255 ),
 ( #10659, #43016 ),
 ( #57234, #96284 ),
 ( #26853, #97276 ),
 ( #50631, #82092 ),
 ( #80595, #97762 ),
 ( #57728, #5052 ),
 ( #95804, #64857 ),
 ( #51130, #58235 ),
 ( #66834, #72975 ),
 ( #49157, #88708 ),
 ( #4043, #80092 ),
 ( #4540, #65828 ),
 ( #73955, #33973 ),
 ( #35932, #27843 ),
 ( #19763, #35440 ),
 ( #41535, #89215 ),
 ( #12665, #72479 ),
 ( #81098, #66343 ),
 ( #58720, #81585 ) ),
 .UNSPECIFIED., .F., .F., .F.,
 ( 4, 3, 3, 3, 3, 3, 3, 3, 3, 3, 4 ),
 ( 2, 2 ),
 ( 0.000000000000000000, 0.1122669598086814963, 0.2243161639709700950, 0.3396355846219198393, 0.4553962076585126861, 0.5677860799922443968, 0.6749047109689583213, 0.7773884377078411623, 0.8775581155834147884, 0.9782364162377933381, 1.000000000000000000 ),
 ( 0.000000000000000000, 1.000000000000000000 ),
 .UNSPECIFIED. ) ;
#6977 = LINE ( 'NONE', #14086, #67802 ) ;
#6978 = CARTESIAN_POINT ( 'NONE',  ( 192.4470566622854903, 271.7249251123275826, 14.07432190622019874 ) ) ;
#6979 = CARTESIAN_POINT ( 'NONE',  ( 192.5309820353861312, 271.7291774915358360, -14.57346003379339727 ) ) ;
#6980 = CARTESIAN_POINT ( 'NONE',  ( 71.68255973785201718, 72.12657461437540007, 3.318624374305790603 ) ) ;
#6981 = CARTESIAN_POINT ( 'NONE',  ( 83.76059554491119741, 44.12875889070350155, 8.054854059989002835 ) ) ;
#6982 = CARTESIAN_POINT ( 'NONE',  ( 67.06923665261433598, 197.9824982072973683, 3.021315404115420679E-15 ) ) ;
#6983 = CARTESIAN_POINT ( 'NONE',  ( 82.72605847261863232, 53.97080330652735825, -15.84526420522619539 ) ) ;
#6984 = CARTESIAN_POINT ( 'NONE',  ( 80.17458025225667484, 217.0958772461660544, -9.188101187500095079 ) ) ;
#6985 = DIRECTION ( 'NONE',  ( -0.8660254037844387076, -0.4999999999999998890, -0.000000000000000000 ) ) ;
#6986 = CARTESIAN_POINT ( 'NONE',  ( 193.2100161762185735, 295.9974307820218087, -12.46499585622781758 ) ) ;
#6987 = LINE ( 'NONE', #7479, #98083 ) ;
#6988 = B_SPLINE_CURVE_WITH_KNOTS ( 'NONE', 3,
 ( #43229, #28040, #80297, #3281 ),
 .UNSPECIFIED., .F., .F.,
 ( 4, 4 ),
 ( 0.03632738840161289090, 0.04501103663793783877 ),
 .UNSPECIFIED. ) ;
#6989 = CARTESIAN_POINT ( 'NONE',  ( 161.1093323826042933, 251.5974460702646809, -13.93502574894237078 ) ) ;
#6990 = FACE_OUTER_BOUND ( 'NONE', #25679, .T. ) ;
#6992 = CARTESIAN_POINT ( 'NONE',  ( 76.56391922124960558, 51.24501030970186122, 16.05347363888732559 ) ) ;
#6991 = CARTESIAN_POINT ( 'NONE',  ( 99.82146873615951677, 239.9860189848785410, -2.679491924311252493 ) ) ;
#6993 = B_SPLINE_CURVE_WITH_KNOTS ( 'NONE', 3,
 ( #14162, #29367, #22252, #76946, #52641, #98785, #22762, #28869, #61741, #82620, #99765, #30856, #68844, #90716, #84110, #52148 ),
 .UNSPECIFIED., .F., .F.,
 ( 4, 1, 2, 2, 2, 1, 2, 2, 4 ),
 ( 0.000000000000000000, 0.1250000000000023592, 0.1875000000000024980, 0.2500000000000026645, 0.5000000000000045519, 0.6250000000000039968, 0.6875000000000037748, 0.7500000000000034417, 1.000000000000000000 ),
 .UNSPECIFIED. ) ;
#6994 = SURFACE_SIDE_STYLE ('',( #52097 ) ) ;
#6995 = CARTESIAN_POINT ( 'NONE',  ( 185.6713631041849055, 258.9584525764907426, -6.747383155299178092 ) ) ;
#6996 = CARTESIAN_POINT ( 'NONE',  ( 161.9775247817796924, 252.0936927241524472, 14.33142805341373283 ) ) ;
#6997 = CARTESIAN_POINT ( 'NONE',  ( 195.7578697689113199, 291.5844189092309193, 17.18796537138345215 ) ) ;
#6998 = CARTESIAN_POINT ( 'NONE',  ( 72.23865006290041890, 71.95475215217993536, 3.607730569270008125 ) ) ;
#6999 = CARTESIAN_POINT ( 'NONE',  ( 26.45420224557697608, 176.8923013555409796, 4.594050593750050204 ) ) ;
#7000 = CARTESIAN_POINT ( 'NONE',  ( 59.17381130624904273, 192.7202760586659736, -5.415160957724236172E-17 ) ) ;
#7001 = CARTESIAN_POINT ( 'NONE',  ( 157.6335212189247557, 257.6177276032722716, 16.76495363836117036 ) ) ;
#7002 = CARTESIAN_POINT ( 'NONE',  ( 46.78603705595332229, 27.41603393254330712, -1.583844403245396437 ) ) ;
#7003 = CARTESIAN_POINT ( 'NONE',  ( 82.32019150160303411, 49.92528730339438425, -13.92079164607254071 ) ) ;
#7004 = CARTESIAN_POINT ( 'NONE',  ( -5.895715345004023611, 160.7365022471901739, -10.00000000000009059 ) ) ;
#7005 = CARTESIAN_POINT ( 'NONE',  ( 52.89478003304684250, 201.3458772461660260, 9.188101187500095079 ) ) ;
#7006 = VECTOR ( 'NONE', #78316, 1000.000000000000227 ) ;
#7007 = EDGE_CURVE ( 'NONE', #31723, #20265, #46214, .T. ) ;
#7008 = CARTESIAN_POINT ( 'NONE',  ( 22.00287929847174695, 28.10171378149919263, 9.188101187500008038 ) ) ;
#7009 = CARTESIAN_POINT ( 'NONE',  ( 151.2646864780760723, 268.6488729594320830, -14.38346604407754548 ) ) ;
#7010 = CARTESIAN_POINT ( 'NONE',  ( 149.4965729687386045, 271.7113353911534546, -11.48413836595348059 ) ) ;
#7011 = CARTESIAN_POINT ( 'NONE',  ( 14.23992353553176926, 11.14754757982088407, -5.678558825948276656 ) ) ;
#7012 = CARTESIAN_POINT ( 'NONE',  ( 157.7593757092099906, 257.3997412317380054, -18.08445832352326121 ) ) ;
#7013 = CARTESIAN_POINT ( 'NONE',  ( 76.95477351241487440, 63.69079797318030955, 15.35326628456841824 ) ) ;
#7014 = CARTESIAN_POINT ( 'NONE',  ( 193.0622221429366050, 289.4054684591471300, 16.71589558189321778 ) ) ;
#7015 = ORIENTED_EDGE ( 'NONE', *, *, #33038, .F. ) ;
#7016 = CARTESIAN_POINT ( 'NONE',  ( 182.2103161154203406, 281.0079499109055519, -16.50159754525817135 ) ) ;
#7017 = CARTESIAN_POINT ( 'NONE',  ( 153.3639763765071677, 265.0127961955333262, 17.70482533658931956 ) ) ;
#7018 = EDGE_CURVE ( 'NONE', #67254, #82333, #70027, .T. ) ;
#7019 = DIRECTION ( 'NONE',  ( -0.8660254037844359321, -0.5000000000000051070, -0.000000000000000000 ) ) ;
#7020 = CARTESIAN_POINT ( 'NONE',  ( 110.8733765985977300, 241.4865022471902876, -10.00000000000009415 ) ) ;
#7021 = CARTESIAN_POINT ( 'NONE',  ( 161.1238074876215478, 251.5723744529297505, 13.42537408252843179 ) ) ;
#7022 = DIRECTION ( 'NONE',  ( -0.5000000000000005551, 0.8660254037844383745, -1.877843081442120711E-16 ) ) ;
#7023 = EDGE_LOOP ( 'NONE', ( #78278, #84620, #89349, #5803 ) ) ;
#7024 = AXIS2_PLACEMENT_3D ( 'NONE', #71217, #85967, #47876 ) ;
#7025 = CARTESIAN_POINT ( 'NONE',  ( 77.30051420685094854, 49.22732157280278642, 15.33771541198130350 ) ) ;
#7026 = VERTEX_POINT ( 'NONE', #47235 ) ;
#7027 = CARTESIAN_POINT ( 'NONE',  ( 166.5700286350222541, 264.7009711577636608, 17.59451997628320541 ) ) ;
#7028 = CARTESIAN_POINT ( 'NONE',  ( 190.2971537673054456, 279.0018434785596924, -16.59784016563796172 ) ) ;
#7029 = ADVANCED_FACE ( 'NONE', ( #63442 ), #31032, .F. ) ;
#7030 = DIRECTION ( 'NONE',  ( 0.4999999999999992784, -0.8660254037844390407, 0.000000000000000000 ) ) ;
#7031 = ORIENTED_EDGE ( 'NONE', *, *, #14781, .T. ) ;
#7033 = DIRECTION ( 'NONE',  ( 1.000000000000000000, 0.000000000000000000, 0.000000000000000000 ) ) ;
#7032 = CIRCLE ( 'NONE', #50709, 70.00000000000001421 ) ;
#7034 = CARTESIAN_POINT ( 'NONE',  ( 164.9971748156432056, 244.8635054444190757, -1.825016704039769788 ) ) ;
#7035 = B_SPLINE_CURVE_WITH_KNOTS ( 'NONE', 3,
 ( #40011, #48648, #63331, #24337, #86691, #62311, #85177, #85696, #31920, #70431, #71452, #79583, #55214, #39015, #87213, #46622, #2041, #94768, #10144, #93779, #41009, #78550, #77552, #9138 ),
 .UNSPECIFIED., .F., .F.,
 ( 4, 2, 2, 2, 2, 2, 2, 2, 2, 2, 2, 4 ),
 ( 0.000000000000000000, 0.1250000000000209277, 0.2500000000000418554, 0.3750000000000627831, 0.4375000000000565104, 0.5000000000000502931, 0.5625000000000439648, 0.6250000000000376366, 0.6875000000000314193, 0.7500000000000250910, 0.8750000000000125455, 1.000000000000000000 ),
 .UNSPECIFIED. ) ;
#7036 = CARTESIAN_POINT ( 'NONE',  ( 194.8067605455144076, 293.2317884077015151, -16.00245909155922774 ) ) ;
#7037 = CARTESIAN_POINT ( 'NONE',  ( -17.42236680055705023, 149.2012482093457777, 0.000000000000000000 ) ) ;
#7038 = CARTESIAN_POINT ( 'NONE',  ( -66.55019942848203129, 42.78701949053055387, -10.00000000000000000 ) ) ;
#7039 = VERTEX_POINT ( 'NONE', #53817 ) ;
#7040 = CARTESIAN_POINT ( 'NONE',  ( 18.65184876021338312, 28.95586893147755703, 7.433330006724141015 ) ) ;
#7041 = CARTESIAN_POINT ( 'NONE',  ( 175.4168809732710201, 254.3420697835979638, 7.923593415617963487 ) ) ;
#7042 = DIRECTION ( 'NONE',  ( -0.8770933717188629242, -0.4803199113995137437, 0.000000000000000000 ) ) ;
#7043 = EDGE_CURVE ( 'NONE', #58283, #10175, #70532, .T. ) ;
#7044 = VERTEX_POINT ( 'NONE', #85284 ) ;
#7045 = CARTESIAN_POINT ( 'NONE',  ( 181.1156277128715431, 292.7914473640799997, 9.490545386343454126 ) ) ;
#7046 = ADVANCED_FACE ( 'NONE', ( #92382 ), #30545, .T. ) ;
#7047 = CARTESIAN_POINT ( 'NONE',  ( 159.9531724557437826, 253.5999738052623229, -15.71074128491364874 ) ) ;
#7048 = ORIENTED_EDGE ( 'NONE', *, *, #19660, .T. ) ;
#7049 = CARTESIAN_POINT ( 'NONE',  ( 173.4043485434340823, 285.5429356164705723, 10.51786951157661143 ) ) ;
#7051 = CARTESIAN_POINT ( 'NONE',  ( 68.06773744437363405, 65.18829879967773877, -10.70695411350301818 ) ) ;
#7050 = CARTESIAN_POINT ( 'NONE',  ( 163.1916290246161054, 283.6901710720853771, -3.096747601227128666 ) ) ;
#7052 = CARTESIAN_POINT ( 'NONE',  ( 208.3226489551340990, 269.8215829728092103, -1.240262689467544366 ) ) ;
#7053 = CARTESIAN_POINT ( 'NONE',  ( 163.9149533033796047, 246.7379680887036670, 7.273005089308705706 ) ) ;
#7054 = CARTESIAN_POINT ( 'NONE',  ( 198.4706398937704819, 286.8857632237200619, 17.04020736381253798 ) ) ;
#7055 = CARTESIAN_POINT ( 'NONE',  ( -19.65312891409030271, 93.06504152958497400, 10.00000000000000888 ) ) ;
#7056 = CARTESIAN_POINT ( 'NONE',  ( 130.0249940097159254, 252.0024278399161517, -9.188101187500093303 ) ) ;
#7057 = CARTESIAN_POINT ( 'NONE',  ( 176.3695042043887327, 268.9327831528794945, 16.12022517601484850 ) ) ;
#7058 = CARTESIAN_POINT ( 'NONE',  ( 182.0444953139967197, 260.3474170450806469, 9.385908224742504302 ) ) ;
#7059 = CARTESIAN_POINT ( 'NONE',  ( 74.43750904794977430, 201.5327760586659167, 1.948934522072303157E-15 ) ) ;
#7060 = ORIENTED_EDGE ( 'NONE', *, *, #6142, .F. ) ;
#7061 = CARTESIAN_POINT ( 'NONE',  ( 173.8505786369982786, 250.7855131160717121, 2.429319715737904950 ) ) ;
#7062 = CARTESIAN_POINT ( 'NONE',  ( 161.9461893331167914, 280.9078031139047198, -10.53061385661272276 ) ) ;
#7063 = ORIENTED_EDGE ( 'NONE', *, *, #11979, .F. ) ;
#7064 = CARTESIAN_POINT ( 'NONE',  ( 32.30839531297598199, 123.0650415295850593, -60.00000000000000000 ) ) ;
#7065 = ORIENTED_EDGE ( 'NONE', *, *, #85582, .F. ) ;
#7066 = EDGE_CURVE ( 'NONE', #19179, #66781, #32390, .T. ) ;
#7067 = CARTESIAN_POINT ( 'NONE',  ( 68.76057960370418698, 222.0530062829863027, -4.648177544792955347E-16 ) ) ;
#7068 = CARTESIAN_POINT ( 'NONE',  ( 67.15236828973634431, 67.72320738538478224, 6.588214651295674074 ) ) ;
#7069 = CARTESIAN_POINT ( 'NONE',  ( 194.2311797008547103, 284.7782822170849499, 17.68315500314775335 ) ) ;
#7070 = CARTESIAN_POINT ( 'NONE',  ( 146.6363376198206652, 276.6654083370839885, -0.5879280619134327202 ) ) ;
#7071 = CARTESIAN_POINT ( 'NONE',  ( 68.02005152741377003, 65.43521726584035036, 10.42530429588983054 ) ) ;
#7072 = CARTESIAN_POINT ( 'NONE',  ( 194.3799873100184641, 293.9709813348915191, 15.33105633561973669 ) ) ;
#7073 = CARTESIAN_POINT ( 'NONE',  ( 70.18763995946753198, 63.26540913664066323, 13.15406633596375485 ) ) ;
#7074 = VERTEX_POINT ( 'NONE', #56325 ) ;
#7075 = EDGE_CURVE ( 'NONE', #88359, #90349, #41118, .T. ) ;
#7076 = CARTESIAN_POINT ( 'NONE',  ( 161.7135578690656246, 250.5508968284854063, -12.67518793468364002 ) ) ;
#7077 = VERTEX_POINT ( 'NONE', #73056 ) ;
#7078 = CARTESIAN_POINT ( 'NONE',  ( 76.07595347892329585, 51.40484473107772345, -15.65947719172055486 ) ) ;
#7079 = EDGE_CURVE ( 'NONE', #78204, #68063, #17852, .T. ) ;
#7080 = ADVANCED_FACE ( 'NONE', ( #3651 ), #34531, .F. ) ;
#7081 = CARTESIAN_POINT ( 'NONE',  ( 75.88031102442633369, 65.78928292664191702, -14.15509851726639390 ) ) ;
#7082 = VECTOR ( 'NONE', #55718, 999.9999999999998863 ) ;
#7083 = EDGE_CURVE ( 'NONE', #67877, #76666, #72051, .T. ) ;
#7084 = CARTESIAN_POINT ( 'NONE',  ( 194.8918758260624315, 279.6717792136230401, 17.28916287495260917 ) ) ;
#7085 = CARTESIAN_POINT ( 'NONE',  ( 162.9141107278308880, 261.5451400836783478, 17.20276467470873172 ) ) ;
#7086 = CARTESIAN_POINT ( 'NONE',  ( 138.1979352100490530, 262.8464784336661637, 1.353441290958777327E-15 ) ) ;
#7087 = ORIENTED_EDGE ( 'NONE', *, *, #68019, .F. ) ;
#7088 = CARTESIAN_POINT ( 'NONE',  ( 87.75230366022445594, 44.21248639555269477, 4.670146826978181842 ) ) ;
#7089 = EDGE_CURVE ( 'NONE', #50774, #99290, #39529, .T. ) ;
#7090 = DIRECTION ( 'NONE',  ( -1.000000000000000000, 0.000000000000000000, 0.000000000000000000 ) ) ;
#7091 = EDGE_CURVE ( 'NONE', #18050, #24730, #4126, .T. ) ;
#7092 = CARTESIAN_POINT ( 'NONE',  ( 87.97614123416462917, 44.06541336701370426, -1.724168466821650147 ) ) ;
#7093 = CARTESIAN_POINT ( 'NONE',  ( 153.0444155045374544, 265.5662918618958201, -16.15173036748435109 ) ) ;
#7094 = CARTESIAN_POINT ( 'NONE',  ( 72.67799729538583620, 70.93760247754363490, 7.641220802698796888 ) ) ;
#7095 = CIRCLE ( 'NONE', #2281, 0.1418229129684506207 ) ;
#7096 = CARTESIAN_POINT ( 'NONE',  ( 68.45771554780012025, 67.43233330954889482, -8.366793215440479159 ) ) ;
#7097 = ORIENTED_EDGE ( 'NONE', *, *, #20698, .T. ) ;
#7098 = CARTESIAN_POINT ( 'NONE',  ( 198.5871620011634491, 266.6819785607618769, 4.508239282148444715 ) ) ;
#7099 = CARTESIAN_POINT ( 'NONE',  ( -19.65312891409030271, 93.06504152958497400, -10.00000000000000888 ) ) ;
#7100 = CARTESIAN_POINT ( 'NONE',  ( 72.35093020053528790, 71.14706991326251284, -6.078630472467451362 ) ) ;
#7101 = CARTESIAN_POINT ( 'NONE',  ( 184.5883480666688286, 263.6785044138370040, -12.30340380393476707 ) ) ;
#7102 = CARTESIAN_POINT ( 'NONE',  ( 198.8150538021965588, 265.6931018340174546, 1.636156699923587254 ) ) ;
#7103 = ORIENTED_EDGE ( 'NONE', *, *, #50199, .F. ) ;
#7104 = AXIS2_PLACEMENT_3D ( 'NONE', #35213, #58500, #89473 ) ;
#7105 = LINE ( 'NONE', #76042, #38425 ) ;
#7106 = CARTESIAN_POINT ( 'NONE',  ( 183.6995465130360117, 281.2503605932585060, 17.37810211150572570 ) ) ;
#7107 = DIRECTION ( 'NONE',  ( -0.7561390817803210762, 0.6544109481086124447, 0.000000000000000000 ) ) ;
#7109 = CARTESIAN_POINT ( 'NONE',  ( 196.9080397933726942, 269.7016881256661804, 12.39056067425276630 ) ) ;
#7108 = CARTESIAN_POINT ( 'NONE',  ( 165.3498924805469414, 258.0561931571047580, -16.34667607723879001 ) ) ;
#7110 = CARTESIAN_POINT ( 'NONE',  ( 25.44954664093420149, 26.64441083166262203, -10.00000000000000533 ) ) ;
#7111 = LINE ( 'NONE', #76048, #82351 ) ;
#7112 = CARTESIAN_POINT ( 'NONE',  ( 165.7002536143517091, 285.3157116585052222, -3.145807942481822828 ) ) ;
#7113 = CARTESIAN_POINT ( 'NONE',  ( 15.73079442999205924, 32.58029201028040944, 1.583844403245363353 ) ) ;
#7114 = CARTESIAN_POINT ( 'NONE',  ( -97.59541525468981149, 48.06504152958505216, 36.50000000000000000 ) ) ;
#7115 = CARTESIAN_POINT ( 'NONE',  ( -8.863483026448420787, 159.5643266524160140, 9.188101187500095079 ) ) ;
#7116 = PLANE ( 'NONE',  #24194 ) ;
#7117 = EDGE_LOOP ( 'NONE', ( #367, #26154, #1745, #35741 ) ) ;
#7118 = CARTESIAN_POINT ( 'NONE',  ( 66.73473034183035679, 67.48348876847576605, -6.586817036978919404 ) ) ;
#7119 = CARTESIAN_POINT ( 'NONE',  ( 72.54816569808835425, 70.68207713539275971, -7.935695741106848722 ) ) ;
#7120 = CARTESIAN_POINT ( 'NONE',  ( 202.7163547726785282, 274.3787297666792711, -12.85394322792611632 ) ) ;
#7121 = CARTESIAN_POINT ( 'NONE',  ( 81.62507666485218749, 41.61289278366178479, 5.610847245266504579 ) ) ;
#7122 = CARTESIAN_POINT ( 'NONE',  ( 14.68175618682351136, 167.0327760586659451, 1.948934522072302763E-15 ) ) ;
#7123 = CARTESIAN_POINT ( 'NONE',  ( 21.20711791317337003, 34.01751292744057054, 6.180339887498949913 ) ) ;
#7124 = CARTESIAN_POINT ( 'NONE',  ( 74.15479259499207387, 55.62765001666249276, -16.59030973340311022 ) ) ;
#7125 = B_SPLINE_CURVE_WITH_KNOTS ( 'NONE', 3,
 ( #90677, #58704, #21233, #97746, #52605, #28314 ),
 .UNSPECIFIED., .F., .F.,
 ( 4, 2, 4 ),
 ( 0.001525191237219494008, 0.001894091869566394458, 0.002262992501913294908 ),
 .UNSPECIFIED. ) ;
#7126 = CARTESIAN_POINT ( 'NONE',  ( 170.0564342972344321, 270.6948931233863505, -17.19293478356221883 ) ) ;
#7127 = CARTESIAN_POINT ( 'NONE',  ( 150.1215823127449198, 276.5650925005066938, 4.233095963711685172 ) ) ;
#7128 = CARTESIAN_POINT ( 'NONE',  ( 179.4321052950799356, 255.0977940521856340, -4.021643327155957515 ) ) ;
#7129 = CARTESIAN_POINT ( 'NONE',  ( 188.1673108261343543, 259.1851068472254269, -0.8032118547848330348 ) ) ;
#7130 = CARTESIAN_POINT ( 'NONE',  ( 56.38594494382682853, 203.3615022471902307, -10.00000000000009592 ) ) ;
#7131 = DIRECTION ( 'NONE',  ( 0.9981280818701453450, 0.06115825522547521653, 0.000000000000000000 ) ) ;
#7132 = CARTESIAN_POINT ( 'NONE',  ( 189.8238368927809745, 301.8624653444729802, -0.3620111495846872751 ) ) ;
#7133 = CARTESIAN_POINT ( 'NONE',  ( 19.11978928545374501, 181.8458772461660544, 9.188101187500095079 ) ) ;
#7134 = CARTESIAN_POINT ( 'NONE',  ( -14.83894680564148238, 24.48641780169620219, -10.00000000000000000 ) ) ;
#7135 = CARTESIAN_POINT ( 'NONE',  ( 125.6679772465819127, 253.3615022471903444, 5.000000000000046185 ) ) ;
#7136 = CARTESIAN_POINT ( 'NONE',  ( 41.76871284172324295, 36.06628583063844928, -9.188101187500006262 ) ) ;
#7137 = CARTESIAN_POINT ( 'NONE',  ( 42.45923888023187232, 122.5484010731363043, 10.00000000000000000 ) ) ;
#7138 = EDGE_CURVE ( 'NONE', #46017, #14068, #4579, .T. ) ;
#7139 = CARTESIAN_POINT ( 'NONE',  ( 164.7694554770609159, 245.2579269087094076, -3.003635650077957742 ) ) ;
#7140 = CARTESIAN_POINT ( 'NONE',  ( 189.1957819607296187, 268.1245522628738627, 13.92255382446146150 ) ) ;
#7141 = CARTESIAN_POINT ( 'NONE',  ( 202.5650245025327081, 277.7940810556053179, -15.59262966521933791 ) ) ;
#7142 = CARTESIAN_POINT ( 'NONE',  ( 179.6677993555305477, 263.0935507050606930, -13.53422970562010974 ) ) ;
#7143 = CONTEXT_DEPENDENT_SHAPE_REPRESENTATION ( #14219, #12826 ) ;
#7144 = CARTESIAN_POINT ( 'NONE',  ( 18.92729281690869314, 22.87878583063841020, -9.188101187500006262 ) ) ;
#7145 = CARTESIAN_POINT ( 'NONE',  ( 13.76346889243896321, 13.11029122506292843, -8.090169943749478065 ) ) ;
#7146 = CARTESIAN_POINT ( 'NONE',  ( 71.84836080304555139, 59.06364556286701628, 15.87505501405348340 ) ) ;
#7147 = CARTESIAN_POINT ( 'NONE',  ( 155.6435836392643637, 261.0644005951349982, 17.58841156286628049 ) ) ;
#7148 = VERTEX_POINT ( 'NONE', #82180 ) ;
#7149 = CARTESIAN_POINT ( 'NONE',  ( 181.6976215744686556, 289.2235858052403614, 12.51094214070181465 ) ) ;
#7150 = CARTESIAN_POINT ( 'NONE',  ( 87.08523622459452440, 45.32592727123765286, -7.867701777046974598 ) ) ;
#7151 = CARTESIAN_POINT ( 'NONE',  ( -19.10035114162887737, 41.33634930963552279, 59.99999999999999289 ) ) ;
#7152 = CARTESIAN_POINT ( 'NONE',  ( 81.87175288788205307, 42.17655061954369700, 7.612090732984669650 ) ) ;
#7153 = EDGE_CURVE ( 'NONE', #30262, #70893, #60791, .T. ) ;
#7154 = VERTEX_POINT ( 'NONE', #67416 ) ;
#7155 = CARTESIAN_POINT ( 'NONE',  ( 157.3525109086878899, 264.5174536549614572, 17.64881377233731641 ) ) ;
#7156 = CARTESIAN_POINT ( 'NONE',  ( 69.42645013659684139, 70.63508196826001040, -1.496691613166120982 ) ) ;
#7157 = CARTESIAN_POINT ( 'NONE',  ( 76.63732740674304011, 63.83366213508917753, 14.86362707207269551 ) ) ;
#7158 = ADVANCED_FACE ( 'NONE', ( #74046 ), #20341, .T. ) ;
#7159 = CARTESIAN_POINT ( 'NONE',  ( 179.4449360448816719, 257.2231220042240238, -7.316974778047405259 ) ) ;
#7160 = ORIENTED_EDGE ( 'NONE', *, *, #55084, .T. ) ;
#7161 = EDGE_LOOP ( 'NONE', ( #92672, #19343, #85360, #2232 ) ) ;
#7163 = CARTESIAN_POINT ( 'NONE',  ( 164.4864504671816690, 245.7481059646165704, 6.337356894698421783 ) ) ;
#7162 = CARTESIAN_POINT ( 'NONE',  ( 80.74974841587442143, 43.27611110060701805, 10.01619596027649095 ) ) ;
#7164 = VERTEX_POINT ( 'NONE', #28935 ) ;
#7165 = CARTESIAN_POINT ( 'NONE',  ( 190.8443993347725325, 300.0947993426467519, 8.522468760355437212 ) ) ;
#7166 = CARTESIAN_POINT ( 'NONE',  ( 71.18266754637075167, 67.94496896153198406, 10.47851208213521446 ) ) ;
#7167 = CARTESIAN_POINT ( 'NONE',  ( 80.22399782384964340, 57.81478883376428257, 16.60249858296848657 ) ) ;
#7168 = DIRECTION ( 'NONE',  ( 0.5544813661758196677, 0.8321961394790273747, 0.000000000000000000 ) ) ;
#7170 = VERTEX_POINT ( 'NONE', #52213 ) ;
#7169 = B_SPLINE_CURVE_WITH_KNOTS ( 'NONE', 3,
 ( #54201, #76061, #85169, #98857, #83674, #46614, #29433, #75545, #21830, #6640, #14729, #45610, #7120, #18238, #63324, #17215, #87704, #17739 ),
 .UNSPECIFIED., .F., .F.,
 ( 4, 2, 2, 2, 2, 2, 2, 2, 4 ),
 ( 0.003007356136897285266, 0.003103104521746957896, 0.003198852906596630959, 0.003294601291446303589, 0.003390349676295976653, 0.003581846445995281580, 0.003773343215694586941, 0.004539330294491807950, 0.006071304452086345380 ),
 .UNSPECIFIED. ) ;
#7171 = CARTESIAN_POINT ( 'NONE',  ( 189.9925954911225290, 301.5701668779311717, 0.1154287172046158938 ) ) ;
#7172 = CIRCLE ( 'NONE', #39549, 0.1418229129684575596 ) ;
#7173 = EDGE_LOOP ( 'NONE', ( #69366, #3079, #91309, #12802 ) ) ;
#7174 = CARTESIAN_POINT ( 'NONE',  ( 157.1135969804030310, 258.5182628004787944, 17.19660297500358226 ) ) ;
#7175 = CARTESIAN_POINT ( 'NONE',  ( 158.0882106229127828, 265.1277990769271469, 17.41991095839799542 ) ) ;
#7176 = B_SPLINE_CURVE_WITH_KNOTS ( 'NONE', 3,
 ( #91327, #21887, #54775, #84238 ),
 .UNSPECIFIED., .F., .F.,
 ( 4, 4 ),
 ( 0.008222014946565199198, 0.01444170924531920988 ),
 .UNSPECIFIED. ) ;
#7177 = VERTEX_POINT ( 'NONE', #59811 ) ;
#7178 = CARTESIAN_POINT ( 'NONE',  ( 148.9275518150011806, 272.6969089400084272, 12.34519124974546500 ) ) ;
#7179 = CARTESIAN_POINT ( 'NONE',  ( 81.60871807086439844, 59.37387260405306932, -0.4240240480782162535 ) ) ;
#7180 = ORIENTED_EDGE ( 'NONE', *, *, #78042, .T. ) ;
#7181 = DIRECTION ( 'NONE',  ( 0.000000000000000000, 0.000000000000000000, 1.000000000000000000 ) ) ;
#7182 = CARTESIAN_POINT ( 'NONE',  ( 160.0710471321888235, 254.2385718108182573, 15.38664727912921926 ) ) ;
#7183 = FACE_OUTER_BOUND ( 'NONE', #37313, .T. ) ;
#7184 = CARTESIAN_POINT ( 'NONE',  ( 83.75851852475534542, 52.19494488360223983, 14.66139263155008798 ) ) ;
#7185 = VERTEX_POINT ( 'NONE', #20849 ) ;
#7186 = ORIENTED_EDGE ( 'NONE', *, *, #8917, .F. ) ;
#7187 = EDGE_CURVE ( 'NONE', #44016, #33601, #45047, .T. ) ;
#7188 = CARTESIAN_POINT ( 'NONE',  ( 86.54292033101232562, 46.25028892199808439, 8.970843135639702481 ) ) ;
#7189 = CARTESIAN_POINT ( 'NONE',  ( 79.70677143361787387, 46.01134058561530793, 12.98241517792750699 ) ) ;
#7190 = CARTESIAN_POINT ( 'NONE',  ( 190.1693911629507738, 301.2639477917662703, -5.112716700269980485 ) ) ;
#7191 = CARTESIAN_POINT ( 'NONE',  ( 82.33309958831539177, 53.73407448881687287, 15.84243556053685431 ) ) ;
#7192 = CARTESIAN_POINT ( 'NONE',  ( 149.7166446726674565, 271.3301600186404698, 12.26048591517335495 ) ) ;
#7193 = CARTESIAN_POINT ( 'NONE',  ( 133.0291931787496367, 257.6115022471902876, -5.000000000000047962 ) ) ;
#7194 = CARTESIAN_POINT ( 'NONE',  ( 191.7416542989093671, 298.5407081574186350, 9.608469308039788714 ) ) ;
#7195 = CARTESIAN_POINT ( 'NONE',  ( 191.5893301551938350, 298.8045413135534432, -8.323356515452589477 ) ) ;
#7196 = EDGE_CURVE ( 'NONE', #66499, #6194, #58004, .T. ) ;
#7197 = CARTESIAN_POINT ( 'NONE',  ( 163.4623095168547025, 257.8152101734419261, 15.54367929412465976 ) ) ;
#7198 = CARTESIAN_POINT ( 'NONE',  ( 69.05858150271376417, 65.60398784760005242, 10.87676190501699836 ) ) ;
#7200 = CARTESIAN_POINT ( 'NONE',  ( 162.0192538899617318, 268.0510789565263394, -17.53028463913764057 ) ) ;
#7199 = CARTESIAN_POINT ( 'NONE',  ( 149.0598351764325002, 272.4677874370131576, -11.59078276432863674 ) ) ;
#7201 = DIRECTION ( 'NONE',  ( -0.8660254037844387076, -0.4999999999999998890, -0.000000000000000000 ) ) ;
#7202 = CARTESIAN_POINT ( 'NONE',  ( 171.4770449210933236, 289.0940507889877722, 4.287227504194440542 ) ) ;
#7203 = CARTESIAN_POINT ( 'NONE',  ( 78.44703544257603767, 47.42314817051035902, 14.26473360639000987 ) ) ;
#7204 = ORIENTED_EDGE ( 'NONE', *, *, #62645, .T. ) ;
#7205 = CARTESIAN_POINT ( 'NONE',  ( 190.7661460928718498, 300.2303379334758233, -3.568894913151918313 ) ) ;
#7206 = CARTESIAN_POINT ( 'NONE',  ( 80.04801989711464216, 52.84706496129958708, -15.53468051483373991 ) ) ;
#7207 = EDGE_CURVE ( 'NONE', #17355, #2827, #70957, .T. ) ;
#7208 = CARTESIAN_POINT ( 'NONE',  ( 202.9521567073010146, 278.0333832980851412, 15.07843176052885781 ) ) ;
#7209 = CARTESIAN_POINT ( 'NONE',  ( 79.17243950938065211, 45.84086033299786322, 13.07686966769901638 ) ) ;
#7210 = LINE ( 'NONE', #84757, #83975 ) ;
#7211 = CARTESIAN_POINT ( 'NONE',  ( 147.9974455564266691, 274.3079002362971437, -10.09869768668086820 ) ) ;
#7212 = CARTESIAN_POINT ( 'NONE',  ( 167.7560327080170453, 284.3066376844275283, -7.994707968029326928 ) ) ;
#7213 = ORIENTED_EDGE ( 'NONE', *, *, #78877, .T. ) ;
#7214 = CARTESIAN_POINT ( 'NONE',  ( 80.20448007545800806, 58.22194284664072939, -16.60717859687067843 ) ) ;
#7215 = CARTESIAN_POINT ( 'NONE',  ( 159.3586121662929713, 254.6297824347537642, -15.50090345830412630 ) ) ;
#7216 = CARTESIAN_POINT ( 'NONE',  ( 72.56735714755242839, 71.56619014045929816, 5.379842731025054725 ) ) ;
#7217 = CARTESIAN_POINT ( 'NONE',  ( 35.87196818813498567, 201.5177522451419350, 5.000000000000046185 ) ) ;
#7218 = CARTESIAN_POINT ( 'NONE',  ( 114.8970466070627907, 227.9548013555409796, -4.594050593750042211 ) ) ;
#7219 = CARTESIAN_POINT ( 'NONE',  ( 199.1867231605587278, 285.6454706231928071, -17.41989184023605475 ) ) ;
#7220 = CARTESIAN_POINT ( 'NONE',  ( 66.79023490949526831, 67.33564584442949297, -6.933441031880490435 ) ) ;
#7221 = LINE ( 'NONE', #23414, #59978 ) ;
#7222 = DIRECTION ( 'NONE',  ( 0.000000000000000000, 0.000000000000000000, 1.000000000000000000 ) ) ;
#7223 = CARTESIAN_POINT ( 'NONE',  ( 33.24700223256990483, 183.8768266524160140, -9.188101187500091527 ) ) ;
#7224 = CARTESIAN_POINT ( 'NONE',  ( 82.20387338395363486, 40.63080856265045782, 3.356284137154774694 ) ) ;
#7225 = CARTESIAN_POINT ( 'NONE',  ( -27.42236680055714260, 166.5217562850347406, 1.224646799147364892E-15 ) ) ;
#7226 = EDGE_LOOP ( 'NONE', ( #49077, #100262, #35616, #57875 ) ) ;
#7227 = CARTESIAN_POINT ( 'NONE',  ( 71.72736245888779649, 65.63246871389105763, 12.21051025674438506 ) ) ;
#7228 = CARTESIAN_POINT ( 'NONE',  ( 178.4621772040343899, 265.6203404136728068, 16.07317361885528584 ) ) ;
#7229 = CARTESIAN_POINT ( 'NONE',  ( 26.96143514339544467, 174.8262482093457777, 3.021315404115420679E-15 ) ) ;
#7230 = CARTESIAN_POINT ( 'NONE',  ( 190.1607982559816890, 301.2788311432216233, -4.972636536415983244 ) ) ;
#7231 = CARTESIAN_POINT ( 'NONE',  ( 46.32860941106298469, 116.4404604047837779, 177.5919119679930134 ) ) ;
#7232 = VECTOR ( 'NONE', #19733, 1000.000000000000227 ) ;
#7233 = ADVANCED_FACE ( 'NONE', ( #82682 ), #51213, .F. ) ;
#7234 = CARTESIAN_POINT ( 'NONE',  ( 151.2546443255573934, 275.3395117651207897, -9.775857568146751220 ) ) ;
#7235 = CARTESIAN_POINT ( 'NONE',  ( -25.86065208768103219, 41.70698537633906255, 59.99999999999999289 ) ) ;
#7236 = CARTESIAN_POINT ( 'NONE',  ( 101.7620676594010405, 242.8927522451419634, 2.944929066748280225E-16 ) ) ;
#7237 = CARTESIAN_POINT ( 'NONE',  ( 194.6626581126282929, 293.0278785836280235, -14.76912774068482292 ) ) ;
#7238 = ORIENTED_EDGE ( 'NONE', *, *, #25961, .F. ) ;
#7239 = EDGE_CURVE ( 'NONE', #1456, #11457, #92521, .T. ) ;
#7240 = VECTOR ( 'NONE', #599, 1000.000000000000114 ) ;
#7241 = CARTESIAN_POINT ( 'NONE',  ( 163.0309151244508712, 248.2691671304387739, 11.27270415168660200 ) ) ;
#7242 = CARTESIAN_POINT ( 'NONE',  ( 154.9082074166165910, 263.9767827779738241, 17.34157506132131488 ) ) ;
#7243 = CARTESIAN_POINT ( 'NONE',  ( 14.24839638916628459, 179.0333772461660544, 9.188101187500095079 ) ) ;
#7244 = CARTESIAN_POINT ( 'NONE',  ( 8.399671500380161859, 16.80066082961419482, 10.00000000000000533 ) ) ;
#7245 = CARTESIAN_POINT ( 'NONE',  ( 192.2881851781887406, 272.0424645381762048, 14.23089303299685149 ) ) ;
#7246 = CARTESIAN_POINT ( 'NONE',  ( 71.57792465326454590, 59.00132549361326539, -15.84990762337844572 ) ) ;
#7247 = CARTESIAN_POINT ( 'NONE',  ( 73.17900167297862879, 69.84980244707995212, 9.598651498403647508 ) ) ;
#7249 = CARTESIAN_POINT ( 'NONE',  ( 77.36034478572226192, 203.2202760586659736, -5.415160957724236172E-17 ) ) ;
#7248 = CARTESIAN_POINT ( 'NONE',  ( 174.8809725116003619, 286.3757395011697326, 10.48282596314093063 ) ) ;
#7250 = CARTESIAN_POINT ( 'NONE',  ( 200.4592688079413847, 283.4413569069752725, 18.39277739746426832 ) ) ;
#7251 = CARTESIAN_POINT ( 'NONE',  ( -17.33262083840142509, 129.0458036431182904, -30.52142883766501669 ) ) ;
#7252 = CARTESIAN_POINT ( 'NONE',  ( 71.55555785148570180, 70.00198118308297524, 8.105299072955192585 ) ) ;
#7253 = CARTESIAN_POINT ( 'NONE',  ( 8.207198731066840836, 28.23654200823201066, 1.583844403245363353 ) ) ;
#7254 = ORIENTED_EDGE ( 'NONE', *, *, #54717, .T. ) ;
#7255 =( BOUNDED_CURVE ( )  B_SPLINE_CURVE ( 2, ( #14900, #45790, #76710, #100029, #30615, #61500, #31095, #22996, #15385 ),
 .UNSPECIFIED., .F., .T. ) 
 B_SPLINE_CURVE_WITH_KNOTS ( ( 3, 2, 2, 2, 3 ),
 ( 0.9233870967741935054, 0.9247311827956988806, 0.9274193548387096309, 0.9301075268817203812, 0.9314516129032257563 ),
 .UNSPECIFIED. ) 
 CURVE ( )  GEOMETRIC_REPRESENTATION_ITEM ( )  RATIONAL_B_SPLINE_CURVE ( ( 0.9330127018922194093, 0.9330127018922194093, 1.000000000000000000, 0.8660254037844387076, 1.000000000000000000, 0.8660254037844387076, 1.000000000000000000, 0.9330127018922194093, 0.9330127018922194093 ) ) 
 REPRESENTATION_ITEM ( '' )  );
#7256 = CARTESIAN_POINT ( 'NONE',  ( 162.2803608993413320, 267.3877610371002902, 16.48173369095244567 ) ) ;
#7257 = CARTESIAN_POINT ( 'NONE',  ( 14.02286894203806433, 172.2365022471902307, 10.00000000000009592 ) ) ;
#7258 = CARTESIAN_POINT ( 'NONE',  ( 163.8111161534324935, 246.9178193081252743, -7.110480325054721717 ) ) ;
#7259 = CARTESIAN_POINT ( 'NONE',  ( 140.0928864244750685, 245.5643266524160424, -9.188101187500093303 ) ) ;
#7260 = CARTESIAN_POINT ( 'NONE',  ( 32.08968265630385019, 27.03085787977765264, 9.188101187500006262 ) ) ;
#7261 = CARTESIAN_POINT ( 'NONE',  ( 164.0665640930923246, 260.4805839323781811, -16.15133822266555441 ) ) ;
#7262 = DIRECTION ( 'NONE',  ( 0.000000000000000000, 0.000000000000000000, 1.000000000000000000 ) ) ;
#7263 = CARTESIAN_POINT ( 'NONE',  ( 196.4338619668326942, 281.5298852278613140, -17.66916360587062584 ) ) ;
#7264 = EDGE_CURVE ( 'NONE', #90523, #11943, #13724, .T. ) ;
#7266 = CARTESIAN_POINT ( 'NONE',  ( -20.01211276271284945, 173.6868197944959036, -22.49999999999984013 ) ) ;
#7265 = CARTESIAN_POINT ( 'NONE',  ( 68.31860697027661899, 67.22880204738007137, 9.390919083417214708 ) ) ;
#7267 = CARTESIAN_POINT ( 'NONE',  ( 68.58219988125976840, 64.16363137176722375, 11.86921294676530891 ) ) ;
#7268 = ORIENTED_EDGE ( 'NONE', *, *, #85914, .F. ) ;
#7269 = CARTESIAN_POINT ( 'NONE',  ( 190.9907605556751093, 299.8412942717858414, 8.799173206188184437 ) ) ;
#7270 = FACE_OUTER_BOUND ( 'NONE', #9816, .T. ) ;
#7271 = FACE_OUTER_BOUND ( 'NONE', #5084, .T. ) ;
#7272 = CARTESIAN_POINT ( 'NONE',  ( 196.5433769452094737, 289.0926436443681382, 16.88005588253986033 ) ) ;
#7273 = CARTESIAN_POINT ( 'NONE',  ( 8.301057521190555732, 26.83396525600388571, -2.839279412974133887 ) ) ;
#7274 = ORIENTED_EDGE ( 'NONE', *, *, #22277, .F. ) ;
#7275 = CARTESIAN_POINT ( 'NONE',  ( 165.9969153545198708, 246.1123342570000716, -1.176638740111072723 ) ) ;
#7276 = VECTOR ( 'NONE', #26233, 1000.000000000000000 ) ;
#7277 = CARTESIAN_POINT ( 'NONE',  ( -16.08955603893133812, 171.5177522451419350, 5.000000000000046185 ) ) ;
#7278 = CARTESIAN_POINT ( 'NONE',  ( 29.78943643340442549, 199.5530062829863027, -4.648177544792955347E-16 ) ) ;
#7279 = CARTESIAN_POINT ( 'NONE',  ( 71.75944102250285539, 72.15356206472488054, 0.5915691668053513208 ) ) ;
#7280 = EDGE_CURVE ( 'NONE', #72868, #26607, #98799, .T. ) ;
#7281 = CARTESIAN_POINT ( 'NONE',  ( 200.7975900406536596, 281.6935573902783858, -16.84479620147121537 ) ) ;
#7282 = CARTESIAN_POINT ( 'NONE',  ( -27.64350997085663408, 76.90478749174087625, 0.000000000000000000 ) ) ;
#7283 = CARTESIAN_POINT ( 'NONE',  ( 96.56591523669446531, 219.8927522451417929, -10.00000000000009237 ) ) ;
#7284 = ADVANCED_FACE ( 'NONE', ( #6629 ), #63314, .T. ) ;
#7285 = CARTESIAN_POINT ( 'NONE',  ( 148.1846377449773513, 246.3615022471901739, 5.000000000000051514 ) ) ;
#7286 = CARTESIAN_POINT ( 'NONE',  ( 201.1679199471075492, 282.2139371290980989, -16.62385308864941535 ) ) ;
#7287 = CARTESIAN_POINT ( 'NONE',  ( -22.72465050930169994, 22.87247442008841958, 10.00000000000000000 ) ) ;
#7288 = CARTESIAN_POINT ( 'NONE',  ( -71.61465314115659453, 63.06504152958490295, 10.00000000000000888 ) ) ;
#7289 = ORIENTED_EDGE ( 'NONE', *, *, #84191, .F. ) ;
#7290 = CARTESIAN_POINT ( 'NONE',  ( 190.0274641710971082, 301.5097725526222803, 3.738976720635653450 ) ) ;
#7291 = DIRECTION ( 'NONE',  ( -0.8660254037844387076, -0.4999999999999998890, -0.000000000000000000 ) ) ;
#7292 = CARTESIAN_POINT ( 'NONE',  ( 82.19618238725253434, 45.38674811654465913, -10.67622378202659483 ) ) ;
#7293 = B_SPLINE_CURVE_WITH_KNOTS ( 'NONE', 3,
 ( #39344, #46969, #31746, #93093, #99686, #16067, #100193, #70769, #6969, #30778, #7982, #24172, #38858, #77888, #1384, #92608 ),
 .UNSPECIFIED., .F., .F.,
 ( 4, 2, 2, 2, 2, 2, 2, 4 ),
 ( -9.572876425213601166E-06, 3.117184193876883545E-05, 7.191656030275126528E-05, 0.0001534059970307206650, 0.0003163848704866175331, 0.0006423426173984245506, 0.0009683003643102314597, 0.001294258111222038260 ),
 .UNSPECIFIED. ) ;
#7294 = ORIENTED_EDGE ( 'NONE', *, *, #95774, .F. ) ;
#7295 = DIRECTION ( 'NONE',  ( 1.000000000000000000, 0.000000000000000000, 0.000000000000000000 ) ) ;
#7296 = CARTESIAN_POINT ( 'NONE',  ( 79.25704083171594050, 59.98661423191556707, -16.48971415753126735 ) ) ;
#7297 = B_SPLINE_CURVE_WITH_KNOTS ( 'NONE', 3,
 ( #15027, #92583, #836, #84975, #86009, #61128, #30246, #7435, #15520, #84485, #92104, #39808, #8941, #23125, #24143, #38827, #22649, #47924, #16039, #77857, #54018, #45919, #70739, #76837, #39314, #94082, #38328, #69734, #46422, #31231, #100165, #77347, #340, #55028, #16535, #47432, #1351, #86503, #63137, #17031, #62117, #93064, #23619, #54512, #78863, #85491, #46940, #37829 ),
 .UNSPECIFIED., .F., .F.,
 ( 4, 2, 2, 2, 2, 2, 2, 2, 2, 2, 2, 2, 2, 2, 2, 2, 2, 2, 2, 2, 2, 2, 2, 4 ),
 ( 0.002769618252134798449, 0.002972599584400432374, 0.003175580916666066733, 0.003277071582798824281, 0.003378562248931581830, 0.003480052915064339378, 0.003581543581197097360, 0.003784524913462612456, 0.003987506245728127986, 0.004393468910259121750, 0.005205394239320976571, 0.006017319568382830525, 0.006829244897444684478, 0.007641170226506538432, 0.007742660892639252612, 0.007793406225705632254, 0.007844151558772011895, 0.007894896891838391537, 0.007945642224904771178, 0.008047132891037544339, 0.008250114223303045558, 0.008453095555568546776, 0.008859058220099485029, 0.009265020884630421547 ),
 .UNSPECIFIED. ) ;
#7298 = CARTESIAN_POINT ( 'NONE',  ( 149.7200635338602410, 271.3242383773507527, -12.12223662813266500 ) ) ;
#7299 = CARTESIAN_POINT ( 'NONE',  ( 69.98626866712953642, 62.70234947095676148, 13.41362294286624923 ) ) ;
#7300 = ORIENTED_EDGE ( 'NONE', *, *, #3882, .T. ) ;
#7301 = CARTESIAN_POINT ( 'NONE',  ( 102.5829875751790468, 230.0333772461660828, 9.188101187500095079 ) ) ;
#7302 = CARTESIAN_POINT ( 'NONE',  ( 203.6711767524177219, 277.8781691579084736, 15.55577513624845132 ) ) ;
#7303 = CARTESIAN_POINT ( 'NONE',  ( 73.40082382908687464, 69.73317320774677341, -9.891058063621702701 ) ) ;
#7304 = CARTESIAN_POINT ( 'NONE',  ( 181.1220979881137794, 271.7127838054424274, -16.46451683054539927 ) ) ;
#7305 = CARTESIAN_POINT ( 'NONE',  ( 81.41048206884038052, 42.10864841836186656, -7.936452042242466476 ) ) ;
#7306 = VERTEX_POINT ( 'NONE', #76534 ) ;
#7307 = VERTEX_POINT ( 'NONE', #92750 ) ;
#7308 = ORIENTED_EDGE ( 'NONE', *, *, #68211, .T. ) ;
#7309 = CARTESIAN_POINT ( 'NONE',  ( 80.79947158083696479, 47.80592219649970076, 13.19143189947888750 ) ) ;
#7310 = AXIS2_PLACEMENT_3D ( 'NONE', #27249, #66729, #28230 ) ;
#7311 = VERTEX_POINT ( 'NONE', #14718 ) ;
#7312 = CARTESIAN_POINT ( 'NONE',  ( 149.7489224357368869, 277.2657599369866830, -4.201129737586335011 ) ) ;
#7313 = ORIENTED_EDGE ( 'NONE', *, *, #40123, .T. ) ;
#7314 = CARTESIAN_POINT ( 'NONE',  ( 207.7655736232174206, 270.7864657513322300, 3.530742899761726949 ) ) ;
#7315 = EDGE_CURVE ( 'NONE', #21409, #30521, #17866, .T. ) ;
#7316 = DIRECTION ( 'NONE',  ( 0.000000000000000000, 0.000000000000000000, -1.000000000000000000 ) ) ;
#7317 = CARTESIAN_POINT ( 'NONE',  ( 169.3571508527084291, 283.0956279022483955, 12.63651818596384935 ) ) ;
#7318 = CARTESIAN_POINT ( 'NONE',  ( 80.93613592869992601, 42.95327845849681836, -9.503115154567232992 ) ) ;
#7319 = CIRCLE ( 'NONE', #65608, 70.00000000000001421 ) ;
#7320 = CARTESIAN_POINT ( 'NONE',  ( 70.42618839682489806, 68.43364653649702234, -8.625854842549946611 ) ) ;
#7321 = CARTESIAN_POINT ( 'NONE',  ( 79.11723855630626190, 59.11194703662724237, -16.21433712332713029 ) ) ;
#7322 = CARTESIAN_POINT ( 'NONE',  ( 13.89352694080530171, 28.99752408145591076, 5.678558825948277544 ) ) ;
#7323 = CARTESIAN_POINT ( 'NONE',  ( 200.3935147155627305, 278.4751539331289223, -15.53795961942556936 ) ) ;
#7324 = CARTESIAN_POINT ( 'NONE',  ( 80.14478464935454838, 57.78471241749841170, 16.60281329265515637 ) ) ;
#7326 = ORIENTED_EDGE ( 'NONE', *, *, #41107, .T. ) ;
#7325 = CARTESIAN_POINT ( 'NONE',  ( 122.5466773502276254, 234.8927522451417360, -10.00000000000009237 ) ) ;
#7327 = B_SPLINE_CURVE_WITH_KNOTS ( 'NONE', 3,
 ( #29257, #67752, #91088, #44930 ),
 .UNSPECIFIED., .F., .F.,
 ( 4, 4 ),
 ( 0.000000000000000000, 0.0003654356002692110196 ),
 .UNSPECIFIED. ) ;
#7328 = CARTESIAN_POINT ( 'NONE',  ( 202.6551236945213361, 279.6380246773706517, 15.55476940527561425 ) ) ;
#7329 = CARTESIAN_POINT ( 'NONE',  ( 186.6492374970252683, 259.8286487250865662, 2.870770739009044004 ) ) ;
#7330 = CARTESIAN_POINT ( 'NONE',  ( 77.23208049594958879, 49.18074735263096642, -15.33539087807836765 ) ) ;
#7331 = CARTESIAN_POINT ( 'NONE',  ( 68.11396990072299218, 66.09066184265174115, -10.54551009852403709 ) ) ;
#7332 = CARTESIAN_POINT ( 'NONE',  ( 169.7764802368346295, 254.5828642248548874, 11.32100359419826141 ) ) ;
#7333 = CARTESIAN_POINT ( 'NONE',  ( 158.4097777638608875, 281.2458747730524919, 2.072559225148736584 ) ) ;
#7334 = VERTEX_POINT ( 'NONE', #30 ) ;
#7335 = CARTESIAN_POINT ( 'NONE',  ( 155.5849683057210768, 261.1659253309343853, -17.10048217785023539 ) ) ;
#7336 = CARTESIAN_POINT ( 'NONE',  ( -22.72465050930169994, 22.87247442008841958, -10.00000000000000000 ) ) ;
#7337 = CARTESIAN_POINT ( 'NONE',  ( 2.096977440541873516, 182.0177522451419350, 5.000000000000046185 ) ) ;
#7338 = CARTESIAN_POINT ( 'NONE',  ( 193.0018192671613519, 266.8968850134971262, -11.37984971561561842 ) ) ;
#7339 = LINE ( 'NONE', #100068, #27621 ) ;
#7340 = B_SPLINE_CURVE_WITH_KNOTS ( 'NONE', 3,
 ( #95055, #25616, #56501, #87488, #77313, #70191, #23588, #46904, #801, #62586, #26116, #48917, #65599, #26614, #72744, #50399, #87975, #41288, #35199, #4296, #49406, #73223, #80353, #33725, #11923, #96549, #49906, #58002, #57492, #80864, #79853 ),
 .UNSPECIFIED., .F., .F.,
 ( 4, 3, 3, 3, 3, 3, 3, 3, 3, 3, 4 ),
 ( 0.000000000000000000, 0.1333490885032317108, 0.3007194338854392579, 0.4699862290245125918, 0.5844252810809411613, 0.6686540514502808952, 0.7354980260655639146, 0.8028463152565747940, 0.8633854507757208196, 0.9437142632667219200, 1.000000000000000000 ),
 .UNSPECIFIED. ) ;
#7341 = CARTESIAN_POINT ( 'NONE',  ( 203.5339801188816580, 278.1158006978202479, -14.61497198938462105 ) ) ;
#7342 = CARTESIAN_POINT ( 'NONE',  ( 72.04401715163407971, 72.30798015014887881, 0.7277735660157971243 ) ) ;
#7343 = EDGE_CURVE ( 'NONE', #19698, #52344, #15704, .T. ) ;
#7344 = CARTESIAN_POINT ( 'NONE',  ( 162.1569020246023456, 250.8293869144198140, -12.73294256043488026 ) ) ;
#7345 = CARTESIAN_POINT ( 'NONE',  ( -10.75808714510939090, 164.5958772461660544, -9.188101187500095079 ) ) ;
#7346 = CARTESIAN_POINT ( 'NONE',  ( -70.00000000000000000, 15.00000000000000000, 59.99999999999999289 ) ) ;
#7347 = ORIENTED_EDGE ( 'NONE', *, *, #70785, .F. ) ;
#7348 = VERTEX_POINT ( 'NONE', #39001 ) ;
#7349 = CARTESIAN_POINT ( 'NONE',  ( 165.7655117394099591, 246.1853102806505831, -2.777750405961522784 ) ) ;
#7350 = DIRECTION ( 'NONE',  ( -1.000000000000000000, -1.156482317317871331E-15, 0.000000000000000000 ) ) ;
#7351 = CYLINDRICAL_SURFACE ( 'NONE', #11418, 17.82106496071139645 ) ;
#7352 = VECTOR ( 'NONE', #44199, 1000.000000000000000 ) ;
#7353 = LINE ( 'NONE', #67669, #95506 ) ;
#7354 = CARTESIAN_POINT ( 'NONE',  ( 158.4485968073939546, 275.2084588272041401, -13.86993402366507944 ) ) ;
#7355 = CARTESIAN_POINT ( 'NONE',  ( 84.44632881057094664, 46.78574307426487167, 10.85411661781247084 ) ) ;
#7356 = CARTESIAN_POINT ( 'NONE',  ( 150.2414568861867679, 276.5756577973505728, 3.692317353432758242 ) ) ;
#7357 = CARTESIAN_POINT ( 'NONE',  ( 19.71535529843806245, 176.0643266524160424, 9.188101187500095079 ) ) ;
#7358 = CARTESIAN_POINT ( 'NONE',  ( 114.4904897814500515, 249.1589784336661069, -6.496448406907675876E-16 ) ) ;
#7359 = FACE_OUTER_BOUND ( 'NONE', #18145, .T. ) ;
#7360 = CARTESIAN_POINT ( 'NONE',  ( 196.2076153567640517, 275.2112971549272515, 16.01702815084858855 ) ) ;
#7361 = CARTESIAN_POINT ( 'NONE',  ( 153.5108272444703630, 274.2076890947117818, -12.10491928328822020 ) ) ;
#7362 = CARTESIAN_POINT ( 'NONE',  ( 178.5305822085327350, 283.8616835467783517, -14.84070646491336554 ) ) ;
#7363 = CARTESIAN_POINT ( 'NONE',  ( 190.5307517086160942, 299.7706353115473235, -5.301913143154168395 ) ) ;
#7364 = CARTESIAN_POINT ( 'NONE',  ( 80.64483776220907885, 57.31469717126433494, -16.23318395240539758 ) ) ;
#7365 = CARTESIAN_POINT ( 'NONE',  ( 68.52821507787726318, 64.25720321475604635, -12.41134622814902322 ) ) ;
#7366 = CARTESIAN_POINT ( 'NONE',  ( 207.2337123599961899, 271.7076764818092443, -5.443417788256701861 ) ) ;
#7367 = VECTOR ( 'NONE', #16895, 1000.000000000000114 ) ;
#7368 = CARTESIAN_POINT ( 'NONE',  ( 15.82905546192370494, 46.33330469044422983, 59.99999999999999289 ) ) ;
#7369 = CARTESIAN_POINT ( 'NONE',  ( 189.2674249387218595, 262.5240697966969492, 8.133003587096190756 ) ) ;
#7370 = CARTESIAN_POINT ( 'NONE',  ( 168.2540853406581789, 278.3014265215951468, 14.24901084982592891 ) ) ;
#7371 = CARTESIAN_POINT ( 'NONE',  ( 175.4112849191630232, 256.5165010529896676, -10.85204326945974174 ) ) ;
#7372 = CARTESIAN_POINT ( 'NONE',  ( 68.99418107762870989, 68.85582864506679357, 6.521622189437183081 ) ) ;
#7373 = DIRECTION ( 'NONE',  ( -0.5280678506503699854, -0.8492021815265776707, 0.000000000000000000 ) ) ;
#7374 = CARTESIAN_POINT ( 'NONE',  ( 181.0085414047549932, 266.3579488787440255, -14.72432788045776242 ) ) ;
#7375 = ORIENTED_EDGE ( 'NONE', *, *, #55972, .T. ) ;
#7376 = CIRCLE ( 'NONE', #76942, 70.00000000000001421 ) ;
#7377 = CARTESIAN_POINT ( 'NONE',  ( -67.91103796225580425, 44.10201266000169085, -10.00000000000000000 ) ) ;
#7378 = CARTESIAN_POINT ( 'NONE',  ( 185.0762662215304601, 269.6689080139000225, 15.62688583476976056 ) ) ;
#7379 = CARTESIAN_POINT ( 'NONE',  ( 88.45577462806285496, 228.0024278399160664, -9.188101187500093303 ) ) ;
#7380 = CARTESIAN_POINT ( 'NONE',  ( 11.76515913632831101, 28.83396525600389282, -2.839279412974133887 ) ) ;
#7381 = CARTESIAN_POINT ( 'NONE',  ( 71.82426268295279215, 61.16778308377749340, -15.19677902312525219 ) ) ;
#7382 = CARTESIAN_POINT ( 'NONE',  ( 159.0906380018002153, 259.2649656523443582, -17.57712761084927067 ) ) ;
#7384 = CARTESIAN_POINT ( 'NONE',  ( 195.2852648346649005, 278.9764887875277850, 16.29283862267904226 ) ) ;
#7383 = DIRECTION ( 'NONE',  ( -0.5951734788405994570, 0.8035972437015812542, 0.000000000000000000 ) ) ;
#7385 = CARTESIAN_POINT ( 'NONE',  ( -22.42236680055709641, 157.8615022471902591, 0.000000000000000000 ) ) ;
#7386 = FACE_OUTER_BOUND ( 'NONE', #4057, .T. ) ;
#7387 = CARTESIAN_POINT ( 'NONE',  ( 149.8377514179171328, 271.8685197739567343, -11.50488653483219537 ) ) ;
#7388 = CARTESIAN_POINT ( 'NONE',  ( 40.83172133312034191, 29.28920272979929962, -7.433330006724141015 ) ) ;
#7389 = LINE ( 'NONE', #24091, #67747 ) ;
#7390 = FACE_BOUND ( 'NONE', #72110, .T. ) ;
#7391 = VERTEX_POINT ( 'NONE', #69906 ) ;
#7392 = CARTESIAN_POINT ( 'NONE',  ( 27.58635055662477953, 24.43085787977765122, -9.188101187500008038 ) ) ;
#7393 = CARTESIAN_POINT ( 'NONE',  ( 178.3972326700113911, 280.2571014150069004, 15.75398658722560974 ) ) ;
#7394 = CARTESIAN_POINT ( 'NONE',  ( 199.1702776998127433, 269.7223802865422613, 9.247749995336496553 ) ) ;
#7395 = CARTESIAN_POINT ( 'NONE',  ( 196.6288634187112052, 290.0758136547079289, -16.31544900032282186 ) ) ;
#7396 = ADVANCED_FACE ( 'NONE', ( #521 ), #31408, .T. ) ;
#7397 = DIRECTION ( 'NONE',  ( -1.000000000000000000, 0.000000000000000000, 0.000000000000000000 ) ) ;
#7398 = DIRECTION ( 'NONE',  ( -0.9762722099447388446, -0.2165469281463391626, 0.000000000000000000 ) ) ;
#7399 = CARTESIAN_POINT ( 'NONE',  ( 183.6390766470569247, 264.5367329039647757, -13.38022241395614387 ) ) ;
#7400 = EDGE_CURVE ( 'NONE', #76991, #97421, #66683, .T. ) ;
#7401 = CARTESIAN_POINT ( 'NONE',  ( 172.2491325584012998, 253.6515925324379737, -8.857966409642921590 ) ) ;
#7402 = CARTESIAN_POINT ( 'NONE',  ( 152.9920137376499838, 265.6570543845515431, 16.15798175643282164 ) ) ;
#7403 = ORIENTED_EDGE ( 'NONE', *, *, #58194, .F. ) ;
#7404 = CARTESIAN_POINT ( 'NONE',  ( 79.22511366827423274, 47.14223421634689970, -13.88362136263801005 ) ) ;
#7405 = ADVANCED_FACE ( 'NONE', ( #80562 ), #18227, .F. ) ;
#7406 = CARTESIAN_POINT ( 'NONE',  ( 30.33837380989695731, 32.91421378149920685, 9.188101187500008038 ) ) ;
#7407 = VERTEX_POINT ( 'NONE', #94749 ) ;
#7408 = CARTESIAN_POINT ( 'NONE',  ( 166.8517212214031815, 249.4051957966311193, 6.977118993877414965 ) ) ;
#7409 = EDGE_CURVE ( 'NONE', #27141, #91686, #64317, .T. ) ;
#7410 = CARTESIAN_POINT ( 'NONE',  ( 86.76627553996233644, 43.48886326763260968, 2.108659042064822575 ) ) ;
#7411 = VERTEX_POINT ( 'NONE', #87195 ) ;
#7412 = CARTESIAN_POINT ( 'NONE',  ( 86.32721218574307898, 47.55264674982593220, -11.12316258729872054 ) ) ;
#7413 = DIRECTION ( 'NONE',  ( 0.3535533905932811694, -0.6123724356958052395, 0.7071067811865344721 ) ) ;
#7414 = CARTESIAN_POINT ( 'NONE',  ( 84.71425524834847920, 50.25098136614051469, 13.83365903171529077 ) ) ;
#7415 = CARTESIAN_POINT ( 'NONE',  ( 192.9271913386342021, 296.4872977703604420, -11.97251109041730288 ) ) ;
#7416 = CARTESIAN_POINT ( 'NONE',  ( 200.6985908945154335, 283.0268388936558495, -17.74173253065502820 ) ) ;
#7417 = CARTESIAN_POINT ( 'NONE',  ( -27.42236680055714260, 166.5217562850347406, 1.224646799147364892E-15 ) ) ;
#7418 = VECTOR ( 'NONE', #20191, 1000.000000000000000 ) ;
#7419 = CARTESIAN_POINT ( 'NONE',  ( 110.4458243891416487, 246.1199935810941213, 2.679491924311251605 ) ) ;
#7420 = CARTESIAN_POINT ( 'NONE',  ( 81.54078422002766047, 55.47956193386177404, -16.32023236213573014 ) ) ;
#7421 = CARTESIAN_POINT ( 'NONE',  ( 154.3830968479286980, 271.8928371781024680, -14.51477723473457360 ) ) ;
#7422 = ORIENTED_EDGE ( 'NONE', *, *, #31757, .F. ) ;
#7424 = CIRCLE ( 'NONE', #73826, 11.89249999999999652 ) ;
#7423 = CARTESIAN_POINT ( 'NONE',  ( -22.42236680055709641, 157.8615022471902591, 0.000000000000000000 ) ) ;
#7425 = VERTEX_POINT ( 'NONE', #97617 ) ;
#7426 = ORIENTED_EDGE ( 'NONE', *, *, #65463, .F. ) ;
#7427 = CARTESIAN_POINT ( 'NONE',  ( 172.5528256599575911, 270.8946351329052504, 16.43625532445414805 ) ) ;
#7428 = CARTESIAN_POINT ( 'NONE',  ( 84.39448865303761238, 50.06170295690048988, 13.83095091856771219 ) ) ;
#7430 = CARTESIAN_POINT ( 'NONE',  ( 185.2570508126727873, 282.0811717828997303, -17.42469797758589678 ) ) ;
#7429 = CARTESIAN_POINT ( 'NONE',  ( 170.7847687409972366, 255.2762072239008830, -11.40120098929249437 ) ) ;
#7431 = CARTESIAN_POINT ( 'NONE',  ( 206.2849804695184446, 273.3509283188774930, -9.687080623179198824 ) ) ;
#7432 = CARTESIAN_POINT ( 'NONE',  ( 197.9901163037401943, 272.1418500761980681, -13.83221381771805625 ) ) ;
#7433 = CARTESIAN_POINT ( 'NONE',  ( 72.26813344353081447, 61.62913406889816059, -14.61747620878596265 ) ) ;
#7434 = CARTESIAN_POINT ( 'NONE',  ( 82.51358517225706635, 41.00440080157959954, 1.051676170051975223 ) ) ;
#7435 = CARTESIAN_POINT ( 'NONE',  ( 171.6432221199900141, 250.7645099467145542, -5.701615499911769191 ) ) ;
#7436 = CARTESIAN_POINT ( 'NONE',  ( 77.02263550477385934, 63.85671778288190836, -15.30752586418454086 ) ) ;
#7437 = CARTESIAN_POINT ( 'NONE',  ( 178.0376065834567498, 255.4657367285703060, 5.065382276933755534 ) ) ;
#7438 = CARTESIAN_POINT ( 'NONE',  ( 111.8924135700967355, 247.6589784336661069, -6.496448406907675876E-16 ) ) ;
#7439 = ORIENTED_EDGE ( 'NONE', *, *, #88245, .T. ) ;
#7440 = CARTESIAN_POINT ( 'NONE',  ( 186.6478515376321070, 262.8385383458236788, -9.776049215535964620 ) ) ;
#7441 = CARTESIAN_POINT ( 'NONE',  ( 41.62797693021462209, 26.96004757982093381, -5.678558825948276656 ) ) ;
#7442 = CARTESIAN_POINT ( 'NONE',  ( 187.9511160036650779, 273.8878269306266020, 16.63997191726063463 ) ) ;
#7443 = VERTEX_POINT ( 'NONE', #28184 ) ;
#7444 = VERTEX_POINT ( 'NONE', #10123 ) ;
#7445 = CYLINDRICAL_SURFACE ( 'NONE', #83823, 6.749999999999988454 ) ;
#7446 = CARTESIAN_POINT ( 'NONE',  ( 72.22311968498431156, 63.76148163533759572, -13.58264511429491783 ) ) ;
#7447 = DIRECTION ( 'NONE',  ( -1.000000000000000000, 0.000000000000000000, 0.000000000000000000 ) ) ;
#7448 = CARTESIAN_POINT ( 'NONE',  ( 192.1298366743677946, 297.8683565605218746, 11.31374600872841008 ) ) ;
#7449 = CARTESIAN_POINT ( 'NONE',  ( 28.51231065420501309, 32.16454794089043645, -10.00000000000000355 ) ) ;
#7450 = CARTESIAN_POINT ( 'NONE',  ( 74.06060638490031067, 55.49390267324601922, -16.11553875424677074 ) ) ;
#7451 = ORIENTED_EDGE ( 'NONE', *, *, #90040, .T. ) ;
#7452 = AXIS2_PLACEMENT_3D ( 'NONE', #81552, #20225, #82062 ) ;
#7453 = LINE ( 'NONE', #77367, #52834 ) ;
#7454 = ORIENTED_EDGE ( 'NONE', *, *, #97583, .T. ) ;
#7455 = CARTESIAN_POINT ( 'NONE',  ( 79.22526226284777806, 49.23273016502245980, 14.90489237802606759 ) ) ;
#7456 = DIRECTION ( 'NONE',  ( -0.8660254037844378194, -0.5000000000000014433, -0.000000000000000000 ) ) ;
#7457 = EDGE_LOOP ( 'NONE', ( #68987, #39055, #19288, #64040 ) ) ;
#7458 = CARTESIAN_POINT ( 'NONE',  ( 188.5893119661470223, 266.4960058560010339, -11.84220618477010767 ) ) ;
#7459 = CARTESIAN_POINT ( 'NONE',  ( 82.93017357788667709, 175.3855496052738374, 36.50000000000000000 ) ) ;
#7460 = DIRECTION ( 'NONE',  ( -0.000000000000000000, -0.000000000000000000, -1.000000000000000000 ) ) ;
#7461 = ADVANCED_FACE ( 'NONE', ( #17728, #33939 ), #72445, .T. ) ;
#7462 = CARTESIAN_POINT ( 'NONE',  ( 81.32600941128136185, 42.90402669303311711, 8.279988871130893102 ) ) ;
#7464 = DIRECTION ( 'NONE',  ( 0.4999999999999998890, -0.8660254037844385966, 0.000000000000000000 ) ) ;
#7463 = CARTESIAN_POINT ( 'NONE',  ( 184.1240780222136095, 289.0015729834078684, -14.54488561116068901 ) ) ;
#7465 = CARTESIAN_POINT ( 'NONE',  ( 201.4066285247549786, 281.8004817444100354, -17.79749223817309201 ) ) ;
#7466 = EDGE_LOOP ( 'NONE', ( #16361, #29232, #8163, #52616 ) ) ;
#7467 = CARTESIAN_POINT ( 'NONE',  ( 190.8907028847385448, 300.0145992415348815, -5.421341690443150618 ) ) ;
#7468 = CARTESIAN_POINT ( 'NONE',  ( 192.1379539184286216, 266.4068991655999525, -11.89392551111776619 ) ) ;
#7469 = CARTESIAN_POINT ( 'NONE',  ( 82.25663186038693198, 41.25091070164440055, -3.462110524831779834 ) ) ;
#7470 = CARTESIAN_POINT ( 'NONE',  ( 192.8090185325462471, 271.7505329995509555, -14.77105383832748942 ) ) ;
#7471 = CARTESIAN_POINT ( 'NONE',  ( 9.458193372709645885, 176.2677522451418497, 10.00000000000009592 ) ) ;
#7472 = CARTESIAN_POINT ( 'NONE',  ( 82.66671967738665217, 42.53264105941079265, 6.324155599994208288 ) ) ;
#7473 = CARTESIAN_POINT ( 'NONE',  ( 22.51478983128357925, 15.12755873383625982, -6.180339887498949025 ) ) ;
#7474 = CARTESIAN_POINT ( 'NONE',  ( 192.2414585986055897, 284.0409920799691008, -16.66054451170961315 ) ) ;
#7475 = CARTESIAN_POINT ( 'NONE',  ( 82.57676729861134390, 54.19068042909008653, -15.92587557605580706 ) ) ;
#7476 = CARTESIAN_POINT ( 'NONE',  ( 67.72511797709034909, 222.1589784336661637, -6.496448406907675876E-16 ) ) ;
#7477 = CARTESIAN_POINT ( 'NONE',  ( 28.60096323907606219, 193.9865022471902876, 10.00000000000009415 ) ) ;
#7478 = CARTESIAN_POINT ( 'NONE',  ( 147.5749398328735822, 275.0397016159798227, -4.620786157167191099 ) ) ;
#7479 = CARTESIAN_POINT ( 'NONE',  ( 65.92723761088207368, 68.94945291059252668, -2.624861928015914003 ) ) ;
#7480 = ADVANCED_FACE ( 'NONE', ( #24809 ), #34414, .F. ) ;
#7481 = B_SPLINE_CURVE_WITH_KNOTS ( 'NONE', 3,
 ( #38563, #14776, #30969, #70469 ),
 .UNSPECIFIED., .F., .F.,
 ( 4, 4 ),
 ( 0.03663086090994036731, 0.04529359754877385069 ),
 .UNSPECIFIED. ) ;
#7482 = CARTESIAN_POINT ( 'NONE',  ( 78.72787672744944132, 47.58481813695765084, 14.26461805045499531 ) ) ;
#7483 = VECTOR ( 'NONE', #19716, 1000.000000000000000 ) ;
#7484 = CARTESIAN_POINT ( 'NONE',  ( 207.7666684749232786, 270.7845694125510931, -6.630926507062123498 ) ) ;
#7485 = CARTESIAN_POINT ( 'NONE',  ( -19.65312891409030271, 93.06504152958497400, -10.00000000000000888 ) ) ;
#7486 = VECTOR ( 'NONE', #39821, 1000.000000000000000 ) ;
#7488 = CARTESIAN_POINT ( 'NONE',  ( 76.25812641337097375, 51.35648307871889529, 15.62532910699416000 ) ) ;
#7487 = CARTESIAN_POINT ( 'NONE',  ( 73.49482902488119862, 69.19712283778764572, -10.00323161215957768 ) ) ;
#7489 = CARTESIAN_POINT ( 'NONE',  ( 144.6270795744234476, 268.7413018095040798, -2.761272660171008000E-15 ) ) ;
#7490 = PLANE ( 'NONE',  #24890 ) ;
#7491 = CARTESIAN_POINT ( 'NONE',  ( 164.7073188963636028, 245.3655506234856034, -4.606661621890939529 ) ) ;
#7492 = CARTESIAN_POINT ( 'NONE',  ( 157.3025066944120454, 258.1910615777721887, 18.21299529665260053 ) ) ;
#7493 = CARTESIAN_POINT ( 'NONE',  ( -19.92236680055706088, 153.5313752282680184, 0.000000000000000000 ) ) ;
#7494 = CARTESIAN_POINT ( 'NONE',  ( 47.75258065019424691, 204.5024278399160949, 9.188101187500095079 ) ) ;
#7495 = CARTESIAN_POINT ( 'NONE',  ( 163.9488516144422192, 247.0953858819488005, -6.080757577568762784 ) ) ;
#7496 = CARTESIAN_POINT ( 'NONE',  ( -19.65312891409030271, 93.06504152958497400, -59.99999999999999289 ) ) ;
#7497 = CYLINDRICAL_SURFACE ( 'NONE', #30383, 17.82106496071139645 ) ;
#7498 = CARTESIAN_POINT ( 'NONE',  ( 144.9642793207625004, 248.3768266524159856, -9.188101187500091527 ) ) ;
#7499 = CYLINDRICAL_SURFACE ( 'NONE', #2118, 10.00000000000010658 ) ;
#7500 = CARTESIAN_POINT ( 'NONE',  ( 200.2187516388992492, 271.0431823872724522, -11.39384425366991493 ) ) ;
#7501 = CARTESIAN_POINT ( 'NONE',  ( 21.85012855468117721, 24.56628583063841376, 9.188101187500006262 ) ) ;
#7502 = VECTOR ( 'NONE', #62413, 1000.000000000000000 ) ;
#7503 = CARTESIAN_POINT ( 'NONE',  ( 151.1126408083691501, 268.9122237844355254, -15.82705194100464396 ) ) ;
#7504 = CARTESIAN_POINT ( 'NONE',  ( 146.8358616138309571, 276.3198226421291679, 4.054088818585255716 ) ) ;
#7505 = CARTESIAN_POINT ( 'NONE',  ( 9.796739006517501736, 23.84336893147754566, -7.433330006724137462 ) ) ;
#7506 = CARTESIAN_POINT ( 'NONE',  ( 56.95410056540391253, 209.8149278399160949, -9.188101187500095079 ) ) ;
#7507 = CARTESIAN_POINT ( 'NONE',  ( 76.88515868761567162, 63.85673109229074385, 14.90669629514164463 ) ) ;
#7508 = CARTESIAN_POINT ( 'NONE',  ( 175.7685826524176491, 291.0674233232674624, 2.543747227769448394 ) ) ;
#7509 = CARTESIAN_POINT ( 'NONE',  ( 198.3150362131025588, 287.1552767044814800, 18.53472937702030521 ) ) ;
#7510 = DIRECTION ( 'NONE',  ( 0.9919084036772433111, -0.1269555777209603609, 0.000000000000000000 ) ) ;
#7511 = CARTESIAN_POINT ( 'NONE',  ( 201.4689129737137989, 281.6926019142917994, 17.66990927715608706 ) ) ;
#7512 = EDGE_CURVE ( 'NONE', #51824, #20349, #95241, .T. ) ;
#7513 = B_SPLINE_CURVE_WITH_KNOTS ( 'NONE', 3,
 ( #68668, #53467, #24073, #52978, #84420, #68175, #77800, #46354, #14966, #69169, #6393, #54966, #93003, #99593, #77278, #70161, #23556, #60558 ),
 .UNSPECIFIED., .F., .F.,
 ( 4, 2, 2, 2, 2, 2, 2, 2, 4 ),
 ( 0.002569504393709426404, 0.002648854729461323342, 0.002728205065213220280, 0.002807555400965117652, 0.002886905736717014590, 0.003045606408220883927, 0.003204307079724752830, 0.003839109765740250126, 0.005108715137771275075 ),
 .UNSPECIFIED. ) ;
#7514 = AXIS2_PLACEMENT_3D ( 'NONE', #60263, #38468, #93213 ) ;
#7515 = CARTESIAN_POINT ( 'NONE',  ( 78.88977525980774885, 55.53746465279655808, -16.10141863661490191 ) ) ;
#7516 = CARTESIAN_POINT ( 'NONE',  ( 87.78256729009754622, 45.12882416216076820, -6.783508070075447982 ) ) ;
#7517 = CARTESIAN_POINT ( 'NONE',  ( 109.6465072765698636, 224.1115022471901739, -5.000000000000041744 ) ) ;
#7518 = CARTESIAN_POINT ( 'NONE',  ( 161.0952649348064938, 251.6218116045831437, 13.81854265722852482 ) ) ;
#7519 = CARTESIAN_POINT ( 'NONE',  ( 207.0548180518391916, 272.0175305127218053, 7.721676452263806389 ) ) ;
#7520 = ORIENTED_EDGE ( 'NONE', *, *, #20042, .F. ) ;
#7521 = CARTESIAN_POINT ( 'NONE',  ( 76.94662761810361928, 49.67608497600890871, 15.05378093682414509 ) ) ;
#7522 = CARTESIAN_POINT ( 'NONE',  ( 82.66218641157266234, 53.85062555766313608, 15.82228755104997120 ) ) ;
#7523 = ORIENTED_EDGE ( 'NONE', *, *, #37488, .T. ) ;
#7524 = EDGE_CURVE ( 'NONE', #39339, #33343, #52976, .T. ) ;
#7525 = CARTESIAN_POINT ( 'NONE',  ( 159.8946522441011382, 253.7013337850969492, -16.68230890105693121 ) ) ;
#7526 = CARTESIAN_POINT ( 'NONE',  ( 186.8357760858314975, 276.5851586346784075, -17.24064928530544094 ) ) ;
#7527 = CARTESIAN_POINT ( 'NONE',  ( -17.42236680055705023, 149.2012482093457777, 0.000000000000000000 ) ) ;
#7528 = EDGE_CURVE ( 'NONE', #83021, #81006, #13504, .T. ) ;
#7529 = ORIENTED_EDGE ( 'NONE', *, *, #61826, .F. ) ;
#7530 = ORIENTED_EDGE ( 'NONE', *, *, #62985, .F. ) ;
#7531 = CARTESIAN_POINT ( 'NONE',  ( 207.6918009085542849, 270.9142438413412037, 7.009114282139513818 ) ) ;
#7532 = CARTESIAN_POINT ( 'NONE',  ( 147.9311236323648870, 274.4227731784279172, -7.799459659034405412 ) ) ;
#7533 = ADVANCED_FACE ( 'NONE', ( #23055 ), #47726, .F. ) ;
#7534 = CARTESIAN_POINT ( 'NONE',  ( 50.06890205215325551, 99.29708757740750968, 10.00000000000000000 ) ) ;
#7535 = FACE_OUTER_BOUND ( 'NONE', #52527, .T. ) ;
#7536 = EDGE_LOOP ( 'NONE', ( #43758, #94952, #84107, #75164 ) ) ;
#7537 = CARTESIAN_POINT ( 'NONE',  ( 22.95008440877049338, 15.11110640527292226, -2.839279412974138328 ) ) ;
#7538 = CARTESIAN_POINT ( 'NONE',  ( 75.71249384252782022, 58.31751109039055336, 16.01915597449171358 ) ) ;
#7539 = CARTESIAN_POINT ( 'NONE',  ( 188.1018771210319471, 260.4230313274653099, 6.875771660441075461 ) ) ;
#7540 = CARTESIAN_POINT ( 'NONE',  ( -22.42236680055709641, 157.8615022471902591, 0.000000000000000000 ) ) ;
#7541 = ORIENTED_EDGE ( 'NONE', *, *, #93952, .F. ) ;
#7542 = DIRECTION ( 'NONE',  ( 0.7071067811865474617, 0.000000000000000000, 0.7071067811865474617 ) ) ;
#7543 = CARTESIAN_POINT ( 'NONE',  ( 206.4640281786353171, 273.0408085897082060, -10.81921452789957883 ) ) ;
#7544 = VERTEX_POINT ( 'NONE', #94013 ) ;
#7545 = CARTESIAN_POINT ( 'NONE',  ( 174.6338837768408609, 286.4401551613050856, 11.66525039651988749 ) ) ;
#7547 = CARTESIAN_POINT ( 'NONE',  ( 68.29626403325076467, 65.68998705335020816, -10.32719566005510181 ) ) ;
#7546 = CARTESIAN_POINT ( 'NONE',  ( 159.2472135755374154, 282.4118482373870052, -3.281722807136270958 ) ) ;
#7548 = CARTESIAN_POINT ( 'NONE',  ( 162.6257765080958677, 248.9708877980734485, -10.42859054881151160 ) ) ;
#7549 = CARTESIAN_POINT ( 'NONE',  ( 163.7729086741176161, 246.9839966035275438, 6.099406794390714204 ) ) ;
#7550 = CARTESIAN_POINT ( 'NONE',  ( 188.5838923881401001, 295.0354966342055718, -11.12588321966210714 ) ) ;
#7551 = CARTESIAN_POINT ( 'NONE',  ( 164.3625597711517230, 265.6729452914248668, -17.82104740451561753 ) ) ;
#7553 = CARTESIAN_POINT ( 'NONE',  ( 135.5998589986957370, 261.3464784336661637, 1.353441290958777525E-15 ) ) ;
#7552 = B_SPLINE_CURVE_WITH_KNOTS ( 'NONE', 3,
 ( #7354, #77779, #100081, #23539 ),
 .UNSPECIFIED., .F., .F.,
 ( 4, 4 ),
 ( 0.008629964147991740775, 0.01453130706412321220 ),
 .UNSPECIFIED. ) ;
#7554 = DIRECTION ( 'NONE',  ( 1.156482317317871331E-15, -1.000000000000000000, 0.000000000000000000 ) ) ;
#7555 = CARTESIAN_POINT ( 'NONE',  ( 178.9693536223838635, 258.2551845487027435, 9.752734003342059310 ) ) ;
#7556 = CARTESIAN_POINT ( 'NONE',  ( 74.81622161422296813, 207.8768266524159856, -9.188101187500091527 ) ) ;
#7557 = ORIENTED_EDGE ( 'NONE', *, *, #35687, .T. ) ;
#7558 = DIRECTION ( 'NONE',  ( 1.156482317317871331E-15, -1.000000000000000000, 0.000000000000000000 ) ) ;
#7559 = CARTESIAN_POINT ( 'NONE',  ( 13.35896364390118052, 31.21091486745859811, -1.111400068045478839E-16 ) ) ;
#7560 = CARTESIAN_POINT ( 'NONE',  ( 181.4954090331713417, 255.0423029034424189, 0.9094182891644410072 ) ) ;
#7561 = AXIS2_PLACEMENT_3D ( 'NONE', #72825, #3418, #34777 ) ;
#7562 = ORIENTED_EDGE ( 'NONE', *, *, #81631, .T. ) ;
#7563 = CARTESIAN_POINT ( 'NONE',  ( -19.83262083840137180, 133.3759306620404459, -30.52142883766495629 ) ) ;
#7564 = ORIENTED_EDGE ( 'NONE', *, *, #90388, .F. ) ;
#7565 = ORIENTED_EDGE ( 'NONE', *, *, #15260, .F. ) ;
#7566 = CARTESIAN_POINT ( 'NONE',  ( 90.33589715100974615, 211.4155109091896065, 2.679491924311254714 ) ) ;
#7567 = CARTESIAN_POINT ( 'NONE',  ( 67.15984093255737264, 67.73264523994713215, 6.578533426557070740 ) ) ;
#7568 = CARTESIAN_POINT ( 'NONE',  ( 197.9225324884813801, 286.9052520424737622, 16.93390111457149416 ) ) ;
#7570 = B_SPLINE_SURFACE_WITH_KNOTS ( 'NONE', 3, 1, ( 
 ( #88917, #30396 ),
 ( #22298, #67024 ),
 ( #84634, #29898 ),
 ( #92251, #14699 ),
 ( #53198, #15685 ),
 ( #22801, #15175 ),
 ( #61288, #78009 ),
 ( #92730, #84153 ),
 ( #82291, #97951 ),
 ( #53680, #76510 ),
 ( #68884, #45582 ),
 ( #58907, #46077 ),
 ( #12, #38981 ),
 ( #93227, #76988 ),
 ( #7594, #7093 ),
 ( #23788, #91735 ),
 ( #5241, #499 ),
 ( #61784, #16197 ),
 ( #46579, #37975 ),
 ( #38482, #74664 ),
 ( #36121, #99811 ),
 ( #8601, #62271 ),
 ( #69396, #69887 ),
 ( #30896, #23281 ),
 ( #54170, #31387 ),
 ( #77516, #60770 ),
 ( #54673, #85137 ),
 ( #1000, #8107 ),
 ( #12862, #85657 ),
 ( #47089, #39466 ),
 ( #43721, #51322 ),
 ( #70391, #89876 ),
 ( #20451, #94235 ),
 ( #94729, #33396 ) ),
 .UNSPECIFIED., .T., .F., .F.,
 ( 4, 2, 2, 2, 2, 2, 2, 2, 2, 2, 2, 2, 2, 2, 2, 2, 4 ),
 ( 2, 2 ),
 ( 0.000000000000000000, 0.06250000000000000000, 0.1250000000000000000, 0.1875000000000000000, 0.2500000000000000000, 0.3125000000000000000, 0.3750000000000000000, 0.4375000000000000000, 0.5000000000000000000, 0.5625000000000000000, 0.6250000000000000000, 0.6875000000000000000, 0.7500000000000000000, 0.8125000000000000000, 0.8750000000000000000, 0.9375000000000000000, 1.000000000000000000 ),
 ( 0.000000000000000000, 1.000000000000000000 ),
 .UNSPECIFIED. ) ;
#7569 = CARTESIAN_POINT ( 'NONE',  ( 191.4852287632733123, 298.9848502134979071, -9.870565261052552941 ) ) ;
#7571 = SHAPE_REPRESENTATION ( 'Screw-Connected Movable Jaw', ( #68784 ), #31602 ) ;
#7572 = CARTESIAN_POINT ( 'NONE',  ( 80.97708524682441578, 55.98081928642064753, 16.09453298904065832 ) ) ;
#7573 = CARTESIAN_POINT ( 'NONE',  ( 193.7706395672514645, 295.0264025848412075, 15.16938698680137065 ) ) ;
#7574 = VECTOR ( 'NONE', #79278, 1000.000000000000000 ) ;
#7575 = CARTESIAN_POINT ( 'NONE',  ( 71.72731785887494027, 67.47519123564113386, 10.61382998831304114 ) ) ;
#7576 = CARTESIAN_POINT ( 'NONE',  ( 81.44681538588882574, 208.6423013555409796, -4.594050593750043987 ) ) ;
#7577 = ORIENTED_EDGE ( 'NONE', *, *, #94957, .T. ) ;
#7578 = VERTEX_POINT ( 'NONE', #71701 ) ;
#7579 = CARTESIAN_POINT ( 'NONE',  ( -0.2492734796364602656, 27.10516647459198225, 10.00000000000000000 ) ) ;
#7580 = ORIENTED_EDGE ( 'NONE', *, *, #96113, .F. ) ;
#7581 = CARTESIAN_POINT ( 'NONE',  ( 76.38099514367294773, 51.62635831307756007, -15.66874856699700835 ) ) ;
#7582 = CARTESIAN_POINT ( 'NONE',  ( 76.27580996045810480, 65.11309384637550579, -14.21297909825325156 ) ) ;
#7583 = EDGE_CURVE ( 'NONE', #14234, #64644, #73493, .T. ) ;
#7585 = AXIS2_PLACEMENT_3D ( 'NONE', #29665, #90525, #21096 ) ;
#7584 = CARTESIAN_POINT ( 'NONE',  ( 165.3478801264585627, 285.2307890726268056, 0.5090311687081423564 ) ) ;
#7586 = PLANE ( 'NONE',  #73644 ) ;
#7587 = CARTESIAN_POINT ( 'NONE',  ( 99.70756906128829655, 216.8262482093457493, 3.021315404115420679E-15 ) ) ;
#7588 = ORIENTED_EDGE ( 'NONE', *, *, #22472, .F. ) ;
#7589 = AXIS2_PLACEMENT_3D ( 'NONE', #91727, #61779, #45091 ) ;
#7590 = CARTESIAN_POINT ( 'NONE',  ( 82.05742212450444129, 43.66019292712455524, -8.741533095782198615 ) ) ;
#7591 = DIRECTION ( 'NONE',  ( -0.1039558454088829048, 0.1800568059919617214, 0.9781476007338041345 ) ) ;
#7592 = EDGE_CURVE ( 'NONE', #47832, #42238, #49255, .T. ) ;
#7593 = CARTESIAN_POINT ( 'NONE',  ( 38.12578301810894033, 22.41603393254328935, -1.583844403245396437 ) ) ;
#7594 = CARTESIAN_POINT ( 'NONE',  ( 201.1679199471075492, 282.2139371290980989, -16.62385308864941535 ) ) ;
#7595 = VECTOR ( 'NONE', #44915, 1000.000000000000114 ) ;
#7596 = CARTESIAN_POINT ( 'NONE',  ( 72.62753967730402849, 70.91775434214520146, 7.625672695449478233 ) ) ;
#7597 = CARTESIAN_POINT ( 'NONE',  ( 74.10896984709266633, 66.64336536303099479, -12.55719438977912894 ) ) ;
#7598 = ORIENTED_EDGE ( 'NONE', *, *, #21938, .T. ) ;
#7599 = CARTESIAN_POINT ( 'NONE',  ( 197.7849526899220223, 266.3861572259672243, 4.467793449146438611 ) ) ;
#7600 = CARTESIAN_POINT ( 'NONE',  ( 181.4735074999749145, 292.1586133693310785, 10.55809797880889001 ) ) ;
#7601 = CARTESIAN_POINT ( 'NONE',  ( 82.22237228838635303, 40.83607612262022002, 1.050915814309854479 ) ) ;
#7602 = CARTESIAN_POINT ( 'NONE',  ( 80.24968131911825253, 48.58851929088046262, 13.79783264785077179 ) ) ;
#7603 = CARTESIAN_POINT ( 'NONE',  ( 198.5109395995180535, 266.2319359199144060, 1.007832260215294928 ) ) ;
#7604 = EDGE_CURVE ( 'NONE', #31824, #5449, #85433, .T. ) ;
#7605 = CARTESIAN_POINT ( 'NONE',  ( 156.8938808821919793, 272.5684933834573940, 14.39157411223618688 ) ) ;
#7606 = ORIENTED_EDGE ( 'NONE', *, *, #82998, .T. ) ;
#7607 = CARTESIAN_POINT ( 'NONE',  ( 190.9335643195044838, 299.9403610588350944, -4.692880224846124548 ) ) ;
#7608 = CARTESIAN_POINT ( 'NONE',  ( 202.7865629936218284, 279.4103651332174536, 17.10878160033216133 ) ) ;
#7609 = LINE ( 'NONE', #1016, #16237 ) ;
#7611 = CARTESIAN_POINT ( 'NONE',  ( 74.09603869131957765, 55.10132886373268946, 16.60403961883766755 ) ) ;
#7610 = CARTESIAN_POINT ( 'NONE',  ( 155.6435836392643637, 261.0644005951349982, 17.58841156286628049 ) ) ;
#7612 = CARTESIAN_POINT ( 'NONE',  ( 21.04067422097218909, 35.08080186712593473, -3.090169943749475845 ) ) ;
#7613 = EDGE_CURVE ( 'NONE', #23003, #5719, #1282, .T. ) ;
#7614 = DIRECTION ( 'NONE',  ( -0.000000000000000000, -0.000000000000000000, 1.000000000000000000 ) ) ;
#7615 = CARTESIAN_POINT ( 'NONE',  ( 164.6292270401010853, 284.5473998418419797, -3.121378508483925174 ) ) ;
#7616 = LINE ( 'NONE', #2024, #1612 ) ;
#7617 = CARTESIAN_POINT ( 'NONE',  ( 198.6562788533279615, 286.5642271139020636, 17.47134757795404525 ) ) ;
#7618 = CARTESIAN_POINT ( 'NONE',  ( 142.3930928536209422, 263.0177522451418781, 5.000000000000046185 ) ) ;
#7619 = CARTESIAN_POINT ( 'NONE',  ( 49.91331508509971826, 100.8438505198844553, 177.5919119679930134 ) ) ;
#7620 = ORIENTED_EDGE ( 'NONE', *, *, #62851, .T. ) ;
#7621 = CARTESIAN_POINT ( 'NONE',  ( 178.5504536548465353, 256.2493563142403445, 8.783846101583462129 ) ) ;
#7622 = DIRECTION ( 'NONE',  ( -0.000000000000000000, 0.000000000000000000, -1.000000000000000000 ) ) ;
#7623 = CARTESIAN_POINT ( 'NONE',  ( 81.59433360772331412, 41.62595464265170619, 5.684377094819374143 ) ) ;
#7624 = CARTESIAN_POINT ( 'NONE',  ( 31.32559514186443295, 179.7048013555409796, 4.594050593750051981 ) ) ;
#7625 = CARTESIAN_POINT ( 'NONE',  ( 49.93482446054089507, 85.48106202472366988, 10.00000000000000000 ) ) ;
#7626 = VECTOR ( 'NONE', #30044, 1000.000000000000114 ) ;
#7627 = CARTESIAN_POINT ( 'NONE',  ( 181.1531766136657495, 275.2180700950633536, -16.44407546173127344 ) ) ;
#7628 = CARTESIAN_POINT ( 'NONE',  ( 34.87460501429023907, 19.94473085651394584, 1.475505719884397138E-15 ) ) ;
#7629 = CARTESIAN_POINT ( 'NONE',  ( 83.07478186481714033, 41.77647167697862329, -3.762335041875428665 ) ) ;
#7630 = CARTESIAN_POINT ( 'NONE',  ( 157.6921299354026189, 257.5162143285667753, -18.18720974599499840 ) ) ;
#7631 = CARTESIAN_POINT ( 'NONE',  ( 38.52196584993465223, 56.41980893122115504, 10.00000000000000000 ) ) ;
#7632 = ADVANCED_FACE ( 'NONE', ( #64075 ), #99465, .F. ) ;
#7633 = CARTESIAN_POINT ( 'NONE',  ( 175.6261675056671550, 253.6354083681499105, -3.856844943141242155 ) ) ;
#7634 = CARTESIAN_POINT ( 'NONE',  ( 187.5747766728329964, 259.5710330847772411, -0.7742262142532535529 ) ) ;
#7635 = EDGE_CURVE ( 'NONE', #49046, #64894, #34712, .T. ) ;
#7636 = AXIS2_PLACEMENT_3D ( 'NONE', #53078, #60160, #74419 ) ;
#7637 = CARTESIAN_POINT ( 'NONE',  ( 61.65426615018211010, 219.7365022471903160, 2.944929066748280225E-16 ) ) ;
#7638 = CARTESIAN_POINT ( 'NONE',  ( 34.18796084459998497, 43.23654200823204263, 1.583844403245397769 ) ) ;
#7639 = CARTESIAN_POINT ( 'NONE',  ( 147.6140518775699491, 274.9719575673779559, 8.457032797753797126 ) ) ;
#7640 = CARTESIAN_POINT ( 'NONE',  ( 25.77718602916411683, 191.8149278399160949, -9.188101187500095079 ) ) ;
#7641 = CARTESIAN_POINT ( 'NONE',  ( 67.34360286252885430, 66.37718443452089900, -8.893619794688017777 ) ) ;
#7642 = CARTESIAN_POINT ( 'NONE',  ( -33.12036098009136964, 24.37273002035945169, -10.00000000000000000 ) ) ;
#7643 = CARTESIAN_POINT ( 'NONE',  ( 203.0652949094600501, 269.8798128736668218, -6.158547683694125752 ) ) ;
#7644 = CARTESIAN_POINT ( 'NONE',  ( 151.0388915836658725, 269.0399611886400635, -14.24896787280406585 ) ) ;
#7645 = CARTESIAN_POINT ( 'NONE',  ( 207.6508796976096107, 270.9851214578045528, 6.713685698622268383 ) ) ;
#7646 = EDGE_CURVE ( 'NONE', #71488, #58166, #68624, .T. ) ;
#7647 = CARTESIAN_POINT ( 'NONE',  ( 188.9965416891025995, 268.2223090079140206, 13.67363464215795865 ) ) ;
#7648 = CARTESIAN_POINT ( 'NONE',  ( 162.0898649156316935, 280.9600800141846548, -10.51109445094396833 ) ) ;
#7649 = CARTESIAN_POINT ( 'NONE',  ( 179.6688721834134412, 263.0910175821119878, -13.35864055896102620 ) ) ;
#7650 = APPLICATION_PROTOCOL_DEFINITION ( 'draft international standard', 'automotive_design', 1998, #56961 ) ;
#7651 = CARTESIAN_POINT ( 'NONE',  ( 21.45440292344354916, 18.10170272979926764, -7.433330006724141015 ) ) ;
#7652 = CARTESIAN_POINT ( 'NONE',  ( 7.004301291108590455, 25.81751292744054282, -6.180339887498951690 ) ) ;
#7653 = CARTESIAN_POINT ( 'NONE',  ( 72.04273812837081437, 59.28583566120335036, 15.84548535924249890 ) ) ;
#7654 = CARTESIAN_POINT ( 'NONE',  ( 188.9004165423950212, 270.0841463155638849, -14.13780846912426448 ) ) ;
#7655 = ORIENTED_EDGE ( 'NONE', *, *, #47099, .T. ) ;
#7656 = AXIS2_PLACEMENT_3D ( 'NONE', #84596, #23243, #15639 ) ;
#7657 = CARTESIAN_POINT ( 'NONE',  ( 159.0906380018002153, 259.2649656523443582, -17.57712761084927067 ) ) ;
#7658 = ADVANCED_FACE ( 'NONE', ( #51872 ), #34214, .T. ) ;
#7659 = CARTESIAN_POINT ( 'NONE',  ( 110.0000000000000000, 0.000000000000000000, 9.212605237762131694 ) ) ;
#7660 = CARTESIAN_POINT ( 'NONE',  ( 73.62988499754025895, 59.71431543555856791, -15.50958422211314769 ) ) ;
#7661 = CARTESIAN_POINT ( 'NONE',  ( 81.33432549305550197, 42.42221510689188335, 7.504012747830186569 ) ) ;
#7662 = CARTESIAN_POINT ( 'NONE',  ( 155.7054361929259301, 262.7846159439811800, -17.64293531980526808 ) ) ;
#7663 = ADVANCED_FACE ( 'NONE', ( #75564 ), #6153, .F. ) ;
#7664 = ORIENTED_EDGE ( 'NONE', *, *, #85464, .F. ) ;
#7665 = CARTESIAN_POINT ( 'NONE',  ( 74.56414817410228579, 187.8759306620403322, -17.47570218321536473 ) ) ;
#7666 = CARTESIAN_POINT ( 'NONE',  ( 71.62184359327899585, 71.38130220946494831, -4.266802885512482213 ) ) ;
#7667 = CARTESIAN_POINT ( 'NONE',  ( 72.93869098254521077, 57.08676652230623461, 16.39928802407133190 ) ) ;
#7668 = CARTESIAN_POINT ( 'NONE',  ( 83.78898797060510617, 41.32812536727200836, 2.261347060406205589 ) ) ;
#7669 = ORIENTED_EDGE ( 'NONE', *, *, #82733, .F. ) ;
#7670 = ORIENTED_EDGE ( 'NONE', *, *, #44948, .F. ) ;
#7671 = VECTOR ( 'NONE', #25991, 1000.000000000000114 ) ;
#7673 = CARTESIAN_POINT ( 'NONE',  ( 82.90655991062965313, 42.38495858070367461, -5.749555441042302206 ) ) ;
#7672 = CARTESIAN_POINT ( 'NONE',  ( 201.3911183001464451, 266.9640362439821502, -3.754059931952923534 ) ) ;
#7674 = ORIENTED_EDGE ( 'NONE', *, *, #67129, .T. ) ;
#7675 = CARTESIAN_POINT ( 'NONE',  ( 153.2583947049096764, 265.1956690150883560, -17.64103123457563882 ) ) ;
#7676 = CARTESIAN_POINT ( 'NONE',  ( -50.66096862766640641, 31.69950886434491721, -10.00000000000000000 ) ) ;
#7677 = CARTESIAN_POINT ( 'NONE',  ( 79.83586840751161162, 57.89405847684007256, 16.26501041126315528 ) ) ;
#7678 = CARTESIAN_POINT ( 'NONE',  ( -63.08903959183645327, 39.77784189046417396, 10.00000000000000000 ) ) ;
#7679 = ORIENTED_EDGE ( 'NONE', *, *, #1880, .F. ) ;
#7680 = CARTESIAN_POINT ( 'NONE',  ( 189.8314329296643450, 301.8493086226544619, -0.8085564604676659384 ) ) ;
#7681 = CARTESIAN_POINT ( 'NONE',  ( 149.1486417047969155, 272.3139700178423368, -11.47583619705022606 ) ) ;
#7682 = ORIENTED_EDGE ( 'NONE', *, *, #26998, .F. ) ;
#7683 = CARTESIAN_POINT ( 'NONE',  ( -2.512112762712735314, 143.3759306620403891, -22.49999999999983658 ) ) ;
#7684 = CARTESIAN_POINT ( 'NONE',  ( 158.8801886266397787, 265.4961833764209018, 16.91276571221451164 ) ) ;
#7685 = ORIENTED_EDGE ( 'NONE', *, *, #55264, .F. ) ;
#7686 = CARTESIAN_POINT ( 'NONE',  ( 190.5477107455830321, 300.6086790531491033, 3.126266616601216963 ) ) ;
#7687 = CARTESIAN_POINT ( 'NONE',  ( 74.56414817410227158, 187.8759306620403322, 17.47570218321536473 ) ) ;
#7688 = VERTEX_POINT ( 'NONE', #99367 ) ;
#7689 = CARTESIAN_POINT ( 'NONE',  ( -6.294050206057209884, 74.34147604373191598, 14.84309344784631080 ) ) ;
#7690 = CARTESIAN_POINT ( 'NONE',  ( 34.88136640284594847, 21.10801979619931146, 3.090169943749476733 ) ) ;
#7691 = DIRECTION ( 'NONE',  ( 0.5000000000000000000, -0.8660254037844387076, 0.000000000000000000 ) ) ;
#7692 = CARTESIAN_POINT ( 'NONE',  ( -78.71521058394759507, 57.86724000996476747, 10.00000000000000000 ) ) ;
#7693 = ORIENTED_EDGE ( 'NONE', *, *, #2779, .T. ) ;
#7694 = ORIENTED_EDGE ( 'NONE', *, *, #40866, .F. ) ;
#7695 = CARTESIAN_POINT ( 'NONE',  ( 190.0914054637564163, 299.5768487891093628, 6.564776197388576762 ) ) ;
#7696 = CARTESIAN_POINT ( 'NONE',  ( 75.78130554586792300, 207.8927522451418213, -10.00000000000009237 ) ) ;
#7697 = CARTESIAN_POINT ( 'NONE',  ( 148.2159754900428936, 273.9293952882992471, 9.267836332806297150 ) ) ;
#7698 = CARTESIAN_POINT ( 'NONE',  ( 190.5477107455830321, 300.6086790531491033, 3.126266616601216963 ) ) ;
#7699 = CARTESIAN_POINT ( 'NONE',  ( 172.7484569319901482, 276.2894592982432869, -15.71612304295510043 ) ) ;
#7700 = CARTESIAN_POINT ( 'NONE',  ( 146.8598618121150423, 276.2782530793093656, -0.7992850717744983680 ) ) ;
#7701 = CARTESIAN_POINT ( 'NONE',  ( 147.5540328368684300, 275.0759135952944234, -4.750028533202499403 ) ) ;
#7702 = DIRECTION ( 'NONE',  ( 0.4996954135095463823, -0.8654978445076774163, -0.03489949670249753444 ) ) ;
#7703 = VECTOR ( 'NONE', #88792, 1000.000000000000000 ) ;
#7704 = DIRECTION ( 'NONE',  ( 0.4999999999999998890, -0.8660254037844385966, 0.000000000000000000 ) ) ;
#7705 = FACE_OUTER_BOUND ( 'NONE', #59598, .T. ) ;
#7706 = CARTESIAN_POINT ( 'NONE',  ( 67.19619177694202961, 66.60445450608504814, 8.464027507732211575 ) ) ;
#7707 = CARTESIAN_POINT ( 'NONE',  ( 72.55717859591010210, 65.07642316054428022, -12.92391924280964588 ) ) ;
#7708 = CARTESIAN_POINT ( 'NONE',  ( 78.67232457920248123, 47.52898336996674544, 14.25219103194631032 ) ) ;
#7709 = VECTOR ( 'NONE', #2453, 999.9999999999998863 ) ;
#7710 = ORIENTED_EDGE ( 'NONE', *, *, #51836, .T. ) ;
#7711 = CARTESIAN_POINT ( 'NONE',  ( 149.7662956631658631, 271.2441619804512243, -12.26682131771685036 ) ) ;
#7712 = CARTESIAN_POINT ( 'NONE',  ( 83.16083141524212863, 41.41346057833686700, -1.656387949955075323 ) ) ;
#7713 = CARTESIAN_POINT ( 'NONE',  ( 87.74379322371484591, 45.04902437494477851, -6.671288900681476619 ) ) ;
#7714 = CARTESIAN_POINT ( 'NONE',  ( 79.38855964867086357, 46.21855749211306374, 12.64186050921641957 ) ) ;
#7715 = B_SPLINE_CURVE_WITH_KNOTS ( 'NONE', 3,
 ( #54312, #33543, #94375, #73914 ),
 .UNSPECIFIED., .F., .F.,
 ( 4, 4 ),
 ( 0.0008745192274822840206, 0.006137245505070649740 ),
 .UNSPECIFIED. ) ;
#7716 = CARTESIAN_POINT ( 'NONE',  ( 43.39556388706024848, 195.8615022471902591, -10.00000000000009592 ) ) ;
#7717 = CARTESIAN_POINT ( 'NONE',  ( 39.64431452495995245, 58.26521502737223557, 10.00000000000000000 ) ) ;
#7718 = CARTESIAN_POINT ( 'NONE',  ( 165.4078582752671878, 283.6377208367567846, -8.325660689787278912 ) ) ;
#7719 = VERTEX_POINT ( 'NONE', #29946 ) ;
#7720 = CARTESIAN_POINT ( 'NONE',  ( 162.8480293090835005, 248.5859346546387769, -9.753154585358942086 ) ) ;
#7721 = VECTOR ( 'NONE', #53627, 1000.000000000000000 ) ;
#7722 = CARTESIAN_POINT ( 'NONE',  ( 72.34273340409356479, 71.56583958283731306, 5.071847820242139981 ) ) ;
#7723 = CARTESIAN_POINT ( 'NONE',  ( 38.03703169759608471, 202.7677522451419350, -5.000000000000047962 ) ) ;
#7724 = CARTESIAN_POINT ( 'NONE',  ( 121.9060058492368483, 247.3149278399160949, -9.188101187500095079 ) ) ;
#7725 = EDGE_CURVE ( 'NONE', #90569, #18043, #62500, .T. ) ;
#7726 = CARTESIAN_POINT ( 'NONE',  ( 151.3999564459286375, 268.4145785023736153, -15.40574304386609050 ) ) ;
#7727 = VECTOR ( 'NONE', #7542, 1000.000000000000114 ) ;
#7728 = CARTESIAN_POINT ( 'NONE',  ( -22.42236680055709641, 157.8615022471902591, 0.000000000000000000 ) ) ;
#7729 = CARTESIAN_POINT ( 'NONE',  ( 157.8763546842245376, 257.1971277035954699, 17.68444922773363004 ) ) ;
#7730 = CARTESIAN_POINT ( 'NONE',  ( 172.6900760593800044, 250.5973497951363811, -4.149042267653843652 ) ) ;
#7731 = CARTESIAN_POINT ( 'NONE',  ( 50.29670382169353360, 199.8458772461660260, 9.188101187500095079 ) ) ;
#7732 = CARTESIAN_POINT ( 'NONE',  ( 178.7655400679708464, 291.8864583725769535, -5.901772721150448042 ) ) ;
#7733 = CIRCLE ( 'NONE', #69194, 0.1418229129680858847 ) ;
#7734 = DIRECTION ( 'NONE',  ( -0.8660254037844387076, -0.4999999999999998890, -0.000000000000000000 ) ) ;
#7735 = ORIENTED_EDGE ( 'NONE', *, *, #9431, .F. ) ;
#7736 = LINE ( 'NONE', #62412, #94816 ) ;
#7737 = DIRECTION ( 'NONE',  ( 0.000000000000000000, 0.000000000000000000, 1.000000000000000000 ) ) ;
#7738 = EDGE_CURVE ( 'NONE', #60977, #12604, #75831, .T. ) ;
#7739 = CARTESIAN_POINT ( 'NONE',  ( 73.18372135689499203, 60.26031415148027293, 15.75792897287434435 ) ) ;
#7740 = EDGE_CURVE ( 'NONE', #54118, #54173, #63842, .T. ) ;
#7741 = CARTESIAN_POINT ( 'NONE',  ( 190.9335643195044838, 299.9403610588350944, -4.692880224846124548 ) ) ;
#7742 = CARTESIAN_POINT ( 'NONE',  ( -8.109353775345800486, 61.89996032967495410, -10.00000000000000000 ) ) ;
#7743 = CARTESIAN_POINT ( 'NONE',  ( 191.2104420009116836, 280.2857515794617598, 17.80337293751487593 ) ) ;
#7744 = CARTESIAN_POINT ( 'NONE',  ( 156.3864393596315381, 270.3627023744734856, -14.79408036704170470 ) ) ;
#7745 = AXIS2_PLACEMENT_3D ( 'NONE', #65694, #18115, #81446 ) ;
#7746 = CARTESIAN_POINT ( 'NONE',  ( 109.4119587261636752, 220.6427522451417644, 1.119607411625061291E-15 ) ) ;
#7747 = LINE ( 'NONE', #46739, #6251 ) ;
#7748 = ORIENTED_EDGE ( 'NONE', *, *, #38014, .T. ) ;
#7749 = CARTESIAN_POINT ( 'NONE',  ( 163.4260108471723640, 247.5848412648317662, 10.45113099391573108 ) ) ;
#7750 = CARTESIAN_POINT ( 'NONE',  ( 85.05033292184569405, 46.62834512446820412, -10.94201510068669414 ) ) ;
#7751 = CARTESIAN_POINT ( 'NONE',  ( 32.70573635520464251, 183.5643266524160140, 9.188101187500095079 ) ) ;
#7752 = CARTESIAN_POINT ( 'NONE',  ( 10.46840290624634306, 27.81751292744054993, -6.180339887498951690 ) ) ;
#7753 = CARTESIAN_POINT ( 'NONE',  ( 195.9351945738247309, 273.3307776679702670, 15.22350882708002118 ) ) ;
#7754 = CARTESIAN_POINT ( 'NONE',  ( 146.9709166616330549, 276.0859004375172390, 3.755270622130282732 ) ) ;
#7755 = DIRECTION ( 'NONE',  ( -0.9263643838751195458, -0.3766285016932073293, 0.000000000000000000 ) ) ;
#7757 = CARTESIAN_POINT ( 'NONE',  ( 65.85835811776894388, 199.6423013555410080, -4.594050593750043987 ) ) ;
#7756 = CARTESIAN_POINT ( 'NONE',  ( 198.2782625130438987, 277.4159975312159645, -15.37005889760090405 ) ) ;
#7758 = CARTESIAN_POINT ( 'NONE',  ( 164.4414259850711915, 245.8260906552167171, -6.983224448873608381 ) ) ;
#7759 = CARTESIAN_POINT ( 'NONE',  ( 73.01029701701182262, 57.12463796210177236, 16.39976797707190315 ) ) ;
#7760 = CARTESIAN_POINT ( 'NONE',  ( 182.0338464029501040, 278.3680066549227945, 17.69288446120480174 ) ) ;
#7761 = CARTESIAN_POINT ( 'NONE',  ( 66.70287695511908055, 68.38935073730952752, -4.375220962393981061 ) ) ;
#7762 = VERTEX_POINT ( 'NONE', #16244 ) ;
#7763 = ADVANCED_FACE ( 'NONE', ( #8151 ), #86702, .T. ) ;
#7764 = CARTESIAN_POINT ( 'NONE',  ( 23.90999230191038549, 184.6115022471902591, 10.00000000000009592 ) ) ;
#7765 = B_SPLINE_CURVE_WITH_KNOTS ( 'NONE', 3,
 ( #38243, #61051, #6383, #37266, #84407, #14480, #77265, #45361, #14952, #22570, #76764, #91507, #24932, #69158, #100088, #76293, #99091, #45842, #22072, #52967, #71559, #30675, #92024, #9244, #37755, #92501, #68660, #99583, #23047, #79185, #53944, #84902, #40119, #71059, #94873, #1660, #63443, #94378, #55806, #86799, #48239, #40622, #2156, #29675, #33035, #63934, #25435, #56326 ),
 .UNSPECIFIED., .F., .F.,
 ( 4, 2, 2, 2, 2, 2, 2, 2, 2, 2, 2, 2, 2, 2, 2, 2, 2, 2, 2, 2, 2, 2, 2, 4 ),
 ( 0.0005154968519531658369, 0.0009585995601737966462, 0.001180150914284111997, 0.001290926591339269618, 0.001401702268394427239, 0.001512477945449584643, 0.001623253622504742264, 0.001844804976615087430, 0.002287907684835912420, 0.003174113101277619645, 0.004060318517719327738, 0.004946523934161035398, 0.005389626642381843691, 0.005611177996492257812, 0.005721953673547463572, 0.005777341512075067319, 0.005832729350602670199, 0.005888117189130273946, 0.005943505027657876826, 0.006054280704713086055, 0.006275832058823504513, 0.006718934767044361378, 0.007162037475265219111, 0.007605140183486076844 ),
 .UNSPECIFIED. ) ;
#7766 = CARTESIAN_POINT ( 'NONE',  ( 163.7085541710205234, 247.0954618725873217, -6.713544974106887331 ) ) ;
#7767 = VECTOR ( 'NONE', #54858, 1000.000000000000114 ) ;
#7768 = CARTESIAN_POINT ( 'NONE',  ( 150.4851912698882757, 251.5643266524160424, -9.188101187500093303 ) ) ;
#7769 = CARTESIAN_POINT ( 'NONE',  ( 36.75658403392715456, 24.14754757982092315, -5.678558825948276656 ) ) ;
#7770 = DIRECTION ( 'NONE',  ( -0.8660254037844379305, -0.5000000000000014433, -0.000000000000000000 ) ) ;
#7771 = CARTESIAN_POINT ( 'NONE',  ( 188.8015641287956612, 261.8435057067845833, 6.507177985326441316 ) ) ;
#7772 = EDGE_CURVE ( 'NONE', #46269, #82418, #65276, .T. ) ;
#7773 = CARTESIAN_POINT ( 'NONE',  ( 206.3907062969896060, 273.1678058140250300, 11.56942460516550675 ) ) ;
#7774 = CARTESIAN_POINT ( 'NONE',  ( 88.42017002704760387, 43.92753743058676719, 1.721442031696316377 ) ) ;
#7775 = EDGE_CURVE ( 'NONE', #3488, #53634, #84283, .T. ) ;
#7776 = CARTESIAN_POINT ( 'NONE',  ( 66.17642628206915845, 69.10264375944338155, 2.573923083425510239 ) ) ;
#7777 = ORIENTED_EDGE ( 'NONE', *, *, #78793, .F. ) ;
#7778 = CARTESIAN_POINT ( 'NONE',  ( 81.42668684898659137, 52.12787871455454081, 15.51728826852514587 ) ) ;
#7779 = AXIS2_PLACEMENT_3D ( 'NONE', #47223, #17846, #86290 ) ;
#7780 = CARTESIAN_POINT ( 'NONE',  ( 181.4396949203754161, 287.4694724887078223, 13.37274027909958640 ) ) ;
#7781 = DIRECTION ( 'NONE',  ( 0.000000000000000000, 1.000000000000000000, 0.000000000000000000 ) ) ;
#7782 = CARTESIAN_POINT ( 'NONE',  ( 11.99789328850488879, 15.43085787977761214, -9.188101187500008038 ) ) ;
#7783 = EDGE_LOOP ( 'NONE', ( #72377, #54402, #75895, #30848 ) ) ;
#7784 = CARTESIAN_POINT ( 'NONE',  ( -33.79156961297667294, 36.11817918669349581, 59.99999999999999289 ) ) ;
#7785 = CIRCLE ( 'NONE', #45009, 70.00000000000001421 ) ;
#7786 = EDGE_CURVE ( 'NONE', #37787, #34490, #58232, .T. ) ;
#7787 = CARTESIAN_POINT ( 'NONE',  ( 205.0994677818405023, 275.4042965269534307, -14.14519517703424789 ) ) ;
#7788 = ADVANCED_FACE ( 'NONE', ( #95802 ), #81583, .F. ) ;
#7789 = CARTESIAN_POINT ( 'NONE',  ( 200.8812236821030126, 282.2243460117538234, -16.60069316942784567 ) ) ;
#7790 = CARTESIAN_POINT ( 'NONE',  ( 189.2654362934434289, 294.2704508525881693, 12.90651062627435053 ) ) ;
#7791 = DIRECTION ( 'NONE',  ( 0.09547062131715944311, -0.9954322480537364237, 0.000000000000000000 ) ) ;
#7792 = CARTESIAN_POINT ( 'NONE',  ( 163.1369207721744772, 248.0855599626920593, -11.24692769914530110 ) ) ;
#7793 = LINE ( 'NONE', #60976, #87261 ) ;
#7794 = ORIENTED_EDGE ( 'NONE', *, *, #25882, .T. ) ;
#7795 = VECTOR ( 'NONE', #68295, 1000.000000000000000 ) ;
#7796 = ORIENTED_EDGE ( 'NONE', *, *, #91300, .F. ) ;
#7797 = CARTESIAN_POINT ( 'NONE',  ( 190.5361265807717359, 281.4599470083306869, 16.99703021481662191 ) ) ;
#7798 = CARTESIAN_POINT ( 'NONE',  ( 73.04137136423049981, 70.75758827781731952, 7.534468892676039253 ) ) ;
#7799 = ORIENTED_EDGE ( 'NONE', *, *, #28444, .F. ) ;
#7800 = CARTESIAN_POINT ( 'NONE',  ( 190.7705347155322499, 300.2227366160529414, 3.504769718465625239 ) ) ;
#7801 = CARTESIAN_POINT ( 'NONE',  ( 157.4068442735347446, 281.9945091197541274, 2.874377194828706905 ) ) ;
#7802 = CARTESIAN_POINT ( 'NONE',  ( 84.74040462907180427, 45.11266949017006311, -8.735513756553579867 ) ) ;
#7803 = VERTEX_POINT ( 'NONE', #72477 ) ;
#7804 = CARTESIAN_POINT ( 'NONE',  ( 58.43017357788679789, 217.8207943907112849, 2.194453944013935930E-14 ) ) ;
#7805 = CARTESIAN_POINT ( 'NONE',  ( 79.32558605478152458, 59.69129752972264669, -16.52184683405511834 ) ) ;
#7806 = VECTOR ( 'NONE', #24913, 1000.000000000000114 ) ;
#7807 = CARTESIAN_POINT ( 'NONE',  ( 149.6890529486499872, 271.3779502865075983, -12.51465682618088593 ) ) ;
#7808 = CARTESIAN_POINT ( 'NONE',  ( 69.81793561852694552, 62.72544707633330319, 13.91621835302064447 ) ) ;
#7809 = ORIENTED_EDGE ( 'NONE', *, *, #98151, .F. ) ;
#7810 = CARTESIAN_POINT ( 'NONE',  ( 93.65192705076950119, 231.0024278399160949, -9.188101187500093303 ) ) ;
#7811 = CARTESIAN_POINT ( 'NONE',  ( 155.3841941879665853, 261.5136763037301648, 18.59686659711820411 ) ) ;
#7812 = CARTESIAN_POINT ( 'NONE',  ( 191.4685399627163633, 299.0137560639802814, 7.545791216288330716 ) ) ;
#7813 = CARTESIAN_POINT ( 'NONE',  ( 166.7187202459675746, 278.5591580196478958, -14.78021074750266273 ) ) ;
#7814 = B_SPLINE_SURFACE_WITH_KNOTS ( 'NONE', 3, 1, ( 
 ( #63290, #99940 ),
 ( #52813, #71910 ),
 ( #14818, #94233 ),
 ( #9617, #76157 ),
 ( #37609, #99443 ),
 ( #30020, #24784 ),
 ( #39969, #2000 ),
 ( #79544, #2511 ),
 ( #76629, #17702 ),
 ( #55666, #62782 ),
 ( #40479, #48605 ),
 ( #64296, #38099 ),
 ( #45218, #40964 ),
 ( #70904, #7215 ),
 ( #69010, #71410 ),
 ( #94727, #32886 ),
 ( #30524, #83770 ),
 ( #79026, #86653 ),
 ( #32394, #6732 ),
 ( #93739, #25287 ),
 ( #56173, #14330 ),
 ( #17184, #68522 ),
 ( #87169, #48086 ),
 ( #24299, #55175 ),
 ( #86159, #78512 ),
 ( #16693, #47584 ),
 ( #1512, #12609 ),
 ( #50579, #10603 ),
 ( #73406, #89640 ),
 ( #43474, #34393 ),
 ( #41475, #72424 ),
 ( #74418, #5003 ),
 ( #3992, #56688 ),
 ( #82034, #11119 ) ),
 .UNSPECIFIED., .T., .F., .F.,
 ( 4, 2, 2, 2, 2, 2, 2, 2, 2, 2, 2, 2, 2, 2, 2, 2, 4 ),
 ( 2, 2 ),
 ( 0.000000000000000000, 0.06250000000000000000, 0.1250000000000000000, 0.1875000000000000000, 0.2500000000000000000, 0.3125000000000000000, 0.3750000000000000000, 0.4375000000000000000, 0.5000000000000000000, 0.5625000000000000000, 0.6250000000000000000, 0.6875000000000000000, 0.7500000000000000000, 0.8125000000000000000, 0.8750000000000000000, 0.9375000000000000000, 1.000000000000000000 ),
 ( 0.000000000000000000, 1.000000000000000000 ),
 .UNSPECIFIED. ) ;
#7815 = EDGE_LOOP ( 'NONE', ( #2630, #20932, #91451, #80762 ) ) ;
#7816 = ORIENTED_EDGE ( 'NONE', *, *, #22121, .T. ) ;
#7817 = EDGE_LOOP ( 'NONE', ( #1320, #44662, #61100, #72372 ) ) ;
#7818 = CARTESIAN_POINT ( 'NONE',  ( 73.43380971014073566, 61.55604703159713864, 14.92230597848644358 ) ) ;
#7819 = ORIENTED_EDGE ( 'NONE', *, *, #79029, .F. ) ;
#7820 = CARTESIAN_POINT ( 'NONE',  ( 152.6547697591180111, 278.7515079535921814, -4.825746761778547445 ) ) ;
#7821 = CARTESIAN_POINT ( 'NONE',  ( 87.85893154554855755, 45.08040635541048857, 6.601944857759019847 ) ) ;
#7822 = ORIENTED_EDGE ( 'NONE', *, *, #17356, .T. ) ;
#7823 = CARTESIAN_POINT ( 'NONE',  ( 208.3117541397001844, 269.8404533466799080, 2.895672523916592578 ) ) ;
#7824 = AXIS2_PLACEMENT_3D ( 'NONE', #25236, #70847, #63242 ) ;
#7825 = CYLINDRICAL_SURFACE ( 'NONE', #75652, 16.60714546451156792 ) ;
#7826 = CARTESIAN_POINT ( 'NONE',  ( 165.1189985546704975, 271.0502085123236498, 16.97077559774535871 ) ) ;
#7828 = EDGE_CURVE ( 'NONE', #72764, #95045, #35438, .T. ) ;
#7827 = CARTESIAN_POINT ( 'NONE',  ( -19.57455831887243036, 93.18311100154903670, 59.99999999999999289 ) ) ;
#7829 = DIRECTION ( 'NONE',  ( 0.9942962326340548662, 0.1066536533351087890, 0.000000000000000000 ) ) ;
#7830 = CARTESIAN_POINT ( 'NONE',  ( 82.74681249865726329, 53.90498867430740404, -15.82393922498146921 ) ) ;
#7831 = VERTEX_POINT ( 'NONE', #65343 ) ;
#7832 = DIRECTION ( 'NONE',  ( -0.3105719460338542404, -0.9505498757754611283, 0.000000000000000000 ) ) ;
#7833 = CARTESIAN_POINT ( 'NONE',  ( 10.42942532566755354, 26.99752408145590721, 5.678558825948277544 ) ) ;
#7834 = VECTOR ( 'NONE', #68400, 1000.000000000000000 ) ;
#7835 = CARTESIAN_POINT ( 'NONE',  ( 33.00691499580853616, 42.55466486950702887, 7.012934429366973338E-14 ) ) ;
#7836 = CARTESIAN_POINT ( 'NONE',  ( -22.42236680055709641, 157.8615022471902591, 0.000000000000000000 ) ) ;
#7838 = ORIENTED_EDGE ( 'NONE', *, *, #18191, .T. ) ;
#7837 = LINE ( 'NONE', #46304, #23424 ) ;
#7839 = CARTESIAN_POINT ( 'NONE',  ( 170.9828833598360234, 259.0842644313817686, -13.89840066965689758 ) ) ;
#7840 = CARTESIAN_POINT ( 'NONE',  ( 206.6268150440956504, 272.7588534679261443, -10.76664753678610609 ) ) ;
#7841 = CARTESIAN_POINT ( 'NONE',  ( 80.08958074560355556, 44.70221173755660971, 11.12270814150613241 ) ) ;
#7842 = CARTESIAN_POINT ( 'NONE',  ( 81.59622370732601837, 46.04426866650761241, -11.56528914279085996 ) ) ;
#7843 = CARTESIAN_POINT ( 'NONE',  ( 171.1494736412307418, 255.4807717095144994, 11.23012609300629450 ) ) ;
#7844 = CARTESIAN_POINT ( 'NONE',  ( 194.0472512474883047, 263.4056162429215533, -0.7688519765262188388 ) ) ;
#7845 = ORIENTED_EDGE ( 'NONE', *, *, #25758, .T. ) ;
#7846 = CARTESIAN_POINT ( 'NONE',  ( 193.8618999797658091, 294.8683349136467200, -15.25219021621163051 ) ) ;
#7847 = CARTESIAN_POINT ( 'NONE',  ( 75.06349586682163988, 67.01194365216522897, -13.14257922886206487 ) ) ;
#7848 = CIRCLE ( 'NONE', #79037, 70.00000000000001421 ) ;
#7849 = CARTESIAN_POINT ( 'NONE',  ( 163.1218343930725894, 256.2508100442478849, -16.13596270478102923 ) ) ;
#7850 = CARTESIAN_POINT ( 'NONE',  ( -0.9341114727036623488, 180.2677522451419350, -5.000000000000047962 ) ) ;
#7851 = CARTESIAN_POINT ( 'NONE',  ( 87.42789010471635436, 209.0327760586659451, 1.948934522072302763E-15 ) ) ;
#7852 = EDGE_CURVE ( 'NONE', #36064, #16265, #2071, .T. ) ;
#7853 = CARTESIAN_POINT ( 'NONE',  ( 192.8523012050875707, 267.1932176075470124, -11.09616388545629384 ) ) ;
#7854 = VECTOR ( 'NONE', #27344, 1000.000000000000000 ) ;
#7855 = FACE_OUTER_BOUND ( 'NONE', #51529, .T. ) ;
#7856 = CARTESIAN_POINT ( 'NONE',  ( 203.5365106480763018, 278.1114176926849382, -15.57541962905212252 ) ) ;
#7857 = VECTOR ( 'NONE', #96091, 1000.000000000000000 ) ;
#7858 = CARTESIAN_POINT ( 'NONE',  ( 176.0164579604465018, 289.8288593268874251, 9.535015465809415502 ) ) ;
#7859 = CARTESIAN_POINT ( 'NONE',  ( 7.266240119036749157, 168.8768266524159856, -9.188101187500091527 ) ) ;
#7860 = CARTESIAN_POINT ( 'NONE',  ( 200.9110265982630779, 282.6588894614233141, 17.52479721249226685 ) ) ;
#7861 = EDGE_LOOP ( 'NONE', ( #9188, #92716, #77192, #81964 ) ) ;
#7862 = VECTOR ( 'NONE', #7291, 1000.000000000000000 ) ;
#7863 = VERTEX_POINT ( 'NONE', #37911 ) ;
#7864 = CARTESIAN_POINT ( 'NONE',  ( 155.5995420464182644, 262.6346450740109617, -17.48312782858739567 ) ) ;
#7865 = CARTESIAN_POINT ( 'NONE',  ( 198.1306167967736940, 265.0230878689690144, -3.023881929457708395 ) ) ;
#7866 = ADVANCED_FACE ( 'NONE', ( #52126 ), #83076, .T. ) ;
#7867 = CARTESIAN_POINT ( 'NONE',  ( 85.04690354554347209, 46.11796720474825406, -9.797488362679569462 ) ) ;
#7868 = CARTESIAN_POINT ( 'NONE',  ( 205.4029933437358295, 274.8785748323546159, -13.50815392427034922 ) ) ;
#7869 = EDGE_CURVE ( 'NONE', #9430, #40063, #49690, .T. ) ;
#7870 = CARTESIAN_POINT ( 'NONE',  ( -37.33262083840156720, 163.6868197944959888, 1.732050807568908724 ) ) ;
#7871 = AXIS2_PLACEMENT_3D ( 'NONE', #69574, #99002, #23460 ) ;
#7872 =( BOUNDED_CURVE ( )  B_SPLINE_CURVE ( 2, ( #18600, #94125, #55070, #40861, #8490, #72310, #70789, #79434, #39360, #9999, #33809, #8983, #39854, #71808, #88052, #87052, #79929, #1399, #2404, #17587, #63182, #57071, #24679, #77904, #95645, #56579, #86546, #87566, #33283, #94622, #25179, #17077, #48493, #86055, #70274, #885, #78913, #64185, #95134, #56059, #47478, #47967, #18095, #48993, #31764, #9499, #16582, #10489, #62668, #2917, #40365, #41370, #93620, #26192, #24187, #71304, #78402, #81923, #59554, #58567, #51475, #4380, #43865, #74807, #50473, #28671, #34772, #49479, #67170, #28177, #80943, #59048, #43368, #73791, #35280, #73299, #89539, #26685, #41882, #11009, #81426, #97132, #12499, #74315, #4897, #90531, #57573, #5385, #80435, #36271, #97609, #49988, #72820, #66186, #98093, #35781, #20592, #42365, #66675, #3412, #11998, #34286, #58083, #42855, #65183, #90020, #27699, #20100, #19112, #96131, #96628, #88546, #11511, #3890, #82442, #50971, #65673, #13005, #27194, #89063, #19615, #13494, #23044, #92499, #13980, #84405, #22070, #5878, #31145, #99581, #61049, #6381, #77263, #45359, #53941, #68658, #67674, #30165, #60548, #7357, #44855, #21580, #75795, #36764, #45839, #69156, #76762, #14950, #38752, #84900, #15441, #37264, #37752, #46340, #68163, #99089, #29672, #91505, #76291, #52965, #83916, #62036, #7875, #51980, #98603, #14478, #21102, #6863, #264, #92022, #100086, #82919, #69655, #22568, #44365, #29186, #53454, #75297, #61553, #52465, #38241, #60054, #91017, #30673, #83410, #757, #24556, #1270, #86425, #93500, #47354, #8370, #17461, #40744, #48371, #55933, #10377, #95011, #25571, #78276, #9365, #32155, #63062, #33677, #94005, #40244, #86931, #8860, #71689, #92989, #56460, #23543, #70144, #55436, #85933, #78780, #79319, #54434, #39727, #31641, #9887, #2285, #15958, #85409, #62541, #79813, #47840, #48878, #24060, #33163, #54954, #64067, #16951, #94500, #71185, #87451, #17984, #1781, #72186, #70658, #46861, #41247, #2796, #77783, #32660, #39235, #16458, #63560, #25057, #87937, #57451, #65558, #3776, #73184, #57956, #81310, #42738, #11881, #35658, #41754, #81800, #10877, #64574, #96506, #3292, #49366, #34658, #88430, #95530, #56951, #80826, #72700, #18480, #11395, #43242, #42248, #27075, #34172, #58448, #88942, #19501, #80310, #65064, #49861, #50355, #73674, #4255, #35155, #18990, #66062, #96014, #26575, #97012, #27581, #26075, #19973, #89419, #97486, #12376, #50850, #74184, #4775, #66558, #79636, #25910, #47673, #48188, #78100, #93837, #71009, #79134, #9714, #32498, #63388, #9192, #87272, #24391, #40067, #94329, #1097, #47178, #64898, #87765, #40571, #41578, #31974, #78606, #8690, #95355, #86246, #24882, #62879, #56782, #39559, #56275, #10700, #55265, #86750, #55758, #71511, #16783, #70483, #17284, #1611, #2102, #32983, #63887, #72519, #94823, #3128, #25387, #17803, #48702, #10203, #95844, #41066, #72004, #2608, #33496, #64391, #54777, #18304, #49203, #80136, #85755, #34013, #16285, #80638, #3606, #19322, #89733, #73499, #74511, #49683, #18800, #96327, #13201, #81623, #82643, #34484, #12706, #36470, #35480, #28374, #50185, #20294, #66384, #57775, #26399, #58763, #74001, #51693, #44059, #74999, #82134, #97314, #11215, #65384, #65877, #5578, #42082, #73014, #88253, #27396, #27881, #51171, #50671, #26897, #88750, #96832, #57276, #81139, #11705, #42565, #12196, #67374, #4082, #20800, #34974, #58278, #5090, #89254, #19804, #43055, #4587, #43577, #35970, #66872, #97805, #59252, #90231, #29128, #43303, #35717, #50413, #82863, #97546, #66616, #4313, #27136, #81859, #28112, #58987, #12436, #74251, #89477, #67107, #35217, #20036, #4836, #81371, #58021, #36699, #5813, #27639, #98032, #89956, #19553, #44794, #12945, #74746, #20534, #11939, #75231, #89002, #36203, #90964, #42795, #51412, #82375, #43805, #66119, #50909, #73729, #59492, #13436, #90471, #28609, #52405, #67608, #98538, #5326, #59995, #21041, #51923, #58504, #44302, #21522, #83350, #13916, #75730, #34714, #65614, #97067, #96569, #48693, #52903, #6315, #60487, #83854, #99526, #70998, #37206, #2093, #30109, #7810, #68107, #40058, #63879, #37692, #68602, #1602, #17794, #15382, #9703, #60992, #32485, #46279, #91959, #99029, #63380, #29615, #25377, #86740, #22507, #17275, #94319, #30611, #61496, #53401, #77205, #14420, #91446, #22007, #7301, #24874, #55748, #92447, #76236, #6811, #22993, #45302, #48178, #94814, #84350, #38182, #14897, #100025, #45786, #76707, #69098, #79123, #40563, #71500, #32971, #56267, #87260, #53884, #84844, #96318, #43045, #88242, #20285, #49672, #26885, #73490, #34004, #58268, #79628, #81614, #10192, #56774, #80629, #72510, #65375, #42556, #41057, #95836, #87755, #4074, #71994, #2599, #33484, #49190, #66373, #34477, #35469, #18296, #65863, #41567, #19795, #42075, #81131, #57764, #73989, #4574, #11204, #58753, #64889, #64383, #97305, #27872, #34963, #19312, #95344, #80127, #18792, #89724, #25901, #26388, #88740, #73007, #3596, #50177, #11697, #96823, #27381, #10688, #57267, #89244, #50662, #12186, #75482, #20788, #35962, #83104, #5567, #82123, #12696, #28877, #59239, #43564, #98288, #45546, #59752, #52155, #66863, #99280, #13675, #44548, #51679, #90217, #67360, #6065, #36959, #90723, #21278, #36459, #83604, #82628, #67871, #98792, #97793, #74502, #53162, #22258, #44046, #14171, #29374, #28363, #61247, #91696, #13190, #60240, #91201, #21761, #45056, #75996, #6574, #30363, #74987, #76477, #92215, #7056, #29863, #52650, #51160, #37445, #37937, #68355, #84116, #60734, #14668, #5080, #68850, #99771, #31354, #23744, #38444, #70869, #85617, #54638, #92696, #15138, #69852, #69359, #100277, #17154, #1477, #16160, #46036, #23247, #8073, #464, #30864, #76952, #24754, #94200, #15643, #86127, #47059, #7553, #32853, #965, #62744, #38947, #78994, #77972, #55635, #70353, #61747, #54134, #8568, #62237, #39434, #85097, #77477, #46540, #47551, #32358, #78478, #16656, #40444, #86620, #48052 ),
 .UNSPECIFIED., .F., .T. ) 
 B_SPLINE_CURVE_WITH_KNOTS ( ( 3, 2, 2, 2, 2, 2, 2, 2, 2, 2, 2, 2, 2, 2, 2, 2, 2, 2, 2, 2, 2, 2, 2, 2, 2, 2, 2, 2, 2, 2, 2, 2, 2, 2, 2, 2, 2, 2, 2, 2, 2, 2, 2, 2, 2, 2, 2, 2, 2, 2, 2, 2, 2, 2, 2, 2, 2, 2, 2, 2, 2, 2, 2, 2, 2, 2, 2, 2, 2, 2, 2, 2, 2, 2, 2, 2, 2, 2, 2, 2, 2, 2, 2, 2, 2, 2, 2, 2, 2, 2, 2, 2, 2, 2, 2, 2, 2, 2, 2, 2, 2, 2, 2, 2, 2, 2, 2, 2, 2, 2, 2, 2, 2, 2, 2, 2, 2, 2, 2, 2, 2, 2, 2, 2, 2, 2, 2, 2, 2, 2, 2, 2, 2, 2, 2, 2, 2, 2, 2, 2, 2, 2, 2, 2, 2, 2, 2, 2, 2, 2, 2, 2, 2, 2, 2, 2, 2, 2, 2, 2, 2, 2, 2, 2, 2, 2, 2, 2, 2, 2, 2, 2, 2, 2, 2, 2, 2, 2, 2, 2, 2, 2, 2, 2, 2, 2, 2, 2, 2, 2, 2, 2, 2, 2, 2, 2, 2, 2, 2, 2, 2, 2, 2, 2, 2, 2, 2, 2, 2, 2, 2, 2, 2, 2, 2, 2, 2, 2, 2, 2, 2, 2, 2, 2, 2, 2, 2, 2, 2, 2, 2, 2, 2, 2, 2, 2, 2, 2, 2, 2, 2, 2, 2, 2, 2, 2, 2, 2, 2, 2, 2, 2, 2, 2, 2, 2, 2, 2, 2, 2, 2, 2, 2, 2, 2, 2, 2, 2, 2, 2, 2, 2, 2, 2, 2, 2, 2, 2, 2, 2, 2, 2, 2, 2, 2, 2, 2, 2, 2, 2, 2, 2, 2, 2, 2, 2, 2, 2, 2, 2, 2, 2, 2, 2, 2, 2, 2, 2, 2, 2, 2, 2, 2, 2, 2, 2, 2, 2, 2, 2, 2, 2, 2, 2, 2, 2, 2, 2, 2, 2, 2, 2, 2, 2, 2, 2, 2, 2, 2, 2, 2, 2, 2, 2, 2, 2, 2, 2, 2, 2, 2, 2, 2, 2, 2, 2, 2, 2, 2, 2, 2, 2, 2, 2, 2, 2, 2, 3 ),
 ( 0.000000000000000000, 0.002688172043010752903, 0.005376344086021505805, 0.008064516129032257841, 0.01075268817204301161, 0.01344086021505376365, 0.01612903225806451568, 0.01881720430107526945, 0.02150537634408602322, 0.02419354838709677352, 0.02688172043010752729, 0.02956989247311828106, 0.03225806451612903136, 0.03494623655913978166, 0.03763440860215053890, 0.04032258064516128920, 0.04301075268817204644, 0.04569892473118279674, 0.04838709677419354704, 0.05107526881720430428, 0.05376344086021505458, 0.05645161290322580488, 0.05913978494623656212, 0.06182795698924731242, 0.06451612903225806273, 0.06720430107526881303, 0.06989247311827956333, 0.07258064516129032751, 0.07526881720430107781, 0.07795698924731182811, 0.08064516129032257841, 0.08333333333333332871, 0.08602150537634409289, 0.08870967741935484319, 0.09139784946236559349, 0.09408602150537634379, 0.09677419354838709409, 0.09946236559139784439, 0.1021505376344086086, 0.1048387096774193589, 0.1075268817204301092, 0.1102150537634408595, 0.1129032258064516098, 0.1155913978494623601, 0.1182795698924731242, 0.1209677419354838745, 0.1236559139784946248, 0.1263440860215053752, 0.1290322580645161255, 0.1317204301075268758, 0.1344086021505376261, 0.1370967741935483764, 0.1397849462365591267, 0.1424731182795699047, 0.1451612903225806550, 0.1478494623655914053, 0.1505376344086021556, 0.1532258064516129059, 0.1559139784946236562, 0.1586021505376344065, 0.1612903225806451568, 0.1639784946236559071, 0.1666666666666666574, 0.1693548387096774077, 0.1720430107526881858, 0.1747311827956989361, 0.1774193548387096864, 0.1801075268817204367, 0.1827956989247311870, 0.1854838709677419373, 0.1881720430107526876, 0.1908602150537634379, 0.1935483870967741882, 0.1962365591397849385, 0.1989247311827956888, 0.2016129032258064391, 0.2043010752688172171, 0.2069892473118279674, 0.2096774193548387177, 0.2123655913978494680, 0.2150537634408602183, 0.2177419354838709686, 0.2204301075268817189, 0.2231182795698924692, 0.2258064516129032195, 0.2284946236559139698, 0.2311827956989247201, 0.2338709677419354704, 0.2365591397849462485, 0.2392473118279569988, 0.2419354838709677491, 0.2446236559139784994, 0.2473118279569892497, 0.2500000000000000000, 0.2526881720430107503, 0.2553763440860215006, 0.2580645161290322509, 0.2607526881720430012, 0.2634408602150537515, 0.2661290322580645018, 0.2688172043010752521, 0.2715053763440860024, 0.2741935483870967527, 0.2768817204301075030, 0.2795698924731182533, 0.2822580645161290591, 0.2849462365591398094, 0.2876344086021505597, 0.2903225806451613100, 0.2930107526881720603, 0.2956989247311828106, 0.2983870967741935609, 0.3010752688172043112, 0.3037634408602150615, 0.3064516129032258118, 0.3091397849462365621, 0.3118279569892473124, 0.3145161290322580627, 0.3172043010752688130, 0.3198924731182795633, 0.3225806451612903136, 0.3252688172043010639, 0.3279569892473118142, 0.3306451612903225645, 0.3333333333333333148, 0.3360215053763440651, 0.3387096774193548154, 0.3413978494623655657, 0.3440860215053763715, 0.3467741935483871218, 0.3494623655913978721, 0.3521505376344086224, 0.3548387096774193727, 0.3575268817204301230, 0.3602150537634408733, 0.3629032258064516236, 0.3655913978494623739, 0.3682795698924731242, 0.3709677419354838745, 0.3736559139784946248, 0.3763440860215053752, 0.3790322580645161255, 0.3817204301075268758, 0.3844086021505376261, 0.3870967741935483764, 0.3897849462365591267, 0.3924731182795698770, 0.3951612903225806273, 0.3978494623655913776, 0.4005376344086021279, 0.4032258064516128782, 0.4059139784946236285, 0.4086021505376344343, 0.4112903225806451846, 0.4139784946236559349, 0.4166666666666666852, 0.4193548387096774355, 0.4220430107526881858, 0.4247311827956989361, 0.4274193548387096864, 0.4301075268817204367, 0.4327956989247311870, 0.4354838709677419373, 0.4381720430107526876, 0.4408602150537634379, 0.4435483870967741882, 0.4462365591397849385, 0.4489247311827956888, 0.4516129032258064391, 0.4543010752688171894, 0.4569892473118279397, 0.4596774193548386900, 0.4623655913978494403, 0.4650537634408601906, 0.4677419354838709409, 0.4704301075268817467, 0.4731182795698924970, 0.4758064516129032473, 0.4784946236559139976, 0.4811827956989247479, 0.4838709677419354982, 0.4865591397849462485, 0.4892473118279569988, 0.4919354838709677491, 0.4946236559139784994, 0.4973118279569892497, 0.5000000000000000000, 0.5026881720430107503, 0.5053763440860215006, 0.5080645161290322509, 0.5107526881720430012, 0.5134408602150537515, 0.5161290322580645018, 0.5188172043010752521, 0.5215053763440860024, 0.5241935483870967527, 0.5268817204301075030, 0.5295698924731182533, 0.5322580645161290036, 0.5349462365591397539, 0.5376344086021505042, 0.5403225806451612545, 0.5430107526881720048, 0.5456989247311827551, 0.5483870967741935054, 0.5510752688172042557, 0.5537634408602150060, 0.5564516129032257563, 0.5591397849462365066, 0.5618279569892472569, 0.5645161290322581182, 0.5672043010752688685, 0.5698924731182796188, 0.5725806451612903691, 0.5752688172043011194, 0.5779569892473118697, 0.5806451612903226200, 0.5833333333333333703, 0.5860215053763441206, 0.5887096774193548709, 0.5913978494623656212, 0.5940860215053763715, 0.5967741935483871218, 0.5994623655913978721, 0.6021505376344086224, 0.6048387096774193727, 0.6075268817204301230, 0.6102150537634408733, 0.6129032258064516236, 0.6155913978494623739, 0.6182795698924731242, 0.6209677419354838745, 0.6236559139784946248, 0.6263440860215053752, 0.6290322580645161255, 0.6317204301075268758, 0.6344086021505376261, 0.6370967741935483764, 0.6397849462365591267, 0.6424731182795698770, 0.6451612903225806273, 0.6478494623655913776, 0.6505376344086021279, 0.6532258064516128782, 0.6559139784946236285, 0.6586021505376343788, 0.6612903225806451291, 0.6639784946236558794, 0.6666666666666666297, 0.6693548387096773800, 0.6720430107526881303, 0.6747311827956988806, 0.6774193548387096309, 0.6801075268817203812, 0.6827956989247311315, 0.6854838709677418818, 0.6881720430107527431, 0.6908602150537634934, 0.6935483870967742437, 0.6962365591397849940, 0.6989247311827957443, 0.7016129032258064946, 0.7043010752688172449, 0.7069892473118279952, 0.7096774193548387455, 0.7123655913978494958, 0.7150537634408602461, 0.7177419354838709964, 0.7204301075268817467, 0.7231182795698924970, 0.7258064516129032473, 0.7284946236559139976, 0.7311827956989247479, 0.7338709677419354982, 0.7365591397849462485, 0.7392473118279569988, 0.7419354838709677491, 0.7446236559139784994, 0.7473118279569892497, 0.7500000000000000000, 0.7526881720430107503, 0.7553763440860215006, 0.7580645161290322509, 0.7607526881720430012, 0.7634408602150537515, 0.7661290322580645018, 0.7688172043010752521, 0.7715053763440860024, 0.7741935483870967527, 0.7768817204301075030, 0.7795698924731182533, 0.7822580645161290036, 0.7849462365591397539, 0.7876344086021505042, 0.7903225806451612545, 0.7930107526881720048, 0.7956989247311827551, 0.7983870967741935054, 0.8010752688172042557, 0.8037634408602150060, 0.8064516129032257563, 0.8091397849462365066, 0.8118279569892472569, 0.8145161290322581182, 0.8172043010752688685, 0.8198924731182796188, 0.8225806451612903691, 0.8252688172043011194, 0.8279569892473118697, 0.8306451612903226200, 0.8333333333333333703, 0.8360215053763441206, 0.8387096774193548709, 0.8413978494623656212, 0.8440860215053763715, 0.8467741935483871218, 0.8494623655913978721, 0.8521505376344086224, 0.8548387096774193727, 0.8575268817204301230, 0.8602150537634408733, 0.8629032258064516236, 0.8655913978494623739, 0.8682795698924731242, 0.8709677419354838745, 0.8736559139784946248, 0.8763440860215053752, 0.8790322580645161255, 0.8817204301075268758, 0.8844086021505376261, 0.8870967741935483764, 0.8897849462365591267, 0.8924731182795698770, 0.8951612903225806273, 0.8978494623655913776, 0.9005376344086021279, 0.9032258064516128782, 0.9059139784946236285, 0.9086021505376343788, 0.9112903225806451291, 0.9139784946236558794, 0.9166666666666666297, 0.9193548387096773800, 0.9220430107526881303, 0.9247311827956988806, 0.9274193548387096309, 0.9301075268817203812, 0.9327956989247311315, 0.9354838709677418818, 0.9381720430107527431, 0.9408602150537634934, 0.9435483870967742437, 0.9462365591397849940, 0.9489247311827957443, 0.9516129032258064946, 0.9543010752688172449, 0.9569892473118279952, 0.9596774193548387455, 0.9623655913978494958, 0.9650537634408602461, 0.9677419354838709964, 0.9704301075268817467, 0.9731182795698924970, 0.9758064516129032473, 0.9784946236559139976, 0.9811827956989247479, 0.9838709677419354982, 0.9855363728105643872 ),
 .UNSPECIFIED. ) 
 CURVE ( )  GEOMETRIC_REPRESENTATION_ITEM ( )  RATIONAL_B_SPLINE_CURVE ( ( 1.000000000000000000, 0.8660254037844387076, 1.000000000000000000, 0.8660254037844387076, 1.000000000000000000, 0.8660254037844387076, 1.000000000000000000, 0.8660254037844387076, 1.000000000000000000, 0.8660254037844387076, 1.000000000000000000, 0.8660254037844387076, 1.000000000000000000, 0.8660254037844387076, 1.000000000000000000, 0.8660254037844387076, 1.000000000000000000, 0.8660254037844387076, 1.000000000000000000, 0.8660254037844387076, 1.000000000000000000, 0.8660254037844387076, 1.000000000000000000, 0.8660254037844387076, 1.000000000000000000, 0.8660254037844387076, 1.000000000000000000, 0.8660254037844387076, 1.000000000000000000, 0.8660254037844387076, 1.000000000000000000, 0.8660254037844387076, 1.000000000000000000, 0.8660254037844387076, 1.000000000000000000, 0.8660254037844387076, 1.000000000000000000, 0.8660254037844387076, 1.000000000000000000, 0.8660254037844387076, 1.000000000000000000, 0.8660254037844387076, 1.000000000000000000, 0.8660254037844387076, 1.000000000000000000, 0.8660254037844387076, 1.000000000000000000, 0.8660254037844387076, 1.000000000000000000, 0.8660254037844387076, 1.000000000000000000, 0.8660254037844387076, 1.000000000000000000, 0.8660254037844387076, 1.000000000000000000, 0.8660254037844387076, 1.000000000000000000, 0.8660254037844387076, 1.000000000000000000, 0.8660254037844387076, 1.000000000000000000, 0.8660254037844387076, 1.000000000000000000, 0.8660254037844387076, 1.000000000000000000, 0.8660254037844387076, 1.000000000000000000, 0.8660254037844387076, 1.000000000000000000, 0.8660254037844387076, 1.000000000000000000, 0.8660254037844387076, 1.000000000000000000, 0.8660254037844387076, 1.000000000000000000, 0.8660254037844387076, 1.000000000000000000, 0.8660254037844387076, 1.000000000000000000, 0.8660254037844387076, 1.000000000000000000, 0.8660254037844387076, 1.000000000000000000, 0.8660254037844387076, 1.000000000000000000, 0.8660254037844387076, 1.000000000000000000, 0.8660254037844387076, 1.000000000000000000, 0.8660254037844387076, 1.000000000000000000, 0.8660254037844387076, 1.000000000000000000, 0.8660254037844387076, 1.000000000000000000, 0.8660254037844387076, 1.000000000000000000, 0.8660254037844387076, 1.000000000000000000, 0.8660254037844387076, 1.000000000000000000, 0.8660254037844387076, 1.000000000000000000, 0.8660254037844387076, 1.000000000000000000, 0.8660254037844387076, 1.000000000000000000, 0.8660254037844387076, 1.000000000000000000, 0.8660254037844387076, 1.000000000000000000, 0.8660254037844387076, 1.000000000000000000, 0.8660254037844387076, 1.000000000000000000, 0.8660254037844387076, 1.000000000000000000, 0.8660254037844387076, 1.000000000000000000, 0.8660254037844387076, 1.000000000000000000, 0.8660254037844387076, 1.000000000000000000, 0.8660254037844387076, 1.000000000000000000, 0.8660254037844387076, 1.000000000000000000, 0.8660254037844387076, 1.000000000000000000, 0.8660254037844387076, 1.000000000000000000, 0.8660254037844387076, 1.000000000000000000, 0.8660254037844387076, 1.000000000000000000, 0.8660254037844387076, 1.000000000000000000, 0.8660254037844387076, 1.000000000000000000, 0.8660254037844387076, 1.000000000000000000, 0.8660254037844387076, 1.000000000000000000, 0.8660254037844387076, 1.000000000000000000, 0.8660254037844387076, 1.000000000000000000, 0.8660254037844387076, 1.000000000000000000, 0.8660254037844387076, 1.000000000000000000, 0.8660254037844387076, 1.000000000000000000, 0.8660254037844387076, 1.000000000000000000, 0.8660254037844387076, 1.000000000000000000, 0.8660254037844387076, 1.000000000000000000, 0.8660254037844387076, 1.000000000000000000, 0.8660254037844387076, 1.000000000000000000, 0.8660254037844387076, 1.000000000000000000, 0.8660254037844387076, 1.000000000000000000, 0.8660254037844387076, 1.000000000000000000, 0.8660254037844387076, 1.000000000000000000, 0.8660254037844387076, 1.000000000000000000, 0.8660254037844387076, 1.000000000000000000, 0.8660254037844387076, 1.000000000000000000, 0.8660254037844387076, 1.000000000000000000, 0.8660254037844387076, 1.000000000000000000, 0.8660254037844387076, 1.000000000000000000, 0.8660254037844387076, 1.000000000000000000, 0.8660254037844387076, 1.000000000000000000, 0.8660254037844387076, 1.000000000000000000, 0.8660254037844387076, 1.000000000000000000, 0.8660254037844387076, 1.000000000000000000, 0.8660254037844387076, 1.000000000000000000, 0.8660254037844387076, 1.000000000000000000, 0.8660254037844387076, 1.000000000000000000, 0.8660254037844387076, 1.000000000000000000, 0.8660254037844387076, 1.000000000000000000, 0.8660254037844387076, 1.000000000000000000, 0.8660254037844387076, 1.000000000000000000, 0.8660254037844387076, 1.000000000000000000, 0.8660254037844387076, 1.000000000000000000, 0.8660254037844387076, 1.000000000000000000, 0.8660254037844387076, 1.000000000000000000, 0.8660254037844387076, 1.000000000000000000, 0.8660254037844387076, 1.000000000000000000, 0.8660254037844387076, 1.000000000000000000, 0.8660254037844387076, 1.000000000000000000, 0.8660254037844387076, 1.000000000000000000, 0.8660254037844387076, 1.000000000000000000, 0.8660254037844387076, 1.000000000000000000, 0.8660254037844387076, 1.000000000000000000, 0.8660254037844387076, 1.000000000000000000, 0.8660254037844387076, 1.000000000000000000, 0.8660254037844387076, 1.000000000000000000, 0.8660254037844387076, 1.000000000000000000, 0.8660254037844387076, 1.000000000000000000, 0.8660254037844387076, 1.000000000000000000, 0.8660254037844387076, 1.000000000000000000, 0.8660254037844387076, 1.000000000000000000, 0.8660254037844387076, 1.000000000000000000, 0.8660254037844387076, 1.000000000000000000, 0.8660254037844387076, 1.000000000000000000, 0.8660254037844387076, 1.000000000000000000, 0.8660254037844387076, 1.000000000000000000, 0.8660254037844387076, 1.000000000000000000, 0.8660254037844387076, 1.000000000000000000, 0.8660254037844387076, 1.000000000000000000, 0.8660254037844387076, 1.000000000000000000, 0.8660254037844387076, 1.000000000000000000, 0.8660254037844387076, 1.000000000000000000, 0.8660254037844387076, 1.000000000000000000, 0.8660254037844387076, 1.000000000000000000, 0.8660254037844387076, 1.000000000000000000, 0.8660254037844387076, 1.000000000000000000, 0.8660254037844387076, 1.000000000000000000, 0.8660254037844387076, 1.000000000000000000, 0.8660254037844387076, 1.000000000000000000, 0.8660254037844387076, 1.000000000000000000, 0.8660254037844387076, 1.000000000000000000, 0.8660254037844387076, 1.000000000000000000, 0.8660254037844387076, 1.000000000000000000, 0.8660254037844387076, 1.000000000000000000, 0.8660254037844387076, 1.000000000000000000, 0.8660254037844387076, 1.000000000000000000, 0.8660254037844387076, 1.000000000000000000, 0.8660254037844387076, 1.000000000000000000, 0.8660254037844387076, 1.000000000000000000, 0.8660254037844387076, 1.000000000000000000, 0.8660254037844387076, 1.000000000000000000, 0.8660254037844387076, 1.000000000000000000, 0.8660254037844387076, 1.000000000000000000, 0.8660254037844387076, 1.000000000000000000, 0.8660254037844387076, 1.000000000000000000, 0.8660254037844387076, 1.000000000000000000, 0.8660254037844387076, 1.000000000000000000, 0.8660254037844387076, 1.000000000000000000, 0.8660254037844387076, 1.000000000000000000, 0.8660254037844387076, 1.000000000000000000, 0.8660254037844387076, 1.000000000000000000, 0.8660254037844387076, 1.000000000000000000, 0.8660254037844387076, 1.000000000000000000, 0.8660254037844387076, 1.000000000000000000, 0.8660254037844387076, 1.000000000000000000, 0.8660254037844387076, 1.000000000000000000, 0.8660254037844387076, 1.000000000000000000, 0.8660254037844387076, 1.000000000000000000, 0.8660254037844387076, 1.000000000000000000, 0.8660254037844387076, 1.000000000000000000, 0.8660254037844387076, 1.000000000000000000, 0.8660254037844387076, 1.000000000000000000, 0.8660254037844387076, 1.000000000000000000, 0.8660254037844387076, 1.000000000000000000, 0.8660254037844387076, 1.000000000000000000, 0.8660254037844387076, 1.000000000000000000, 0.8660254037844387076, 1.000000000000000000, 0.8660254037844387076, 1.000000000000000000, 0.8660254037844387076, 1.000000000000000000, 0.8660254037844387076, 1.000000000000000000, 0.8660254037844387076, 1.000000000000000000, 0.8660254037844387076, 1.000000000000000000, 0.8660254037844387076, 1.000000000000000000, 0.8660254037844387076, 1.000000000000000000, 0.8660254037844387076, 1.000000000000000000, 0.8660254037844387076, 1.000000000000000000, 0.8660254037844387076, 1.000000000000000000, 0.8660254037844387076, 1.000000000000000000, 0.8660254037844387076, 1.000000000000000000, 0.8660254037844387076, 1.000000000000000000, 0.8660254037844387076, 1.000000000000000000, 0.8660254037844387076, 1.000000000000000000, 0.8660254037844387076, 1.000000000000000000, 0.8660254037844387076, 1.000000000000000000, 0.8660254037844387076, 1.000000000000000000, 0.8660254037844387076, 1.000000000000000000, 0.8660254037844387076, 1.000000000000000000, 0.8660254037844387076, 1.000000000000000000, 0.8660254037844387076, 1.000000000000000000, 0.8660254037844387076, 1.000000000000000000, 0.8660254037844387076, 1.000000000000000000, 0.8660254037844387076, 1.000000000000000000, 0.8660254037844387076, 1.000000000000000000, 0.8660254037844387076, 1.000000000000000000, 0.8660254037844387076, 1.000000000000000000, 0.8660254037844387076, 1.000000000000000000, 0.8660254037844387076, 1.000000000000000000, 0.8660254037844387076, 1.000000000000000000, 0.8660254037844387076, 1.000000000000000000, 0.8660254037844387076, 1.000000000000000000, 0.8660254037844387076, 1.000000000000000000, 0.8660254037844387076, 1.000000000000000000, 0.8660254037844387076, 1.000000000000000000, 0.8660254037844387076, 1.000000000000000000, 0.8660254037844387076, 1.000000000000000000, 0.8660254037844387076, 1.000000000000000000, 0.8660254037844387076, 1.000000000000000000, 0.8660254037844387076, 1.000000000000000000, 0.8660254037844387076, 1.000000000000000000, 0.8660254037844387076, 1.000000000000000000, 0.8660254037844387076, 1.000000000000000000, 0.8660254037844387076, 1.000000000000000000, 0.8660254037844387076, 1.000000000000000000, 0.8660254037844387076, 1.000000000000000000, 0.8660254037844387076, 1.000000000000000000, 0.8660254037844387076, 1.000000000000000000, 0.8660254037844387076, 1.000000000000000000, 0.8660254037844387076, 1.000000000000000000, 0.8660254037844387076, 1.000000000000000000, 0.8660254037844387076, 1.000000000000000000, 0.8660254037844387076, 1.000000000000000000, 0.8660254037844387076, 1.000000000000000000, 0.8660254037844387076, 1.000000000000000000, 0.8660254037844387076, 1.000000000000000000, 0.8660254037844387076, 1.000000000000000000, 0.8660254037844387076, 1.000000000000000000, 0.8660254037844387076, 1.000000000000000000, 0.8660254037844387076, 1.000000000000000000, 0.8660254037844387076, 1.000000000000000000, 0.8660254037844387076, 1.000000000000000000, 0.8660254037844387076, 1.000000000000000000, 0.8660254037844387076, 1.000000000000000000, 0.8660254037844387076, 1.000000000000000000, 0.8660254037844387076, 1.000000000000000000, 0.8660254037844387076, 1.000000000000000000, 0.8660254037844387076, 1.000000000000000000, 0.8660254037844387076, 1.000000000000000000, 0.8660254037844387076, 1.000000000000000000, 0.8660254037844387076, 1.000000000000000000, 0.8660254037844387076, 1.000000000000000000, 0.8660254037844387076, 1.000000000000000000, 0.8660254037844387076, 1.000000000000000000, 0.8660254037844387076, 1.000000000000000000, 0.8660254037844387076, 1.000000000000000000, 0.8660254037844387076, 1.000000000000000000, 0.8660254037844387076, 1.000000000000000000, 0.8660254037844387076, 1.000000000000000000, 0.8660254037844387076, 1.000000000000000000, 0.8660254037844387076, 1.000000000000000000, 0.8660254037844387076, 1.000000000000000000, 0.8660254037844387076, 1.000000000000000000, 0.8660254037844387076, 1.000000000000000000, 0.8660254037844387076, 1.000000000000000000, 0.8660254037844387076, 1.000000000000000000, 0.8660254037844387076, 1.000000000000000000, 0.8660254037844387076, 1.000000000000000000, 0.8660254037844387076, 1.000000000000000000, 0.8660254037844387076, 1.000000000000000000, 0.8660254037844387076, 1.000000000000000000, 0.8660254037844387076, 1.000000000000000000, 0.8660254037844387076, 1.000000000000000000, 0.8660254037844387076, 1.000000000000000000, 0.8660254037844387076, 1.000000000000000000, 0.8660254037844387076, 1.000000000000000000, 0.8660254037844387076, 1.000000000000000000, 0.8660254037844387076, 1.000000000000000000, 0.8660254037844387076, 1.000000000000000000, 0.8660254037844387076, 1.000000000000000000, 0.8660254037844387076, 1.000000000000000000, 0.8660254037844387076, 1.000000000000000000, 0.8660254037844387076, 1.000000000000000000, 0.8660254037844387076, 1.000000000000000000, 0.8660254037844387076, 1.000000000000000000, 0.8660254037844387076, 1.000000000000000000, 0.8660254037844387076, 1.000000000000000000, 0.8660254037844387076, 1.000000000000000000, 0.8660254037844387076, 1.000000000000000000, 0.8660254037844387076, 1.000000000000000000, 0.8660254037844387076, 1.000000000000000000, 0.8660254037844387076, 1.000000000000000000, 0.8660254037844387076, 1.000000000000000000, 0.8660254037844387076, 1.000000000000000000, 0.8660254037844387076, 1.000000000000000000, 0.8660254037844387076, 1.000000000000000000, 0.8660254037844387076, 1.000000000000000000, 0.8660254037844387076, 1.000000000000000000, 0.8660254037844387076, 1.000000000000000000, 0.8660254037844387076, 1.000000000000000000, 0.8660254037844387076, 1.000000000000000000, 0.8660254037844387076, 1.000000000000000000, 0.8660254037844387076, 1.000000000000000000, 0.8660254037844387076, 1.000000000000000000, 0.8660254037844387076, 1.000000000000000000, 0.8660254037844387076, 1.000000000000000000, 0.8660254037844387076, 1.000000000000000000, 0.8660254037844387076, 1.000000000000000000, 0.8660254037844387076, 1.000000000000000000, 0.8660254037844387076, 1.000000000000000000, 0.8660254037844387076, 1.000000000000000000, 0.8660254037844387076, 1.000000000000000000, 0.8660254037844387076, 1.000000000000000000, 0.8660254037844387076, 1.000000000000000000, 0.8660254037844387076, 1.000000000000000000, 0.8660254037844387076, 1.000000000000000000, 0.8660254037844387076, 1.000000000000000000, 0.8660254037844387076, 1.000000000000000000, 0.8660254037844387076, 1.000000000000000000, 0.8660254037844387076, 1.000000000000000000, 0.8660254037844387076, 1.000000000000000000, 0.8660254037844387076, 1.000000000000000000, 0.8660254037844387076, 1.000000000000000000, 0.8660254037844387076, 1.000000000000000000, 0.8660254037844387076, 1.000000000000000000, 0.8660254037844387076, 1.000000000000000000, 0.8660254037844387076, 1.000000000000000000, 0.8660254037844387076, 1.000000000000000000, 0.8660254037844387076, 1.000000000000000000, 0.8660254037844387076, 1.000000000000000000, 0.8660254037844387076, 1.000000000000000000, 0.8660254037844387076, 1.000000000000000000, 0.8660254037844387076, 1.000000000000000000, 0.8660254037844387076, 1.000000000000000000, 0.8660254037844387076, 1.000000000000000000, 0.8660254037844387076, 1.000000000000000000, 0.8660254037844387076, 1.000000000000000000, 0.8660254037844387076, 1.000000000000000000, 0.8660254037844387076, 1.000000000000000000, 0.8660254037844387076, 1.000000000000000000, 0.8660254037844387076, 1.000000000000000000, 0.8660254037844387076, 1.000000000000000000, 0.8660254037844387076, 1.000000000000000000, 0.8660254037844387076, 1.000000000000000000, 0.8660254037844387076, 1.000000000000000000, 0.8660254037844387076, 1.000000000000000000, 0.8660254037844387076, 1.000000000000000000, 0.8660254037844387076, 1.000000000000000000, 0.8660254037844387076, 1.000000000000000000, 0.8660254037844387076, 1.000000000000000000, 0.8660254037844387076, 1.000000000000000000, 0.8660254037844387076, 1.000000000000000000, 0.8660254037844387076, 1.000000000000000000, 0.8660254037844387076, 1.000000000000000000, 0.8660254037844387076, 1.000000000000000000, 0.8660254037844387076, 1.000000000000000000, 0.8660254037844387076, 1.000000000000000000, 0.8660254037844387076, 1.000000000000000000, 0.8660254037844387076, 1.000000000000000000, 0.8660254037844387076, 1.000000000000000000, 0.8660254037844387076, 1.000000000000000000, 0.8660254037844387076, 1.000000000000000000, 0.8660254037844387076, 1.000000000000000000, 0.8660254037844387076, 1.000000000000000000, 0.8660254037844387076, 1.000000000000000000, 0.8660254037844387076, 1.000000000000000000, 0.9169986265629754829, 0.9368410486966849415 ) ) 
 REPRESENTATION_ITEM ( '' )  );
#7873 = CARTESIAN_POINT ( 'NONE',  ( 82.79468719140261612, 43.39660814947434631, 7.776906916868496111 ) ) ;
#7874 = CARTESIAN_POINT ( 'NONE',  ( 153.6043694648998894, 279.0369973721463452, 3.800317288925857628 ) ) ;
#7875 = CARTESIAN_POINT ( 'NONE',  ( 22.04262502322622908, 183.5333772461660544, 9.188101187500095079 ) ) ;
#7876 = CARTESIAN_POINT ( 'NONE',  ( 113.4351080945290278, 245.4869531367911009, 4.594050593750046652 ) ) ;
#7877 = CARTESIAN_POINT ( 'NONE',  ( 183.1556239524084333, 257.7435932540183217, -2.690512520808968411 ) ) ;
#7878 = VERTEX_POINT ( 'NONE', #12662 ) ;
#7879 = CARTESIAN_POINT ( 'NONE',  ( 34.87168918123982309, 179.3932355074535394, -2.679491924311248496 ) ) ;
#7880 = CARTESIAN_POINT ( 'NONE',  ( 175.3097973626215662, 281.1046532212878901, -14.83871771951074692 ) ) ;
#7881 = VECTOR ( 'NONE', #69671, 1000.000000000000000 ) ;
#7882 = CARTESIAN_POINT ( 'NONE',  ( 139.8153705705071843, 239.9824982072973967, 3.021315404115420679E-15 ) ) ;
#7883 = CARTESIAN_POINT ( 'NONE',  ( 200.6117230619925635, 269.0360104864248001, 9.242361455687714056 ) ) ;
#7884 = CARTESIAN_POINT ( 'NONE',  ( 155.2419697281468416, 261.7600162942170527, 18.58580762350309357 ) ) ;
#7885 = CARTESIAN_POINT ( 'NONE',  ( 207.1158949475991164, 271.9117422260973740, -5.823035679195911918 ) ) ;
#7886 = CARTESIAN_POINT ( 'NONE',  ( -40.67952639183666008, 27.60432558407080350, -10.00000000000000000 ) ) ;
#7887 = CARTESIAN_POINT ( 'NONE',  ( 147.9500839974939197, 274.3899328626944225, -9.375093207164509224 ) ) ;
#7888 = CARTESIAN_POINT ( 'NONE',  ( 190.4677317829447247, 263.8822203009034411, 7.824480301607388277 ) ) ;
#7889 = CARTESIAN_POINT ( 'NONE',  ( 167.8570435341544567, 278.4618103485150868, 14.78497630034688726 ) ) ;
#7890 = CARTESIAN_POINT ( 'NONE',  ( 176.5481980778163518, 256.7330344388156504, -11.15910957749502330 ) ) ;
#7891 = CARTESIAN_POINT ( 'NONE',  ( 69.54386771901253894, 69.60617901769191462, 5.634068191784291635 ) ) ;
#7892 = CARTESIAN_POINT ( 'NONE',  ( 189.8763472015711216, 301.7715148217271803, -0.1184663095182975079 ) ) ;
#7893 = CARTESIAN_POINT ( 'NONE',  ( 181.1200065746923826, 266.1666110466232453, -14.84348402710393877 ) ) ;
#7894 = ORIENTED_EDGE ( 'NONE', *, *, #59618, .F. ) ;
#7895 = CARTESIAN_POINT ( 'NONE',  ( 32.30839531297598910, 123.0650415295850593, 203.6502102582797420 ) ) ;
#7896 = EDGE_CURVE ( 'NONE', #94177, #57995, #74956, .T. ) ;
#7897 = CARTESIAN_POINT ( 'NONE',  ( 163.7423057141168385, 247.0370024851108610, -6.909410042141566066 ) ) ;
#7898 = CARTESIAN_POINT ( 'NONE',  ( 30.62257814894733698, 105.2525989182601194, 59.99999999999999289 ) ) ;
#7899 = CARTESIAN_POINT ( 'NONE',  ( 91.43256340568937901, 235.8464784336661353, 1.353441290958777327E-15 ) ) ;
#7900 = CARTESIAN_POINT ( 'NONE',  ( 17.35761498915574563, 12.94754757982088300, 5.678558825948272215 ) ) ;
#7901 = CARTESIAN_POINT ( 'NONE',  ( -6.813555604197667037, 155.3262482093457777, -6.972266317189433020E-16 ) ) ;
#7902 = DIRECTION ( 'NONE',  ( 0.000000000000000000, 0.3470917258701495256, -0.9378311862123592801 ) ) ;
#7904 = CARTESIAN_POINT ( 'NONE',  ( 195.0772487819253911, 279.0847438180149993, 16.30750567507551096 ) ) ;
#7903 = DIRECTION ( 'NONE',  ( -0.3473448497826165382, 0.9377374661009827417, 0.000000000000000000 ) ) ;
#7905 = CARTESIAN_POINT ( 'NONE',  ( 155.0898067732971697, 280.3139227198241201, -4.343794903066061863 ) ) ;
#7906 = CARTESIAN_POINT ( 'NONE',  ( -65.00000000000000000, 10.00000000000000178, 59.99999999999999289 ) ) ;
#7907 = CARTESIAN_POINT ( 'NONE',  ( 146.0195742355162452, 245.1115022471902023, -5.000000000000041744 ) ) ;
#7908 = FACE_OUTER_BOUND ( 'NONE', #76573, .T. ) ;
#7909 = CARTESIAN_POINT ( 'NONE',  ( 204.2143397907769611, 276.5280330293650195, 13.36303585211030054 ) ) ;
#7910 = LINE ( 'NONE', #55967, #53942 ) ;
#7911 = ORIENTED_EDGE ( 'NONE', *, *, #99719, .T. ) ;
#7912 = CARTESIAN_POINT ( 'NONE',  ( 192.7785635360272352, 266.6923795695631156, 11.52468468594655526 ) ) ;
#7913 = CARTESIAN_POINT ( 'NONE',  ( 32.08968265630385019, 27.03085787977765264, 9.188101187500006262 ) ) ;
#7914 = CARTESIAN_POINT ( 'NONE',  ( 196.1370092075112268, 290.1209220278959720, 16.40156295354631411 ) ) ;
#7915 = CARTESIAN_POINT ( 'NONE',  ( 200.6117230619925635, 269.0360104864248001, 9.242361455687714056 ) ) ;
#7916 = DIRECTION ( 'NONE',  ( -0.5000000000000001110, 0.8660254037844384856, 0.000000000000000000 ) ) ;
#7917 = EDGE_CURVE ( 'NONE', #98290, #59369, #13646, .T. ) ;
#7918 = ORIENTED_EDGE ( 'NONE', *, *, #59421, .T. ) ;
#7919 = LINE ( 'NONE', #17379, #50220 ) ;
#7920 = CARTESIAN_POINT ( 'NONE',  ( 49.63464994930628649, 103.0251469596019120, -10.00000000000000000 ) ) ;
#7921 = CARTESIAN_POINT ( 'NONE',  ( 179.9071714477294961, 262.8436713092991113, -12.82472271075318737 ) ) ;
#7922 = CARTESIAN_POINT ( 'NONE',  ( 44.18536904650256503, 64.34838820550514527, -10.00000000000000000 ) ) ;
#7923 = CARTESIAN_POINT ( 'NONE',  ( 152.7153488183568300, 266.1362520814392951, 17.33540622643059237 ) ) ;
#7924 = VERTEX_POINT ( 'NONE', #74470 ) ;
#7925 = CARTESIAN_POINT ( 'NONE',  ( 73.07852875935716952, 69.76346136681742394, 9.633212380859575319 ) ) ;
#7926 = AXIS2_PLACEMENT_3D ( 'NONE', #70764, #70255, #16561 ) ;
#7927 = CARTESIAN_POINT ( 'NONE',  ( 35.97235683590213284, 38.95586893147758190, 7.433330006724141015 ) ) ;
#7928 = VERTEX_POINT ( 'NONE', #51128 ) ;
#7929 = CARTESIAN_POINT ( 'NONE',  ( 163.7166294601506991, 282.3380383384618995, 10.03031969300557513 ) ) ;
#7930 = CARTESIAN_POINT ( 'NONE',  ( 89.29477061917849312, 46.06123908072883921, 1.850091733736755357E-15 ) ) ;
#7931 = VERTEX_POINT ( 'NONE', #44519 ) ;
#7932 = CARTESIAN_POINT ( 'NONE',  ( 86.46734690923850053, 47.05374834302038067, -10.53985889464877523 ) ) ;
#7933 = CARTESIAN_POINT ( 'NONE',  ( 206.1014820340073186, 273.6687569322920126, 12.23319432534553108 ) ) ;
#7934 = CARTESIAN_POINT ( 'NONE',  ( 84.47262166381923976, 50.18302823219130460, 13.87459367389479326 ) ) ;
#7935 = CARTESIAN_POINT ( 'NONE',  ( 193.1476055184262464, 296.1055292122517244, -12.13892458995638535 ) ) ;
#7936 = DIRECTION ( 'NONE',  ( 1.000000000000000000, 0.000000000000000000, 0.000000000000000000 ) ) ;
#7938 = EDGE_CURVE ( 'NONE', #9864, #22636, #50502, .T. ) ;
#7937 = AXIS2_PLACEMENT_3D ( 'NONE', #20205, #12102, #34397 ) ;
#7939 = CARTESIAN_POINT ( 'NONE',  ( 23.64814127513158937, 118.0650415295850451, -24.99999999999999289 ) ) ;
#7940 = CARTESIAN_POINT ( 'NONE',  ( 45.84141126897937824, 27.26216523072498532, -2.296566073217252530E-15 ) ) ;
#7941 = CARTESIAN_POINT ( 'NONE',  ( 81.49556199178041993, 55.44509743070403118, -16.31886845347543158 ) ) ;
#7942 = EDGE_LOOP ( 'NONE', ( #41453, #80243, #46344, #86963 ) ) ;
#7943 = CARTESIAN_POINT ( 'NONE',  ( 163.2237683175472398, 249.5215337783042173, 11.38175491140649598 ) ) ;
#7944 = ORIENTED_EDGE ( 'NONE', *, *, #12713, .T. ) ;
#7945 = ORIENTED_EDGE ( 'NONE', *, *, #10017, .T. ) ;
#7946 = CARTESIAN_POINT ( 'NONE',  ( 87.13833003848017711, 45.89157147215227894, -8.651152695689850347 ) ) ;
#7947 = AXIS2_PLACEMENT_3D ( 'NONE', #41847, #72795, #81398 ) ;
#7948 = EDGE_LOOP ( 'NONE', ( #22873, #24495, #78486, #63746 ) ) ;
#7949 = CARTESIAN_POINT ( 'NONE',  ( 165.4922176576098138, 275.0575853646175233, -16.02269507257410908 ) ) ;
#7950 = CARTESIAN_POINT ( 'NONE',  ( 206.7044739906782809, 272.6243442267827959, -10.28926534613781030 ) ) ;
#7951 = CARTESIAN_POINT ( 'NONE',  ( 148.4832040919255292, 276.1351389192656143, -5.425582376124524764 ) ) ;
#7952 = DIRECTION ( 'NONE',  ( -0.000000000000000000, -1.000000000000000000, -0.000000000000000000 ) ) ;
#7953 = CARTESIAN_POINT ( 'NONE',  ( 30.34687108590969373, 93.06504152958497400, -45.00000000000001421 ) ) ;
#7954 = CARTESIAN_POINT ( 'NONE',  ( 182.0016526522884135, 263.2485514694740800, 14.07076055901416112 ) ) ;
#7955 = CARTESIAN_POINT ( 'NONE',  ( 32.24342178309110096, 47.97677246190463052, -10.00000000000000000 ) ) ;
#7956 = CARTESIAN_POINT ( 'NONE',  ( 183.4628397030323015, 284.7042858584374017, -15.01390401402201213 ) ) ;
#7957 = CARTESIAN_POINT ( 'NONE',  ( 122.2582625392304863, 232.2048013555409796, 4.594050593750051981 ) ) ;
#7958 = CARTESIAN_POINT ( 'NONE',  ( 186.4788919898187203, 262.6505567889508370, -9.037439985774382123 ) ) ;
#7959 = CARTESIAN_POINT ( 'NONE',  ( 45.84141126897937824, 27.26216523072498887, -2.296566073217252530E-15 ) ) ;
#7960 = CARTESIAN_POINT ( 'NONE',  ( 177.3572886147324823, 288.7233493041218821, -9.936058525762780036 ) ) ;
#7961 = ORIENTED_EDGE ( 'NONE', *, *, #43432, .T. ) ;
#7962 = AXIS2_PLACEMENT_3D ( 'NONE', #63084, #40268, #15987 ) ;
#7963 = ORIENTED_EDGE ( 'NONE', *, *, #4460, .F. ) ;
#7964 = FACE_OUTER_BOUND ( 'NONE', #38206, .T. ) ;
#7965 = CARTESIAN_POINT ( 'NONE',  ( 76.39071540512284741, 62.51181499478219905, -15.22731582648911797 ) ) ;
#7966 = CARTESIAN_POINT ( 'NONE',  ( 180.2794780956456293, 294.9385830392915864, -2.005224010670390022 ) ) ;
#7967 = CARTESIAN_POINT ( 'NONE',  ( 203.5726949774746117, 269.0034548673361883, -6.096665150295551783 ) ) ;
#7968 = CARTESIAN_POINT ( 'NONE',  ( 72.98212971150626061, 65.41051458920003370, 12.90293089110194380 ) ) ;
#7969 = CARTESIAN_POINT ( 'NONE',  ( 201.3053499423511425, 281.9759013948520874, -16.75960365258566398 ) ) ;
#7970 = CARTESIAN_POINT ( 'NONE',  ( 173.8410576106227552, 287.9787963164463918, -9.990854418439887752 ) ) ;
#7971 = ORIENTED_EDGE ( 'NONE', *, *, #96808, .F. ) ;
#7972 = DIRECTION ( 'NONE',  ( -0.000000000000000000, 0.000000000000000000, 1.000000000000000000 ) ) ;
#7973 = CARTESIAN_POINT ( 'NONE',  ( 175.9428832018305400, 255.2228740406303871, -7.310609490979488534 ) ) ;
#7974 = ORIENTED_EDGE ( 'NONE', *, *, #37580, .T. ) ;
#7975 = CARTESIAN_POINT ( 'NONE',  ( 148.1632261683078013, 274.0207597936089883, -7.853210555358286271 ) ) ;
#7976 = CARTESIAN_POINT ( 'NONE',  ( 200.1294354126899009, 267.3366221627135246, -6.812218948514619399 ) ) ;
#7977 = ORIENTED_EDGE ( 'NONE', *, *, #11020, .F. ) ;
#7978 = CARTESIAN_POINT ( 'NONE',  ( 191.4451218093941804, 267.1586281749990235, -12.73097342071060289 ) ) ;
#7979 = CARTESIAN_POINT ( 'NONE',  ( 160.0225884613553262, 278.6577504188115881, 10.44739908625478186 ) ) ;
#7980 = CARTESIAN_POINT ( 'NONE',  ( 193.6750207660124374, 264.1248559586345550, 4.439471659852311625 ) ) ;
#7981 = CARTESIAN_POINT ( 'NONE',  ( 158.4419986971542471, 263.4018671416569077, 17.51825679525311230 ) ) ;
#7982 = CARTESIAN_POINT ( 'NONE',  ( 204.6046391762972689, 273.0979756738785795, -10.26949011951421298 ) ) ;
#7984 = CARTESIAN_POINT ( 'NONE',  ( 160.2115073521705710, 281.2659082526984662, 5.619886021066055726 ) ) ;
#7983 = CARTESIAN_POINT ( 'NONE',  ( 152.3764452470134358, 269.7209059243594993, 14.08360062969545368 ) ) ;
#7985 = CARTESIAN_POINT ( 'NONE',  ( 200.8251833487811666, 282.8075743310126882, -16.74393672780000131 ) ) ;
#7986 = EDGE_LOOP ( 'NONE', ( #83273, #55679, #63909, #41721 ) ) ;
#7987 = CARTESIAN_POINT ( 'NONE',  ( 147.4368675721658519, 275.2788497866417288, 5.050119523016719292 ) ) ;
#7988 = CARTESIAN_POINT ( 'NONE',  ( 71.69128320130467102, 63.41209966293108380, 13.59476739478700225 ) ) ;
#7989 = CARTESIAN_POINT ( 'NONE',  ( 163.9293054476912630, 248.0008627108990993, -8.754753442298728316 ) ) ;
#7990 = DIRECTION ( 'NONE',  ( 0.4999999999999985012, -0.8660254037844394848, -1.387778780781440351E-15 ) ) ;
#7991 = CARTESIAN_POINT ( 'NONE',  ( -110.0000000000000426, 4.999999999999999112, -14.21260523776211215 ) ) ;
#7992 = EDGE_CURVE ( 'NONE', #63243, #33752, #91810, .T. ) ;
#7993 = CARTESIAN_POINT ( 'NONE',  ( 188.5978122785818414, 298.5986698468521467, -4.210741860408480974 ) ) ;
#7994 = CARTESIAN_POINT ( 'NONE',  ( 83.78033978848483798, 44.16145733190557365, 8.087935607909994218 ) ) ;
#7995 = ADVANCED_FACE ( 'NONE', ( #53131 ), #12885, .F. ) ;
#7996 = CARTESIAN_POINT ( 'NONE',  ( 57.59477206639473224, 197.3927522451417929, -10.00000000000009237 ) ) ;
#7997 = CARTESIAN_POINT ( 'NONE',  ( 194.2199708651012600, 294.2481379475345875, 15.50834247347371253 ) ) ;
#7998 = CARTESIAN_POINT ( 'NONE',  ( 84.13204908911603752, 50.42604040346916605, 13.71367173376234838 ) ) ;
#7999 = CARTESIAN_POINT ( 'NONE',  ( 71.18060993283003768, 70.65244408663559739, -5.504285530961238848 ) ) ;
#8000 = EDGE_CURVE ( 'NONE', #88645, #88734, #60942, .T. ) ;
#8001 = CARTESIAN_POINT ( 'NONE',  ( 69.94448162217048548, 217.3149278399160949, -9.188101187500095079 ) ) ;
#8002 = CARTESIAN_POINT ( 'NONE',  ( 69.28126399264922952, 70.99872114787820010, 2.214918965755282798 ) ) ;
#8004 = DIRECTION ( 'NONE',  ( 0.000000000000000000, 1.000000000000000000, 0.000000000000000000 ) ) ;
#8003 = B_SPLINE_CURVE_WITH_KNOTS ( 'NONE', 3,
 ( #70684, #86452, #94527, #10401 ),
 .UNSPECIFIED., .F., .F.,
 ( 4, 4 ),
 ( 0.01296045245666641033, 0.01919682551789810704 ),
 .UNSPECIFIED. ) ;
#8005 = CARTESIAN_POINT ( 'NONE',  ( 208.1612901671020381, 270.1010645919285480, -2.401583477149568768 ) ) ;
#8006 = ADVANCED_FACE ( 'NONE', ( #74695 ), #67047, .T. ) ;
#8008 = CARTESIAN_POINT ( 'NONE',  ( 202.8874463667715133, 279.2356300052831557, -15.29930322226033468 ) ) ;
#8007 = AXIS2_PLACEMENT_3D ( 'NONE', #31791, #22335, #47010 ) ;
#8009 = CIRCLE ( 'NONE', #90565, 10.00000000000000711 ) ;
#8010 = CARTESIAN_POINT ( 'NONE',  ( 78.66002983668515469, 59.34402786614296588, 16.16707823594543214 ) ) ;
#8011 = CARTESIAN_POINT ( 'NONE',  ( 84.87890672887020571, 50.20346095951408927, -13.33159439321596196 ) ) ;
#8012 = CARTESIAN_POINT ( 'NONE',  ( 43.23318412030275226, 195.7677522451418781, 10.00000000000009592 ) ) ;
#8014 = CARTESIAN_POINT ( 'NONE',  ( 75.93802828010240091, 51.44302491467914251, 15.68598613182542501 ) ) ;
#8013 = CARTESIAN_POINT ( 'NONE',  ( 73.46468938206548671, 69.84266834477836028, -9.805732075891272714 ) ) ;
#8015 = CARTESIAN_POINT ( 'NONE',  ( 169.2469165748500188, 252.1036659777226703, -8.798953830286828648 ) ) ;
#8016 = CARTESIAN_POINT ( 'NONE',  ( 164.0701913188777041, 246.4690879585942866, -4.479195405916993167 ) ) ;
#8017 = CARTESIAN_POINT ( 'NONE',  ( 196.0395593785976018, 291.0965181932902510, 15.97855489120023087 ) ) ;
#8018 = CARTESIAN_POINT ( 'NONE',  ( 172.3741624485570867, 252.4865239976215037, 8.880853820034850798 ) ) ;
#8019 = CARTESIAN_POINT ( 'NONE',  ( 73.12133584826474930, 57.41764960941905116, -15.88333458976553381 ) ) ;
#8020 = VECTOR ( 'NONE', #97593, 999.9999999999998863 ) ;
#8021 = CARTESIAN_POINT ( 'NONE',  ( 30.62142885764206568, 197.6744531367911293, 4.594050593750047540 ) ) ;
#8022 = CARTESIAN_POINT ( 'NONE',  ( 62.82726920452340380, 197.8923013555409796, 4.594050593750050204 ) ) ;
#8023 = CARTESIAN_POINT ( 'NONE',  ( 58.91185237153143106, 211.4865022471902876, -10.00000000000009592 ) ) ;
#8024 = CARTESIAN_POINT ( 'NONE',  ( 88.40016726344319409, 43.81338102853380434, 0.1423130075416286777 ) ) ;
#8025 = CARTESIAN_POINT ( 'NONE',  ( -6.761740748788464650, 160.2365022471902023, 10.00000000000009592 ) ) ;
#8026 = CARTESIAN_POINT ( 'NONE',  ( 77.38944774667987758, 49.20504137781674814, 15.31118821561086740 ) ) ;
#8028 = CIRCLE ( 'NONE', #95445, 70.00000000000001421 ) ;
#8027 = CARTESIAN_POINT ( 'NONE',  ( 196.4711259686879146, 269.6575937712059385, -10.81078490099711864 ) ) ;
#8029 = CARTESIAN_POINT ( 'NONE',  ( 27.91230638117223606, 28.06628583063842797, -9.188101187500006262 ) ) ;
#8030 = CARTESIAN_POINT ( 'NONE',  ( 149.0164813726494799, 272.5428784278667536, -11.67305721329070423 ) ) ;
#8031 = CARTESIAN_POINT ( 'NONE',  ( 6.943673075435188302, 24.98502408145590437, -5.678558825948271327 ) ) ;
#8032 = CARTESIAN_POINT ( 'NONE',  ( 62.50250967810423930, 197.7048013555409796, 4.594050593750051981 ) ) ;
#8033 = DIRECTION ( 'NONE',  ( 0.000000000000000000, -0.000000000000000000, 1.000000000000000000 ) ) ;
#8034 = CARTESIAN_POINT ( 'NONE',  ( 82.75623256556472995, 53.92166175363784930, -15.45821587292255472 ) ) ;
#8035 = CARTESIAN_POINT ( 'NONE',  ( 198.3075590527773784, 287.1682275260610027, 16.94807365630277118 ) ) ;
#8036 = CARTESIAN_POINT ( 'NONE',  ( 185.8492146212669240, 258.6745004276652935, -5.862532207920108540 ) ) ;
#8037 = CARTESIAN_POINT ( 'NONE',  ( 153.3739204864665169, 276.7760111581692399, 7.465203695501545056 ) ) ;
#8038 = B_SPLINE_CURVE_WITH_KNOTS ( 'NONE', 3,
 ( #29667, #22564, #28667, #84400, #90528, #67167, #83911, #60544, #51976, #6377, #14945, #82916, #13490, #14474, #30160, #37748, #44360, #75293, #45835, #5874, #84896, #21576, #76758, #61549 ),
 .UNSPECIFIED., .F., .F.,
 ( 4, 2, 2, 2, 1, 2, 2, 1, 1, 2, 2, 1, 2, 4 ),
 ( 0.000000000000000000, 0.1493091583479830842, 0.2239637375219751536, 0.2612910271089707859, 0.2986183166959664459, 0.3732728958699557120, 0.3919365406634525151, 0.4106001854569493736, 0.4479274750439458108, 0.4852547646309422480, 0.5225820542179386852, 0.5599093438049350668, 0.5785729885984347565, 0.5972366333919344461 ),
 .UNSPECIFIED. ) ;
#8039 = CARTESIAN_POINT ( 'NONE',  ( 74.31895847488682705, 57.06360514179990417, -16.02672806696303809 ) ) ;
#8040 = CARTESIAN_POINT ( 'NONE',  ( 112.2445834879231086, 235.6115022471902307, 10.00000000000009592 ) ) ;
#8041 = CARTESIAN_POINT ( 'NONE',  ( 11.48687755014677947, 188.9860189848785410, -2.679491924311252493 ) ) ;
#8042 = CARTESIAN_POINT ( 'NONE',  ( 207.6209998424140792, 271.0368748851258260, 6.610167240481342965 ) ) ;
#8043 = VERTEX_POINT ( 'NONE', #38647 ) ;
#8044 = CARTESIAN_POINT ( 'NONE',  ( 77.39365065043905645, 49.53244676146400849, 14.91118474622092016 ) ) ;
#8045 = CARTESIAN_POINT ( 'NONE',  ( 83.01075186827047503, 53.40825386585734691, 15.63370843945823019 ) ) ;
#8046 = EDGE_LOOP ( 'NONE', ( #64127, #40262, #63002, #14828, #49382, #64510 ) ) ;
#8047 = CARTESIAN_POINT ( 'NONE',  ( 206.5237403681858552, 272.9373840435757188, -10.81420335655575116 ) ) ;
#8048 = CARTESIAN_POINT ( 'NONE',  ( 194.0630436426056633, 294.0785447019548542, 13.99500891659908852 ) ) ;
#8049 = CARTESIAN_POINT ( 'NONE',  ( 71.62264301235484254, 72.47875319116253934, -0.1882495702471937982 ) ) ;
#8050 = VERTEX_POINT ( 'NONE', #93391 ) ;
#8051 = CARTESIAN_POINT ( 'NONE',  ( -19.65312891409030271, 93.06504152958497400, 177.5919119679930134 ) ) ;
#8052 = ORIENTED_EDGE ( 'NONE', *, *, #15658, .F. ) ;
#8053 = CARTESIAN_POINT ( 'NONE',  ( 65.84203434077124939, 68.97034509070658714, -2.213548117778525004 ) ) ;
#8054 = CARTESIAN_POINT ( 'NONE',  ( 194.4032909867620447, 293.9306181827685123, -16.05392006271526384 ) ) ;
#8055 = ADVANCED_FACE ( 'NONE', ( #24452 ), #39126, .F. ) ;
#8056 = ORIENTED_EDGE ( 'NONE', *, *, #58512, .F. ) ;
#8057 = CARTESIAN_POINT ( 'NONE',  ( 30.03287232231581072, 25.84335787977764554, 9.188101187500006262 ) ) ;
#8058 = LINE ( 'NONE', #53631, #53268 ) ;
#8059 = CARTESIAN_POINT ( 'NONE',  ( 179.4408063581041688, 277.4340371255875652, 17.62723233342114071 ) ) ;
#8060 = ORIENTED_EDGE ( 'NONE', *, *, #52765, .T. ) ;
#8061 = CARTESIAN_POINT ( 'NONE',  ( 182.4832887632573488, 293.7996546558092632, 9.189678001673824426 ) ) ;
#8062 = CARTESIAN_POINT ( 'NONE',  ( -3.027006198515987734, 162.3927522451418213, 10.00000000000009948 ) ) ;
#8063 = ORIENTED_EDGE ( 'NONE', *, *, #79934, .F. ) ;
#8064 = CARTESIAN_POINT ( 'NONE',  ( -19.78401074640790469, 93.01041841532075694, 59.99999999999999289 ) ) ;
#8066 = CARTESIAN_POINT ( 'NONE',  ( 67.69188770687451040, 65.70569729239960566, -10.69268924707425406 ) ) ;
#8065 = CARTESIAN_POINT ( 'NONE',  ( 67.87906010048776295, 65.45581163343211983, 10.32193553156050925 ) ) ;
#8067 = CARTESIAN_POINT ( 'NONE',  ( 207.6837091943624785, 270.9282591014416539, -1.156610046911421552 ) ) ;
#8068 = CARTESIAN_POINT ( 'NONE',  ( 204.5133713884061706, 276.4194452585140311, 14.87364779308245843 ) ) ;
#8069 = CARTESIAN_POINT ( 'NONE',  ( 41.54549712337441747, 24.39040679176986615, -6.890680421881970419E-14 ) ) ;
#8070 = CARTESIAN_POINT ( 'NONE',  ( 205.1300674467857164, 275.3512963525735131, -12.60245643603069610 ) ) ;
#8072 = ADVANCED_FACE ( 'NONE', ( #31540 ), #70040, .T. ) ;
#8071 = B_SPLINE_CURVE_WITH_KNOTS ( 'NONE', 3,
 ( #51600, #28289, #35894, #96748 ),
 .UNSPECIFIED., .F., .F.,
 ( 4, 4 ),
 ( 0.009085677135906682078, 0.01422205901525189567 ),
 .UNSPECIFIED. ) ;
#8073 = CARTESIAN_POINT ( 'NONE',  ( 138.9560545341254851, 251.0333772461660260, 9.188101187500095079 ) ) ;
#8074 = VECTOR ( 'NONE', #65142, 1000.000000000000114 ) ;
#8075 = CARTESIAN_POINT ( 'NONE',  ( 166.5418805794664934, 264.7512503615053561, 17.71810435351582669 ) ) ;
#8076 = CARTESIAN_POINT ( 'NONE',  ( 181.3477783452750316, 260.0325310163331096, 9.501399873363059356 ) ) ;
#8077 = CARTESIAN_POINT ( 'NONE',  ( 81.12205585946965414, 208.4548013555409796, -4.594050593750042211 ) ) ;
#8078 = VERTEX_POINT ( 'NONE', #1162 ) ;
#8079 = CARTESIAN_POINT ( 'NONE',  ( 191.5451565139252068, 298.8810523045859213, 7.782291334092181323 ) ) ;
#8080 = CARTESIAN_POINT ( 'NONE',  ( 79.61837626304058801, 45.86816547348837503, 12.91835716780937737 ) ) ;
#8081 = ORIENTED_EDGE ( 'NONE', *, *, #91677, .F. ) ;
#8082 = DIRECTION ( 'NONE',  ( -0.9054088711727241723, 0.4245406647209821194, 0.000000000000000000 ) ) ;
#8083 = ORIENTED_EDGE ( 'NONE', *, *, #9633, .F. ) ;
#8084 = CARTESIAN_POINT ( 'NONE',  ( 66.44361335696784465, 67.86098865684965631, 6.695726806363200723 ) ) ;
#8085 = CARTESIAN_POINT ( 'NONE',  ( 197.9292284917571862, 286.8924113709215362, 16.93415600513534969 ) ) ;
#8086 = CARTESIAN_POINT ( 'NONE',  ( 147.2999496562918296, 275.5159985734018164, -0.1418322875769767455 ) ) ;
#8087 = DIRECTION ( 'NONE',  ( 0.6835488936653759673, 0.7299047266382376886, 0.000000000000000000 ) ) ;
#8088 = CARTESIAN_POINT ( 'NONE',  ( 70.95953762786423624, 65.45173126332643676, 11.97092896923417094 ) ) ;
#8089 = CARTESIAN_POINT ( 'NONE',  ( 86.64296780859545777, 211.6423013555409796, -4.594050593750043987 ) ) ;
#8090 = ORIENTED_EDGE ( 'NONE', *, *, #96617, .T. ) ;
#8091 = AXIS2_PLACEMENT_3D ( 'NONE', #68663, #36276, #99586 ) ;
#8092 = VERTEX_POINT ( 'NONE', #85823 ) ;
#8093 = B_SPLINE_SURFACE_WITH_KNOTS ( 'NONE', 3, 1, ( 
 ( #57261, #18787 ),
 ( #42068, #78593 ),
 ( #73001, #9178 ),
 ( #31959, #24378 ),
 ( #19305, #96312 ),
 ( #50172, #13186 ),
 ( #44042, #12179 ),
 ( #81124, #35957 ),
 ( #82624, #35464 ),
 ( #27868, #58261 ),
 ( #83100, #5563 ),
 ( #81609, #43559 ),
 ( #36452, #43040 ),
 ( #74982, #52151 ),
 ( #50657, #11692 ),
 ( #51155, #34471 ),
 ( #44543, #20281 ),
 ( #20784, #59748 ),
 ( #67356, #42551 ),
 ( #73484, #21274 ),
 ( #98284, #13670 ),
 ( #4568, #4068 ),
 ( #73984, #34958 ),
 ( #28872, #90719 ),
 ( #26880, #82119 ),
 ( #28358, #51675 ),
 ( #65858, #58747 ),
 ( #89720, #66369 ),
 ( #97300, #12692 ),
 ( #74498, #5076 ),
 ( #66859, #27375 ) ),
 .UNSPECIFIED., .F., .F., .F.,
 ( 4, 3, 3, 3, 3, 3, 3, 3, 3, 3, 4 ),
 ( 2, 2 ),
 ( 0.000000000000000000, 0.1122669598086897952, 0.2243161639709869148, 0.3396355846219287211, 0.4553962076585368890, 0.5677860799922546109, 0.6749047109689865209, 0.7773884377078494889, 0.8775581155834415448, 0.9782364162377932271, 1.000000000000000000 ),
 ( 0.000000000000000000, 1.000000000000000000 ),
 .UNSPECIFIED. ) ;
#8094 = CARTESIAN_POINT ( 'NONE',  ( 200.3809179181201614, 283.5770646289640240, -17.08954332461089365 ) ) ;
#8095 = ORIENTED_EDGE ( 'NONE', *, *, #39768, .T. ) ;
#8096 = CARTESIAN_POINT ( 'NONE',  ( 76.29399651998687659, 51.64836840559479469, -16.17400485107173225 ) ) ;
#8097 = CARTESIAN_POINT ( 'NONE',  ( 184.1785766904203001, 275.2410092694960895, 16.37069233236986676 ) ) ;
#8098 = CARTESIAN_POINT ( 'NONE',  ( 164.6869624841032191, 245.4008089637804346, 1.435659848726088317 ) ) ;
#8099 = CIRCLE ( 'NONE', #90656, 0.1418229129681557177 ) ;
#8100 = CARTESIAN_POINT ( 'NONE',  ( 162.5148320529283126, 285.2034568178174254, 0.5437328601018158736 ) ) ;
#8101 = DIRECTION ( 'NONE',  ( -0.000000000000000000, -0.000000000000000000, -1.000000000000000000 ) ) ;
#8102 = FACE_OUTER_BOUND ( 'NONE', #11429, .T. ) ;
#8103 = ORIENTED_EDGE ( 'NONE', *, *, #42003, .T. ) ;
#8104 = CARTESIAN_POINT ( 'NONE',  ( 82.97179646587753155, 43.66170675654236533, -8.010128394304160793 ) ) ;
#8105 = CARTESIAN_POINT ( 'NONE',  ( 186.0258092806693355, 259.0446144625114471, 6.352418251517233827 ) ) ;
#8106 = CARTESIAN_POINT ( 'NONE',  ( 30.74868702942336895, 36.49103043416551628, -8.090169943749479842 ) ) ;
#8107 = CARTESIAN_POINT ( 'NONE',  ( 152.8721808860877616, 265.8646109718731623, -17.65676496037632504 ) ) ;
#8108 = CARTESIAN_POINT ( 'NONE',  ( 72.42968441479126795, 70.75204143367579945, 7.711333220305030878 ) ) ;
#8109 = B_SPLINE_CURVE_WITH_KNOTS ( 'NONE', 3,
 ( #7774, #83316, #31060, #38147, #53849, #46770, #84319, #61950, #52867, #90933, #69065, #8278, #39145, #99993, #45752, #98505, #83818, #29095, #59961, #15349, #21483, #52373, #13878, #45269, #44760, #6279, #76202, #23963, #56361, #85844, #70565 ),
 .UNSPECIFIED., .F., .F.,
 ( 4, 3, 3, 3, 3, 3, 3, 3, 3, 3, 4 ),
 ( 0.000000000000000000, 0.1333490885032350692, 0.3007194338854288218, 0.4699862290245104268, 0.5844252810809298371, 0.6686540514502736787, 0.7354980260655487045, 0.8028463152565475935, 0.8633854507757110497, 0.9437142632667278042, 1.000000000000000000 ),
 .UNSPECIFIED. ) ;
#8110 = CARTESIAN_POINT ( 'NONE',  ( 72.53392552391629522, 67.03926855329653733, -11.49449286787162983 ) ) ;
#8111 = ORIENTED_EDGE ( 'NONE', *, *, #81856, .F. ) ;
#8112 = CARTESIAN_POINT ( 'NONE',  ( 195.7809538458540999, 265.2618777367464418, 5.140530321345854858 ) ) ;
#8113 = CYLINDRICAL_SURFACE ( 'NONE', #74186, 17.82106496071139645 ) ;
#8114 = LINE ( 'NONE', #22304, #30135 ) ;
#8115 = CARTESIAN_POINT ( 'NONE',  ( 170.2203850864397339, 251.3096531866638657, 6.994710684270507350 ) ) ;
#8116 = CARTESIAN_POINT ( 'NONE',  ( 83.83362232629562527, 51.98300042451027991, 14.54734556420943292 ) ) ;
#8117 = DIRECTION ( 'NONE',  ( -0.000000000000000000, 0.000000000000000000, -1.000000000000000000 ) ) ;
#8118 = ADVANCED_FACE ( 'NONE', ( #15842 ), #22943, .F. ) ;
#8119 = VERTEX_POINT ( 'NONE', #9775 ) ;
#8120 = CARTESIAN_POINT ( 'NONE',  ( 182.6549766561670651, 262.8541459689510020, 13.52474329316464896 ) ) ;
#8121 = CARTESIAN_POINT ( 'NONE',  ( -17.43116445825134164, 103.7197590629589712, 44.61401193002000554 ) ) ;
#8122 = CARTESIAN_POINT ( 'NONE',  ( 205.2121761402296443, 275.2090799237855094, -14.05269615702442465 ) ) ;
#8124 = CARTESIAN_POINT ( 'NONE',  ( 74.16423100742596830, 55.12596566212364735, 16.60428178130680266 ) ) ;
#8123 = FACE_OUTER_BOUND ( 'NONE', #33475, .T. ) ;
#8125 = CARTESIAN_POINT ( 'NONE',  ( 59.71366722694061480, 216.8297689869269220, -2.679491924311252493 ) ) ;
#8126 = CARTESIAN_POINT ( 'NONE',  ( 23.18815102787819526, 35.16126292948896293, -6.180339887498951690 ) ) ;
#8127 = CARTESIAN_POINT ( 'NONE',  ( 162.6991225460172927, 284.8212170328912975, -3.897741803361528756 ) ) ;
#8128 = CARTESIAN_POINT ( 'NONE',  ( 67.44257088943837175, 67.25355904234817217, -8.657396272410815996 ) ) ;
#8129 = CARTESIAN_POINT ( 'NONE',  ( 191.3281377348044714, 262.2149640667300332, 2.921411013909792853 ) ) ;
#8130 = CARTESIAN_POINT ( 'NONE',  ( -17.68663747114990770, 172.8464784336661353, 1.353441290958777327E-15 ) ) ;
#8131 = FACE_OUTER_BOUND ( 'NONE', #15741, .T. ) ;
#8132 = ORIENTED_EDGE ( 'NONE', *, *, #33889, .T. ) ;
#8133 = AXIS2_PLACEMENT_3D ( 'NONE', #89744, #20308, #27893 ) ;
#8134 = CARTESIAN_POINT ( 'NONE',  ( 175.0396866787711474, 255.0033583533873980, 9.305020555032612606 ) ) ;
#8135 = CARTESIAN_POINT ( 'NONE',  ( 72.82118101371948171, 71.12637341421535098, -7.461520388884598454 ) ) ;
#8136 = CARTESIAN_POINT ( 'NONE',  ( 160.5893190321802138, 270.9897182155185078, 16.60663562724527864 ) ) ;
#8137 = CARTESIAN_POINT ( 'NONE',  ( 23.01690360248371903, 184.0958772461660544, -9.188101187500095079 ) ) ;
#8138 = CARTESIAN_POINT ( 'NONE',  ( 23.49395736812309465, 37.65659080271452552, -1.878358725466461243E-16 ) ) ;
#8139 = CARTESIAN_POINT ( 'NONE',  ( 84.64602481627416353, 42.28124168067370192, -1.971784886792609326 ) ) ;
#8140 = CARTESIAN_POINT ( 'NONE',  ( 172.1705709408975054, 271.8423139197483920, -16.44096766034999035 ) ) ;
#8141 = CARTESIAN_POINT ( 'NONE',  ( 72.42633913402016788, 63.30405477351032317, 14.41398973578453102 ) ) ;
#8142 = CARTESIAN_POINT ( 'NONE',  ( 84.32653914613003110, 47.10518720127514314, 11.76817659212875178 ) ) ;
#8143 = CARTESIAN_POINT ( 'NONE',  ( 187.7916437398309313, 259.1520801313256470, -0.7955774063839984311 ) ) ;
#8144 = AXIS2_PLACEMENT_3D ( 'NONE', #3520, #96240, #26800 ) ;
#8145 = CARTESIAN_POINT ( 'NONE',  ( 78.97477422587097351, 209.7365022471902023, 10.00000000000009592 ) ) ;
#8146 = CARTESIAN_POINT ( 'NONE',  ( 164.4888076835817401, 246.1997653861143647, 1.812879387509452656 ) ) ;
#8147 = CARTESIAN_POINT ( 'NONE',  ( 206.7596416265183734, 271.4678399409689291, 6.202658291405857227 ) ) ;
#8148 = CARTESIAN_POINT ( 'NONE',  ( 25.61497981383703149, 185.5958772461660544, -9.188101187500095079 ) ) ;
#8149 = CARTESIAN_POINT ( 'NONE',  ( 120.4921787521148246, 228.8262482093457777, 3.021315404115420679E-15 ) ) ;
#8150 = PRESENTATION_STYLE_ASSIGNMENT (( #15226 ) ) ;
#8151 = FACE_OUTER_BOUND ( 'NONE', #20425, .T. ) ;
#8152 = CARTESIAN_POINT ( 'NONE',  ( 151.1699610800269511, 268.8129421616204695, -14.28929860221299286 ) ) ;
#8153 = DIRECTION ( 'NONE',  ( -0.000000000000000000, 0.000000000000000000, 1.000000000000000000 ) ) ;
#8154 = CARTESIAN_POINT ( 'NONE',  ( 48.29091023345864642, 82.53782597618220507, -10.00000000000000000 ) ) ;
#8155 = CARTESIAN_POINT ( 'NONE',  ( 163.1227589771032456, 280.8252380815225138, -10.04696615151233630 ) ) ;
#8156 = CARTESIAN_POINT ( 'NONE',  ( 163.7939847032603780, 282.2082574975837019, 10.05568170618017554 ) ) ;
#8157 = ITEM_DEFINED_TRANSFORMATION ( 'NONE', 'NONE', #57505,  #68784 ) ;
#8158 = CARTESIAN_POINT ( 'NONE',  ( 23.79748941506785442, 22.24335787977763346, -9.188101187500008038 ) ) ;
#8159 = CARTESIAN_POINT ( 'NONE',  ( 148.3190727836317535, 273.7508255376806119, 8.080277324579027365 ) ) ;
#8160 = CARTESIAN_POINT ( 'NONE',  ( 71.40067601551650966, 59.33978977576644098, 15.22537452595757657 ) ) ;
#8161 = EDGE_CURVE ( 'NONE', #87772, #65984, #36864, .T. ) ;
#8162 = CARTESIAN_POINT ( 'NONE',  ( 189.0689802957956260, 269.8288687927027354, -15.50864081522695415 ) ) ;
#8163 = ORIENTED_EDGE ( 'NONE', *, *, #98832, .F. ) ;
#8164 = CARTESIAN_POINT ( 'NONE',  ( 185.3610915123994118, 291.1297846198819457, 13.42384461072851387 ) ) ;
#8165 = CARTESIAN_POINT ( 'NONE',  ( 8.350964356584899662, 25.79752408145590792, -5.678558825948271327 ) ) ;
#8166 = CARTESIAN_POINT ( 'NONE',  ( 75.50015568109331809, 59.09779916697999624, -15.89073866529240675 ) ) ;
#8167 = CARTESIAN_POINT ( 'NONE',  ( 81.57924373063931966, 42.55821344299342002, 7.494866049281546871 ) ) ;
#8168 = ORIENTED_EDGE ( 'NONE', *, *, #19129, .T. ) ;
#8170 = LINE ( 'NONE', #55732, #8553 ) ;
#8169 =( BOUNDED_CURVE ( )  B_SPLINE_CURVE ( 2, ( #17916, #95464, #2722, #42187, #81243, #96946, #73123, #79251, #34115, #11817, #26016, #3714, #2218 ),
 .UNSPECIFIED., .F., .T. ) 
 B_SPLINE_CURVE_WITH_KNOTS ( ( 3, 2, 2, 2, 2, 2, 3 ),
 ( 0.7625000000000000666, 0.7650000000000000133, 0.7700000000000000178, 0.7750000000000000222, 0.7800000000000000266, 0.7850000000000000311, 0.7875000000000000888 ),
 .UNSPECIFIED. ) 
 CURVE ( )  GEOMETRIC_REPRESENTATION_ITEM ( )  RATIONAL_B_SPLINE_CURVE ( ( 0.9755282581475767101, 0.9755282581475772652, 1.000000000000000000, 0.9510565162951535312, 1.000000000000000000, 0.9510565162951535312, 1.000000000000000000, 0.9510565162951535312, 1.000000000000000000, 0.9510565162951535312, 1.000000000000000000, 0.9755282581475761550, 0.9755282581475767101 ) ) 
 REPRESENTATION_ITEM ( '' )  );
#8171 = CARTESIAN_POINT ( 'NONE',  ( 72.38671951208186783, 71.75852817245944948, -5.691748070601700960 ) ) ;
#8172 = CARTESIAN_POINT ( 'NONE',  ( 20.86070775165960001, 33.81751292744056769, -6.180339887498951690 ) ) ;
#8173 = CARTESIAN_POINT ( 'NONE',  ( 85.11007338816820322, 42.50720964942713209, 4.151688445370292690 ) ) ;
#8174 = EDGE_CURVE ( 'NONE', #80145, #57629, #84792, .T. ) ;
#8175 = ORIENTED_EDGE ( 'NONE', *, *, #14170, .T. ) ;
#8176 = VERTEX_POINT ( 'NONE', #92884 ) ;
#8178 = CARTESIAN_POINT ( 'NONE',  ( 87.29749550895752463, 43.60436139353286222, -0.5288150457691258577 ) ) ;
#8177 = CARTESIAN_POINT ( 'NONE',  ( 189.5516473586634731, 274.6233775832965875, -15.96870692800988678 ) ) ;
#8179 = ORIENTED_EDGE ( 'NONE', *, *, #1363, .F. ) ;
#8180 = CARTESIAN_POINT ( 'NONE',  ( 201.1060504099706350, 282.3210983108598384, -18.18000168485860257 ) ) ;
#8181 = LINE ( 'NONE', #52276, #91771 ) ;
#8182 = CARTESIAN_POINT ( 'NONE',  ( 79.84564975497875139, 57.94052304378403306, 16.26602973072665392 ) ) ;
#8183 = CARTESIAN_POINT ( 'NONE',  ( 76.67779265155198232, 63.58935824677200088, 15.33226443842420927 ) ) ;
#8184 = EDGE_CURVE ( 'NONE', #57534, #13459, #9261, .T. ) ;
#8185 = CARTESIAN_POINT ( 'NONE',  ( 148.3837145175834280, 273.6388627701866767, 8.841971351370922605 ) ) ;
#8186 = PLANE ( 'NONE',  #31771 ) ;
#8187 = VERTEX_POINT ( 'NONE', #55821 ) ;
#8188 = CARTESIAN_POINT ( 'NONE',  ( 157.0935036675524827, 258.5530654392286465, 17.32636058289560665 ) ) ;
#8189 = CARTESIAN_POINT ( 'NONE',  ( 160.9230069893865789, 266.6111081704525532, 16.55276295507343320 ) ) ;
#8190 = EDGE_LOOP ( 'NONE', ( #11816, #3710, #17508, #3501 ) ) ;
#8191 = CARTESIAN_POINT ( 'NONE',  ( 32.45774345291223995, 27.24335787977765833, -9.188101187500008038 ) ) ;
#8192 = CARTESIAN_POINT ( 'NONE',  ( 149.1856130393175306, 272.2499337880290682, 11.44243872309708188 ) ) ;
#8193 = DIRECTION ( 'NONE',  ( 0.3535533905932853882, -0.6123724356958029080, -0.7071067811865343611 ) ) ;
#8194 = ORIENTED_EDGE ( 'NONE', *, *, #47470, .F. ) ;
#8195 = CARTESIAN_POINT ( 'NONE',  ( 64.18017357788670552, 207.8615022471903728, 5.188172501216618598E-14 ) ) ;
#8196 = CARTESIAN_POINT ( 'NONE',  ( 190.7851751463332164, 300.1973786460605425, 8.237717828100052486 ) ) ;
#8197 = CARTESIAN_POINT ( 'NONE',  ( 167.7294354343802354, 268.7536494340877766, 17.80279610524468126 ) ) ;
#8198 = CARTESIAN_POINT ( 'NONE',  ( -17.42236680055705023, 149.2012482093457777, 0.000000000000000000 ) ) ;
#8199 = EDGE_LOOP ( 'NONE', ( #54144, #36257 ) ) ;
#8200 = VERTEX_POINT ( 'NONE', #46751 ) ;
#8201 = LINE ( 'NONE', #92340, #96599 ) ;
#8202 = DIRECTION ( 'NONE',  ( -0.4145187862775162602, 0.7179675985244458047, -0.5591929034707565638 ) ) ;
#8203 = CARTESIAN_POINT ( 'NONE',  ( 180.7942833579522812, 266.7097690628117448, -16.23795806611159520 ) ) ;
#8204 = CARTESIAN_POINT ( 'NONE',  ( 148.3190727836317535, 273.7508255376806119, 8.080277324579027365 ) ) ;
#8205 = EDGE_LOOP ( 'NONE', ( #12958, #2341, #55389, #75767, #70838 ) ) ;
#8206 = CARTESIAN_POINT ( 'NONE',  ( 190.7222376050763444, 300.3063896652212179, 3.365789908110941475 ) ) ;
#8207 = CARTESIAN_POINT ( 'NONE',  ( 171.3649617487770911, 251.0102673366500596, 7.372720983288576946 ) ) ;
#8208 = LINE ( 'NONE', #16300, #93651 ) ;
#8209 = CARTESIAN_POINT ( 'NONE',  ( 193.2100161762185735, 295.9974307820218087, -12.46499585622781758 ) ) ;
#8210 = DIRECTION ( 'NONE',  ( 0.4999999999999998890, -0.8660254037844385966, 0.000000000000000000 ) ) ;
#8211 = CARTESIAN_POINT ( 'NONE',  ( 71.45246435704785881, 70.41140176850349519, 6.448010139539340102 ) ) ;
#8212 = CARTESIAN_POINT ( 'NONE',  ( 28.46864935082050252, 149.7156766241961350, -37.49999999999994316 ) ) ;
#8213 = CARTESIAN_POINT ( 'NONE',  ( 67.50571429351523989, 67.05925936848247204, 8.976381766308007215 ) ) ;
#8214 = CARTESIAN_POINT ( 'NONE',  ( 70.48980766314222990, 65.45931048306678690, -11.73774681883049098 ) ) ;
#8215 = CARTESIAN_POINT ( 'NONE',  ( 78.74835927026373383, 47.64973151805292417, 14.29178299612483194 ) ) ;
#8216 = CARTESIAN_POINT ( 'NONE',  ( 111.8384605302426991, 241.5024278399160664, -9.188101187500093303 ) ) ;
#8217 = ORIENTED_EDGE ( 'NONE', *, *, #57447, .F. ) ;
#8218 = CARTESIAN_POINT ( 'NONE',  ( 147.3047606266276546, 275.5076657283461827, -0.02269072295920609994 ) ) ;
#8219 = EDGE_CURVE ( 'NONE', #43051, #45411, #54327, .T. ) ;
#8220 = CARTESIAN_POINT ( 'NONE',  ( 70.24270501652357268, 65.21164827444138723, 11.83463923091347603 ) ) ;
#8221 = ADVANCED_FACE ( 'NONE', ( #77677 ), #51703, .F. ) ;
#8222 = DIRECTION ( 'NONE',  ( 0.000000000000000000, 0.000000000000000000, 1.000000000000000000 ) ) ;
#8223 = CARTESIAN_POINT ( 'NONE',  ( 155.5322964227545413, 261.2571557083629159, -18.35853982030605280 ) ) ;
#8224 = CARTESIAN_POINT ( 'NONE',  ( 164.2712161151136172, 246.1209027979328710, 7.276091357954241445 ) ) ;
#8225 = CARTESIAN_POINT ( 'NONE',  ( 83.68493280611274088, 51.65299594367198210, -14.83749715326822205 ) ) ;
#8226 = CARTESIAN_POINT ( 'NONE',  ( 169.2964062698280543, 285.1489873681304630, -7.912550111543783515 ) ) ;
#8227 = ORIENTED_EDGE ( 'NONE', *, *, #41239, .F. ) ;
#8228 = CARTESIAN_POINT ( 'NONE',  ( 80.37814466807276403, 57.92114694875621694, -16.24750869670133113 ) ) ;
#8229 = B_SPLINE_CURVE_WITH_KNOTS ( 'NONE', 3,
 ( #8918, #63118, #25111, #47899 ),
 .UNSPECIFIED., .F., .F.,
 ( 4, 4 ),
 ( 0.04273337087810722551, 0.04887066958154943214 ),
 .UNSPECIFIED. ) ;
#8230 = CARTESIAN_POINT ( 'NONE',  ( 72.13809228306983812, 71.45234993612235996, 5.060403501811140181 ) ) ;
#8231 = CARTESIAN_POINT ( 'NONE',  ( 74.63339219689319748, 67.07035889417386443, 12.49364407091348106 ) ) ;
#8232 = ADVANCED_FACE ( 'NONE', ( #65944 ), #96897, .T. ) ;
#8233 = CARTESIAN_POINT ( 'NONE',  ( 128.5905526607566856, 254.2369531367911293, -4.594050593750048428 ) ) ;
#8234 = CARTESIAN_POINT ( 'NONE',  ( 198.5511052797322975, 286.7463930869835167, -17.24711022262289006 ) ) ;
#8235 = ADVANCED_FACE ( 'NONE', ( #89313 ), #76069, .T. ) ;
#8236 = CYLINDRICAL_SURFACE ( 'NONE', #62725, 17.82106496071139645 ) ;
#8237 = CARTESIAN_POINT ( 'NONE',  ( 157.4656258344471098, 257.9085309395441641, 18.30485740784190796 ) ) ;
#8238 = CARTESIAN_POINT ( 'NONE',  ( 167.5421813246326792, 287.5986610761024167, 3.969292590682533373 ) ) ;
#8239 = CARTESIAN_POINT ( 'NONE',  ( 55.76366273096530080, 196.8768266524160140, 9.188101187500098632 ) ) ;
#8240 = CARTESIAN_POINT ( 'NONE',  ( 85.72774873836118559, 48.77901937666835153, -12.00006183775103352 ) ) ;
#8241 = VERTEX_POINT ( 'NONE', #74831 ) ;
#8243 = ADVANCED_FACE ( 'NONE', ( #97632 ), #22620, .F. ) ;
#8242 = CARTESIAN_POINT ( 'NONE',  ( 71.09705276464538315, 63.61861273659285843, 13.28640888171760714 ) ) ;
#8244 = CARTESIAN_POINT ( 'NONE',  ( 191.4420812244453600, 260.8157448279923187, -1.331758356259544085 ) ) ;
#8245 = EDGE_CURVE ( 'NONE', #68766, #73260, #52003, .T. ) ;
#8246 = B_SPLINE_CURVE_WITH_KNOTS ( 'NONE', 3,
 ( #50888, #90448, #66098, #12413, #28091, #50392, #66596, #4290, #82840, #73708, #97046, #27112, #89933, #27614, #19532, #74225, #35190, #29106, #90943, #21494, #20511, #59465, #58480, #81344, #44280, #13409, #89453, #52384, #4814, #74724, #12920, #35696, #44770, #51386, #5301, #36180, #67082, #98006, #28586, #82353, #20009, #88977, #21017, #81836, #5787, #83326 ),
 .UNSPECIFIED., .F., .F.,
 ( 4, 1, 1, 1, 2, 2, 1, 1, 1, 2, 2, 1, 1, 2, 2, 1, 1, 2, 2, 1, 1, 2, 2, 1, 2, 2, 1, 2, 2, 4 ),
 ( 0.000000000000000000, 0.06250000000000249800, 0.09375000000000141553, 0.1093750000000008743, 0.1171874999999998473, 0.1249999999999988343, 0.1874999999999915345, 0.2187499999999893141, 0.2343749999999881761, 0.2421874999999883982, 0.2499999999999885925, 0.3124999999999791278, 0.3437499999999751310, 0.3593749999999745759, 0.3749999999999739653, 0.4374999999999647504, 0.4687499999999613087, 0.4843749999999601985, 0.4999999999999590328, 0.5624999999999589217, 0.5937499999999593658, 0.6093749999999600320, 0.6249999999999608091, 0.6874999999999679146, 0.7187499999999724665, 0.7499999999999769074, 0.8124999999999835687, 0.8437499999999857891, 0.8749999999999878986, 1.000000000000000000 ),
 .UNSPECIFIED. ) ;
#8247 = CARTESIAN_POINT ( 'NONE',  ( 15.77842244150312645, 191.4637435831425307, 2.679491924311251605 ) ) ;
#8248 = CARTESIAN_POINT ( 'NONE',  ( 190.4240181651484818, 300.8229208869809668, -4.214281362166949485 ) ) ;
#8249 = CARTESIAN_POINT ( 'NONE',  ( 82.09965751949748380, 41.85612385560651205, -5.535113643993918586 ) ) ;
#8250 = CARTESIAN_POINT ( 'NONE',  ( 202.9547455376043672, 279.1190644220934018, -15.19669173352461478 ) ) ;
#8251 = CARTESIAN_POINT ( 'NONE',  ( 181.5435273739199715, 262.6800588168453032, 12.44797431397677379 ) ) ;
#8252 = CARTESIAN_POINT ( 'NONE',  ( 117.3505249275209792, 231.8927522451417929, -10.00000000000009059 ) ) ;
#8253 = CARTESIAN_POINT ( 'NONE',  ( 194.5617139857802442, 293.2599130566108556, -14.58798304743176821 ) ) ;
#8254 = ORIENTED_EDGE ( 'NONE', *, *, #65508, .T. ) ;
#8255 = B_SPLINE_CURVE_WITH_KNOTS ( 'NONE', 3,
 ( #96730, #12603, #58178, #89636 ),
 .UNSPECIFIED., .F., .F.,
 ( 4, 4 ),
 ( 0.000000000000000000, 0.002752262309457068155 ),
 .UNSPECIFIED. ) ;
#8256 = CARTESIAN_POINT ( 'NONE',  ( 189.8147415777049218, 301.8782188922952514, -0.5019643756309712934 ) ) ;
#8257 = CARTESIAN_POINT ( 'NONE',  ( 13.61667370911268193, 23.56454794089040661, 10.00000000000000355 ) ) ;
#8258 = CARTESIAN_POINT ( 'NONE',  ( 23.88258191050314494, 196.8464784336661637, 1.353441290958777327E-15 ) ) ;
#8259 = CARTESIAN_POINT ( 'NONE',  ( 14.97590445773717782, 13.81029122506293305, 8.090169943749479842 ) ) ;
#8260 = CARTESIAN_POINT ( 'NONE',  ( 80.17333107395900527, 49.88587112779518407, -14.95505157533469820 ) ) ;
#8261 = CARTESIAN_POINT ( 'NONE',  ( 72.02251067321300582, 59.31025418870372334, -15.33526842769922460 ) ) ;
#8262 = B_SPLINE_CURVE_WITH_KNOTS ( 'NONE', 3,
 ( #63642, #33241, #78362, #95093, #78865, #10452, #87527, #47926, #17034, #24638, #9451, #41325, #1354, #18058, #16538, #88012, #33766, #63139, #1855, #41835, #47434, #25658, #62623, #40323, #39810, #56537, #10963, #80393, #56016, #70742, #87012, #17541, #64654, #48954, #32239, #48448, #32737, #24145, #95604, #94084, #72269, #93578, #9959, #86506, #40818, #2363, #55030, #86012, #3851, #82398, #66635, #97087, #27656, #96591 ),
 .UNSPECIFIED., .F., .F.,
 ( 4, 2, 2, 2, 2, 2, 2, 2, 2, 2, 2, 2, 2, 2, 2, 2, 2, 2, 2, 2, 2, 2, 2, 2, 2, 2, 4 ),
 ( 0.0006996174624294505600, 0.0009087055706953546834, 0.001117793678961258915, 0.001222337733094224855, 0.001326881787227190794, 0.001431425841360156950, 0.001535969895493122890, 0.001745058003759054552, 0.001954146112024986864, 0.002372322328556768223, 0.003208674761620287138, 0.004045027194683806053, 0.004881379627747325402, 0.005299555844279047780, 0.005508643952544909836, 0.005613188006677764103, 0.005665460033744189501, 0.005717732060810614900, 0.005770004087877040298, 0.005822276114943466564, 0.005926820169076324300, 0.006135908277342071865, 0.006554084493873547045, 0.006763172602139241700, 0.006972260710404936355, 0.007181348818670631011, 0.007390436926936325666 ),
 .UNSPECIFIED. ) ;
#8263 = PLANE ( 'NONE',  #42604 ) ;
#8265 = CARTESIAN_POINT ( 'NONE',  ( 62.31280629920263436, 206.7833772461660828, -9.188101187500095079 ) ) ;
#8264 = CARTESIAN_POINT ( 'NONE',  ( 177.4980249182310104, 288.1765118805776069, 10.70887779921548422 ) ) ;
#8266 = CARTESIAN_POINT ( 'NONE',  ( 200.1385401540174769, 283.9968752310148830, 17.30012534137638625 ) ) ;
#8267 = CARTESIAN_POINT ( 'NONE',  ( 72.79574698827143209, 57.15038201193220857, 15.89495189336207304 ) ) ;
#8268 = CARTESIAN_POINT ( 'NONE',  ( 71.90991478695079309, 70.64910724575318568, 7.404170080562185063 ) ) ;
#8269 = CARTESIAN_POINT ( 'NONE',  ( 66.33153531111928203, 68.76406954428721008, -4.318981651738461380 ) ) ;
#8270 = ORIENTED_EDGE ( 'NONE', *, *, #32550, .F. ) ;
#8271 = CARTESIAN_POINT ( 'NONE',  ( 30.33301404664494427, 194.9865022471903160, -10.00000000000009415 ) ) ;
#8272 = CARTESIAN_POINT ( 'NONE',  ( -13.11024591527734628, 6.000000000000000000, 32.50000000000000000 ) ) ;
#8273 = CARTESIAN_POINT ( 'NONE',  ( -16.90171517502901466, 170.2369531367911293, -4.594050593750048428 ) ) ;
#8274 = CARTESIAN_POINT ( 'NONE',  ( 25.90481151690805106, 33.14336893147756768, 7.433330006724141015 ) ) ;
#8275 = CARTESIAN_POINT ( 'NONE',  ( 167.3985425305344563, 262.3805089322066237, -16.46154190842169740 ) ) ;
#8276 = CARTESIAN_POINT ( 'NONE',  ( 186.6027929891679662, 261.0133341855545268, 6.348929212563308333 ) ) ;
#8277 = CARTESIAN_POINT ( 'NONE',  ( 205.8452707775803390, 274.1125278458945900, 11.42742867493066328 ) ) ;
#8278 = CARTESIAN_POINT ( 'NONE',  ( 88.38522318935277156, 43.99954571450756902, 2.365518284841161556 ) ) ;
#8279 = CARTESIAN_POINT ( 'NONE',  ( 66.06920883062277028, 68.60566076105189381, 1.839620377662104955 ) ) ;
#8280 = ORIENTED_EDGE ( 'NONE', *, *, #31399, .T. ) ;
#8281 = CARTESIAN_POINT ( 'NONE',  ( -22.42236680055709641, 157.8615022471902591, 0.000000000000000000 ) ) ;
#8282 =( NAMED_UNIT ( * ) PLANE_ANGLE_UNIT ( ) SI_UNIT ( $, .RADIAN. ) );
#8283 = LINE ( 'NONE', #15868, #38586 ) ;
#8284 = CARTESIAN_POINT ( 'NONE',  ( 14.05589992062122917, 20.06628583063840310, -9.188101187500006262 ) ) ;
#8285 = VERTEX_POINT ( 'NONE', #99116 ) ;
#8286 = CARTESIAN_POINT ( 'NONE',  ( 159.8869478387880747, 253.7146782065408672, 15.67510143967828995 ) ) ;
#8287 = EDGE_CURVE ( 'NONE', #15150, #11106, #69133, .T. ) ;
#8288 = CARTESIAN_POINT ( 'NONE',  ( 88.30263053946062257, 44.32431199883396289, -2.152525388235255743 ) ) ;
#8289 = CARTESIAN_POINT ( 'NONE',  ( 71.53080809438634446, 72.38941617099003167, 1.021674839914435085 ) ) ;
#8290 = EDGE_CURVE ( 'NONE', #47161, #11048, #87902, .T. ) ;
#8291 = CARTESIAN_POINT ( 'NONE',  ( 153.3100492430090753, 265.1062007306585997, 16.32434963471121492 ) ) ;
#8292 = CARTESIAN_POINT ( 'NONE',  ( 207.6628070930962906, 270.9644626028195376, 7.378217122120054761 ) ) ;
#8293 = CARTESIAN_POINT ( 'NONE',  ( 149.6775655717086124, 272.1443760297916583, 11.34356142435849968 ) ) ;
#8294 = CARTESIAN_POINT ( 'NONE',  ( 162.6757594134126350, 248.8843148665554281, -10.86406770146305867 ) ) ;
#8295 = AXIS2_PLACEMENT_3D ( 'NONE', #55879, #71634, #90347 ) ;
#8296 = CARTESIAN_POINT ( 'NONE',  ( 200.7484899876179441, 282.9404111291507888, -16.88964748465601673 ) ) ;
#8297 = ORIENTED_EDGE ( 'NONE', *, *, #78443, .T. ) ;
#8298 = EDGE_LOOP ( 'NONE', ( #27743, #92476, #47293, #4169 ) ) ;
#8299 = DIRECTION ( 'NONE',  ( -0.7059494278973847958, 0.7082622432767082810, 0.000000000000000000 ) ) ;
#8300 = DIRECTION ( 'NONE',  ( -1.000000000000000000, 0.000000000000000000, 0.000000000000000000 ) ) ;
#8301 = ORIENTED_EDGE ( 'NONE', *, *, #52583, .F. ) ;
#8302 = LINE ( 'NONE', #85340, #7862 ) ;
#8303 = CARTESIAN_POINT ( 'NONE',  ( 74.14312167556930433, 66.30466486950707861, 1.224646799147354045E-15 ) ) ;
#8305 = ADVANCED_FACE ( 'NONE', ( #29698 ), #82946, .T. ) ;
#8304 = VERTEX_POINT ( 'NONE', #77298 ) ;
#8306 = CARTESIAN_POINT ( 'NONE',  ( -19.65312891409030271, 93.06504152958497400, -10.00000000000000888 ) ) ;
#8307 = CARTESIAN_POINT ( 'NONE',  ( 180.2836023094594395, 259.4510097613480752, -11.78144428920749753 ) ) ;
#8308 = CARTESIAN_POINT ( 'NONE',  ( 149.2923684163597784, 272.0650280510108701, -12.99082738998495756 ) ) ;
#8309 = CARTESIAN_POINT ( 'NONE',  ( 69.37236052325044966, 62.78824976232480282, 13.73178353374107630 ) ) ;
#8310 = VERTEX_POINT ( 'NONE', #53484 ) ;
#8311 = CARTESIAN_POINT ( 'NONE',  ( 203.6735071151937575, 277.8741328511802635, 15.93813992116388434 ) ) ;
#8312 = CARTESIAN_POINT ( 'NONE',  ( 151.3284628043366524, 268.5384091220288383, 14.49047510809488237 ) ) ;
#8313 = DIRECTION ( 'NONE',  ( -0.7033187449715098127, 0.7108746323872447981, 0.000000000000000000 ) ) ;
#8314 = ORIENTED_EDGE ( 'NONE', *, *, #65131, .T. ) ;
#8315 = EDGE_CURVE ( 'NONE', #82473, #7026, #12805, .T. ) ;
#8316 = ORIENTED_EDGE ( 'NONE', *, *, #94051, .F. ) ;
#8317 = EDGE_CURVE ( 'NONE', #26527, #41212, #18910, .T. ) ;
#8318 = EDGE_LOOP ( 'NONE', ( #92089, #92490, #7204, #44804, #47810, #34508, #32729 ) ) ;
#8319 = CARTESIAN_POINT ( 'NONE',  ( 72.82800908514342098, 58.96091748745875805, 15.56478197890324289 ) ) ;
#8320 = ORIENTED_EDGE ( 'NONE', *, *, #59425, .T. ) ;
#8321 = LINE ( 'NONE', #84359, #65467 ) ;
#8322 = VERTEX_POINT ( 'NONE', #70686 ) ;
#8323 = CARTESIAN_POINT ( 'NONE',  ( 164.3053959849042087, 246.0617015268593661, -7.251939739328854273 ) ) ;
#8324 = CARTESIAN_POINT ( 'NONE',  ( 82.68100460170427368, 47.33644815824931840, 12.13400673372383665 ) ) ;
#8325 = CARTESIAN_POINT ( 'NONE',  ( 167.8360140743272666, 281.0956243233280816, 11.63507309386356248 ) ) ;
#8326 = CARTESIAN_POINT ( 'NONE',  ( 147.7112127936102866, 274.8036699242858276, -9.124700685424272706 ) ) ;
#8327 = CARTESIAN_POINT ( 'NONE',  ( 82.73351218272506458, 53.30090480274827769, -15.28980472815078784 ) ) ;
#8328 = CARTESIAN_POINT ( 'NONE',  ( 158.9097751959179448, 255.4071908717584449, -17.55082260428511631 ) ) ;
#8329 = CARTESIAN_POINT ( 'NONE',  ( 76.31890144197360826, 56.60031049123248437, -16.61185794330136289 ) ) ;
#8330 = CARTESIAN_POINT ( 'NONE',  ( 13.34565549823491004, 29.74646525600389424, 2.839279412974139660 ) ) ;
#8331 = CARTESIAN_POINT ( 'NONE',  ( 163.8187377589169955, 282.1776765746977844, 8.479121753608614753 ) ) ;
#8332 = DIRECTION ( 'NONE',  ( -0.8660254037844387076, -0.4999999999999998890, -0.000000000000000000 ) ) ;
#8334 = VERTEX_POINT ( 'NONE', #85962 ) ;
#8333 = CARTESIAN_POINT ( 'NONE',  ( 159.5764336135613632, 254.2525046211064819, 15.32981087583629076 ) ) ;
#8335 = CARTESIAN_POINT ( 'NONE',  ( 190.4882032423914211, 300.7117490721083755, 5.365042449410100112 ) ) ;
#8336 = EDGE_CURVE ( 'NONE', #82018, #90758, #77814, .T. ) ;
#8337 = FACE_OUTER_BOUND ( 'NONE', #45670, .T. ) ;
#8338 = CARTESIAN_POINT ( 'NONE',  ( 159.9788992190088948, 253.5554137441726255, -15.81862932303382330 ) ) ;
#8339 = LINE ( 'NONE', #26051, #52156 ) ;
#8340 = CARTESIAN_POINT ( 'NONE',  ( 84.59171082261967456, 45.66142255087724777, -9.512095294586423222 ) ) ;
#8341 = CARTESIAN_POINT ( 'NONE',  ( -33.75225536883275623, 24.49963747467413100, 177.5919119679930134 ) ) ;
#8342 = CARTESIAN_POINT ( 'NONE',  ( 72.04273812837080015, 59.28583566120335746, 15.84548535902080246 ) ) ;
#8343 = EDGE_LOOP ( 'NONE', ( #85101, #79486, #80841, #57397 ) ) ;
#8345 = EDGE_CURVE ( 'NONE', #66029, #36928, #44159, .T. ) ;
#8344 = CARTESIAN_POINT ( 'NONE',  ( 194.0719046999502666, 294.5045960684578858, -14.15255333265519333 ) ) ;
#8346 = CARTESIAN_POINT ( 'NONE',  ( 75.02238714290076871, 66.92454316053132857, -13.18498694845918706 ) ) ;
#8347 = DIRECTION ( 'NONE',  ( 0.2776767122488391082, 0.9606745773021556634, 0.000000000000000000 ) ) ;
#8348 = CARTESIAN_POINT ( 'NONE',  ( 7.365298646897277202, 168.3927522451418213, 10.00000000000009592 ) ) ;
#8349 = CARTESIAN_POINT ( 'NONE',  ( 84.34250105585179824, 213.3768266524160140, 9.188101187500096856 ) ) ;
#8350 = CARTESIAN_POINT ( 'NONE',  ( 82.11234663424232849, 40.76891643967551460, -1.025997306391484232 ) ) ;
#8351 = ADVANCED_FACE ( 'NONE', ( #78808 ), #84139, .F. ) ;
#8352 = CARTESIAN_POINT ( 'NONE',  ( 7.184267760421183091, 27.08080186712590631, -3.090169943749475845 ) ) ;
#8353 = CARTESIAN_POINT ( 'NONE',  ( 167.0511520614714129, 278.3166273224070437, -13.37090358088792286 ) ) ;
#8354 = CARTESIAN_POINT ( 'NONE',  ( 170.8054577101068219, 287.4915981561377976, 8.526299399445241178 ) ) ;
#8356 = CARTESIAN_POINT ( 'NONE',  ( 75.71688963635942571, 65.45405155058689672, 14.28099675560567583 ) ) ;
#8355 = CARTESIAN_POINT ( 'NONE',  ( 9.864316330390064280, 170.3768266524160140, -9.188101187500091527 ) ) ;
#8357 = EDGE_CURVE ( 'NONE', #75006, #66118, #88458, .T. ) ;
#8358 = CARTESIAN_POINT ( 'NONE',  ( 200.1444820856229967, 283.9865835035790269, 17.93386694781497326 ) ) ;
#8359 = ORIENTED_EDGE ( 'NONE', *, *, #40222, .F. ) ;
#8360 = EDGE_CURVE ( 'NONE', #92132, #85089, #97511, .T. ) ;
#8361 = ORIENTED_EDGE ( 'NONE', *, *, #38134, .F. ) ;
#8362 = EDGE_CURVE ( 'NONE', #7928, #41027, #47215, .T. ) ;
#8363 = PLANE ( 'NONE',  #70920 ) ;
#8364 = CARTESIAN_POINT ( 'NONE',  ( 198.7984568860927084, 266.5006840448155572, -2.860727480615956608 ) ) ;
#8365 = CARTESIAN_POINT ( 'NONE',  ( 86.62620551031615435, 45.88478951247049764, -8.398712350495802781 ) ) ;
#8366 = CIRCLE ( 'NONE', #6770, 0.1418229129681557177 ) ;
#8367 = CARTESIAN_POINT ( 'NONE',  ( 144.6270795744234476, 268.7413018095040798, -2.761272660171008000E-15 ) ) ;
#8368 = CARTESIAN_POINT ( 'NONE',  ( 113.8346084569740242, 224.9824982072974251, 3.021315404115420679E-15 ) ) ;
#8369 = DIRECTION ( 'NONE',  ( -0.000000000000000000, -1.000000000000000000, -0.000000000000000000 ) ) ;
#8370 = CARTESIAN_POINT ( 'NONE',  ( 30.97368554763575688, 182.5643266524159856, -9.188101187500093303 ) ) ;
#8371 = CARTESIAN_POINT ( 'NONE',  ( 128.5097966488581562, 238.8768266524159856, 9.188101187500098632 ) ) ;
#8372 = CARTESIAN_POINT ( 'NONE',  ( 196.9839693152069344, 276.0740101548715302, 15.26896795715265220 ) ) ;
#8373 = EDGE_LOOP ( 'NONE', ( #82400, #81364, #79540, #5600 ) ) ;
#8374 = CARTESIAN_POINT ( 'NONE',  ( 206.8217325168575371, 270.0045844243117017, 3.350393751014514532 ) ) ;
#8375 = CARTESIAN_POINT ( 'NONE',  ( 181.9483594117699568, 259.9271416659100851, -11.10351924915216948 ) ) ;
#8376 = FACE_OUTER_BOUND ( 'NONE', #40190, .T. ) ;
#8377 = CARTESIAN_POINT ( 'NONE',  ( 80.63908856232002620, 57.54704143882187140, -16.24041183338051297 ) ) ;
#8378 = CARTESIAN_POINT ( 'NONE',  ( 155.3017250444513024, 261.6565170503553190, 18.58368563027307374 ) ) ;
#8379 = CARTESIAN_POINT ( 'NONE',  ( 161.8882824960653579, 250.2482648971885340, -13.83574485983625557 ) ) ;
#8380 = CARTESIAN_POINT ( 'NONE',  ( 43.33680334696484948, 124.1889737374328462, 10.00000000000000000 ) ) ;
#8381 = CARTESIAN_POINT ( 'NONE',  ( 194.2154056360670040, 294.2560451561701029, -15.66696967429384557 ) ) ;
#8382 = CARTESIAN_POINT ( 'NONE',  ( 191.8200757322313166, 264.7651863584280250, 7.775292329195298890 ) ) ;
#8383 = LINE ( 'NONE', #37766, #48222 ) ;
#8384 = CARTESIAN_POINT ( 'NONE',  ( 18.71383987920370728, 191.6115022471903160, -5.000000000000047962 ) ) ;
#8385 = CARTESIAN_POINT ( 'NONE',  ( 146.6138605399200117, 276.7043397814778132, -0.5394499176159462950 ) ) ;
#8386 = CARTESIAN_POINT ( 'NONE',  ( 148.2267527339363369, 273.9107285543102535, 7.913369084260907016 ) ) ;
#8387 = CARTESIAN_POINT ( 'NONE',  ( -19.65312891409030271, 93.06504152958497400, 45.00000000000000711 ) ) ;
#8388 = ORIENTED_EDGE ( 'NONE', *, *, #78097, .T. ) ;
#8389 = DIRECTION ( 'NONE',  ( -0.000000000000000000, -0.000000000000000000, 1.000000000000000000 ) ) ;
#8390 = CARTESIAN_POINT ( 'NONE',  ( 82.00425190520714125, 41.38475440514466186, -5.931279945963702005 ) ) ;
#8391 = CARTESIAN_POINT ( 'NONE',  ( 110.6480226958041158, 228.5643266524160708, 9.188101187500095079 ) ) ;
#8392 = CARTESIAN_POINT ( 'NONE',  ( 13.26084062165525523, 25.84336893147755276, -7.433330006724137462 ) ) ;
#8393 = CARTESIAN_POINT ( 'NONE',  ( 190.9501423151522772, 299.9116471280854626, 8.746938802470586083 ) ) ;
#8394 = DIRECTION ( 'NONE',  ( -0.3037402332698203589, -0.8935232438716380621, -0.3306933373297692436 ) ) ;
#8396 = CARTESIAN_POINT ( 'NONE',  ( 87.14941533941508567, 43.54552546780055877, 0.3078308432578384934 ) ) ;
#8395 = CARTESIAN_POINT ( 'NONE',  ( 144.5581563630821051, 244.2677522451417929, -5.000000000000041744 ) ) ;
#8397 = CARTESIAN_POINT ( 'NONE',  ( 190.8990369860722183, 300.0001641545892994, -8.015708032567667729 ) ) ;
#8398 = DIRECTION ( 'NONE',  ( -0.6855440362341557181, 0.7280311630581363103, 0.000000000000000000 ) ) ;
#8399 = CARTESIAN_POINT ( 'NONE',  ( 196.4808189786114951, 290.3322341467384717, -17.84817245450773271 ) ) ;
#8400 = CARTESIAN_POINT ( 'NONE',  ( 192.5076277540105423, 297.2140032159341558, -13.10094381206144298 ) ) ;
#8401 = CARTESIAN_POINT ( 'NONE',  ( 81.40599722213572420, 56.18777044664494014, -16.43392898140639957 ) ) ;
#8402 = VERTEX_POINT ( 'NONE', #42765 ) ;
#8403 = CARTESIAN_POINT ( 'NONE',  ( 192.8451718961534311, 267.2100971994023553, 11.16589986606910756 ) ) ;
#8404 = CARTESIAN_POINT ( 'NONE',  ( 177.5337925685473408, 280.1858537220425092, 16.79564202278857721 ) ) ;
#8405 = CARTESIAN_POINT ( 'NONE',  ( 196.8542736181493922, 268.1164828960293676, 9.403776070750170746 ) ) ;
#8406 = ORIENTED_EDGE ( 'NONE', *, *, #55999, .T. ) ;
#8407 = B_SPLINE_SURFACE_WITH_KNOTS ( 'NONE', 3, 1, ( 
 ( #32735, #1853 ),
 ( #96589, #64652 ),
 ( #17538, #26646 ),
 ( #49941, #72266 ),
 ( #26149, #3848 ),
 ( #41322, #19572 ),
 ( #9447, #27153 ),
 ( #40816, #19067 ),
 ( #33762, #57027 ),
 ( #49437, #87010 ),
 ( #71259, #2872 ),
 ( #18558, #79391 ),
 ( #80390, #63639 ),
 ( #48445, #25132 ),
 ( #9957, #56014 ),
 ( #64141, #71763 ),
 ( #87524, #2359 ),
 ( #56535, #34732 ),
 ( #10960, #33237 ),
 ( #41832, #72778 ),
 ( #95091, #18056 ),
 ( #25655, #34244 ),
 ( #65140, #88505 ),
 ( #65632, #11472 ),
 ( #80901, #50432 ),
 ( #42326, #73254 ),
 ( #58038, #44317 ),
 ( #75747, #74269 ),
 ( #11955, #82877 ),
 ( #12453, #43323 ),
 ( #91459, #90487 ),
 ( #36222, #6330 ),
 ( #82394, #60503 ),
 ( #81387, #99047 ) ),
 .UNSPECIFIED., .T., .F., .F.,
 ( 4, 2, 2, 2, 2, 2, 2, 2, 2, 2, 2, 2, 2, 2, 2, 2, 4 ),
 ( 2, 2 ),
 ( 0.000000000000000000, 0.06250000000000000000, 0.1250000000000000000, 0.1875000000000000000, 0.2500000000000000000, 0.3125000000000000000, 0.3750000000000000000, 0.4375000000000000000, 0.5000000000000000000, 0.5625000000000000000, 0.6250000000000000000, 0.6875000000000000000, 0.7500000000000000000, 0.8125000000000000000, 0.8750000000000000000, 0.9375000000000000000, 1.000000000000000000 ),
 ( 0.000000000000000000, 1.000000000000000000 ),
 .UNSPECIFIED. ) ;
#8408 = CARTESIAN_POINT ( 'NONE',  ( 190.6688270659779221, 284.0946164064107506, -17.60360843008351495 ) ) ;
#8409 = CARTESIAN_POINT ( 'NONE',  ( 179.9379124811931945, 262.8721604542064370, -12.83149901144461147 ) ) ;
#8410 = DIRECTION ( 'NONE',  ( 0.000000000000000000, 0.000000000000000000, 1.000000000000000000 ) ) ;
#8411 = CARTESIAN_POINT ( 'NONE',  ( 175.7824178399792174, 285.8628427244275372, -13.39878279634721103 ) ) ;
#8412 = ORIENTED_EDGE ( 'NONE', *, *, #41376, .F. ) ;
#8413 = CARTESIAN_POINT ( 'NONE',  ( 73.15617415350918407, 69.83382733437846923, 9.602067989434942774 ) ) ;
#8414 = CARTESIAN_POINT ( 'NONE',  ( 30.11829213135327521, 40.49540643055189548, 3.479690158560446702E-15 ) ) ;
#8415 = VERTEX_POINT ( 'NONE', #96041 ) ;
#8416 = CARTESIAN_POINT ( 'NONE',  ( 165.7186082895867685, 248.5901142549738836, 7.040988221872656716 ) ) ;
#8417 = CARTESIAN_POINT ( 'NONE',  ( -89.11465314115667979, 93.37593066204033221, -30.52142883766496695 ) ) ;
#8418 = CARTESIAN_POINT ( 'NONE',  ( 204.4329329219251861, 276.5587687693421799, 13.28840463846547948 ) ) ;
#8420 = ADVANCED_FACE ( 'NONE', ( #49892 ), #80850, .T. ) ;
#8419 = ORIENTED_EDGE ( 'NONE', *, *, #82703, .T. ) ;
#8421 = CARTESIAN_POINT ( 'NONE',  ( 74.49716087599448144, 188.9919560658248656, 17.97570218321540381 ) ) ;
#8422 = CARTESIAN_POINT ( 'NONE',  ( 158.8391802440265508, 255.5294649151923636, 17.60341940305819364 ) ) ;
#8423 = CARTESIAN_POINT ( 'NONE',  ( 192.8238735239056325, 296.6662494747970982, -11.98739424064265791 ) ) ;
#8424 = CARTESIAN_POINT ( 'NONE',  ( 160.8697417715285951, 254.0124291816641176, 15.72951850990217437 ) ) ;
#8425 = CARTESIAN_POINT ( 'NONE',  ( 86.69150557076659425, 44.85198809650525931, -7.441768515828623975 ) ) ;
#8426 = CARTESIAN_POINT ( 'NONE',  ( 84.82070890866113189, 50.11195492342548619, -13.71672402108478295 ) ) ;
#8427 = CARTESIAN_POINT ( 'NONE',  ( 81.57862098688173091, 55.52127002482139062, -16.32346926850663138 ) ) ;
#8428 = VERTEX_POINT ( 'NONE', #27606 ) ;
#8429 = ADVANCED_FACE ( 'NONE', ( #20001 ), #69543, .T. ) ;
#8430 = B_SPLINE_CURVE_WITH_KNOTS ( 'NONE', 3,
 ( #40546, #80107, #31947, #56756, #40040, #16258, #78074, #79609, #63362, #25357, #71481, #86719, #70981, #17776, #24367, #1582, #24855, #39533, #94302, #62850, #64871, #85727, #71976, #47645, #48160, #55239, #86220, #32465, #16756, #55730, #2076 ),
 .UNSPECIFIED., .F., .F.,
 ( 4, 3, 3, 3, 3, 3, 3, 3, 3, 3, 4 ),
 ( 0.000000000000000000, 0.1333490885032380391, 0.3007194338854225490, 0.4699862290244999907, 0.5844252810809225096, 0.6686540514502540278, 0.7354980260655328284, 0.8028463152565535887, 0.8633854507757017238, 0.9437142632667037123, 1.000000000000000000 ),
 .UNSPECIFIED. ) ;
#8431 = ORIENTED_EDGE ( 'NONE', *, *, #21816, .T. ) ;
#8432 = CARTESIAN_POINT ( 'NONE',  ( 163.4927498574098763, 249.4692459082536686, 11.48939803020791750 ) ) ;
#8433 = EDGE_CURVE ( 'NONE', #23987, #52618, #46688, .T. ) ;
#8434 = ORIENTED_EDGE ( 'NONE', *, *, #80875, .F. ) ;
#8435 = CARTESIAN_POINT ( 'NONE',  ( 77.13037345566432634, 49.39794710691812440, -14.91965009447810075 ) ) ;
#8436 = VERTEX_POINT ( 'NONE', #30075 ) ;
#8437 = CARTESIAN_POINT ( 'NONE',  ( 170.2642345923708547, 269.6161715210895409, 17.76022440076183884 ) ) ;
#8438 = PLANE ( 'NONE',  #42869 ) ;
#8439 = ORIENTED_EDGE ( 'NONE', *, *, #36258, .F. ) ;
#8440 = CARTESIAN_POINT ( 'NONE',  ( 189.5059428776464756, 300.4130739301078279, -3.423561384717671796 ) ) ;
#8441 = CARTESIAN_POINT ( 'NONE',  ( 164.9133935349224203, 245.0086188793504505, -2.355115420316610919 ) ) ;
#8442 = CARTESIAN_POINT ( 'NONE',  ( 147.6498877563539338, 274.9098880045899591, -7.398802595780497704 ) ) ;
#8443 = LINE ( 'NONE', #25130, #17252 ) ;
#8444 = CARTESIAN_POINT ( 'NONE',  ( 82.48604300211468399, 40.98759103253163261, 1.037444262390686545 ) ) ;
#8445 = CARTESIAN_POINT ( 'NONE',  ( -86.81108781737714253, 0.000000000000000000, 9.212605237762135246 ) ) ;
#8446 = DIRECTION ( 'NONE',  ( -0.000000000000000000, -0.000000000000000000, -1.000000000000000000 ) ) ;
#8447 = CARTESIAN_POINT ( 'NONE',  ( 178.2153940782017401, 255.1407320482941827, 5.786499683232065649 ) ) ;
#8448 = CARTESIAN_POINT ( 'NONE',  ( 123.3944002380500677, 251.2369531367911293, -4.594050593750048428 ) ) ;
#8449 = CARTESIAN_POINT ( 'NONE',  ( 186.6324081443715386, 262.7608654827037640, -9.067671514656064247 ) ) ;
#8450 = CARTESIAN_POINT ( 'NONE',  ( 34.24030602833327208, 37.95586893147758900, 7.433330006724141015 ) ) ;
#8451 = CARTESIAN_POINT ( 'NONE',  ( 177.3599088863647353, 288.7283238914923800, -9.631439042632086611 ) ) ;
#8452 = ORIENTED_EDGE ( 'NONE', *, *, #49958, .T. ) ;
#8453 = CARTESIAN_POINT ( 'NONE',  ( 202.4565886109826067, 275.5626669239693456, 13.30823948595258344 ) ) ;
#8454 = CARTESIAN_POINT ( 'NONE',  ( 178.2432059713528645, 254.4564803675171163, 1.335616806069444884 ) ) ;
#8455 = CARTESIAN_POINT ( 'NONE',  ( 173.6388580828917441, 290.5488920705779492, -4.957402522865826278 ) ) ;
#8456 = CARTESIAN_POINT ( 'NONE',  ( 157.7365441389748923, 257.4392866714015895, 18.13124212464487073 ) ) ;
#8457 = DIRECTION ( 'NONE',  ( 0.4999999999999992784, -0.8660254037844390407, 0.000000000000000000 ) ) ;
#8458 = CARTESIAN_POINT ( 'NONE',  ( 152.6692142062575499, 266.2161595735824449, -16.77985299603479419 ) ) ;
#8459 = CARTESIAN_POINT ( 'NONE',  ( 173.4606779374792325, 267.5814416807811540, -17.58000433512257032 ) ) ;
#8460 = DIRECTION ( 'NONE',  ( -0.9054088711727241723, 0.4245406647209821194, 0.000000000000000000 ) ) ;
#8461 = CARTESIAN_POINT ( 'NONE',  ( 45.11483101423404918, 69.99284853207299761, -10.00000000000000000 ) ) ;
#8462 =( BOUNDED_CURVE ( )  B_SPLINE_CURVE ( 2, ( #34554, #57845, #99733, #92174, #11286, #3676, #65452, #88826, #50250, #19391, #81204, #54146, #6079 ),
 .UNSPECIFIED., .F., .T. ) 
 B_SPLINE_CURVE_WITH_KNOTS ( ( 3, 2, 2, 2, 2, 2, 3 ),
 ( 0.6125000000000000444, 0.6149999999999999911, 0.6199999999999999956, 0.6250000000000000000, 0.6300000000000000044, 0.6350000000000000089, 0.6375000000000000666 ),
 .UNSPECIFIED. ) 
 CURVE ( )  GEOMETRIC_REPRESENTATION_ITEM ( )  RATIONAL_B_SPLINE_CURVE ( ( 0.9755282581475767101, 0.9755282581475772652, 1.000000000000000000, 0.9510565162951535312, 1.000000000000000000, 0.9510565162951535312, 1.000000000000000000, 0.9510565162951535312, 1.000000000000000000, 0.9510565162951535312, 1.000000000000000000, 0.9755282581475761550, 0.9755282581475767101 ) ) 
 REPRESENTATION_ITEM ( '' )  );
#8463 = VERTEX_POINT ( 'NONE', #82832 ) ;
#8465 = ADVANCED_FACE ( 'NONE', ( #13401 ), #60962, .F. ) ;
#8464 = CARTESIAN_POINT ( 'NONE',  ( 200.5914588262792222, 282.7033700937254821, -16.73555027083989444 ) ) ;
#8466 = CARTESIAN_POINT ( 'NONE',  ( 191.2366886875849161, 273.4737008325631109, 16.52053026652336243 ) ) ;
#8467 = ORIENTED_EDGE ( 'NONE', *, *, #91733, .T. ) ;
#8468 = CARTESIAN_POINT ( 'NONE',  ( 191.7469437388539859, 267.7966411536362443, -12.31490334707406831 ) ) ;
#8469 = EDGE_CURVE ( 'NONE', #22887, #63648, #2191, .T. ) ;
#8470 = CARTESIAN_POINT ( 'NONE',  ( 190.8075292873213300, 283.8500300119202961, -16.71192585804572417 ) ) ;
#8471 = CARTESIAN_POINT ( 'NONE',  ( 173.8469137325424185, 256.4471593116459189, -12.44389045026504270 ) ) ;
#8472 = CARTESIAN_POINT ( 'NONE',  ( 182.3700640764176342, 263.2847133751610045, -13.94439451147478337 ) ) ;
#8473 = FACE_OUTER_BOUND ( 'NONE', #44070, .T. ) ;
#8475 = CARTESIAN_POINT ( 'NONE',  ( 154.9387540737944278, 277.5755234473050450, -8.926225623114506291 ) ) ;
#8474 = CARTESIAN_POINT ( 'NONE',  ( 164.4287473828328245, 284.2046671292196720, -6.974946200865640655 ) ) ;
#8476 = AXIS2_PLACEMENT_3D ( 'NONE', #35070, #36558, #12293 ) ;
#8477 = LINE ( 'NONE', #78390, #55943 ) ;
#8478 = EDGE_LOOP ( 'NONE', ( #51154, #77489, #24724, #33114, #10678, #81299 ) ) ;
#8479 = CARTESIAN_POINT ( 'NONE',  ( 205.2147764766343414, 272.0456487616545473, -9.529409070406817506 ) ) ;
#8480 = CARTESIAN_POINT ( 'NONE',  ( 188.6301707762981152, 265.0060877223691591, -12.46499516475016733 ) ) ;
#8481 = CARTESIAN_POINT ( 'NONE',  ( 72.58119924679503754, 61.32661626603242411, 15.29587950369362659 ) ) ;
#8482 = ADVANCED_FACE ( 'NONE', ( #63475 ), #20983, .T. ) ;
#8483 = DIRECTION ( 'NONE',  ( 0.1857746241280557320, -0.9825923819316327856, 0.000000000000000000 ) ) ;
#8484 = CARTESIAN_POINT ( 'NONE',  ( 25.04665064082949755, 195.2677522451419350, -5.000000000000047962 ) ) ;
#8485 = CARTESIAN_POINT ( 'NONE',  ( 184.5690160051166515, 296.9465964437451930, -4.422075520720778030 ) ) ;
#8486 = FACE_OUTER_BOUND ( 'NONE', #25343, .T. ) ;
#8487 = CARTESIAN_POINT ( 'NONE',  ( 32.84087927488948822, 189.7677522451418497, 10.00000000000009592 ) ) ;
#8488 = CARTESIAN_POINT ( 'NONE',  ( 194.1153812227096864, 294.4292925221022870, 15.54001482840963710 ) ) ;
#8489 = CARTESIAN_POINT ( 'NONE',  ( 71.27925295011586115, 71.54457879798044928, -2.991972160359442245 ) ) ;
#8490 = CARTESIAN_POINT ( 'NONE',  ( -16.14394294671762253, 170.6744531367911293, 4.594050593750047540 ) ) ;
#8491 = CARTESIAN_POINT ( 'NONE',  ( 92.13672968991174628, 217.8768266524159856, 9.188101187500098632 ) ) ;
#8492 = CARTESIAN_POINT ( 'NONE',  ( 31.70422093597033353, 189.1115022471902591, 10.00000000000009592 ) ) ;
#8493 = CARTESIAN_POINT ( 'NONE',  ( 193.2053309019613891, 296.0055459150826778, -12.79465285318189061 ) ) ;
#8494 = CARTESIAN_POINT ( 'NONE',  ( 49.06003799288187395, 95.45573527953635562, 10.00000000000000000 ) ) ;
#8495 = CARTESIAN_POINT ( 'NONE',  ( -26.67497870591645537, 34.81099221456150872, 59.99999999999999289 ) ) ;
#8496 = VECTOR ( 'NONE', #19471, 1000.000000000000000 ) ;
#8497 = CARTESIAN_POINT ( 'NONE',  ( 78.18654183438681571, 55.67423588053517847, 16.15312830067003347 ) ) ;
#8498 = DIRECTION ( 'NONE',  ( -0.5000000000000012212, 0.8660254037844379305, -0.000000000000000000 ) ) ;
#8499 = DIRECTION ( 'NONE',  ( 0.4999999999999998890, -0.8660254037844385966, 0.000000000000000000 ) ) ;
#8501 = CARTESIAN_POINT ( 'NONE',  ( 76.20222849767326068, 51.12960822232545155, 16.07471935095281523 ) ) ;
#8500 = CARTESIAN_POINT ( 'NONE',  ( 73.11394343355392778, 69.60018041412448042, -9.852821959973875110 ) ) ;
#8502 = CARTESIAN_POINT ( 'NONE',  ( 161.2489332459614957, 251.3556502821494121, 13.48038699008507990 ) ) ;
#8503 = CARTESIAN_POINT ( 'NONE',  ( 167.5395076046425800, 250.9340159416122447, -8.858151787760693452 ) ) ;
#8504 = CARTESIAN_POINT ( 'NONE',  ( 161.5266078408477597, 251.3399204103630211, 13.01505764280997468 ) ) ;
#8505 = CARTESIAN_POINT ( 'NONE',  ( 195.6986305151803549, 291.6870243064952888, 16.84182339398051909 ) ) ;
#8506 = DIRECTION ( 'NONE',  ( -0.9762722099447388446, -0.2165469281463391349, 0.000000000000000000 ) ) ;
#8507 = EDGE_CURVE ( 'NONE', #25441, #15769, #79721, .T. ) ;
#8508 = CARTESIAN_POINT ( 'NONE',  ( 161.3145230519951951, 251.2420454056404822, -14.44869077440025151 ) ) ;
#8509 = CARTESIAN_POINT ( 'NONE',  ( 36.16983797034238535, 185.5643266524159856, -9.188101187500093303 ) ) ;
#8510 = EDGE_CURVE ( 'NONE', #2857, #10423, #4672, .T. ) ;
#8511 = CARTESIAN_POINT ( 'NONE',  ( 75.14098114064213974, 208.0643266524159571, -9.188101187500093303 ) ) ;
#8512 = CARTESIAN_POINT ( 'NONE',  ( 164.5641499066685469, 246.8022252770303169, -5.664862832761055955 ) ) ;
#8513 = CARTESIAN_POINT ( 'NONE',  ( 87.99782063670886600, 43.98249463337865706, 0.5325925290962013614 ) ) ;
#8514 = CARTESIAN_POINT ( 'NONE',  ( 167.2234229972659421, 259.6915297064097672, 16.30524142717095515 ) ) ;
#8515 = CARTESIAN_POINT ( 'NONE',  ( 143.5566409438477820, 259.8149278399160949, 9.188101187500093303 ) ) ;
#8517 = CARTESIAN_POINT ( 'NONE',  ( 68.44407863485662347, 70.43973750203463169, -2.495858633798906823 ) ) ;
#8516 = CARTESIAN_POINT ( 'NONE',  ( 71.82992063434448937, 72.13096581328876766, -3.644439638307356955 ) ) ;
#8518 = CARTESIAN_POINT ( 'NONE',  ( 14.20097916528452942, 190.5530062829863311, -4.648177544792955347E-16 ) ) ;
#8519 = CARTESIAN_POINT ( 'NONE',  ( 27.19903172117837542, 31.10171378149920329, 9.188101187500008038 ) ) ;
#8520 = CARTESIAN_POINT ( 'NONE',  ( 150.6386650955079176, 269.7331738006648720, -15.06054658539322766 ) ) ;
#8521 = CARTESIAN_POINT ( 'NONE',  ( 83.07165552766419125, 47.06640118489292490, -11.74642504952208100 ) ) ;
#8522 = CARTESIAN_POINT ( 'NONE',  ( 16.50122538818396478, 18.03085787977762422, 9.188101187500006262 ) ) ;
#8523 = CARTESIAN_POINT ( 'NONE',  ( 65.10058588945754821, 199.2048013555409796, 4.594050593750051981 ) ) ;
#8524 = CARTESIAN_POINT ( 'NONE',  ( 77.00565391796482118, 63.79498567146314514, 14.95288047763914818 ) ) ;
#8525 = CARTESIAN_POINT ( 'NONE',  ( 202.8549823380854491, 279.2918593523859272, -16.39745931995414807 ) ) ;
#8526 = CARTESIAN_POINT ( 'NONE',  ( 198.0858447170796524, 287.5522480202560018, 18.44384186289807559 ) ) ;
#8527 = DIRECTION ( 'NONE',  ( -0.1269555777209603886, -0.9919084036772434221, 0.000000000000000000 ) ) ;
#8528 = CARTESIAN_POINT ( 'NONE',  ( 153.3566685561987413, 276.8094205549507478, 7.774810562162696392 ) ) ;
#8529 = CARTESIAN_POINT ( 'NONE',  ( 75.58399524922207036, 56.66972461617102397, -16.12440502727555014 ) ) ;
#8530 = CARTESIAN_POINT ( 'NONE',  ( 108.3474691708931630, 233.3615022471902591, -10.00000000000009592 ) ) ;
#8531 = DIRECTION ( 'NONE',  ( 0.000000000000000000, 0.000000000000000000, 1.000000000000000000 ) ) ;
#8532 = CARTESIAN_POINT ( 'NONE',  ( 206.9258336080761183, 272.2409381227055292, 6.776000910836894597 ) ) ;
#8533 = ORIENTED_EDGE ( 'NONE', *, *, #96544, .T. ) ;
#8534 = CARTESIAN_POINT ( 'NONE',  ( 77.07619724897867286, 49.54099758213720861, 15.49150516855853965 ) ) ;
#8535 = CARTESIAN_POINT ( 'NONE',  ( 184.7142690891777477, 271.2188788038347411, 16.19071692680373431 ) ) ;
#8536 = ORIENTED_EDGE ( 'NONE', *, *, #63108, .F. ) ;
#8537 = CARTESIAN_POINT ( 'NONE',  ( 159.6288139302610887, 254.1617792512662675, -15.32287760493869477 ) ) ;
#8538 = CARTESIAN_POINT ( 'NONE',  ( 187.2565225563074023, 276.7898775566360996, -17.55325849615163492 ) ) ;
#8539 = DIRECTION ( 'NONE',  ( 0.4999999999999992784, -0.8660254037844390407, 0.000000000000000000 ) ) ;
#8540 = VERTEX_POINT ( 'NONE', #88336 ) ;
#8541 = CARTESIAN_POINT ( 'NONE',  ( 175.2877164847554923, 252.7615608265838034, -0.2531314936308718955 ) ) ;
#8542 = VERTEX_POINT ( 'NONE', #87846 ) ;
#8543 = DIRECTION ( 'NONE',  ( 0.8660254037844395958, 0.4999999999999985567, 0.000000000000000000 ) ) ;
#8544 = CARTESIAN_POINT ( 'NONE',  ( 194.9636675848471441, 292.9600174435121289, -15.57898232594655319 ) ) ;
#8545 = DIRECTION ( 'NONE',  ( -0.4999999999999998890, 0.8660254037844385966, 0.000000000000000000 ) ) ;
#8546 = VECTOR ( 'NONE', #38148, 1000.000000000000000 ) ;
#8548 = ORIENTED_EDGE ( 'NONE', *, *, #27020, .T. ) ;
#8547 = VECTOR ( 'NONE', #8896, 999.9999999999998863 ) ;
#8549 = CARTESIAN_POINT ( 'NONE',  ( 29.15721111571870949, 19.76004757982091320, 5.678558825948272215 ) ) ;
#8550 = CARTESIAN_POINT ( 'NONE',  ( 80.05490797256598512, 44.33250473515553836, 11.49671090876265112 ) ) ;
#8551 = CARTESIAN_POINT ( 'NONE',  ( 66.33640583476365293, 68.86678167005838702, -0.8053330239553019299 ) ) ;
#8552 = CARTESIAN_POINT ( 'NONE',  ( 74.79265276366314197, 66.79451150088600286, -13.18326711696948017 ) ) ;
#8553 = VECTOR ( 'NONE', #23349, 1000.000000000000000 ) ;
#8554 = ORIENTED_EDGE ( 'NONE', *, *, #83804, .F. ) ;
#8556 = EDGE_CURVE ( 'NONE', #36369, #43912, #19404, .T. ) ;
#8555 = CARTESIAN_POINT ( 'NONE',  ( 74.56683408466376761, 152.0817646834693448, 8.907468493598274475E-16 ) ) ;
#8557 = CARTESIAN_POINT ( 'NONE',  ( 194.5579492401075186, 286.5235815387566163, 17.58388259748475235 ) ) ;
#8558 = ADVANCED_FACE ( 'NONE', ( #64981 ), #50263, .T. ) ;
#8559 = ORIENTED_EDGE ( 'NONE', *, *, #6093, .F. ) ;
#8560 = CARTESIAN_POINT ( 'NONE',  ( 174.6714692322213409, 286.2187378199596424, 10.51693356748920039 ) ) ;
#8562 = CARTESIAN_POINT ( 'NONE',  ( 67.68803865064251113, 65.73242611482004349, -10.66275132821461646 ) ) ;
#8561 = CARTESIAN_POINT ( 'NONE',  ( 162.7259096899686313, 284.7569079919674095, -2.578525105315500721 ) ) ;
#8563 = CARTESIAN_POINT ( 'NONE',  ( 163.3409975114459485, 247.7320886816312111, -10.96358124877083640 ) ) ;
#8564 = CARTESIAN_POINT ( 'NONE',  ( 194.5051734451974426, 293.7541525883582381, 14.61790433731063921 ) ) ;
#8565 = CARTESIAN_POINT ( 'NONE',  ( 185.4106159949853634, 292.5018125113814449, -10.86630696919762684 ) ) ;
#8566 = CARTESIAN_POINT ( 'NONE',  ( 205.2414727015710412, 275.1583367910551488, -12.71338796362297963 ) ) ;
#8567 = B_SPLINE_CURVE_WITH_KNOTS ( 'NONE', 3,
 ( #23163, #46457, #79425, #71295 ),
 .UNSPECIFIED., .F., .F.,
 ( 4, 4 ),
 ( 0.01134742446246735960, 0.01727584594350520253 ),
 .UNSPECIFIED. ) ;
#8568 = CARTESIAN_POINT ( 'NONE',  ( 139.3076170325891212, 260.4244531367911577, -4.594050593750046652 ) ) ;
#8569 = CARTESIAN_POINT ( 'NONE',  ( 206.3616846321097853, 270.5654860604214491, 2.445568098436429416 ) ) ;
#8570 = AXIS2_PLACEMENT_3D ( 'NONE', #10162, #33454, #99504 ) ;
#8571 = CARTESIAN_POINT ( 'NONE',  ( 195.3767056438044847, 291.5845065600011026, -15.69873944039788860 ) ) ;
#8572 = CARTESIAN_POINT ( 'NONE',  ( 84.42325706775034178, 228.7369531367911293, -4.594050593750048428 ) ) ;
#8573 = ORIENTED_EDGE ( 'NONE', *, *, #24439, .F. ) ;
#8574 = CARTESIAN_POINT ( 'NONE',  ( 191.4044787581200069, 299.1247133251352466, 7.435199718141230818 ) ) ;
#8575 = DIRECTION ( 'NONE',  ( -1.000000000000000000, 0.000000000000000000, 0.000000000000000000 ) ) ;
#8576 = ORIENTED_EDGE ( 'NONE', *, *, #29047, .F. ) ;
#8577 = CARTESIAN_POINT ( 'NONE',  ( 195.5022618529877150, 292.0271448064274296, -15.80620227310758352 ) ) ;
#8578 = ORIENTED_EDGE ( 'NONE', *, *, #7083, .T. ) ;
#8579 = EDGE_LOOP ( 'NONE', ( #68111, #44555, #69335, #6435 ) ) ;
#8580 = CARTESIAN_POINT ( 'NONE',  ( 80.11894959647150927, 44.23929697926691063, -11.37795504581926842 ) ) ;
#8581 = CYLINDRICAL_SURFACE ( 'NONE', #30061, 70.00000000000002842 ) ;
#8582 = CARTESIAN_POINT ( 'NONE',  ( 146.5310397537613483, 276.8477895910274356, -0.2793038414862049068 ) ) ;
#8583 = DIRECTION ( 'NONE',  ( 1.000000000000000000, 0.000000000000000000, 0.000000000000000000 ) ) ;
#8584 = CARTESIAN_POINT ( 'NONE',  ( 81.30363341997924920, 48.13948513678796814, -13.22891315866029238 ) ) ;
#8585 = DIRECTION ( 'NONE',  ( 0.4999999999999998890, -0.8660254037844385966, 0.000000000000000000 ) ) ;
#8586 = CARTESIAN_POINT ( 'NONE',  ( 84.39645409570583467, 219.5333772461660544, 9.188101187500095079 ) ) ;
#8587 = EDGE_LOOP ( 'NONE', ( #42546, #1569, #55202, #20271 ) ) ;
#8588 = ORIENTED_EDGE ( 'NONE', *, *, #78491, .T. ) ;
#8589 = EDGE_CURVE ( 'NONE', #53003, #57163, #80727, .T. ) ;
#8590 = CARTESIAN_POINT ( 'NONE',  ( 161.4108037507797917, 251.0752823435572623, -14.11420789677157650 ) ) ;
#8591 = ORIENTED_EDGE ( 'NONE', *, *, #97588, .F. ) ;
#8592 = CARTESIAN_POINT ( 'NONE',  ( 24.26937655755794054, 14.41603393254325205, -1.583844403245362020 ) ) ;
#8593 = CARTESIAN_POINT ( 'NONE',  ( 76.28082308479837081, 64.96498169073787210, -14.28860055222916081 ) ) ;
#8594 = CARTESIAN_POINT ( 'NONE',  ( 185.7838608033968910, 272.9513126759449051, -17.26505740043860726 ) ) ;
#8595 = CARTESIAN_POINT ( 'NONE',  ( 207.4096351507161557, 270.9099127066079973, -1.362988047887532694 ) ) ;
#8596 = CARTESIAN_POINT ( 'NONE',  ( 87.60949802315384716, 44.65508912978396694, 4.993525404917304122 ) ) ;
#8597 = EDGE_LOOP ( 'NONE', ( #81403, #71522, #74868, #60209 ) ) ;
#8598 = CARTESIAN_POINT ( 'NONE',  ( 192.2355776333048425, 296.5101708762551311, 11.25704082661979477 ) ) ;
#8599 = CARTESIAN_POINT ( 'NONE',  ( 185.7481537963866458, 259.5269681845950345, 5.863452686169032368 ) ) ;
#8600 = CARTESIAN_POINT ( 'NONE',  ( 200.5039526449628795, 267.3497397166782434, 6.370409075474873006 ) ) ;
#8601 = CARTESIAN_POINT ( 'NONE',  ( 200.7484899876179441, 282.9404111291507888, -16.88964748465601673 ) ) ;
#8602 = PLANE ( 'NONE',  #80570 ) ;
#8603 = CARTESIAN_POINT ( 'NONE',  ( -19.65312891409030271, 93.06504152958497400, 10.00000000000000888 ) ) ;
#8604 = VERTEX_POINT ( 'NONE', #50754 ) ;
#8605 = CARTESIAN_POINT ( 'NONE',  ( 196.2017069210582747, 264.5352342889651709, 5.385840044374106128 ) ) ;
#8606 = DIRECTION ( 'NONE',  ( 0.4999999999999998890, -0.8660254037844385966, 0.000000000000000000 ) ) ;
#8607 = CARTESIAN_POINT ( 'NONE',  ( 29.67553675853319461, 176.3932355074535963, -2.679491924311248496 ) ) ;
#8608 = CARTESIAN_POINT ( 'NONE',  ( 187.9832561701559541, 266.1096952060750596, -13.00726351221733346 ) ) ;
#8609 = FACE_OUTER_BOUND ( 'NONE', #67362, .T. ) ;
#8610 = CARTESIAN_POINT ( 'NONE',  ( 152.8019897319685185, 271.1875699278143088, 14.22014587818035380 ) ) ;
#8611 = ORIENTED_EDGE ( 'NONE', *, *, #75542, .F. ) ;
#8612 = DIRECTION ( 'NONE',  ( -0.8660254037844387076, -0.4999999999999998890, -0.000000000000000000 ) ) ;
#8613 = CARTESIAN_POINT ( 'NONE',  ( 162.9796882977680639, 248.3578945969637743, 9.683801903336119565 ) ) ;
#8614 = EDGE_CURVE ( 'NONE', #54612, #60500, #78106, .T. ) ;
#8615 = FACE_OUTER_BOUND ( 'NONE', #47774, .T. ) ;
#8617 = FACE_BOUND ( 'NONE', #44010, .T. ) ;
#8616 = CARTESIAN_POINT ( 'NONE',  ( 178.5603549463671698, 264.9494309603151692, -15.99590783900550761 ) ) ;
#8618 = CARTESIAN_POINT ( 'NONE',  ( 79.27623980079764010, 52.27818998861121003, 15.92750218127481077 ) ) ;
#8619 = VECTOR ( 'NONE', #17121, 1000.000000000000114 ) ;
#8620 = CARTESIAN_POINT ( 'NONE',  ( 31.49087468139936874, 26.38052372038642091, 10.00000000000000533 ) ) ;
#8621 = CARTESIAN_POINT ( 'NONE',  ( 163.3828304853718407, 283.7865500842125925, -3.144285925872225107 ) ) ;
#8622 = DIRECTION ( 'NONE',  ( -0.000000000000000000, -0.000000000000000000, -1.000000000000000000 ) ) ;
#8623 = CARTESIAN_POINT ( 'NONE',  ( 188.7356621499138214, 259.9383745115107445, 3.760742190882747860 ) ) ;
#8624 = CARTESIAN_POINT ( 'NONE',  ( 161.8807657183444064, 250.2612843381103573, -13.52770735624900311 ) ) ;
#8625 = CARTESIAN_POINT ( 'NONE',  ( 0.9872088458345583684, 177.5024278399160949, 9.188101187500095079 ) ) ;
#8626 = VECTOR ( 'NONE', #43275, 1000.000000000000114 ) ;
#8627 = DIRECTION ( 'NONE',  ( -0.4552093898365321412, 0.8903844177683323258, 0.000000000000000000 ) ) ;
#8628 = VERTEX_POINT ( 'NONE', #41155 ) ;
#8629 = CARTESIAN_POINT ( 'NONE',  ( 160.2015549049794174, 253.9709619308573849, -15.20936558711751552 ) ) ;
#8630 = CARTESIAN_POINT ( 'NONE',  ( -62.95439910331221256, 68.06504152958493137, 60.00000000000000000 ) ) ;
#8631 = DIRECTION ( 'NONE',  ( -0.8660254037844387076, -0.4999999999999998890, -0.000000000000000000 ) ) ;
#8632 = CARTESIAN_POINT ( 'NONE',  ( 21.44705901024191519, 189.3149278399161233, 9.188101187500093303 ) ) ;
#8633 = DIRECTION ( 'NONE',  ( -0.8917477921037005872, -0.4525327339300165286, 0.000000000000000000 ) ) ;
#8634 = CARTESIAN_POINT ( 'NONE',  ( 29.20513097723256024, 32.56454794089043503, 10.00000000000000355 ) ) ;
#8635 = CARTESIAN_POINT ( 'NONE',  ( 83.88249041513446969, 42.01244510319034475, -2.872826126902047417 ) ) ;
#8636 = CARTESIAN_POINT ( 'NONE',  ( 173.4196987977404092, 273.2181934944644013, -16.51998383881567989 ) ) ;
#8637 = CARTESIAN_POINT ( 'NONE',  ( 142.4134467818605572, 241.4824982072973967, 3.021315404115420679E-15 ) ) ;
#8638 = B_SPLINE_SURFACE_WITH_KNOTS ( 'NONE', 3, 1, ( 
 ( #5505, #73421 ),
 ( #36894, #74435 ),
 ( #97724, #52095 ),
 ( #36390, #5016 ),
 ( #42977, #28804 ),
 ( #67295, #73916 ),
 ( #59689, #35897 ),
 ( #13613, #44486 ),
 ( #92633, #30300 ),
 ( #60671, #31286 ),
 ( #61683, #54074 ),
 ( #8013, #84049 ),
 ( #85552, #38885 ),
 ( #69788, #37385 ),
 ( #61185, #77408 ),
 ( #62173, #45484 ),
 ( #46997, #99711 ),
 ( #62678, #77911 ),
 ( #23676, #23182 ),
 ( #68787, #398 ),
 ( #22199, #83542 ),
 ( #14106, #44987 ),
 ( #15082, #7487 ),
 ( #85029, #29799 ),
 ( #100218, #93125 ),
 ( #99213, #53093 ),
 ( #54568, #16093 ),
 ( #8500, #30803 ),
 ( #15576, #91632 ),
 ( #75930, #37876 ),
 ( #39370, #45971 ) ),
 .UNSPECIFIED., .F., .F., .F.,
 ( 4, 3, 3, 3, 3, 3, 3, 3, 3, 3, 4 ),
 ( 2, 2 ),
 ( 0.000000000000000000, 0.1333490885032358464, 0.3007194338854307092, 0.4699862290245053198, 0.5844252810809311693, 0.6686540514502750110, 0.7354980260655511470, 0.8028463152565725736, 0.8633854507757335872, 0.9437142632667383513, 1.000000000000000000 ),
 ( 0.000000000000000000, 1.000000000000000000 ),
 .UNSPECIFIED. ) ;
#8639 = CARTESIAN_POINT ( 'NONE',  ( 187.8983670083758000, 296.6038788229786292, -7.730668491481425875 ) ) ;
#8640 = DIRECTION ( 'NONE',  ( -0.06958655048002569676, 0.1205274409548614395, -0.9902680687415721383 ) ) ;
#8641 = CARTESIAN_POINT ( 'NONE',  ( 65.47921168356340615, 218.6115022471903160, -5.000000000000047962 ) ) ;
#8642 = CARTESIAN_POINT ( 'NONE',  ( 164.4633416896444658, 246.1841640495187846, 1.498163193773305091 ) ) ;
#8643 = CARTESIAN_POINT ( 'NONE',  ( 203.4246719454474146, 270.0952167377922706, 6.029947592111899013 ) ) ;
#8644 = CARTESIAN_POINT ( 'NONE',  ( 31.83936385565518279, 195.3149278399160664, 9.188101187500093303 ) ) ;
#8645 = CARTESIAN_POINT ( 'NONE',  ( 66.71817688721121442, 67.86101298462291709, 6.998882950237777401 ) ) ;
#8646 = CARTESIAN_POINT ( 'NONE',  ( 135.9646106164503010, 237.7592609112380160, 2.679491924311254714 ) ) ;
#8647 = CARTESIAN_POINT ( 'NONE',  ( 203.4080297268528170, 270.2650173722573186, -6.439894855938525176 ) ) ;
#8648 = DIRECTION ( 'NONE',  ( -1.000000000000000000, 0.000000000000000000, 0.000000000000000000 ) ) ;
#8649 = CARTESIAN_POINT ( 'NONE',  ( 80.44215978124604760, 58.39441083166272506, 0.000000000000000000 ) ) ;
#8650 = CARTESIAN_POINT ( 'NONE',  ( -19.53857018403403956, 92.98143509436215481, 59.99999999999999289 ) ) ;
#8651 = CARTESIAN_POINT ( 'NONE',  ( 161.0699900735471601, 279.2409086475570916, -9.794691631822578515 ) ) ;
#8652 = PLANE ( 'NONE',  #95773 ) ;
#8653 = CARTESIAN_POINT ( 'NONE',  ( 17.01121839442928163, 30.79752408145592568, -5.678558825948271327 ) ) ;
#8654 = CARTESIAN_POINT ( 'NONE',  ( 202.7041331321765938, 279.5531378413010657, 17.14708438049711248 ) ) ;
#8655 = FACE_OUTER_BOUND ( 'NONE', #97014, .T. ) ;
#8656 = CARTESIAN_POINT ( 'NONE',  ( 185.6236042504581008, 267.5736580584572266, -14.81396297063468026 ) ) ;
#8657 = ORIENTED_EDGE ( 'NONE', *, *, #42942, .F. ) ;
#8658 = CARTESIAN_POINT ( 'NONE',  ( 6.527493107231251201, 21.95586893147753216, 7.433330006724141015 ) ) ;
#8659 = CARTESIAN_POINT ( 'NONE',  ( 196.8309065691697128, 264.2445955198643901, -3.407952846926960877 ) ) ;
#8660 = CARTESIAN_POINT ( 'NONE',  ( 88.02262071555790612, 44.26851354062424804, 2.809628182802242691 ) ) ;
#8661 = CARTESIAN_POINT ( 'NONE',  ( 45.82169850708434922, 28.58380873178791504, 6.180339887498953466 ) ) ;
#8662 = ORIENTED_EDGE ( 'NONE', *, *, #16471, .F. ) ;
#8663 = CARTESIAN_POINT ( 'NONE',  ( 21.14953632379956616, 183.0177522451418497, -10.00000000000009592 ) ) ;
#8665 = ADVANCED_FACE ( 'NONE', ( #66463 ), #75176, .F. ) ;
#8664 = CARTESIAN_POINT ( 'NONE',  ( 72.54340540113201996, 71.27809821757736586, -6.032689287156388858 ) ) ;
#8667 = CARTESIAN_POINT ( 'NONE',  ( 191.0816511748900268, 299.6838671013740623, 7.311127128005925790 ) ) ;
#8666 = B_SPLINE_CURVE_WITH_KNOTS ( 'NONE', 3,
 ( #97704, #82027, #12092, #50573, #83019, #42954, #35377, #97221, #5485, #35875, #41982, #43469 ),
 .UNSPECIFIED., .F., .F.,
 ( 4, 2, 2, 2, 2, 4 ),
 ( 0.0009047221135296957921, 0.001170349639185115859, 0.001435977164840535926, 0.001967232216151415091, 0.002498487267462294256, 0.003029742318773173421 ),
 .UNSPECIFIED. ) ;
#8668 = CARTESIAN_POINT ( 'NONE',  ( 180.3265683508092820, 256.4805248161748636, -7.849693535446355064 ) ) ;
#8669 = EDGE_CURVE ( 'NONE', #89530, #41986, #63554, .T. ) ;
#8670 = EDGE_LOOP ( 'NONE', ( #87000, #21456, #59012, #82999, #14658, #48072, #24313, #5677 ) ) ;
#8671 = ORIENTED_EDGE ( 'NONE', *, *, #77189, .F. ) ;
#8673 = CARTESIAN_POINT ( 'NONE',  ( 86.97441523645338179, 43.45437750576425628, -1.010700286482205446 ) ) ;
#8672 = CARTESIAN_POINT ( 'NONE',  ( 189.3318025282030135, 274.0192145183515322, -15.65849137438579319 ) ) ;
#8674 = EDGE_LOOP ( 'NONE', ( #19926, #40194, #28069, #5331 ) ) ;
#8675 = CARTESIAN_POINT ( 'NONE',  ( 150.6655900823359389, 269.6865383554857090, 15.31288044136207205 ) ) ;
#8676 = CARTESIAN_POINT ( 'NONE',  ( 71.92536400468701174, 72.18844424196340981, -3.635291937859653544 ) ) ;
#8677 = CARTESIAN_POINT ( 'NONE',  ( 80.02542612678608691, 57.59583086733049129, 16.60012225046076040 ) ) ;
#8678 = FACE_OUTER_BOUND ( 'NONE', #67367, .T. ) ;
#8680 = EDGE_CURVE ( 'NONE', #2343, #53789, #71805, .T. ) ;
#8679 = CARTESIAN_POINT ( 'NONE',  ( 190.2476911738421848, 301.1283281946692796, -1.360079143321618611 ) ) ;
#8682 = CIRCLE ( 'NONE', #5444, 0.1418229129684228651 ) ;
#8681 = CARTESIAN_POINT ( 'NONE',  ( 180.3688922265450287, 287.0481539434517231, -13.70161974464981469 ) ) ;
#8683 = EDGE_LOOP ( 'NONE', ( #34598, #94985, #15901, #4207 ) ) ;
#8684 = CARTESIAN_POINT ( 'NONE',  ( 157.2333142128019858, 258.3109064714224132, 16.87956768598436597 ) ) ;
#8685 = CARTESIAN_POINT ( 'NONE',  ( 159.5569985709834384, 265.8568429881750603, 16.74439774012073556 ) ) ;
#8686 = ORIENTED_EDGE ( 'NONE', *, *, #67834, .F. ) ;
#8687 = CARTESIAN_POINT ( 'NONE',  ( 31.98500480842837490, 19.26216523072496400, -2.296566073217252530E-15 ) ) ;
#8688 = CARTESIAN_POINT ( 'NONE',  ( 157.5331533759313913, 259.5764018409500409, 17.61237877605050173 ) ) ;
#8689 = LINE ( 'NONE', #22390, #57963 ) ;
#8690 = CARTESIAN_POINT ( 'NONE',  ( 52.46142023538962462, 213.3464784336661637, 1.353441290958777525E-15 ) ) ;
#8691 = ORIENTED_EDGE ( 'NONE', *, *, #61102, .T. ) ;
#8692 = CARTESIAN_POINT ( 'NONE',  ( 73.91288345017510153, 68.57868192222672121, 10.89134523673511623 ) ) ;
#8693 = CARTESIAN_POINT ( 'NONE',  ( 159.9040744856012850, 255.4269131533854420, 16.38690128260775936 ) ) ;
#8694 = LINE ( 'NONE', #10206, #100082 ) ;
#8695 = CARTESIAN_POINT ( 'NONE',  ( 173.5145074140515362, 271.4604948858709008, 16.42671096914147810 ) ) ;
#8696 = EDGE_LOOP ( 'NONE', ( #20584, #1358, #74403, #37075 ) ) ;
#8697 = ORIENTED_EDGE ( 'NONE', *, *, #17582, .F. ) ;
#8698 = CARTESIAN_POINT ( 'NONE',  ( 86.55745248666850955, 46.28591021298573338, 9.008290149372946587 ) ) ;
#8699 = VECTOR ( 'NONE', #97023, 1000.000000000000000 ) ;
#8700 = CARTESIAN_POINT ( 'NONE',  ( 190.6218339396177441, 300.4802939150614520, -4.178005820806754755 ) ) ;
#8701 = CARTESIAN_POINT ( 'NONE',  ( 190.5154909595809727, 300.6644853595138329, -0.04129855346138300298 ) ) ;
#8702 = VERTEX_POINT ( 'NONE', #48491 ) ;
#8703 = CARTESIAN_POINT ( 'NONE',  ( 174.6738009877982449, 260.4501079225292415, -14.90946296650636604 ) ) ;
#8704 = CARTESIAN_POINT ( 'NONE',  ( 134.2560625007776025, 254.9865022471902876, -10.00000000000009592 ) ) ;
#8705 = CARTESIAN_POINT ( 'NONE',  ( 161.8926315922002743, 250.2407320417157166, -13.77020595223768495 ) ) ;
#8706 = CARTESIAN_POINT ( 'NONE',  ( 147.3379027498079381, 275.4502618871274535, -3.695260257281167249 ) ) ;
#8707 = AXIS2_PLACEMENT_3D ( 'NONE', #35331, #66241, #36824 ) ;
#8708 = CARTESIAN_POINT ( 'NONE',  ( 163.2951241624277827, 257.7631431858913515, 15.56583983124304638 ) ) ;
#8709 = CARTESIAN_POINT ( 'NONE',  ( 69.44407254868087875, 66.48165845397403473, 10.23672187717776083 ) ) ;
#8710 = CARTESIAN_POINT ( 'NONE',  ( 164.2813349609167517, 246.1033764428878214, 1.949810150281061638 ) ) ;
#8711 = CARTESIAN_POINT ( 'NONE',  ( 67.46085622035505480, 67.01197793175170148, 9.005109031795694108 ) ) ;
#8712 = CARTESIAN_POINT ( 'NONE',  ( 74.28630307215421169, 64.63373713051603886, -13.80664065817792263 ) ) ;
#8713 = CARTESIAN_POINT ( 'NONE',  ( 77.98042497925951011, 47.87864476968928074, 14.07985687966458599 ) ) ;
#8714 = CARTESIAN_POINT ( 'NONE',  ( 110.6480226958041158, 228.5643266524160708, 9.188101187500095079 ) ) ;
#8715 = VERTEX_POINT ( 'NONE', #79432 ) ;
#8716 = CARTESIAN_POINT ( 'NONE',  ( 191.5521510896938935, 298.8689373439769952, -9.847378829740700112 ) ) ;
#8717 = CARTESIAN_POINT ( 'NONE',  ( 70.53859886870293394, 66.00395551958487772, 11.32651892520792458 ) ) ;
#8718 = LINE ( 'NONE', #61897, #78669 ) ;
#8719 = CARTESIAN_POINT ( 'NONE',  ( 203.3041373168503299, 278.5139001086923827, -16.61929732091214973 ) ) ;
#8720 = CARTESIAN_POINT ( 'NONE',  ( 183.2981546842155751, 284.6900415564330160, -14.97990253935919469 ) ) ;
#8721 = CARTESIAN_POINT ( 'NONE',  ( 83.88998279704740924, 51.95482724045139378, -14.52911814644455646 ) ) ;
#8722 = CARTESIAN_POINT ( 'NONE',  ( 166.5497620933320775, 284.9599651698292178, -8.643830016708903941 ) ) ;
#8723 = ORIENTED_EDGE ( 'NONE', *, *, #33511, .F. ) ;
#8724 = CARTESIAN_POINT ( 'NONE',  ( 65.92723761088207368, 68.94945291059252668, -2.624861928015914003 ) ) ;
#8725 = CARTESIAN_POINT ( 'NONE',  ( 182.2911844765873184, 260.6002554270507403, 9.501293399576107745 ) ) ;
#8726 = DIRECTION ( 'NONE',  ( -0.000000000000000000, 0.000000000000000000, 1.000000000000000000 ) ) ;
#8727 = CARTESIAN_POINT ( 'NONE',  ( 122.7720312530212396, 247.8149278399160949, 9.188101187500093303 ) ) ;
#8728 = CARTESIAN_POINT ( 'NONE',  ( 198.8194531333411419, 286.2816009704309863, -17.01510935557533344 ) ) ;
#8729 = CARTESIAN_POINT ( 'NONE',  ( 186.0371838319158542, 296.8243199225140643, 4.660811700844511130 ) ) ;
#8730 = CARTESIAN_POINT ( 'NONE',  ( 187.3796900879174245, 281.3202307012271604, -17.28651300096462151 ) ) ;
#8731 = CARTESIAN_POINT ( 'NONE',  ( -51.42721978966704910, 42.16899896210639298, 54.99999999999999289 ) ) ;
#8732 = CARTESIAN_POINT ( 'NONE',  ( 43.96371950863733247, 202.3149278399160949, -9.188101187500095079 ) ) ;
#8733 = ADVANCED_FACE ( 'NONE', ( #40859 ), #2402, .F. ) ;
#8734 = CARTESIAN_POINT ( 'NONE',  ( 85.50592849318395849, 48.29857843294553277, -11.72635531101612294 ) ) ;
#8735 = VERTEX_POINT ( 'NONE', #57570 ) ;
#8736 = CARTESIAN_POINT ( 'NONE',  ( 71.11978001288902362, 63.69250981634468189, 13.25087439340794226 ) ) ;
#8737 = CARTESIAN_POINT ( 'NONE',  ( 84.14312167556933275, 48.98415679381830756, 0.000000000000000000 ) ) ;
#8738 = CARTESIAN_POINT ( 'NONE',  ( 47.97596991287763757, 210.0530062829863027, 1.101618078115930403E-13 ) ) ;
#8739 = CARTESIAN_POINT ( 'NONE',  ( 175.0982648744423216, 261.2275428049201196, 15.10619652427497428 ) ) ;
#8740 = CARTESIAN_POINT ( 'NONE',  ( 82.19821301579139572, 41.48612719278543182, -5.907191800152080674 ) ) ;
#8741 = EDGE_CURVE ( 'NONE', #55876, #74996, #43366, .T. ) ;
#8742 = CARTESIAN_POINT ( 'NONE',  ( 154.8545429534089237, 262.4310591522755089, -17.81746354318405778 ) ) ;
#8743 = CARTESIAN_POINT ( 'NONE',  ( 181.3882225691092742, 262.6214322978779592, 12.41810020290828120 ) ) ;
#8744 = CARTESIAN_POINT ( 'NONE',  ( 119.9486011388743236, 233.3927522451417929, -10.00000000000009059 ) ) ;
#8745 = CARTESIAN_POINT ( 'NONE',  ( 194.1125532102549300, 292.6514872621661993, -15.55923223616878204 ) ) ;
#8746 = ORIENTED_EDGE ( 'NONE', *, *, #4780, .F. ) ;
#8747 = ADVANCED_FACE ( 'NONE', ( #73789 ), #67892, .T. ) ;
#8748 = CARTESIAN_POINT ( 'NONE',  ( 162.7644741734472120, 248.7306563947940958, 9.865755277559742353 ) ) ;
#8749 = CARTESIAN_POINT ( 'NONE',  ( 87.81665660121321082, 44.77054464327975580, 4.981472615147592542 ) ) ;
#8750 = CARTESIAN_POINT ( 'NONE',  ( 33.19304919271588972, 177.7202760586659736, -5.415160957724236172E-17 ) ) ;
#8751 = CARTESIAN_POINT ( 'NONE',  ( 10.15257209397493199, 21.56454794089039240, 10.00000000000000355 ) ) ;
#8752 = PLANE ( 'NONE',  #67799 ) ;
#8753 = CARTESIAN_POINT ( 'NONE',  ( 39.95181620016202118, 182.3262482093457209, 3.021315404115420679E-15 ) ) ;
#8754 = CARTESIAN_POINT ( 'NONE',  ( 71.78531393134818472, 71.87200472712461874, 2.928372626719420335 ) ) ;
#8756 = CARTESIAN_POINT ( 'NONE',  ( 65.42534541587671981, 199.3923013555409796, 4.594050593750050204 ) ) ;
#8755 = CARTESIAN_POINT ( 'NONE',  ( 198.1679321590325458, 277.6257778925182720, -16.56331389466651061 ) ) ;
#8757 = LINE ( 'NONE', #2173, #11074 ) ;
#8758 = CARTESIAN_POINT ( 'NONE',  ( 184.7849722178042668, 257.5454927209563607, 1.385182159486959774 ) ) ;
#8759 = CARTESIAN_POINT ( 'NONE',  ( 157.8429099974857195, 257.2550556002704525, -17.85752049034686095 ) ) ;
#8760 = CARTESIAN_POINT ( 'NONE',  ( 66.77376812102318127, 68.41195941748605946, -4.433129028897188739 ) ) ;
#8761 =( BOUNDED_CURVE ( )  B_SPLINE_CURVE ( 2, ( #10864, #57942, #26061, #27566, #25556, #96490, #72683, #56938, #96001, #18974, #33149, #49848, #4238 ),
 .UNSPECIFIED., .F., .T. ) 
 B_SPLINE_CURVE_WITH_KNOTS ( ( 3, 2, 2, 2, 2, 2, 3 ),
 ( 0.3125000000000000000, 0.3150000000000000022, 0.3200000000000000067, 0.3250000000000000111, 0.3300000000000000155, 0.3350000000000000200, 0.3375000000000000222 ),
 .UNSPECIFIED. ) 
 CURVE ( )  GEOMETRIC_REPRESENTATION_ITEM ( )  RATIONAL_B_SPLINE_CURVE ( ( 0.9755282581475768211, 0.9755282581475768211, 1.000000000000000000, 0.9510565162951535312, 1.000000000000000000, 0.9510565162951535312, 1.000000000000000000, 0.9510565162951535312, 1.000000000000000000, 0.9510565162951535312, 1.000000000000000000, 0.9755282581475768211, 0.9755282581475768211 ) ) 
 REPRESENTATION_ITEM ( '' )  );
#8762 = ORIENTED_EDGE ( 'NONE', *, *, #87455, .T. ) ;
#8763 = CIRCLE ( 'NONE', #58923, 70.00000000000001421 ) ;
#8764 = CARTESIAN_POINT ( 'NONE',  ( 163.7828826429516766, 268.2613608475996898, 16.53282274799222407 ) ) ;
#8765 = CARTESIAN_POINT ( 'NONE',  ( 16.54877636974260824, 190.3615022471903160, 5.000000000000046185 ) ) ;
#8766 = CARTESIAN_POINT ( 'NONE',  ( -12.48997110076107830, 41.83172881028752954, 59.99999999999999289 ) ) ;
#8767 = CARTESIAN_POINT ( 'NONE',  ( 164.4817765375028102, 245.7562014482918755, -6.334578229142199035 ) ) ;
#8768 = CARTESIAN_POINT ( 'NONE',  ( -9.729855525997876953, 171.3149278399160664, 9.188101187500093303 ) ) ;
#8769 = CARTESIAN_POINT ( 'NONE',  ( 24.06271987006732616, 35.93396525600390845, 2.839279412974139660 ) ) ;
#8771 = CARTESIAN_POINT ( 'NONE',  ( 169.8916322304794733, 263.4028382525763732, 15.84815012191193695 ) ) ;
#8770 = CARTESIAN_POINT ( 'NONE',  ( 166.1729740367198644, 261.7477518458006216, -16.21765485240585747 ) ) ;
#8772 = CARTESIAN_POINT ( 'NONE',  ( 185.7044324113292646, 259.6182011128160525, 7.428341809090757586 ) ) ;
#8773 = CARTESIAN_POINT ( 'NONE',  ( 194.5253693406981483, 291.7191722712467481, 16.18900132190417551 ) ) ;
#8774 = CARTESIAN_POINT ( 'NONE',  ( 186.2106335195739462, 257.9955712153812328, -2.495042034395281938 ) ) ;
#8775 = CARTESIAN_POINT ( 'NONE',  ( 66.28418275192433384, 69.17501406156587507, 2.517326374184488014 ) ) ;
#8776 = VERTEX_POINT ( 'NONE', #83914 ) ;
#8777 = CARTESIAN_POINT ( 'NONE',  ( 150.2345823034905550, 271.5449826357299230, -12.44854083486978347 ) ) ;
#8778 = CARTESIAN_POINT ( 'NONE',  ( 177.9669014565158704, 286.2669617536872124, 13.02687325745571378 ) ) ;
#8779 = DIRECTION ( 'NONE',  ( 0.3715724127386967335, -0.6435822975543782354, -0.6691306063588567943 ) ) ;
#8780 = CARTESIAN_POINT ( 'NONE',  ( 9.725772901699041739, 17.56628583063838889, 9.188101187500006262 ) ) ;
#8781 = CYLINDRICAL_SURFACE ( 'NONE', #66756, 17.82106496071139645 ) ;
#8782 = CARTESIAN_POINT ( 'NONE',  ( 88.29579885706220921, 44.29800590334696153, -2.024579815269742067 ) ) ;
#8783 = EDGE_CURVE ( 'NONE', #59656, #18632, #93742, .T. ) ;
#8784 = CARTESIAN_POINT ( 'NONE',  ( 152.6845319923753834, 266.1896283897672220, 17.20844521882669653 ) ) ;
#8785 = CARTESIAN_POINT ( 'NONE',  ( 49.04287251715432916, 95.72274150194785136, -10.00000000000000000 ) ) ;
#8786 = B_SPLINE_CURVE_WITH_KNOTS ( 'NONE', 3,
 ( #85864, #84832, #62467, #53870 ),
 .UNSPECIFIED., .F., .F.,
 ( 4, 4 ),
 ( 0.004989422848796198559, 0.009972366782226169124 ),
 .UNSPECIFIED. ) ;
#8787 = CARTESIAN_POINT ( 'NONE',  ( 136.0806360202347491, 237.8262482093457493, 3.021315404115420679E-15 ) ) ;
#8788 = CARTESIAN_POINT ( 'NONE',  ( 163.4222916751007801, 247.5912830598222172, -10.52132777929285012 ) ) ;
#8789 = CARTESIAN_POINT ( 'NONE',  ( 43.63646518856938172, 66.22046553916848666, -10.00000000000000000 ) ) ;
#8790 = VERTEX_POINT ( 'NONE', #61045 ) ;
#8791 = ORIENTED_EDGE ( 'NONE', *, *, #11979, .T. ) ;
#8792 = CARTESIAN_POINT ( 'NONE',  ( 155.8093079659346074, 277.0108043004451588, -10.30466594370042621 ) ) ;
#8793 = CARTESIAN_POINT ( 'NONE',  ( 81.87359138893998534, 41.32955797152819599, 5.976920566253460798 ) ) ;
#8794 = ORIENTED_EDGE ( 'NONE', *, *, #68953, .F. ) ;
#8795 = EDGE_CURVE ( 'NONE', #65497, #57017, #2867, .T. ) ;
#8796 = CARTESIAN_POINT ( 'NONE',  ( 155.5450984722979229, 262.5874973419817024, -17.41340391108767705 ) ) ;
#8797 = VERTEX_POINT ( 'NONE', #28175 ) ;
#8799 = EDGE_CURVE ( 'NONE', #87128, #2619, #29184, .T. ) ;
#8798 = CARTESIAN_POINT ( 'NONE',  ( 191.0604813119340690, 299.7205343796033503, -9.270812881586136811 ) ) ;
#8800 = CARTESIAN_POINT ( 'NONE',  ( -22.42236680055709641, 157.8615022471902591, 0.000000000000000000 ) ) ;
#8801 = CARTESIAN_POINT ( 'NONE',  ( 8.118423711322263259, 28.18528772668516424, -1.583844403245363575 ) ) ;
#8802 = CARTESIAN_POINT ( 'NONE',  ( 80.49736582374534066, 43.65955092740581733, 9.838849738494864994 ) ) ;
#8803 = VERTEX_POINT ( 'NONE', #36762 ) ;
#8804 = CARTESIAN_POINT ( 'NONE',  ( 155.6413935076475639, 261.0681940143705901, 18.42569256965892421 ) ) ;
#8805 = CARTESIAN_POINT ( 'NONE',  ( 191.4044787581200069, 299.1247133251352466, 7.435199718141230818 ) ) ;
#8806 = DIRECTION ( 'NONE',  ( 0.000000000000000000, 0.000000000000000000, 1.000000000000000000 ) ) ;
#8807 = EDGE_LOOP ( 'NONE', ( #17709, #98056, #20655, #15252 ) ) ;
#8808 = ORIENTED_EDGE ( 'NONE', *, *, #31406, .F. ) ;
#8809 = ORIENTED_EDGE ( 'NONE', *, *, #62129, .T. ) ;
#8810 = CARTESIAN_POINT ( 'NONE',  ( 73.87636433878275000, 63.53668594947264836, 14.23734624109727420 ) ) ;
#8811 = ORIENTED_EDGE ( 'NONE', *, *, #60241, .T. ) ;
#8812 = CARTESIAN_POINT ( 'NONE',  ( 160.5893190321802138, 270.9897182155185078, 16.60663562724527864 ) ) ;
#8813 = ORIENTED_EDGE ( 'NONE', *, *, #20301, .F. ) ;
#8814 = CARTESIAN_POINT ( 'NONE',  ( 164.4817765375028102, 245.7562014482918755, -6.334578229142199035 ) ) ;
#8815 = CARTESIAN_POINT ( 'NONE',  ( 83.61782708266594000, 50.72174090158058846, 13.98667043904370644 ) ) ;
#8816 = FACE_OUTER_BOUND ( 'NONE', #63321, .T. ) ;
#8817 = CARTESIAN_POINT ( 'NONE',  ( 148.4042165687623083, 273.6033521758856750, -8.709765892313745539 ) ) ;
#8818 = B_SPLINE_CURVE_WITH_KNOTS ( 'NONE', 3,
 ( #37812, #91077, #76824, #46409 ),
 .UNSPECIFIED., .F., .F.,
 ( 4, 4 ),
 ( 0.01052722645609634883, 0.01597497186318108664 ),
 .UNSPECIFIED. ) ;
#8819 = CARTESIAN_POINT ( 'NONE',  ( 82.56707315150609361, 53.27404436626156325, -15.30997931004315404 ) ) ;
#8820 = CARTESIAN_POINT ( 'NONE',  ( 159.1177508122425195, 255.0469665375489399, -17.04660126523272012 ) ) ;
#8821 = CARTESIAN_POINT ( 'NONE',  ( 166.6156759393427080, 247.0710755757112054, 1.913997305269410587 ) ) ;
#8822 = CARTESIAN_POINT ( 'NONE',  ( 18.74326920199815305, 31.79752408145591858, -5.678558825948271327 ) ) ;
#8823 = CARTESIAN_POINT ( 'NONE',  ( 193.6780271845242964, 277.9462545196296333, -17.36184529900156548 ) ) ;
#8824 = CARTESIAN_POINT ( 'NONE',  ( 164.9103019330012216, 245.0139736909548560, 2.841678961959298810 ) ) ;
#8826 = ORIENTED_EDGE ( 'NONE', *, *, #61576, .F. ) ;
#8825 = CARTESIAN_POINT ( 'NONE',  ( 206.9919585703311213, 271.2130891193729099, 4.989103036379466616 ) ) ;
#8827 = CARTESIAN_POINT ( 'NONE',  ( 147.4517449145323269, 275.2530814737808669, -3.583987543978726986 ) ) ;
#8828 = CARTESIAN_POINT ( 'NONE',  ( 155.5798705649511930, 269.2207634517940278, 16.19704775669435648 ) ) ;
#8829 = CARTESIAN_POINT ( 'NONE',  ( 206.3454060440500086, 273.2462681537123785, -9.268083217908118954 ) ) ;
#8830 = DIRECTION ( 'NONE',  ( -0.3077152132536331575, -0.9514785060800222682, 0.000000000000000000 ) ) ;
#8831 = CARTESIAN_POINT ( 'NONE',  ( 83.28211300506427506, 45.81084018523562662, -10.47891480825111366 ) ) ;
#8832 = AXIS2_PLACEMENT_3D ( 'NONE', #92468, #23015, #75259 ) ;
#8833 = CARTESIAN_POINT ( 'NONE',  ( 161.7101619467568980, 250.5567787384628389, 13.05644392949610655 ) ) ;
#8834 = CARTESIAN_POINT ( 'NONE',  ( 104.8833675557553704, 241.3615022471903160, 5.000000000000046185 ) ) ;
#8835 = EDGE_LOOP ( 'NONE', ( #24603, #86146, #88509, #71785 ) ) ;
#8836 = CARTESIAN_POINT ( 'NONE',  ( 155.1935823099396430, 261.8438257609990956, -17.10498131462595595 ) ) ;
#8837 = CYLINDRICAL_SURFACE ( 'NONE', #96566, 10.00000000000010658 ) ;
#8838 = CARTESIAN_POINT ( 'NONE',  ( 177.4096984176076148, 293.8085471629082122, -0.6315254070814751985 ) ) ;
#8839 = CARTESIAN_POINT ( 'NONE',  ( 17.75760349231054391, 174.3927522451418213, 10.00000000000009592 ) ) ;
#8840 = CARTESIAN_POINT ( 'NONE',  ( 85.88519558028406209, 211.2048013555409796, 4.594050593750051981 ) ) ;
#8841 = VECTOR ( 'NONE', #89682, 1000.000000000000114 ) ;
#8842 = CARTESIAN_POINT ( 'NONE',  ( 82.37532108405909526, 40.36264586417863143, -0.9042686866734450657 ) ) ;
#8843 = DIRECTION ( 'NONE',  ( -0.9303772761487930643, -0.3666034970181715757, 0.000000000000000000 ) ) ;
#8844 = CARTESIAN_POINT ( 'NONE',  ( 167.0053736619712765, 278.0716144694669083, -13.57399711851867785 ) ) ;
#8846 = CARTESIAN_POINT ( 'NONE',  ( 75.72624665019681345, 65.60512238633357640, 13.80728453669184930 ) ) ;
#8845 = CARTESIAN_POINT ( 'NONE',  ( 10.02652254571713719, 176.5958772461660544, -9.188101187500095079 ) ) ;
#8847 = EDGE_CURVE ( 'NONE', #4682, #46017, #62273, .T. ) ;
#8848 = CARTESIAN_POINT ( 'NONE',  ( 200.6097954076514895, 283.1806371883870383, 16.82611162221071766 ) ) ;
#8849 = EDGE_LOOP ( 'NONE', ( #90481, #9070, #75347, #22436 ) ) ;
#8851 = ORIENTED_EDGE ( 'NONE', *, *, #4696, .T. ) ;
#8850 = UNCERTAINTY_MEASURE_WITH_UNIT (LENGTH_MEASURE( 1.000000000000000082E-05 ), #27316, 'distance_accuracy_value', 'NONE');
#8852 = DIRECTION ( 'NONE',  ( 1.000000000000000000, 0.000000000000000000, 0.000000000000000000 ) ) ;
#8853 = CARTESIAN_POINT ( 'NONE',  ( 197.5308359676227212, 265.1308937032743529, -2.955964573451065558 ) ) ;
#8854 = EDGE_CURVE ( 'NONE', #41771, #52454, #40242, .T. ) ;
#8855 = LINE ( 'NONE', #61548, #61490 ) ;
#8856 = CARTESIAN_POINT ( 'NONE',  ( 22.65899766026757689, 36.58029201028042365, 1.583844403245397769 ) ) ;
#8857 = CARTESIAN_POINT ( 'NONE',  ( 42.09652578138363310, 185.1115022471902023, -5.000000000000041744 ) ) ;
#8858 = CARTESIAN_POINT ( 'NONE',  ( 82.24352131881794037, 42.57645519026166170, 6.897321416369183389 ) ) ;
#8859 = CARTESIAN_POINT ( 'NONE',  ( 74.00349760290353629, 68.31608301643910863, -11.67389511724663009 ) ) ;
#8860 = CARTESIAN_POINT ( 'NONE',  ( 26.48065812185646806, 198.3464784336661637, 1.353441290958777525E-15 ) ) ;
#8861 = CARTESIAN_POINT ( 'NONE',  ( 196.4397788971523653, 275.7035216443041463, 15.37058611766792993 ) ) ;
#8862 = VERTEX_POINT ( 'NONE', #86423 ) ;
#8863 = EDGE_CURVE ( 'NONE', #15769, #40576, #54952, .T. ) ;
#8864 = CARTESIAN_POINT ( 'NONE',  ( 150.0678585083896905, 271.7085566807550663, -11.68900650907589522 ) ) ;
#8865 = CARTESIAN_POINT ( 'NONE',  ( 182.6207078668202257, 260.7553341194429208, -10.79722308874143266 ) ) ;
#8866 = AXIS2_PLACEMENT_3D ( 'NONE', #60202, #29826, #67323 ) ;
#8867 = FACE_OUTER_BOUND ( 'NONE', #57270, .T. ) ;
#8868 = CARTESIAN_POINT ( 'NONE',  ( 80.30021992591166224, 57.12375492286918899, -16.23351995593440478 ) ) ;
#8869 = CARTESIAN_POINT ( 'NONE',  ( 194.3799873100184641, 293.9709813348915191, 15.33105633561973669 ) ) ;
#8870 = CARTESIAN_POINT ( 'NONE',  ( 186.7967035978091133, 279.0542505165097396, -17.82519856243605005 ) ) ;
#8871 = PLANE ( 'NONE',  #1501 ) ;
#8872 = CARTESIAN_POINT ( 'NONE',  ( 194.6782745185928434, 293.4543327343926080, -14.56555309295305634 ) ) ;
#8873 = EDGE_CURVE ( 'NONE', #48040, #28763, #75049, .T. ) ;
#8874 = CARTESIAN_POINT ( 'NONE',  ( 204.3371846825755824, 276.7246095846310823, 14.72513001683937262 ) ) ;
#8875 = CARTESIAN_POINT ( 'NONE',  ( -25.04755574468712354, 23.27320705613571050, 177.5919119679930134 ) ) ;
#8876 = CARTESIAN_POINT ( 'NONE',  ( 68.21143465159309471, 67.67609039233754231, 7.757874407560066743 ) ) ;
#8877 = CARTESIAN_POINT ( 'NONE',  ( 147.7157269441172218, 274.7958511862549926, 8.036290321896261801 ) ) ;
#8878 = CARTESIAN_POINT ( 'NONE',  ( -4.731736819106161285, 24.67387208536691290, 177.5919119679930134 ) ) ;
#8879 = EDGE_CURVE ( 'NONE', #70239, #7803, #28795, .T. ) ;
#8880 = VERTEX_POINT ( 'NONE', #9885 ) ;
#8881 = CARTESIAN_POINT ( 'NONE',  ( 73.88265267960163385, 56.39564808591543965, 16.54767161977011725 ) ) ;
#8882 = CARTESIAN_POINT ( 'NONE',  ( 139.5243837071329267, 251.3615022471902307, -10.00000000000009592 ) ) ;
#8883 = CARTESIAN_POINT ( 'NONE',  ( 104.4229444624559733, 243.3464784336661353, 1.353441290958777327E-15 ) ) ;
#8884 = CARTESIAN_POINT ( 'NONE',  ( 16.34664070491415444, 11.29860640527290983, -2.839279412974138328 ) ) ;
#8885 = CARTESIAN_POINT ( 'NONE',  ( -13.11024591527734628, 27.99999999999999645, 25.00000000000000000 ) ) ;
#8886 = DIRECTION ( 'NONE',  ( -0.5000000000000003331, 0.8660254037844383745, 0.000000000000000000 ) ) ;
#8888 = CARTESIAN_POINT ( 'NONE',  ( 192.1943038168404314, 277.1473907896511264, 17.36549850453357635 ) ) ;
#8887 = CARTESIAN_POINT ( 'NONE',  ( 188.6826127332440421, 272.6057162039079458, 16.71479996418005243 ) ) ;
#8889 = CARTESIAN_POINT ( 'NONE',  ( 150.9989172662526471, 269.1091987373977190, -14.13682882617413306 ) ) ;
#8890 = CARTESIAN_POINT ( 'NONE',  ( 192.4717705703029651, 263.5766868200552722, -4.344887308562926265 ) ) ;
#8891 = CARTESIAN_POINT ( 'NONE',  ( 149.9258927270312824, 271.7122074278049695, -11.62661048439495382 ) ) ;
#8892 = CARTESIAN_POINT ( 'NONE',  ( 115.5463053363034476, 227.5177522451418213, 5.000000000000051514 ) ) ;
#8893 = CARTESIAN_POINT ( 'NONE',  ( 43.87294039959300562, 25.73415679381825427, 1.333680081654574804E-15 ) ) ;
#8894 = CARTESIAN_POINT ( 'NONE',  ( 86.08503991123366461, 47.67438411149250754, 10.86771628747278129 ) ) ;
#8895 = VERTEX_POINT ( 'NONE', #55931 ) ;
#8896 = DIRECTION ( 'NONE',  ( -0.5104483989331149996, -0.8599083858334093389, 0.000000000000000000 ) ) ;
#8897 = DIRECTION ( 'NONE',  ( 0.5000000000000048850, -0.8660254037844358210, 0.000000000000000000 ) ) ;
#8898 = CARTESIAN_POINT ( 'NONE',  ( 199.9473046934823230, 270.1330773050400467, 9.225012586806066395 ) ) ;
#8899 = EDGE_CURVE ( 'NONE', #43165, #59283, #61412, .T. ) ;
#8900 = EDGE_LOOP ( 'NONE', ( #11588, #42042, #57015 ) ) ;
#8901 = CARTESIAN_POINT ( 'NONE',  ( 75.67384099942408682, 65.13299740138256766, -14.43017819244620803 ) ) ;
#8902 = AXIS2_PLACEMENT_3D ( 'NONE', #96080, #18550, #34237 ) ;
#8903 = DIRECTION ( 'NONE',  ( -0.06442261589618514250, -0.9979227057047518334, 0.000000000000000000 ) ) ;
#8904 = CARTESIAN_POINT ( 'NONE',  ( 181.7171926400567656, 295.8235151057616008, -3.827279785929341038 ) ) ;
#8905 = CARTESIAN_POINT ( 'NONE',  ( 168.7096392155106344, 280.2107777274362093, -14.47775774749160682 ) ) ;
#8906 = EDGE_CURVE ( 'NONE', #90508, #24776, #39301, .T. ) ;
#8907 = VERTEX_POINT ( 'NONE', #55433 ) ;
#8908 = CARTESIAN_POINT ( 'NONE',  ( 42.65610334793076674, 64.00004027534475881, -10.00000000000000000 ) ) ;
#8909 = CARTESIAN_POINT ( 'NONE',  ( 38.77491099913230954, 28.10170272979929962, -7.433330006724141015 ) ) ;
#8910 = ORIENTED_EDGE ( 'NONE', *, *, #50873, .T. ) ;
#8911 = CARTESIAN_POINT ( 'NONE',  ( 66.45672647442243886, 68.66481161880344075, 4.836932588431464453 ) ) ;
#8912 = CARTESIAN_POINT ( 'NONE',  ( 171.3171204526115616, 271.4791138034659070, -17.75561031716327420 ) ) ;
#8913 = FACE_OUTER_BOUND ( 'NONE', #3938, .T. ) ;
#8915 = ORIENTED_EDGE ( 'NONE', *, *, #13828, .T. ) ;
#8914 = AXIS2_PLACEMENT_3D ( 'NONE', #13755, #45148, #12789 ) ;
#8917 = EDGE_CURVE ( 'NONE', #441, #5671, #86582, .T. ) ;
#8916 = CARTESIAN_POINT ( 'NONE',  ( 79.42866338260434134, 59.50128377535573776, 16.18467811310512516 ) ) ;
#8918 = CARTESIAN_POINT ( 'NONE',  ( 168.4809247738020019, 252.9187805847961670, 12.05003015331094041 ) ) ;
#8919 = CARTESIAN_POINT ( 'NONE',  ( 61.85273030166814578, 216.5177522451419065, 5.000000000000046185 ) ) ;
#8920 = CARTESIAN_POINT ( 'NONE',  ( 17.46284523756094131, 33.58029201028041655, 1.583844403245363353 ) ) ;
#8921 = ADVANCED_FACE ( 'NONE', ( #35152 ), #58446, .F. ) ;
#8922 = FACE_OUTER_BOUND ( 'NONE', #46045, .T. ) ;
#8923 = CARTESIAN_POINT ( 'NONE',  ( 84.83229447964083647, 50.15339875539878989, -13.73726727158769023 ) ) ;
#8924 = CARTESIAN_POINT ( 'NONE',  ( 155.2922060645262263, 261.6730044072216401, -16.98884022075611355 ) ) ;
#8925 = EDGE_CURVE ( 'NONE', #77173, #50839, #9198, .T. ) ;
#8926 = ORIENTED_EDGE ( 'NONE', *, *, #90160, .T. ) ;
#8927 = EDGE_CURVE ( 'NONE', #85762, #46298, #33659, .T. ) ;
#8928 = EDGE_LOOP ( 'NONE', ( #2060, #63248, #100266, #19855 ) ) ;
#8929 = CARTESIAN_POINT ( 'NONE',  ( 47.84007798744509898, 106.1754093786579318, -10.00000000000000000 ) ) ;
#8930 = ORIENTED_EDGE ( 'NONE', *, *, #75737, .T. ) ;
#8931 = CARTESIAN_POINT ( 'NONE',  ( 81.17822002178407104, 55.59913327053874355, 16.37131925982175318 ) ) ;
#8932 = ORIENTED_EDGE ( 'NONE', *, *, #16727, .F. ) ;
#8933 = CARTESIAN_POINT ( 'NONE',  ( 86.85107213257295200, 45.77346519082802700, -8.718545132792499430 ) ) ;
#8934 = CARTESIAN_POINT ( 'NONE',  ( 79.18986863112007768, 53.11630500884587036, 15.70188359001152634 ) ) ;
#8935 = ORIENTED_EDGE ( 'NONE', *, *, #42370, .T. ) ;
#8936 = CARTESIAN_POINT ( 'NONE',  ( -52.33464467766007289, 32.58262665401804270, -10.00000000000000000 ) ) ;
#8937 = CARTESIAN_POINT ( 'NONE',  ( 206.0013442967545245, 273.8422005809691768, -10.96701481760672792 ) ) ;
#8938 = CARTESIAN_POINT ( 'NONE',  ( 147.8220999374534586, 274.6116077572435188, -7.200782152036906858 ) ) ;
#8939 = DIRECTION ( 'NONE',  ( 0.000000000000000000, 0.000000000000000000, 1.000000000000000000 ) ) ;
#8940 = CARTESIAN_POINT ( 'NONE',  ( 82.57820959284865125, 40.47900230139654099, 0.8910982540740166602 ) ) ;
#8941 = CARTESIAN_POINT ( 'NONE',  ( 171.5081661771196195, 250.9258183615457085, -5.630105313893144725 ) ) ;
#8942 = CARTESIAN_POINT ( 'NONE',  ( 24.36335893204212155, 173.3262482093457777, 3.021315404115420679E-15 ) ) ;
#8943 = CARTESIAN_POINT ( 'NONE',  ( 163.1953264782998758, 283.8895661455310915, -7.125257539458086598 ) ) ;
#8944 = CARTESIAN_POINT ( 'NONE',  ( 131.1078728602114722, 240.3768266524160424, 9.188101187500098632 ) ) ;
#8945 = CARTESIAN_POINT ( 'NONE',  ( 186.2596960937134156, 262.5193429868782005, -9.036614942780335724 ) ) ;
#8946 = CARTESIAN_POINT ( 'NONE',  ( 42.04415689841856363, 29.98920272979930246, 7.433330006724137462 ) ) ;
#8947 = VERTEX_POINT ( 'NONE', #56949 ) ;
#8948 = AXIS2_PLACEMENT_3D ( 'NONE', #51727, #50703, #82670 ) ;
#8950 = ORIENTED_EDGE ( 'NONE', *, *, #90749, .F. ) ;
#8949 = CARTESIAN_POINT ( 'NONE',  ( 30.23324123896446736, 19.58380873178788306, 6.180339887498953466 ) ) ;
#8951 = CARTESIAN_POINT ( 'NONE',  ( 201.2017102119751826, 274.7757513898055777, 13.37679397288412453 ) ) ;
#8952 = CARTESIAN_POINT ( 'NONE',  ( 180.0144465046176663, 255.7853420670775506, 1.312520848803033324 ) ) ;
#8953 = CARTESIAN_POINT ( 'NONE',  ( 11.47080329375824981, 30.07510926853015221, -10.00000000000000000 ) ) ;
#8954 = CARTESIAN_POINT ( 'NONE',  ( 146.8211202654633496, 276.3453554064738569, 4.006087063231699830 ) ) ;
#8955 = CARTESIAN_POINT ( 'NONE',  ( 73.76584831522595209, 68.38082682530665579, 10.99424229391075514 ) ) ;
#8956 = CARTESIAN_POINT ( 'NONE',  ( 163.7584496161371419, 249.5830917119055243, 11.44878023424904256 ) ) ;
#8957 = CARTESIAN_POINT ( 'NONE',  ( 173.6149320458357295, 287.7500054338993891, -9.932635149992773194 ) ) ;
#8958 = CARTESIAN_POINT ( 'NONE',  ( 26.99866280452971878, 37.36126292948897287, 6.180339887498949913 ) ) ;
#8959 = LINE ( 'NONE', #26170, #85362 ) ;
#8960 = EDGE_LOOP ( 'NONE', ( #97277, #84475, #91819, #20163 ) ) ;
#8961 = CARTESIAN_POINT ( 'NONE',  ( 147.8819534105757043, 274.5079385007862811, -9.338341377131436971 ) ) ;
#8962 = CARTESIAN_POINT ( 'NONE',  ( 152.6809499003229860, 273.9044486092186048, 12.24870461040242553 ) ) ;
#8963 = ORIENTED_EDGE ( 'NONE', *, *, #3828, .F. ) ;
#8964 = CARTESIAN_POINT ( 'NONE',  ( 188.7303249615299592, 266.5716613699773347, -11.84797561876724181 ) ) ;
#8965 = CARTESIAN_POINT ( 'NONE',  ( 160.2698612238776263, 279.1124238657968135, 10.65817527884720306 ) ) ;
#8966 = CARTESIAN_POINT ( 'NONE',  ( 152.1679110164900237, 267.0844421682562029, -17.00361552756096728 ) ) ;
#8967 = FACE_OUTER_BOUND ( 'NONE', #14023, .T. ) ;
#8968 = CARTESIAN_POINT ( 'NONE',  ( 69.13511649644314616, 71.04256955909853843, 2.869324681485878275E-06 ) ) ;
#8970 = CARTESIAN_POINT ( 'NONE',  ( 151.5490211047388414, 275.0384667395342149, -8.636128745347312119 ) ) ;
#8969 = CARTESIAN_POINT ( 'NONE',  ( 153.0404527213268864, 270.0709234468621389, 14.04439096357963379 ) ) ;
#8971 = CARTESIAN_POINT ( 'NONE',  ( 201.1060504099706350, 282.3210983108598384, -18.18000168485860257 ) ) ;
#8972 = VERTEX_POINT ( 'NONE', #18478 ) ;
#8973 = CARTESIAN_POINT ( 'NONE',  ( 190.2287563641723978, 301.1611242470490311, -4.521471513871881953 ) ) ;
#8974 = CARTESIAN_POINT ( 'NONE',  ( 164.5084652402306347, 247.3538846981742267, -7.514466451347210807 ) ) ;
#8975 = CARTESIAN_POINT ( 'NONE',  ( 189.9462279001383536, 274.3542461691521339, -15.66465755634487422 ) ) ;
#8976 = CARTESIAN_POINT ( 'NONE',  ( -106.6146531411566798, 123.6868197944956620, 37.50000000000002132 ) ) ;
#8977 = CARTESIAN_POINT ( 'NONE',  ( 44.35815684012577265, 67.96982248125696913, 10.00000000000000000 ) ) ;
#8978 = VECTOR ( 'NONE', #8082, 1000.000000000000114 ) ;
#8979 = CARTESIAN_POINT ( 'NONE',  ( 85.22936087665587479, 47.20283195921787467, 10.81987217476543073 ) ) ;
#8980 = CARTESIAN_POINT ( 'NONE',  ( 13.95435611255089725, 31.55466486950698268, -1.111400068045478839E-16 ) ) ;
#8981 = CARTESIAN_POINT ( 'NONE',  ( 155.4812142336614329, 261.3456326552338282, 18.45193178807985745 ) ) ;
#8982 = CARTESIAN_POINT ( 'NONE',  ( 69.12254913399198131, 70.55341387760749683, 0.02902045130465960923 ) ) ;
#8983 = CARTESIAN_POINT ( 'NONE',  ( -7.997457622663985966, 160.0643266524160140, -9.188101187500093303 ) ) ;
#8984 = CARTESIAN_POINT ( 'NONE',  ( 95.76303752037657091, 226.0958772461660260, -9.188101187500095079 ) ) ;
#8985 = CARTESIAN_POINT ( 'NONE',  ( 67.69237348538018750, 66.82088825431439716, 8.559571887000263501 ) ) ;
#8986 = CARTESIAN_POINT ( 'NONE',  ( 192.5143468344189728, 297.2023654272867361, -12.06830393602581530 ) ) ;
#8987 = CARTESIAN_POINT ( 'NONE',  ( 40.60966550219798421, 208.6868197944957615, 17.47570218321536117 ) ) ;
#8988 = EDGE_CURVE ( 'NONE', #65735, #30076, #3774, .T. ) ;
#8989 = CARTESIAN_POINT ( 'NONE',  ( 202.8549823380854491, 279.2918593523859272, -16.39745931995414807 ) ) ;
#8990 = CYLINDRICAL_SURFACE ( 'NONE', #65243, 10.00000000000010658 ) ;
#8991 = FILL_AREA_STYLE_COLOUR ( '', #25521 ) ;
#8992 = CARTESIAN_POINT ( 'NONE',  ( 78.06933962600676580, 61.94553563989994416, 15.69501238203493187 ) ) ;
#8994 = CARTESIAN_POINT ( 'NONE',  ( 75.96907744678482288, 51.45858532960258458, 16.17359642618427173 ) ) ;
#8993 = CARTESIAN_POINT ( 'NONE',  ( -0.01211276271276783001, 139.0458036431182620, -22.49999999999983658 ) ) ;
#8995 = CARTESIAN_POINT ( 'NONE',  ( 161.8938357633344651, 250.2386463561303458, 14.09469623995626719 ) ) ;
#8996 = EDGE_CURVE ( 'NONE', #5449, #7185, #96377, .T. ) ;
#8997 = CARTESIAN_POINT ( 'NONE',  ( 166.1003953386458249, 249.2057617637232738, -9.336859914837196683 ) ) ;
#8998 = CARTESIAN_POINT ( 'NONE',  ( 204.8391661702352735, 275.8551521435456380, -13.37474513291600431 ) ) ;
#8999 = CARTESIAN_POINT ( 'NONE',  ( 157.1606030646430554, 258.4368458743103361, 17.96998724893680688 ) ) ;
#9000 = B_SPLINE_CURVE_WITH_KNOTS ( 'NONE', 3,
 ( #74437, #81065, #73423, #19729 ),
 .UNSPECIFIED., .F., .F.,
 ( 4, 4 ),
 ( 0.03993246080742687137, 0.04837343171532907521 ),
 .UNSPECIFIED. ) ;
#9001 = CARTESIAN_POINT ( 'NONE',  ( 169.4078252042709778, 250.4262823970964007, 8.341134405704034194 ) ) ;
#9002 = ADVANCED_FACE ( 'NONE', ( #62292 ), #59933, .F. ) ;
#9003 = CARTESIAN_POINT ( 'NONE',  ( 32.78649236710315762, 198.9244531367911293, -4.594050593750046652 ) ) ;
#9004 = CARTESIAN_POINT ( 'NONE',  ( 59.20026718252854891, 214.1744531367911293, 4.594050593750047540 ) ) ;
#9005 = CARTESIAN_POINT ( 'NONE',  ( 65.93257831369518840, 197.3262482093457777, 3.021315404115420679E-15 ) ) ;
#9007 = CARTESIAN_POINT ( 'NONE',  ( 88.54812304393657030, 43.90120638611161752, -0.3063217976418581845 ) ) ;
#9006 = B_SPLINE_CURVE_WITH_KNOTS ( 'NONE', 3,
 ( #30977, #84235, #45666, #76590, #7175, #30485, #38062, #13316, #44177, #22877, #84724, #46159, #77080, #7684, #38574, #94, #8685, #62874, #39554, #63882, #8189, #2603, #85226, #56270, #25382, #70478, #40566, #87267, #79631, #584, #31469, #40062, #79129, #55259, #46678, #93831, #1092, #61864, #93317, #62360, #54255, #71004, #24386, #86241, #78094, #23871 ),
 .UNSPECIFIED., .F., .F.,
 ( 4, 2, 2, 2, 2, 2, 2, 2, 2, 2, 2, 2, 2, 2, 2, 2, 2, 2, 2, 2, 2, 2, 4 ),
 ( 0.0008836965591771303846, 0.001081134423596614253, 0.001179853355806375053, 0.001278572288016136069, 0.001476010152435624492, 0.001673448016855112915, 0.002068323745694089326, 0.002463199474533066605, 0.003252950932210945702, 0.004042702389888824799, 0.004832453847566703896, 0.005227329576405679440, 0.005424767440825208412, 0.005523486373034932999, 0.005572845839139830421, 0.005622205305244727842, 0.005671564771349624397, 0.005720924237454521818, 0.005819643169664226456, 0.006017081034083765836, 0.006411956762922983374, 0.006806832491762201780, 0.007201708220601420185 ),
 .UNSPECIFIED. ) ;
#9008 = CARTESIAN_POINT ( 'NONE',  ( 98.74902094561561228, 234.4865022471903160, 10.00000000000009415 ) ) ;
#9010 = CARTESIAN_POINT ( 'NONE',  ( 77.69386982215107196, 49.37577063231137942, 15.30935726915745931 ) ) ;
#9009 = CARTESIAN_POINT ( 'NONE',  ( 71.78553924664423391, 72.10835861452468976, -3.632824164035485470 ) ) ;
#9011 = CARTESIAN_POINT ( 'NONE',  ( 196.5129603538013612, 268.9685797610468398, -10.52983625242027976 ) ) ;
#9012 = AXIS2_PLACEMENT_3D ( 'NONE', #14594, #61172, #31760 ) ;
#9013 = CARTESIAN_POINT ( 'NONE',  ( 30.02984208470827454, 19.19860640527293327, 2.839279412974134775 ) ) ;
#9014 = CARTESIAN_POINT ( 'NONE',  ( 150.9115585710837877, 269.2605084359132093, -15.80434701481532578 ) ) ;
#9015 = CARTESIAN_POINT ( 'NONE',  ( 196.2421909983451940, 290.7455499326673021, -17.31908925000307065 ) ) ;
#9016 = CARTESIAN_POINT ( 'NONE',  ( 13.89351337401799391, 10.94754757982087945, 5.678558825948272215 ) ) ;
#9017 = CARTESIAN_POINT ( 'NONE',  ( 66.23672358827711548, 218.2369531367911293, -4.594050593750048428 ) ) ;
#9018 = DIRECTION ( 'NONE',  ( 0.5000000000000014433, -0.8660254037844378194, 0.000000000000000000 ) ) ;
#9019 = CARTESIAN_POINT ( 'NONE',  ( 155.0453531195792038, 262.1005662498678817, -18.46987289964740953 ) ) ;
#9020 = CARTESIAN_POINT ( 'NONE',  ( 198.6755293322981117, 286.5308843062557571, 17.86676876308990103 ) ) ;
#9021 = CARTESIAN_POINT ( 'NONE',  ( 69.64550182367553077, 63.14169069997384298, -13.61487806674371370 ) ) ;
#9022 = CARTESIAN_POINT ( 'NONE',  ( 153.9009929122451013, 264.0826562711307020, 18.02690668714909705 ) ) ;
#9023 = CIRCLE ( 'NONE', #63983, 70.00000000000001421 ) ;
#9024 = CARTESIAN_POINT ( 'NONE',  ( 77.99503874021337424, 55.85935939106580150, -16.14935493097549113 ) ) ;
#9025 = CARTESIAN_POINT ( 'NONE',  ( 87.62574851936349773, 45.15471363961356133, -6.154635046463404535 ) ) ;
#9026 = CARTESIAN_POINT ( 'NONE',  ( 113.4714528099511455, 222.9865022471901455, 1.119607411625061291E-15 ) ) ;
#9027 = CARTESIAN_POINT ( 'NONE',  ( 161.6256441450323678, 250.7031678651938762, 14.48526717260977037 ) ) ;
#9028 = EDGE_CURVE ( 'NONE', #15032, #19489, #51346, .T. ) ;
#9029 = CARTESIAN_POINT ( 'NONE',  ( 206.9878665138179770, 272.1334939782196329, 6.566295309274049252 ) ) ;
#9030 = ORIENTED_EDGE ( 'NONE', *, *, #9370, .F. ) ;
#9031 = CARTESIAN_POINT ( 'NONE',  ( 77.25232559036803082, 49.49244633483773725, 14.92639236986914142 ) ) ;
#9032 = CARTESIAN_POINT ( 'NONE',  ( 188.0748052926907405, 273.3533922738282058, 15.64113677151411608 ) ) ;
#9033 = ORIENTED_EDGE ( 'NONE', *, *, #18204, .T. ) ;
#9034 = CARTESIAN_POINT ( 'NONE',  ( 206.8659638600981623, 272.3446355680395641, -10.26115277030573125 ) ) ;
#9035 = CARTESIAN_POINT ( 'NONE',  ( 194.0754204476036762, 293.3896858871647169, 14.78846558403258094 ) ) ;
#9036 = CARTESIAN_POINT ( 'NONE',  ( 72.23451590016303214, 68.82702540631112242, -9.493575677105072330 ) ) ;
#9037 = ORIENTED_EDGE ( 'NONE', *, *, #13828, .F. ) ;
#9039 = EDGE_CURVE ( 'NONE', #56147, #54118, #4773, .T. ) ;
#9038 = DIRECTION ( 'NONE',  ( -1.000000000000000000, 0.000000000000000000, 0.000000000000000000 ) ) ;
#9040 = ORIENTED_EDGE ( 'NONE', *, *, #14539, .F. ) ;
#9042 = EDGE_CURVE ( 'NONE', #44048, #47944, #16362, .T. ) ;
#9041 = CARTESIAN_POINT ( 'NONE',  ( 79.40193053424152936, 46.39394473022984755, -12.75601862751888760 ) ) ;
#9043 = CARTESIAN_POINT ( 'NONE',  ( 167.4088369852190681, 247.5279131301515179, 3.600464852340231836 ) ) ;
#9044 = CARTESIAN_POINT ( 'NONE',  ( 148.6594212568597868, 273.7599597785030596, 8.554715638618541007 ) ) ;
#9045 = ORIENTED_EDGE ( 'NONE', *, *, #14029, .T. ) ;
#9046 = CARTESIAN_POINT ( 'NONE',  ( 26.65055534615017763, 21.10170272979927830, -7.433330006724141015 ) ) ;
#9047 = VECTOR ( 'NONE', #11022, 1000.000000000000000 ) ;
#9048 = CARTESIAN_POINT ( 'NONE',  ( -12.63042782814763143, 41.81209092917440273, 59.99999999999999289 ) ) ;
#9049 = CARTESIAN_POINT ( 'NONE',  ( 75.28959155135937920, 66.52156427834158592, -13.12148920440117195 ) ) ;
#9050 = CARTESIAN_POINT ( 'NONE',  ( 81.92605646210873260, 48.64405669687059941, -13.31366699692007316 ) ) ;
#9051 = EDGE_CURVE ( 'NONE', #69981, #63769, #99813, .T. ) ;
#9052 = EDGE_CURVE ( 'NONE', #56021, #57780, #34489, .T. ) ;
#9053 = EDGE_LOOP ( 'NONE', ( #21732, #49167 ) ) ;
#9054 = CARTESIAN_POINT ( 'NONE',  ( 166.9369206129118197, 276.4285397603561591, 15.88976881163156563 ) ) ;
#9055 = CARTESIAN_POINT ( 'NONE',  ( -0.5967702463563150372, 158.9155109091896350, 2.679491924311254714 ) ) ;
#9056 = EDGE_LOOP ( 'NONE', ( #35442, #73136, #28121, #69613 ) ) ;
#9057 = CARTESIAN_POINT ( 'NONE',  ( 170.8439975286642607, 284.8586297143663728, 11.08717077125447936 ) ) ;
#9058 =( BOUNDED_CURVE ( )  B_SPLINE_CURVE ( 1, ( #72214, #32686 ),
 .UNSPECIFIED., .F., .F. ) 
 B_SPLINE_CURVE_WITH_KNOTS ( ( 2, 2 ),
 ( 0.000000000000000000, 0.001312499995903266495 ),
 .UNSPECIFIED. ) 
 CURVE ( )  GEOMETRIC_REPRESENTATION_ITEM ( )  RATIONAL_B_SPLINE_CURVE ( ( 0.9368410486966849415, 0.9368410486966849415 ) ) 
 REPRESENTATION_ITEM ( '' )  );
#9060 = CARTESIAN_POINT ( 'NONE',  ( 68.19908846357228072, 65.66916044190364232, -10.28971576526838483 ) ) ;
#9059 = CARTESIAN_POINT ( 'NONE',  ( 163.2652593887152364, 283.8092165855917983, -2.903001196033301312 ) ) ;
#9061 = DIRECTION ( 'NONE',  ( -0.000000000000000000, -0.000000000000000000, 1.000000000000000000 ) ) ;
#9062 = CARTESIAN_POINT ( 'NONE',  ( 194.3799873100184641, 293.9709813348915191, 15.33105633561973669 ) ) ;
#9063 = CARTESIAN_POINT ( 'NONE',  ( 185.6579485543611270, 292.7763231470134428, -10.71670576288961207 ) ) ;
#9064 = CARTESIAN_POINT ( 'NONE',  ( 157.4893260420801653, 257.8674809757739013, -18.30842125257398223 ) ) ;
#9065 = CARTESIAN_POINT ( 'NONE',  ( 164.7389676833716976, 245.3107333163898716, 5.284562706098457241 ) ) ;
#9066 = CARTESIAN_POINT ( 'NONE',  ( 203.4636416406178512, 268.6914787556956981, 2.471263131328804707 ) ) ;
#9067 = CARTESIAN_POINT ( 'NONE',  ( 79.12311323331778112, 59.82187722400571062, 16.49858871944914185 ) ) ;
#9068 = CARTESIAN_POINT ( 'NONE',  ( 93.16496130902324069, 224.5958772461660260, -9.188101187500095079 ) ) ;
#9070 = ORIENTED_EDGE ( 'NONE', *, *, #32666, .F. ) ;
#9069 = B_SPLINE_CURVE_WITH_KNOTS ( 'NONE', 3,
 ( #23829, #32446, #2053, #70438 ),
 .UNSPECIFIED., .F., .F.,
 ( 4, 4 ),
 ( 0.01705236508060226780, 0.02596178682224619186 ),
 .UNSPECIFIED. ) ;
#9071 = CARTESIAN_POINT ( 'NONE',  ( 150.8757650385446993, 269.3225046528533539, 14.31332712971473953 ) ) ;
#9072 = DIRECTION ( 'NONE',  ( 0.000000000000000000, 0.000000000000000000, -1.000000000000000000 ) ) ;
#9073 = CARTESIAN_POINT ( 'NONE',  ( 78.04817985968655591, 62.07294584189650521, -16.01854286150912898 ) ) ;
#9074 = ORIENTED_EDGE ( 'NONE', *, *, #59634, .F. ) ;
#9075 = CARTESIAN_POINT ( 'NONE',  ( 157.0759360137626572, 258.5834935081620642, -16.84194680719508597 ) ) ;
#9076 = VERTEX_POINT ( 'NONE', #87692 ) ;
#9077 = ORIENTED_EDGE ( 'NONE', *, *, #57001, .F. ) ;
#9078 = DIRECTION ( 'NONE',  ( 0.8660254037844384856, 0.5000000000000002220, 0.000000000000000000 ) ) ;
#9079 = CARTESIAN_POINT ( 'NONE',  ( -19.65312891409015350, 9.999999999999801048, 54.99999999999999289 ) ) ;
#9080 = CARTESIAN_POINT ( 'NONE',  ( 67.79725476218452229, 65.71048819351143777, 10.00598338191753101 ) ) ;
#9081 = CARTESIAN_POINT ( 'NONE',  ( 82.42161199636267099, 47.86338641862497667, -12.65011761261475520 ) ) ;
#9082 = CARTESIAN_POINT ( 'NONE',  ( 207.8040920112677270, 270.7197499462034784, 3.100718407159808176 ) ) ;
#9083 = CARTESIAN_POINT ( 'NONE',  ( 82.14994038281616895, 227.4244531367911293, -4.594050593750046652 ) ) ;
#9084 = ORIENTED_EDGE ( 'NONE', *, *, #46651, .T. ) ;
#9085 = ORIENTED_EDGE ( 'NONE', *, *, #51623, .F. ) ;
#9086 = CARTESIAN_POINT ( 'NONE',  ( 161.8723090575478807, 250.2759317042724376, -14.13132104777860221 ) ) ;
#9087 = ORIENTED_EDGE ( 'NONE', *, *, #4586, .T. ) ;
#9088 = EDGE_CURVE ( 'NONE', #37455, #99166, #1534, .T. ) ;
#9089 = CARTESIAN_POINT ( 'NONE',  ( 75.89533479853247400, 64.71926289652466835, -14.30003966153671691 ) ) ;
#9090 = VECTOR ( 'NONE', #73908, 1000.000000000000000 ) ;
#9091 = LINE ( 'NONE', #22794, #28981 ) ;
#9092 = CARTESIAN_POINT ( 'NONE',  ( 183.2572639141025093, 259.6883485553630635, -10.14808137897176898 ) ) ;
#9093 = CARTESIAN_POINT ( 'NONE',  ( 87.81385227123767834, 44.76907565500617636, 4.981894665149344981 ) ) ;
#9094 = EDGE_LOOP ( 'NONE', ( #70749, #65524, #19674, #15290 ) ) ;
#9095 = CARTESIAN_POINT ( 'NONE',  ( 81.80357686921180971, 43.66383732902560411, -8.936250712220841663 ) ) ;
#9096 = DIRECTION ( 'NONE',  ( 0.000000000000000000, 0.000000000000000000, 1.000000000000000000 ) ) ;
#9097 = CARTESIAN_POINT ( 'NONE',  ( -75.14068524134967220, 52.46521621197197760, 10.00000000000000000 ) ) ;
#9098 = CARTESIAN_POINT ( 'NONE',  ( 147.8132215089878798, 275.1406199707106452, -4.592798751325347872 ) ) ;
#9099 = CARTESIAN_POINT ( 'NONE',  ( 175.5358861210679322, 284.6783754363922867, 14.06838304944039564 ) ) ;
#9100 = VECTOR ( 'NONE', #96967, 1000.000000000000114 ) ;
#9101 = FACE_OUTER_BOUND ( 'NONE', #30344, .T. ) ;
#9102 = DIRECTION ( 'NONE',  ( 0.9133924323370933296, -0.1624253398589802222, 0.3732723851573050422 ) ) ;
#9103 = ORIENTED_EDGE ( 'NONE', *, *, #37140, .T. ) ;
#9104 = CARTESIAN_POINT ( 'NONE',  ( 48.17894221477870786, 74.75545800895066861, 10.00000000000000000 ) ) ;
#9105 = CARTESIAN_POINT ( 'NONE',  ( 200.9111546617170916, 282.6586676490145464, 17.66063511622358106 ) ) ;
#9106 = CARTESIAN_POINT ( 'NONE',  ( 83.66159036850885400, 42.08077760457628358, 3.673192525297190869 ) ) ;
#9107 = CARTESIAN_POINT ( 'NONE',  ( 171.4520973777158304, 251.1120003641540848, 7.352569034034808659 ) ) ;
#9108 = CARTESIAN_POINT ( 'NONE',  ( 198.5250552234815018, 266.2012769527108276, 1.136986010074936937 ) ) ;
#9109 = CARTESIAN_POINT ( 'NONE',  ( 156.9036059482025678, 272.7077526247311425, 14.56380410095424871 ) ) ;
#9110 = ORIENTED_EDGE ( 'NONE', *, *, #2786, .F. ) ;
#9111 = EDGE_CURVE ( 'NONE', #483, #84750, #35752, .T. ) ;
#9112 = CARTESIAN_POINT ( 'NONE',  ( 202.8499463704053198, 279.3005819042728604, 17.04674939340617001 ) ) ;
#9113 = AXIS2_PLACEMENT_3D ( 'NONE', #79901, #33784, #57043 ) ;
#9114 = CARTESIAN_POINT ( 'NONE',  ( 207.6209998424140792, 271.0368748851258260, 6.610167240481342965 ) ) ;
#9115 = CARTESIAN_POINT ( 'NONE',  ( 73.60037652456395563, 55.60548681284689820, 16.10385087386687886 ) ) ;
#9116 = CARTESIAN_POINT ( 'NONE',  ( 80.01979875032591849, 57.54866692369599690, 16.59896302490740538 ) ) ;
#9117 = EDGE_CURVE ( 'NONE', #17646, #82741, #95005, .T. ) ;
#9118 = CARTESIAN_POINT ( 'NONE',  ( 28.06847263831340555, 31.90829794293882316, 10.00000000000000355 ) ) ;
#9119 = CARTESIAN_POINT ( 'NONE',  ( 172.1288327371077003, 274.9361716132315792, 16.40855730066342133 ) ) ;
#9120 = CARTESIAN_POINT ( 'NONE',  ( 166.5660939988957239, 286.4811537094821006, -3.256692973398967794 ) ) ;
#9121 = DIRECTION ( 'NONE',  ( 1.000000000000000000, 0.000000000000000000, 0.000000000000000000 ) ) ;
#9122 = VECTOR ( 'NONE', #4989, 1000.000000000000227 ) ;
#9123 = DIRECTION ( 'NONE',  ( -0.8917477921037005872, -0.4525327339300165286, 0.000000000000000000 ) ) ;
#9124 = EDGE_CURVE ( 'NONE', #24743, #49291, #42008, .T. ) ;
#9125 = CARTESIAN_POINT ( 'NONE',  ( 161.6755750489535046, 250.6166850027345276, -13.01404233079112061 ) ) ;
#9126 = EDGE_CURVE ( 'NONE', #90599, #80986, #72009, .T. ) ;
#9127 = CARTESIAN_POINT ( 'NONE',  ( 5.669592554750444435, 164.8923013555410080, 4.594050593750050204 ) ) ;
#9128 = DIRECTION ( 'NONE',  ( -0.6270036013472584102, -0.3336146661356741983, 0.7039657224870761176 ) ) ;
#9129 = ORIENTED_EDGE ( 'NONE', *, *, #97429, .F. ) ;
#9130 = CARTESIAN_POINT ( 'NONE',  ( 160.4993420583414263, 253.2460122621210132, -14.64862292197809879 ) ) ;
#9131 = FACE_BOUND ( 'NONE', #61972, .T. ) ;
#9132 = CARTESIAN_POINT ( 'NONE',  ( 81.60968120880437482, 41.61943387927043148, 5.647669398712323208 ) ) ;
#9133 = CARTESIAN_POINT ( 'NONE',  ( 25.07406103223677007, 173.0327760586659736, 1.948934522072302763E-15 ) ) ;
#9134 = CARTESIAN_POINT ( 'NONE',  ( 181.7815785431583038, 276.1505370498239813, -17.81783396216490445 ) ) ;
#9135 = CARTESIAN_POINT ( 'NONE',  ( 37.75007554933399234, 22.76426979415092333, 3.090169943749476733 ) ) ;
#9136 = CARTESIAN_POINT ( 'NONE',  ( 82.01156895356272969, 41.52670969893105735, -4.853141658140002868 ) ) ;
#9137 = CARTESIAN_POINT ( 'NONE',  ( 146.6647111637776106, 276.6162639173599587, -0.6373001129109082674 ) ) ;
#9138 = CARTESIAN_POINT ( 'NONE',  ( 80.96506752577832344, 55.91141337780396015, 16.08528190432092231 ) ) ;
#9139 = CARTESIAN_POINT ( 'NONE',  ( 167.8099530253072089, 271.3928698661641761, -17.53051755021046532 ) ) ;
#9140 = CARTESIAN_POINT ( 'NONE',  ( 189.4796331244937164, 297.8479079567700296, -7.877982910326568167 ) ) ;
#9141 = CARTESIAN_POINT ( 'NONE',  ( 189.2845499996045930, 259.5340837477176024, -0.8149847707460528001 ) ) ;
#9142 = CARTESIAN_POINT ( 'NONE',  ( 58.11799575139567509, 214.3615022471903160, 5.000000000000046185 ) ) ;
#9143 = CARTESIAN_POINT ( 'NONE',  ( 71.00261025973313167, 66.65379046055741696, -10.97453163846388513 ) ) ;
#9144 = DIRECTION ( 'NONE',  ( -0.000000000000000000, -0.000000000000000000, -1.000000000000000000 ) ) ;
#9145 = EDGE_CURVE ( 'NONE', #86118, #1456, #9663, .T. ) ;
#9146 = CARTESIAN_POINT ( 'NONE',  ( 172.0630936339023265, 254.4764114392720273, 11.54978638049990103 ) ) ;
#9147 = CARTESIAN_POINT ( 'NONE',  ( 30.27021345494340565, 176.0327760586659736, 1.948934522072303157E-15 ) ) ;
#9148 = PLANE ( 'NONE',  #94163 ) ;
#9149 = CARTESIAN_POINT ( 'NONE',  ( 203.3700558458376122, 269.3551942510547406, -5.938188790449932419 ) ) ;
#9150 = CARTESIAN_POINT ( 'NONE',  ( 151.2964716097791325, 268.5938194963972592, -15.66250187539618111 ) ) ;
#9151 = CARTESIAN_POINT ( 'NONE',  ( 198.2505066714982149, 285.2670451491296149, 0.000000000000000000 ) ) ;
#9152 = ORIENTED_EDGE ( 'NONE', *, *, #45013, .T. ) ;
#9153 = CARTESIAN_POINT ( 'NONE',  ( 168.0910689791846266, 281.7684205924134062, -11.46037133588631818 ) ) ;
#9154 = CARTESIAN_POINT ( 'NONE',  ( 163.0740133991062351, 281.1655447304752897, -10.28074664187252196 ) ) ;
#9155 = DIRECTION ( 'NONE',  ( -0.8660254037844387076, -0.4999999999999998890, -0.000000000000000000 ) ) ;
#9156 = CARTESIAN_POINT ( 'NONE',  ( 28.52090319329063206, 17.26216523072495690, -2.296566073217252530E-15 ) ) ;
#9157 = CARTESIAN_POINT ( 'NONE',  ( 202.4017613376760494, 280.0768611521521620, 15.73960524502980540 ) ) ;
#9158 = CARTESIAN_POINT ( 'NONE',  ( 196.7130436017243653, 289.9300093007386749, -16.33278734947153765 ) ) ;
#9159 = CARTESIAN_POINT ( 'NONE',  ( 186.5747885479362935, 268.5526011410998990, -14.20271085587731541 ) ) ;
#9160 = ORIENTED_EDGE ( 'NONE', *, *, #57691, .F. ) ;
#9161 = CARTESIAN_POINT ( 'NONE',  ( 42.07167428219069905, 29.45404122711137163, -8.090169943749478065 ) ) ;
#9162 = AXIS2_PLACEMENT_3D ( 'NONE', #95743, #57171, #49580 ) ;
#9163 = CARTESIAN_POINT ( 'NONE',  ( 9.471979480098337234, 23.65586893147754566, -7.433330006724137462 ) ) ;
#9164 = DIRECTION ( 'NONE',  ( 0.8660254037844384856, 0.5000000000000002220, 3.252519625699449945E-16 ) ) ;
#9165 = CARTESIAN_POINT ( 'NONE',  ( 73.29163036545841692, 59.81749283019145480, -15.42714291014837613 ) ) ;
#9166 = CARTESIAN_POINT ( 'NONE',  ( 87.83435352734132096, 44.15087646923105780, 2.758404312169200345 ) ) ;
#9167 = ORIENTED_EDGE ( 'NONE', *, *, #2150, .F. ) ;
#9168 = CARTESIAN_POINT ( 'NONE',  ( 23.81978131880161698, 177.8927522451418213, -10.00000000000009237 ) ) ;
#9169 = CARTESIAN_POINT ( 'NONE',  ( 72.48661302258760486, 71.52526770760661634, -5.337229783571229014 ) ) ;
#9170 = CARTESIAN_POINT ( 'NONE',  ( 190.8604783348975502, 300.0669496974951471, 7.597731640149610222 ) ) ;
#9171 = CARTESIAN_POINT ( 'NONE',  ( 168.7096392155106344, 280.2107777274362093, -14.47775774749160682 ) ) ;
#9172 = B_SPLINE_CURVE_WITH_KNOTS ( 'NONE', 3,
 ( #55142, #78479, #86621, #79509, #32854, #40446, #94695, #17155, #48053, #71381, #25257, #56140, #87138, #10071, #71880, #27764 ),
 .UNSPECIFIED., .F., .F.,
 ( 4, 1, 2, 2, 2, 1, 2, 2, 4 ),
 ( 0.000000000000000000, 0.1249999999999995282, 0.1875000000000013878, 0.2500000000000032752, 0.5000000000000046629, 0.6250000000000072164, 0.6875000000000065503, 0.7500000000000057732, 1.000000000000000000 ),
 .UNSPECIFIED. ) ;
#9173 = VERTEX_POINT ( 'NONE', #42488 ) ;
#9174 = ORIENTED_EDGE ( 'NONE', *, *, #76170, .T. ) ;
#9176 = CARTESIAN_POINT ( 'NONE',  ( 82.02953226466719627, 42.27987555721853141, -6.567708260245657570 ) ) ;
#9175 = DIRECTION ( 'NONE',  ( -0.9724945078367508433, -0.2329258084183800648, 0.000000000000000000 ) ) ;
#9177 = ORIENTED_EDGE ( 'NONE', *, *, #72191, .T. ) ;
#9178 = CARTESIAN_POINT ( 'NONE',  ( 66.12615603930825614, 68.50702530225942155, -2.650021266571979783 ) ) ;
#9179 = CARTESIAN_POINT ( 'NONE',  ( 71.96596176604222705, 72.21842720279319394, -3.609932465874673646 ) ) ;
#9180 = CARTESIAN_POINT ( 'NONE',  ( 80.02165461388095480, 57.57226732806287828, 16.59957571444259727 ) ) ;
#9181 = DIRECTION ( 'NONE',  ( 0.000000000000000000, 0.000000000000000000, 1.000000000000000000 ) ) ;
#9182 = CARTESIAN_POINT ( 'NONE',  ( 147.6947327179224487, 274.8322142526899370, 9.090449717876689206 ) ) ;
#9183 = EDGE_CURVE ( 'NONE', #3380, #8880, #89181, .T. ) ;
#9184 = CARTESIAN_POINT ( 'NONE',  ( 183.6532122277409655, 289.8064359948238007, -13.38300012774528369 ) ) ;
#9185 = ORIENTED_EDGE ( 'NONE', *, *, #44566, .T. ) ;
#9186 = CIRCLE ( 'NONE', #73915, 9.000000000000007105 ) ;
#9187 = CARTESIAN_POINT ( 'NONE',  ( 45.98627256186106393, 118.1229683434676900, 10.00000000000000000 ) ) ;
#9188 = ORIENTED_EDGE ( 'NONE', *, *, #12031, .F. ) ;
#9189 = CARTESIAN_POINT ( 'NONE',  ( 27.40352323984253502, 36.79752408145593279, -5.678558825948271327 ) ) ;
#9190 = CARTESIAN_POINT ( 'NONE',  ( 198.2489255580726422, 287.2697837179150042, 18.53597557040773225 ) ) ;
#9191 = CARTESIAN_POINT ( 'NONE',  ( 78.60735446189906384, 47.91558663933584228, -14.46554740014634888 ) ) ;
#9192 = CARTESIAN_POINT ( 'NONE',  ( 50.97302584657637681, 209.4244531367911577, -4.594050593750046652 ) ) ;
#9193 = CARTESIAN_POINT ( 'NONE',  ( 74.13497556468038852, 68.62018799133311120, 10.97049235834077408 ) ) ;
#9194 = CARTESIAN_POINT ( 'NONE',  ( 35.21268636174862365, 20.73415679381824006, 1.333680081654574804E-15 ) ) ;
#9195 = CARTESIAN_POINT ( 'NONE',  ( 197.9679655381963244, 287.7564207472362341, 17.61949439995294497 ) ) ;
#9198 = B_SPLINE_CURVE_WITH_KNOTS ( 'NONE', 3,
 ( #3290, #19971, #72183, #26573, #81798, #2794, #95009, #64572, #25569, #56458 ),
 .UNSPECIFIED., .F., .F.,
 ( 4, 2, 2, 2, 4 ),
 ( 0.000000000000000000, 0.2500000000000000000, 0.5000000000000000000, 0.7500000000000000000, 1.000000000000000000 ),
 .UNSPECIFIED. ) ;
#9197 = AXIS2_PLACEMENT_3D ( 'NONE', #82028, #98200, #67273 ) ;
#9196 = CARTESIAN_POINT ( 'NONE',  ( 205.0859877718122561, 268.9368413191317586, -3.038556538008958974 ) ) ;
#9199 = EDGE_LOOP ( 'NONE', ( #6033, #44341, #80743, #37000 ) ) ;
#9200 = DIRECTION ( 'NONE',  ( -0.000000000000000000, -0.000000000000000000, 1.000000000000000000 ) ) ;
#9201 = CARTESIAN_POINT ( 'NONE',  ( 86.12405100256837898, 43.33680938231972135, -3.166424999297555942 ) ) ;
#9202 = CARTESIAN_POINT ( 'NONE',  ( 190.3625087333586521, 300.9294583479858147, -4.271886578030237303 ) ) ;
#9203 = CARTESIAN_POINT ( 'NONE',  ( 77.31487416622417186, 50.45086608835270425, 15.74699347680645012 ) ) ;
#9204 = VERTEX_POINT ( 'NONE', #59170 ) ;
#9205 = CARTESIAN_POINT ( 'NONE',  ( 175.4707219612219831, 261.2647045857924581, -14.43885454850885708 ) ) ;
#9206 = CARTESIAN_POINT ( 'NONE',  ( 139.5965524907817041, 244.7365022471901739, -10.00000000000009237 ) ) ;
#9207 = CARTESIAN_POINT ( 'NONE',  ( 161.6755750489535046, 250.6166850027345276, -13.01404233079112061 ) ) ;
#9208 = CARTESIAN_POINT ( 'NONE',  ( 147.1125781744767949, 275.8405354997948962, -5.216646253929903665 ) ) ;
#9209 = CARTESIAN_POINT ( 'NONE',  ( 190.8187029736043883, 300.1393067457597681, 3.941064102378585954 ) ) ;
#9210 = CARTESIAN_POINT ( 'NONE',  ( 177.6686998861319466, 269.6967534512956490, 16.10014392654021265 ) ) ;
#9211 = CARTESIAN_POINT ( 'NONE',  ( 205.8030308266901898, 274.1856895869457844, 10.55961490432110317 ) ) ;
#9212 = CARTESIAN_POINT ( 'NONE',  ( 67.21548817476096360, 66.87675868597760598, 8.996481726798670309 ) ) ;
#9213 = CARTESIAN_POINT ( 'NONE',  ( 154.8376827341003548, 264.3318404447347802, -17.39305756353265409 ) ) ;
#9214 = DIRECTION ( 'NONE',  ( -0.03487823687206607903, 0.06041087834084090530, 0.9975640502598237536 ) ) ;
#9215 = CARTESIAN_POINT ( 'NONE',  ( 107.0210206738092609, 244.8464784336661353, 1.353441290958777327E-15 ) ) ;
#9216 = EDGE_LOOP ( 'NONE', ( #93305, #455, #67911, #18178 ) ) ;
#9217 = CARTESIAN_POINT ( 'NONE',  ( 190.1358581116424489, 301.3220287403654538, -4.546659160351699036 ) ) ;
#9218 = DIRECTION ( 'NONE',  ( 0.000000000000000000, 0.000000000000000000, 1.000000000000000000 ) ) ;
#9219 = CARTESIAN_POINT ( 'NONE',  ( 84.42663183290281381, 49.91580812419739033, -13.73522929182741947 ) ) ;
#9220 = CARTESIAN_POINT ( 'NONE',  ( 163.7707306762541748, 246.9877690064858484, 7.021959502997312086 ) ) ;
#9221 = CARTESIAN_POINT ( 'NONE',  ( -22.42236680055709641, 157.8615022471902591, 0.000000000000000000 ) ) ;
#9222 = CARTESIAN_POINT ( 'NONE',  ( 175.0461098480248552, 253.1596597119220462, 5.026615068813665488 ) ) ;
#9223 = ORIENTED_EDGE ( 'NONE', *, *, #87220, .T. ) ;
#9224 = CARTESIAN_POINT ( 'NONE',  ( 132.5758265486178971, 258.8967562850347122, -4.648177544792955347E-16 ) ) ;
#9225 = CARTESIAN_POINT ( 'NONE',  ( 154.5661245500915015, 273.4098658877936714, -13.25401299587792536 ) ) ;
#9226 = CARTESIAN_POINT ( 'NONE',  ( 185.7214976327387319, 261.5265365697691777, 10.13965854201554073 ) ) ;
#9227 = CARTESIAN_POINT ( 'NONE',  ( 206.6395994010593427, 272.7367103121227387, -10.00948282007047219 ) ) ;
#9228 = CARTESIAN_POINT ( 'NONE',  ( 138.2797325092426490, 241.4548013555409796, -4.594050593750042211 ) ) ;
#9229 = CARTESIAN_POINT ( 'NONE',  ( 189.7369823924603338, 294.6074541219386447, -12.51098987926648753 ) ) ;
#9230 = DIRECTION ( 'NONE',  ( -0.8660254037844387076, -0.4999999999999998890, -0.000000000000000000 ) ) ;
#9231 = CARTESIAN_POINT ( 'NONE',  ( 187.8039889606625934, 281.5091355175276249, -16.87056948680890756 ) ) ;
#9232 = CARTESIAN_POINT ( 'NONE',  ( 37.48526053816526371, 54.83666944042810343, 10.00000000000000000 ) ) ;
#9233 = CARTESIAN_POINT ( 'NONE',  ( 42.85403768609726427, 204.7369531367911293, -4.594050593750048428 ) ) ;
#9234 = VECTOR ( 'NONE', #14483, 1000.000000000000000 ) ;
#9236 = CARTESIAN_POINT ( 'NONE',  ( 85.35583701238070375, 48.33319239702164083, -12.28927654967825411 ) ) ;
#9235 = AXIS2_PLACEMENT_3D ( 'NONE', #17271, #24379, #9699 ) ;
#9237 = ORIENTED_EDGE ( 'NONE', *, *, #87798, .F. ) ;
#9238 = CARTESIAN_POINT ( 'NONE',  ( 15.54467260552930341, 34.00295985972733348, -10.00000000000000000 ) ) ;
#9239 = B_SPLINE_SURFACE_WITH_KNOTS ( 'NONE', 3, 1, ( 
 ( #61775, #38973 ),
 ( #61277, #76501 ),
 ( #86153, #68383 ),
 ( #7081, #23272 ),
 ( #78001, #62263 ),
 ( #15674, #92242 ),
 ( #68873, #85643 ),
 ( #60761, #46568 ),
 ( #39457, #7582 ),
 ( #29888, #99802 ),
 ( #69877, #22791 ),
 ( #30387, #8593 ),
 ( #53671, #23776 ),
 ( #31378, #93217 ),
 ( #54665, #16189 ),
 ( #3018, #32386 ),
 ( #18694, #79019 ),
 ( #57666, #63282 ),
 ( #70897, #94226 ),
 ( #80025, #63782 ),
 ( #56680, #41978 ),
 ( #1992, #10594 ),
 ( #16686, #78505 ),
 ( #1503, #18197 ),
 ( #11108, #72915 ),
 ( #86646, #71403 ),
 ( #34383, #95740 ),
 ( #26293, #41467 ),
 ( #71903, #40471 ),
 ( #24777, #9089 ),
 ( #17694, #87663 ) ),
 .UNSPECIFIED., .F., .F., .F.,
 ( 4, 3, 3, 3, 3, 3, 3, 3, 3, 3, 4 ),
 ( 2, 2 ),
 ( 0.000000000000000000, 0.1333490885032302675, 0.3007194338854343174, 0.4699862290245060414, 0.5844252810809307253, 0.6686540514502736787, 0.7354980260655518132, 0.8028463152565562533, 0.8633854507757269259, 0.9437142632667357978, 1.000000000000000000 ),
 ( 0.000000000000000000, 1.000000000000000000 ),
 .UNSPECIFIED. ) ;
#9240 = EDGE_CURVE ( 'NONE', #5477, #28117, #47743, .T. ) ;
#9241 = CARTESIAN_POINT ( 'NONE',  ( 68.59152374985116296, 70.15750495373214335, -1.449766717895635937 ) ) ;
#9242 = CARTESIAN_POINT ( 'NONE',  ( -19.65312891409030271, 93.06504152958497400, 177.5919119679930134 ) ) ;
#9243 = LINE ( 'NONE', #7231, #43383 ) ;
#9244 = CARTESIAN_POINT ( 'NONE',  ( 179.4875127409551112, 292.1681930985448048, -6.151068379627264271 ) ) ;
#9245 = CARTESIAN_POINT ( 'NONE',  ( 203.5080190724872011, 278.1607665491929993, -15.47044080916498743 ) ) ;
#9246 = EDGE_CURVE ( 'NONE', #84862, #76229, #50278, .T. ) ;
#9247 = CARTESIAN_POINT ( 'NONE',  ( 178.3290183710584529, 261.2520505181978479, 12.40287639665870145 ) ) ;
#9248 = VECTOR ( 'NONE', #40481, 1000.000000000000114 ) ;
#9249 = CARTESIAN_POINT ( 'NONE',  ( 111.2161783173811500, 245.0177522451419065, 5.000000000000046185 ) ) ;
#9250 = VECTOR ( 'NONE', #75810, 1000.000000000000227 ) ;
#9251 = EDGE_CURVE ( 'NONE', #121, #22248, #3173, .T. ) ;
#9252 = CARTESIAN_POINT ( 'NONE',  ( 194.6369916712518204, 292.8781080588906889, -14.94731529897440048 ) ) ;
#9253 = EDGE_LOOP ( 'NONE', ( #12333, #88653, #19354, #58497 ) ) ;
#9254 = EDGE_CURVE ( 'NONE', #46305, #94453, #18722, .T. ) ;
#9255 = CARTESIAN_POINT ( 'NONE',  ( 190.1158090214649405, 301.3567547831981983, -1.340987185199551845 ) ) ;
#9256 = CARTESIAN_POINT ( 'NONE',  ( 15.32787473065566530, 20.80066082961420904, 10.00000000000000533 ) ) ;
#9257 = CARTESIAN_POINT ( 'NONE',  ( 20.22912401222880519, 191.6744531367911293, 4.594050593750047540 ) ) ;
#9258 = CARTESIAN_POINT ( 'NONE',  ( 16.37683477841346402, 11.58380873178785642, 6.180339887498953466 ) ) ;
#9259 = CIRCLE ( 'NONE', #72421, 3.299999999999998934 ) ;
#9260 = CARTESIAN_POINT ( 'NONE',  ( 84.53604152985417386, 48.58536132937872765, -12.83955353848883441 ) ) ;
#9261 = LINE ( 'NONE', #40132, #27074 ) ;
#9262 = DIRECTION ( 'NONE',  ( 0.2165469281463284212, -0.9762722099447411761, 0.000000000000000000 ) ) ;
#9264 = CARTESIAN_POINT ( 'NONE',  ( 54.99669585504133096, 215.8927522451419634, 2.944929066748280225E-16 ) ) ;
#9263 = FACE_OUTER_BOUND ( 'NONE', #29365, .T. ) ;
#9265 = CARTESIAN_POINT ( 'NONE',  ( 174.3371462983394338, 288.7746536429086746, 7.657097062861912384 ) ) ;
#9266 = CARTESIAN_POINT ( 'NONE',  ( 163.1696954135087481, 256.1584459594707255, -15.01642121154493736 ) ) ;
#9267 = CARTESIAN_POINT ( 'NONE',  ( 205.1300674467857164, 275.3512963525735131, -12.60245643603069610 ) ) ;
#9268 = CARTESIAN_POINT ( 'NONE',  ( 162.2378990465211928, 251.8756868931907320, -13.00729240934857955 ) ) ;
#9269 = VERTEX_POINT ( 'NONE', #89658 ) ;
#9270 = CARTESIAN_POINT ( 'NONE',  ( 22.53878541258498558, 190.4865022471903444, -10.00000000000009415 ) ) ;
#9271 = CARTESIAN_POINT ( 'NONE',  ( 41.08847453908118297, 182.9824982072973967, 3.021315404115420679E-15 ) ) ;
#9272 = CARTESIAN_POINT ( 'NONE',  ( 156.6812872898450735, 261.2670451491295012, 0.000000000000000000 ) ) ;
#9273 = CARTESIAN_POINT ( 'NONE',  ( 0.5816933075168655431, 161.9548013555410080, -4.594050593750042211 ) ) ;
#9274 = CARTESIAN_POINT ( 'NONE',  ( 38.58005528328081368, 27.98920272979929535, 7.433330006724137462 ) ) ;
#9276 = DIRECTION ( 'NONE',  ( -1.000000000000000000, 0.000000000000000000, 0.000000000000000000 ) ) ;
#9275 = CARTESIAN_POINT ( 'NONE',  ( 167.7414737014567834, 262.5146601742941925, -16.66767127326160036 ) ) ;
#9277 = CARTESIAN_POINT ( 'NONE',  ( 186.1263547150109900, 286.8862237501084564, -16.18252752151998308 ) ) ;
#9278 = CARTESIAN_POINT ( 'NONE',  ( 164.4494343874829099, 245.8122196953522121, 2.922779519406129456 ) ) ;
#9279 = CARTESIAN_POINT ( 'NONE',  ( 183.1778755954215683, 257.7828824734294813, -2.226899175085497617 ) ) ;
#9280 = CARTESIAN_POINT ( 'NONE',  ( 66.02078622378404305, 69.01578666960394060, 2.557315166718900468 ) ) ;
#9281 = ORIENTED_EDGE ( 'NONE', *, *, #26945, .T. ) ;
#9282 = DIRECTION ( 'NONE',  ( -0.6355427771210596655, 0.000000000000000000, -0.7720656568254095076 ) ) ;
#9283 = CARTESIAN_POINT ( 'NONE',  ( 178.2609860250628913, 285.7659328021885585, 12.86945330790232411 ) ) ;
#9284 = CARTESIAN_POINT ( 'NONE',  ( 155.1343413150030415, 278.7935486042013622, -5.217350409981026615 ) ) ;
#9285 = CARTESIAN_POINT ( 'NONE',  ( 11.30507296547734342, 15.03085787977761179, 9.188101187500006262 ) ) ;
#9286 = CARTESIAN_POINT ( 'NONE',  ( -51.65147001822730033, 102.0443063789018652, -10.00000000000000000 ) ) ;
#9287 = B_SPLINE_CURVE_WITH_KNOTS ( 'NONE', 3,
 ( #41393, #71831, #72336, #2429, #3909, #10020, #65693, #49501, #18624, #40882, #80456, #26711, #88075, #81445, #33305, #96647 ),
 .UNSPECIFIED., .F., .F.,
 ( 4, 1, 2, 2, 2, 1, 2, 2, 4 ),
 ( 0.000000000000000000, 0.1250000000000000555, 0.1875000000000001388, 0.2500000000000002220, 0.5000000000000042188, 0.6250000000000081046, 0.6875000000000081046, 0.7500000000000081046, 1.000000000000000000 ),
 .UNSPECIFIED. ) ;
#9288 = CARTESIAN_POINT ( 'NONE',  ( 206.7923762329701276, 272.4720930770340033, -9.496103119940368487 ) ) ;
#9289 = CARTESIAN_POINT ( 'NONE',  ( -22.42236680055709641, 157.8615022471902591, 0.000000000000000000 ) ) ;
#9290 = DIRECTION ( 'NONE',  ( 0.000000000000000000, -0.000000000000000000, 1.000000000000000000 ) ) ;
#9291 = DIRECTION ( 'NONE',  ( -0.9919422576440838357, -0.1266907948509199411, 0.000000000000000000 ) ) ;
#9292 = CARTESIAN_POINT ( 'NONE',  ( 87.66431508103863735, 45.37878918399155737, 6.534061628821841161 ) ) ;
#9293 = CARTESIAN_POINT ( 'NONE',  ( 193.7261517370125432, 295.1034577671335342, 14.97744313279139661 ) ) ;
#9294 = EDGE_LOOP ( 'NONE', ( #42218, #78268, #24274, #871 ) ) ;
#9295 = ORIENTED_EDGE ( 'NONE', *, *, #41699, .T. ) ;
#9296 = PLANE ( 'NONE',  #98850 ) ;
#9297 = CARTESIAN_POINT ( 'NONE',  ( 192.1396999271463812, 297.8512729055811974, 12.32430960859512403 ) ) ;
#9298 = ORIENTED_EDGE ( 'NONE', *, *, #99162, .T. ) ;
#9299 = DIRECTION ( 'NONE',  ( -0.9825923819316306762, -0.1857746241280658628, 0.000000000000000000 ) ) ;
#9300 = CARTESIAN_POINT ( 'NONE',  ( 201.9093327396327595, 266.8014760598600219, -0.4683226809548139413 ) ) ;
#9301 = EDGE_LOOP ( 'NONE', ( #9077, #8434, #92845, #50816 ) ) ;
#9302 = CARTESIAN_POINT ( 'NONE',  ( 146.6834825911944620, 276.5837508513432681, 0.6716460511724984261 ) ) ;
#9303 = CARTESIAN_POINT ( 'NONE',  ( 79.16072033191954915, 59.43364827697806163, -16.53552069436851824 ) ) ;
#9305 = EDGE_CURVE ( 'NONE', #59249, #93085, #9000, .T. ) ;
#9304 = AXIS2_PLACEMENT_3D ( 'NONE', #45465, #13592, #60157 ) ;
#9306 = CARTESIAN_POINT ( 'NONE',  ( 14.02357142238433063, 26.83478043621387243, -8.090169943749479842 ) ) ;
#9307 = ORIENTED_EDGE ( 'NONE', *, *, #41896, .T. ) ;
#9308 = CARTESIAN_POINT ( 'NONE',  ( 200.1782072557437857, 283.9281697954355650, 18.05177561285849208 ) ) ;
#9309 = CARTESIAN_POINT ( 'NONE',  ( -19.65312891409030271, 93.06504152958497400, -10.00000000000000888 ) ) ;
#9310 = VECTOR ( 'NONE', #51888, 999.9999999999998863 ) ;
#9311 = CARTESIAN_POINT ( 'NONE',  ( 150.6487462746963502, 269.7157126861102370, 15.18501655901553704 ) ) ;
#9312 = CARTESIAN_POINT ( 'NONE',  ( 40.40883878445526278, 23.73415679381825782, -6.890680421881970419E-14 ) ) ;
#9313 = EDGE_LOOP ( 'NONE', ( #33858, #44053, #54989, #957 ) ) ;
#9314 = CARTESIAN_POINT ( 'NONE',  ( 150.4988332210255351, 277.8983191490532363, -3.431260130123086505 ) ) ;
#9315 = ORIENTED_EDGE ( 'NONE', *, *, #67086, .F. ) ;
#9316 = ORIENTED_EDGE ( 'NONE', *, *, #98609, .F. ) ;
#9317 = CARTESIAN_POINT ( 'NONE',  ( 74.40110702076535176, 66.01700144621987931, 13.09005787277605926 ) ) ;
#9318 = ORIENTED_EDGE ( 'NONE', *, *, #64617, .T. ) ;
#9319 = CARTESIAN_POINT ( 'NONE',  ( 181.5558742819051474, 255.2544784655372894, -2.503599602330015994 ) ) ;
#9320 = VERTEX_POINT ( 'NONE', #20219 ) ;
#9321 = AXIS2_PLACEMENT_3D ( 'NONE', #37875, #22705, #75416 ) ;
#9322 = CARTESIAN_POINT ( 'NONE',  ( 83.16451022896389134, 48.86124166517332412, 13.03494861915621250 ) ) ;
#9324 = EDGE_CURVE ( 'NONE', #45024, #15783, #11136, .T. ) ;
#9323 = CARTESIAN_POINT ( 'NONE',  ( 71.90675068868807784, 70.27826969819891190, 7.152555901417152917 ) ) ;
#9325 = CARTESIAN_POINT ( 'NONE',  ( 147.7785919239399846, 274.6869658471848652, -7.924750738206837397 ) ) ;
#9326 = CARTESIAN_POINT ( 'NONE',  ( -25.04755574468711643, 23.27320705613571761, 10.00000000000000000 ) ) ;
#9327 = DIRECTION ( 'NONE',  ( -1.000000000000000000, 0.000000000000000000, 0.000000000000000000 ) ) ;
#9328 = AXIS2_PLACEMENT_3D ( 'NONE', #95708, #9570, #79991 ) ;
#9329 = DIRECTION ( 'NONE',  ( 0.6363689690731033632, 0.7713848165480284846, 0.000000000000000000 ) ) ;
#9330 = CARTESIAN_POINT ( 'NONE',  ( 24.39888929631063519, 19.80170272979926693, 7.433330006724137462 ) ) ;
#9331 = CARTESIAN_POINT ( 'NONE',  ( 164.3939401533646958, 245.9083385283718712, 2.844462461176849200 ) ) ;
#9332 = CARTESIAN_POINT ( 'NONE',  ( 191.5682800193031312, 298.2129472994870412, -9.046807561926330621 ) ) ;
#9334 = VERTEX_POINT ( 'NONE', #14608 ) ;
#9333 = CARTESIAN_POINT ( 'NONE',  ( 159.3767386493506137, 254.5983864451355032, 15.47015898230477760 ) ) ;
#9335 = AXIS2_PLACEMENT_3D ( 'NONE', #66874, #20296, #19805 ) ;
#9336 = CARTESIAN_POINT ( 'NONE',  ( 146.8562391379555834, 276.2845277350126025, -4.054588560171046296 ) ) ;
#9337 = CARTESIAN_POINT ( 'NONE',  ( 64.47116044126103418, 196.4824982072973683, 3.021315404115420679E-15 ) ) ;
#9338 = CARTESIAN_POINT ( 'NONE',  ( 159.8732321751776624, 253.7384344327741132, -15.51998349828054202 ) ) ;
#9339 = CARTESIAN_POINT ( 'NONE',  ( 162.8751945631634612, 272.8900720096677333, -16.40198242748087054 ) ) ;
#9340 = CARTESIAN_POINT ( 'NONE',  ( 161.2313178023453588, 251.3861611254901618, 13.12937145726518473 ) ) ;
#9341 = CARTESIAN_POINT ( 'NONE',  ( 191.0846563742120736, 261.4476523433388593, -0.01535826789041113555 ) ) ;
#9342 = EDGE_LOOP ( 'NONE', ( #8851, #24414, #58746, #12168 ) ) ;
#9343 = CARTESIAN_POINT ( 'NONE',  ( 189.1639574110850504, 261.6477222806883560, 8.036472575680770447 ) ) ;
#9344 = AXIS2_PLACEMENT_3D ( 'NONE', #41394, #34791, #87590 ) ;
#9345 = CARTESIAN_POINT ( 'NONE',  ( 129.4027117968543621, 255.5177522451419350, 5.000000000000046185 ) ) ;
#9346 = CARTESIAN_POINT ( 'NONE',  ( -2.070769811622737766, 159.6115022471902023, -5.000000000000041744 ) ) ;
#9347 = CARTESIAN_POINT ( 'NONE',  ( 17.25242200676959570, 180.7677522451418497, 10.00000000000009592 ) ) ;
#9348 = CARTESIAN_POINT ( 'NONE',  ( 87.96880888631662287, 221.5958772461660544, -9.188101187500095079 ) ) ;
#9349 = CARTESIAN_POINT ( 'NONE',  ( 82.34602464792934029, 40.35042920187159154, -0.9760158778588673423 ) ) ;
#9350 = CARTESIAN_POINT ( 'NONE',  ( -48.47243291925848752, 30.64988553008148031, -10.00000000000000000 ) ) ;
#9351 = CARTESIAN_POINT ( 'NONE',  ( 163.0959165854295065, 248.1565812974573930, 11.58894702640622754 ) ) ;
#9353 = CARTESIAN_POINT ( 'NONE',  ( 75.81472511161923933, 65.61200627121189655, 13.82990332215134899 ) ) ;
#9352 = CARTESIAN_POINT ( 'NONE',  ( 10.54098545103790840, 167.7048013555410080, 4.594050593750051981 ) ) ;
#9354 = CARTESIAN_POINT ( 'NONE',  ( 200.3765029811139584, 283.5847115241710981, 16.85207472104531590 ) ) ;
#9355 = EDGE_LOOP ( 'NONE', ( #20399, #14686, #45178, #3467 ) ) ;
#9356 = VERTEX_POINT ( 'NONE', #44488 ) ;
#9357 = FACE_BOUND ( 'NONE', #18930, .T. ) ;
#9358 = EDGE_CURVE ( 'NONE', #87622, #32549, #78910, .T. ) ;
#9359 =( BOUNDED_CURVE ( )  B_SPLINE_CURVE ( 2, ( #42435, #4450, #49066, #96696, #35350, #41955, #66259, #72890, #34357 ),
 .UNSPECIFIED., .F., .T. ) 
 B_SPLINE_CURVE_WITH_KNOTS ( ( 3, 2, 2, 2, 3 ),
 ( 0.8588709677419354982, 0.8602150537634408733, 0.8629032258064516236, 0.8655913978494623739, 0.8669354838709677491 ),
 .UNSPECIFIED. ) 
 CURVE ( )  GEOMETRIC_REPRESENTATION_ITEM ( )  RATIONAL_B_SPLINE_CURVE ( ( 0.9330127018922194093, 0.9330127018922194093, 1.000000000000000000, 0.8660254037844387076, 1.000000000000000000, 0.8660254037844387076, 1.000000000000000000, 0.9330127018922194093, 0.9330127018922194093 ) ) 
 REPRESENTATION_ITEM ( '' )  );
#9360 = CARTESIAN_POINT ( 'NONE',  ( 68.66214101563461725, 70.14010656886952688, 1.798991495635525073 ) ) ;
#9361 = CARTESIAN_POINT ( 'NONE',  ( 84.83259501155069415, 44.95299106343530582, 8.440442851456150919 ) ) ;
#9362 = CARTESIAN_POINT ( 'NONE',  ( 33.73290511340745468, 201.8297689869269504, -2.679491924311252493 ) ) ;
#9363 = CARTESIAN_POINT ( 'NONE',  ( 159.0361281840726804, 267.0969579672368468, 17.40288047604528998 ) ) ;
#9364 = CARTESIAN_POINT ( 'NONE',  ( 74.13689204002625388, 68.84749506857346546, -11.26202041109552177 ) ) ;
#9365 = CARTESIAN_POINT ( 'NONE',  ( 34.24843087963692767, 181.3923013555409796, 4.594050593750050204 ) ) ;
#9366 = VECTOR ( 'NONE', #3076, 1000.000000000000000 ) ;
#9367 = CARTESIAN_POINT ( 'NONE',  ( 200.0313018224816801, 276.5939864008022369, 15.71640468486303099 ) ) ;
#9368 = ORIENTED_EDGE ( 'NONE', *, *, #75468, .T. ) ;
#9369 = CARTESIAN_POINT ( 'NONE',  ( 153.5154549565421291, 274.0811790276123361, -11.99900565267187424 ) ) ;
#9370 = EDGE_CURVE ( 'NONE', #19800, #24285, #73081, .T. ) ;
#9371 = CARTESIAN_POINT ( 'NONE',  ( 175.2906584782881794, 281.1313530038279964, -15.08317350289036618 ) ) ;
#9372 = VECTOR ( 'NONE', #47441, 1000.000000000000227 ) ;
#9373 = CARTESIAN_POINT ( 'NONE',  ( -7.997457622663985966, 160.0643266524160140, -9.188101187500093303 ) ) ;
#9374 = CARTESIAN_POINT ( 'NONE',  ( 157.8849654228661166, 257.1822134667773980, 17.43614750057631468 ) ) ;
#9375 = CIRCLE ( 'NONE', #66002, 10.99999999999999112 ) ;
#9376 = CARTESIAN_POINT ( 'NONE',  ( 193.9495889092963807, 294.7164532324382549, 15.46986001312306058 ) ) ;
#9377 = CARTESIAN_POINT ( 'NONE',  ( 161.7412967960748915, 250.5028515975580774, -14.36228887024421041 ) ) ;
#9378 = CARTESIAN_POINT ( 'NONE',  ( 186.3912171902924229, 282.9454464878770068, 16.19148905196400179 ) ) ;
#9379 = CARTESIAN_POINT ( 'NONE',  ( 194.1972774922283236, 294.2874440223457100, -15.09915398317898649 ) ) ;
#9380 = CARTESIAN_POINT ( 'NONE',  ( 192.5650826088840404, 265.1375965416604004, 7.693037692392531213 ) ) ;
#9381 = CARTESIAN_POINT ( 'NONE',  ( 171.6563989851293286, 279.7469309265732704, 14.09156877542037378 ) ) ;
#9382 = CARTESIAN_POINT ( 'NONE',  ( 147.2405539530007559, 275.6188749492528132, 0.4306668706573002492 ) ) ;
#9383 = CARTESIAN_POINT ( 'NONE',  ( 148.4049257185216106, 273.6021238924720365, 8.639190357831699529 ) ) ;
#9384 = ORIENTED_EDGE ( 'NONE', *, *, #43885, .F. ) ;
#9385 = CARTESIAN_POINT ( 'NONE',  ( 75.44414334788326926, 64.33299091768085987, 14.75074754958687429 ) ) ;
#9386 = CARTESIAN_POINT ( 'NONE',  ( 208.2939409893161553, 269.8713066281881083, 2.523744790997269227 ) ) ;
#9387 = CARTESIAN_POINT ( 'NONE',  ( 37.48526053816526371, 54.83666944042810343, -10.00000000000000000 ) ) ;
#9388 = MANIFOLD_SOLID_BREP ( 'Fillet2', #24802 ) ;
#9389 = CARTESIAN_POINT ( 'NONE',  ( 107.4275774994220001, 223.6423013555409796, -4.594050593750043987 ) ) ;
#9390 = CARTESIAN_POINT ( 'NONE',  ( 18.07869151248302941, 12.29860640527291338, -2.839279412974138328 ) ) ;
#9391 = CARTESIAN_POINT ( 'NONE',  ( 190.8860811105559208, 300.0226043892405414, 8.636347304323541252 ) ) ;
#9392 = CARTESIAN_POINT ( 'NONE',  ( -22.42236680055709641, 157.8615022471902591, 0.000000000000000000 ) ) ;
#9393 = CIRCLE ( 'NONE', #91954, 0.1418229129680880773 ) ;
#9395 = CARTESIAN_POINT ( 'NONE',  ( 162.1966646769166402, 251.8715883092360741, -14.10328369067750920 ) ) ;
#9394 = CARTESIAN_POINT ( 'NONE',  ( 157.1837449796689725, 258.3967629017010381, 16.97243084443542216 ) ) ;
#9396 = CARTESIAN_POINT ( 'NONE',  ( 148.5272680744187141, 275.3902207161408455, -7.185975151065171929 ) ) ;
#9397 = CARTESIAN_POINT ( 'NONE',  ( 193.5005633302724277, 262.8551920378705518, -5.236817587991198231 ) ) ;
#9398 = CARTESIAN_POINT ( 'NONE',  ( 149.4456112649506281, 271.7996036513546869, -12.95648166494593667 ) ) ;
#9399 = CARTESIAN_POINT ( 'NONE',  ( 31.74858474661088081, 18.73415679381823651, -6.890680421881970419E-14 ) ) ;
#9400 = CARTESIAN_POINT ( 'NONE',  ( 175.8870957750795583, 292.5986786893511749, -1.137309599147465544 ) ) ;
#9401 = DIRECTION ( 'NONE',  ( 0.9919084036772433111, -0.1269555777209603886, 0.000000000000000000 ) ) ;
#9402 = ORIENTED_EDGE ( 'NONE', *, *, #75737, .F. ) ;
#9403 = DIRECTION ( 'NONE',  ( -0.8660254037844379305, -0.5000000000000011102, -0.000000000000000000 ) ) ;
#9404 = CARTESIAN_POINT ( 'NONE',  ( 191.1334924437351219, 271.5868773173968975, -15.78614548220010150 ) ) ;
#9405 = CARTESIAN_POINT ( 'NONE',  ( 82.29734961797252879, 53.60383310410945512, 15.81226994477779790 ) ) ;
#9406 = ORIENTED_EDGE ( 'NONE', *, *, #12031, .T. ) ;
#9407 = CARTESIAN_POINT ( 'NONE',  ( 75.72636783681542738, 65.12249353091223725, -14.45027308884206718 ) ) ;
#9408 = CARTESIAN_POINT ( 'NONE',  ( -19.65312891409030271, 93.06504152958497400, 59.99999999999999289 ) ) ;
#9409 = CARTESIAN_POINT ( 'NONE',  ( 180.2260403442535051, 295.0423342771414923, -3.480517403894910711 ) ) ;
#9410 = CARTESIAN_POINT ( 'NONE',  ( 152.7531861616124615, 266.0707158804971186, 17.45453282433162556 ) ) ;
#9411 = CIRCLE ( 'NONE', #66041, 70.00000000000001421 ) ;
#9412 = ORIENTED_EDGE ( 'NONE', *, *, #19558, .T. ) ;
#9413 = B_SPLINE_CURVE_WITH_KNOTS ( 'NONE', 3,
 ( #26087, #41258, #10891, #56962 ),
 .UNSPECIFIED., .F., .F.,
 ( 4, 4 ),
 ( 0.02929424324998682050, 0.03843412274503782422 ),
 .UNSPECIFIED. ) ;
#9414 = CARTESIAN_POINT ( 'NONE',  ( 202.6051175132338926, 273.9538057854381350, -13.19822448684500849 ) ) ;
#9415 = CARTESIAN_POINT ( 'NONE',  ( 38.25529575686164208, 27.80170272979929535, 7.433330006724137462 ) ) ;
#9416 = CARTESIAN_POINT ( 'NONE',  ( 73.01784879798562145, 70.40283164995553022, -8.092307369146576335 ) ) ;
#9417 = EDGE_LOOP ( 'NONE', ( #17550, #95200, #90866, #25561 ) ) ;
#9418 = CARTESIAN_POINT ( 'NONE',  ( 78.05395834205243943, 61.78695400133908322, 16.08488452160743165 ) ) ;
#9419 = CARTESIAN_POINT ( 'NONE',  ( 41.47569090598248920, 209.1868197944957899, -18.47570218321542868 ) ) ;
#9420 = CARTESIAN_POINT ( 'NONE',  ( 13.01250597095616612, 184.9865022471903160, 10.00000000000009415 ) ) ;
#9421 = ORIENTED_EDGE ( 'NONE', *, *, #3648, .T. ) ;
#9422 = CARTESIAN_POINT ( 'NONE',  ( 79.43406943547307719, 59.55633321778628897, 16.18157302954037391 ) ) ;
#9423 = DIRECTION ( 'NONE',  ( -0.8660254037844387076, -0.4999999999999998890, -0.000000000000000000 ) ) ;
#9424 = CARTESIAN_POINT ( 'NONE',  ( 164.2059258710715994, 246.2339888178522926, 7.329631442356459914 ) ) ;
#9425 = CARTESIAN_POINT ( 'NONE',  ( 21.14026940803790566, 27.90829794293880539, 10.00000000000000355 ) ) ;
#9426 = DIRECTION ( 'NONE',  ( 1.000000000000000000, 0.000000000000000000, 0.000000000000000000 ) ) ;
#9427 = EDGE_CURVE ( 'NONE', #1759, #4426, #2559, .T. ) ;
#9428 = CARTESIAN_POINT ( 'NONE',  ( 82.00481806099733717, 45.27543476315971560, -11.33045944147468020 ) ) ;
#9429 = CARTESIAN_POINT ( 'NONE',  ( 155.6535436963908694, 261.0471492701456668, -17.87366571046205976 ) ) ;
#9430 = VERTEX_POINT ( 'NONE', #54077 ) ;
#9431 = EDGE_CURVE ( 'NONE', #24288, #80596, #84055, .T. ) ;
#9432 = EDGE_LOOP ( 'NONE', ( #66152, #28594, #66415, #75582, #49979, #14045, #77775, #974, #49654, #44163, #32256 ) ) ;
#9433 = CARTESIAN_POINT ( 'NONE',  ( 178.7753799676760593, 260.4554649793954582, 12.02876886862545902 ) ) ;
#9434 = ORIENTED_EDGE ( 'NONE', *, *, #42423, .F. ) ;
#9435 = CARTESIAN_POINT ( 'NONE',  ( 77.19776191479694205, 49.58695339317465312, -15.48335642945104595 ) ) ;
#9436 = EDGE_LOOP ( 'NONE', ( #87482, #85290 ) ) ;
#9437 = CARTESIAN_POINT ( 'NONE',  ( 173.2337249902883798, 270.7486416191997023, 17.82094672905207133 ) ) ;
#9438 = DIRECTION ( 'NONE',  ( -0.8600446134263880493, -0.5102188382608534578, 0.000000000000000000 ) ) ;
#9439 = ORIENTED_EDGE ( 'NONE', *, *, #8873, .F. ) ;
#9440 = CARTESIAN_POINT ( 'NONE',  ( 185.9161404575009158, 282.4097951900486123, -17.21525070205280628 ) ) ;
#9441 = LINE ( 'NONE', #85486, #20695 ) ;
#9442 = CARTESIAN_POINT ( 'NONE',  ( 70.71926666893401148, 71.45048000115950515, 3.795742845772093865 ) ) ;
#9443 = CARTESIAN_POINT ( 'NONE',  ( 170.8805640699686990, 257.7213711969266114, 14.63406020945912367 ) ) ;
#9444 = CARTESIAN_POINT ( 'NONE',  ( 196.2953682204578456, 263.5854184417236752, 0.8810977108677261471 ) ) ;
#9445 = AXIS2_PLACEMENT_3D ( 'NONE', #2121, #72023, #40085 ) ;
#9446 = B_SPLINE_CURVE_WITH_KNOTS ( 'NONE', 3,
 ( #45027, #90695, #59209, #68327 ),
 .UNSPECIFIED., .F., .F.,
 ( 4, 4 ),
 ( 0.01331880355540019864, 0.01957602511303062343 ),
 .UNSPECIFIED. ) ;
#9448 = EDGE_CURVE ( 'NONE', #11831, #18551, #46480, .T. ) ;
#9447 = CARTESIAN_POINT ( 'NONE',  ( 201.4066285247549786, 281.8004817444100354, -17.79749223817309201 ) ) ;
#9449 = CARTESIAN_POINT ( 'NONE',  ( -31.49356256989596758, 94.88921800892812541, 43.89948692389422291 ) ) ;
#9451 = CARTESIAN_POINT ( 'NONE',  ( 153.9322886533809083, 279.5979162416960548, 2.179338631777613333 ) ) ;
#9450 = CIRCLE ( 'NONE', #85564, 17.82106496071138935 ) ;
#9452 = CARTESIAN_POINT ( 'NONE',  ( 131.5951856977227123, 234.5327760586659451, 1.948934522072303157E-15 ) ) ;
#9454 = B_SPLINE_CURVE_WITH_KNOTS ( 'NONE', 3,
 ( #92109, #29264, #22656, #60134, #21661, #52542, #83493, #44940, #75884, #6462, #29755, #60627, #47436, #15033, #78869, #77351, #86014, #45925, #16541, #40325, #15525, #70745, #46426, #24640, #46946, #9453, #8945, #55520, #7958, #39813, #94583, #77863, #8449, #86508, #47929, #69240, #1356, #17037, #38832, #39320, #7440, #31235, #30756, #100170, #71265, #32241, #16044, #38332, #62625, #84489 ),
 .UNSPECIFIED., .F., .F.,
 ( 4, 2, 2, 2, 2, 2, 2, 2, 2, 2, 2, 2, 2, 2, 2, 2, 2, 2, 2, 2, 2, 2, 2, 2, 4 ),
 ( 0.0002765172614649375328, 0.001291974074908197687, 0.001799702481629788598, 0.002053566684990593919, 0.002180498786671015987, 0.002307430888351438489, 0.002434362990031860557, 0.002561295091712283058, 0.002815159295073127628, 0.003322887701794880085, 0.004338344515238447448, 0.005353801328682013944, 0.005861529735403797625, 0.006115393938764732834, 0.006369258142125667176, 0.006432724192965878426, 0.006496190243806089677, 0.006559656294646300928, 0.006623122345486511311, 0.006876986548847315549, 0.007384714955568918819, 0.007638579158929679688, 0.007892443362290439690, 0.008146307565651199692, 0.008400171769011959694 ),
 .UNSPECIFIED. ) ;
#9453 = CARTESIAN_POINT ( 'NONE',  ( 186.1868697629463725, 262.4753163803031271, -9.036959360852598877 ) ) ;
#9455 = CARTESIAN_POINT ( 'NONE',  ( 43.33837710268888799, 27.94754757982092741, 5.678558825948272215 ) ) ;
#9456 = AXIS2_PLACEMENT_3D ( 'NONE', #41110, #78649, #94370 ) ;
#9457 = ORIENTED_EDGE ( 'NONE', *, *, #90113, .T. ) ;
#9458 = AXIS2_PLACEMENT_3D ( 'NONE', #15664, #8087, #55155 ) ;
#9460 = ORIENTED_EDGE ( 'NONE', *, *, #61819, .F. ) ;
#9459 = CARTESIAN_POINT ( 'NONE',  ( 83.92684454729288746, 43.42296649151629140, -7.738650150025851993 ) ) ;
#9461 = CARTESIAN_POINT ( 'NONE',  ( 200.1427641401880066, 273.7077546088841586, 13.87784847088884810 ) ) ;
#9462 = CARTESIAN_POINT ( 'NONE',  ( 78.08206365161463225, 61.83366292688850763, -15.70979438352861735 ) ) ;
#9463 = CARTESIAN_POINT ( 'NONE',  ( 165.3413037017489273, 246.0692819571209213, -2.848003664914541044 ) ) ;
#9464 = LINE ( 'NONE', #71776, #11066 ) ;
#9465 = CARTESIAN_POINT ( 'NONE',  ( 73.53703480203567722, 67.51361842960002946, 11.62355896671093980 ) ) ;
#9466 = DIRECTION ( 'NONE',  ( -0.000000000000000000, -0.000000000000000000, -1.000000000000000000 ) ) ;
#9467 = CARTESIAN_POINT ( 'NONE',  ( 174.3231258461450466, 287.3639690219702061, -9.459891945542938885 ) ) ;
#9468 = EDGE_CURVE ( 'NONE', #8907, #68859, #6146, .T. ) ;
#9469 = CARTESIAN_POINT ( 'NONE',  ( 31.51172446742527100, 30.14441083166263269, 10.00000000000000533 ) ) ;
#9470 = CARTESIAN_POINT ( 'NONE',  ( 48.58227110419246486, 77.44677708231242264, 177.5919119679930134 ) ) ;
#9471 = VECTOR ( 'NONE', #42394, 1000.000000000000000 ) ;
#9472 = ORIENTED_EDGE ( 'NONE', *, *, #42849, .F. ) ;
#9473 = CARTESIAN_POINT ( 'NONE',  ( 194.4032909867620447, 293.9306181827685123, -16.05392006271526384 ) ) ;
#9474 = CARTESIAN_POINT ( 'NONE',  ( 8.159155267032986103, 175.5177522451418781, -10.00000000000009592 ) ) ;
#9475 = ORIENTED_EDGE ( 'NONE', *, *, #36829, .F. ) ;
#9476 = FACE_OUTER_BOUND ( 'NONE', #82869, .T. ) ;
#9477 = CARTESIAN_POINT ( 'NONE',  ( 190.4221740917990928, 282.9812683428133369, -16.56494496364181401 ) ) ;
#9478 = CARTESIAN_POINT ( 'NONE',  ( 191.9719415786559864, 298.1418388885606419, -10.91218611428179663 ) ) ;
#9479 = CARTESIAN_POINT ( 'NONE',  ( 190.0274641710971082, 301.5097725526222803, 3.738976720635653450 ) ) ;
#9480 = CARTESIAN_POINT ( 'NONE',  ( 163.0171530587457767, 248.2930037274571191, 9.677214176418313940 ) ) ;
#9482 = CARTESIAN_POINT ( 'NONE',  ( 154.9430233944070494, 277.5162282063104158, -8.894456736302846167 ) ) ;
#9481 = CARTESIAN_POINT ( 'NONE',  ( 162.6609004217042127, 282.2048157055750153, -6.605852966852150843 ) ) ;
#9483 = CARTESIAN_POINT ( 'NONE',  ( 199.9620668144054036, 267.3927500580807077, 6.252404634128969185 ) ) ;
#9484 = EDGE_LOOP ( 'NONE', ( #93839, #48345, #75471, #1274 ) ) ;
#9485 = CARTESIAN_POINT ( 'NONE',  ( -105.0000000000000000, 4.999999999999999112, 59.99999999999999289 ) ) ;
#9486 = B_SPLINE_SURFACE_WITH_KNOTS ( 'NONE', 3, 1, ( 
 ( #41780, #1801 ),
 ( #2309, #56974 ),
 ( #64090, #40269 ),
 ( #87473, #71718 ),
 ( #2817, #25079 ),
 ( #33190, #17489 ),
 ( #48899, #87960 ),
 ( #56485, #18504 ),
 ( #78806, #79835 ),
 ( #32685, #9394 ),
 ( #10904, #86954 ),
 ( #18007, #48395 ),
 ( #72213, #80335 ),
 ( #47382, #78306 ),
 ( #63586, #39756 ),
 ( #33708, #9908 ),
 ( #64599, #49390 ),
 ( #72726, #3317 ),
 ( #1299, #63085 ),
 ( #34197, #65087 ),
 ( #94031, #24582 ),
 ( #27101, #67073 ),
 ( #28576, #67573 ),
 ( #36170, #50382 ),
 ( #11420, #89443 ),
 ( #26599, #13398 ),
 ( #19999, #58470 ),
 ( #21008, #5777 ),
 ( #42763, #44270 ),
 ( #58951, #81334 ),
 ( #35179, #89923 ),
 ( #57985, #96531 ),
 ( #20501, #3801 ),
 ( #97996, #12402 ) ),
 .UNSPECIFIED., .T., .F., .F.,
 ( 4, 2, 2, 2, 2, 2, 2, 2, 2, 2, 2, 2, 2, 2, 2, 2, 4 ),
 ( 2, 2 ),
 ( 0.000000000000000000, 0.06250000000000000000, 0.1250000000000000000, 0.1875000000000000000, 0.2500000000000000000, 0.3125000000000000000, 0.3750000000000000000, 0.4375000000000000000, 0.5000000000000000000, 0.5625000000000000000, 0.6250000000000000000, 0.6875000000000000000, 0.7500000000000000000, 0.8125000000000000000, 0.8750000000000000000, 0.9375000000000000000, 1.000000000000000000 ),
 ( 0.000000000000000000, 1.000000000000000000 ),
 .UNSPECIFIED. ) ;
#9487 = EDGE_CURVE ( 'NONE', #32467, #10367, #38887, .T. ) ;
#9488 = CARTESIAN_POINT ( 'NONE',  ( 164.1364336533802373, 247.9930260721589832, -8.912795639077232934 ) ) ;
#9489 = CARTESIAN_POINT ( 'NONE',  ( 190.0387662407789549, 274.4106552748930312, -15.66928402959891997 ) ) ;
#9490 = DIRECTION ( 'NONE',  ( 1.000000000000000000, 0.000000000000000000, 0.000000000000000000 ) ) ;
#9491 = EDGE_CURVE ( 'NONE', #73699, #56530, #68200, .T. ) ;
#9492 = B_SPLINE_CURVE_WITH_KNOTS ( 'NONE', 3,
 ( #83602, #37936, #90214, #99279 ),
 .UNSPECIFIED., .F., .F.,
 ( 4, 4 ),
 ( 0.01043980270801778479, 0.01580741937697933627 ),
 .UNSPECIFIED. ) ;
#9493 = CARTESIAN_POINT ( 'NONE',  ( 186.8081210542937356, 297.5510969845519753, -4.266410382973029769 ) ) ;
#9494 = CARTESIAN_POINT ( 'NONE',  ( 192.6470966816805230, 296.9724359471326807, 11.11268290051284424 ) ) ;
#9495 = CARTESIAN_POINT ( 'NONE',  ( 74.35260113823048300, 68.48135296369000002, 11.70560402319359561 ) ) ;
#9496 = ADVANCED_FACE ( 'NONE', ( #36281 ), #43875, .F. ) ;
#9497 = CARTESIAN_POINT ( 'NONE',  ( 194.0672051292551430, 294.5127359636757660, 15.53337744471869364 ) ) ;
#9498 = CARTESIAN_POINT ( 'NONE',  ( 68.48067871107335236, 70.13512158218014747, 0.9310271535938260401 ) ) ;
#9499 = CARTESIAN_POINT ( 'NONE',  ( 2.016134656476094023, 159.7202760586659451, -5.415160957724236172E-17 ) ) ;
#9500 = CARTESIAN_POINT ( 'NONE',  ( 86.39896429407481548, 226.8149278399160664, 9.188101187500093303 ) ) ;
#9501 = CARTESIAN_POINT ( 'NONE',  ( 67.21538324255706698, 66.58946535461426208, 8.499949113996416727 ) ) ;
#9502 = CARTESIAN_POINT ( 'NONE',  ( 192.4335622838504207, 297.3422883733380786, -12.83044365323471325 ) ) ;
#9503 = CARTESIAN_POINT ( 'NONE',  ( 147.7258779941464297, 275.3197464395427119, 3.871639344198308574 ) ) ;
#9504 = EDGE_CURVE ( 'NONE', #81911, #98268, #45852, .T. ) ;
#9505 = CARTESIAN_POINT ( 'NONE',  ( 203.2369479875374623, 278.6302754407888074, -16.66242713208754367 ) ) ;
#9506 = ADVANCED_FACE ( 'NONE', ( #29685 ), #76775, .T. ) ;
#9507 = VECTOR ( 'NONE', #97237, 1000.000000000000000 ) ;
#9508 = CARTESIAN_POINT ( 'NONE',  ( -28.74356256989596758, 94.88921800892812541, 45.19948692389422717 ) ) ;
#9509 = SURFACE_STYLE_USAGE ( .BOTH. , #32289 ) ;
#9510 = LINE ( 'NONE', #71312, #77599 ) ;
#9512 = CARTESIAN_POINT ( 'NONE',  ( 163.4139553296302267, 247.6057220337265505, -10.31482883765270842 ) ) ;
#9511 = PLANE ( 'NONE',  #19313 ) ;
#9513 = EDGE_CURVE ( 'NONE', #67607, #49038, #29197, .T. ) ;
#9514 = CARTESIAN_POINT ( 'NONE',  ( 178.0260107266225020, 289.8946666044191716, 9.616295053996276820 ) ) ;
#9515 = EDGE_CURVE ( 'NONE', #17295, #56255, #60065, .T. ) ;
#9516 = CARTESIAN_POINT ( 'NONE',  ( 46.50192534792603283, 74.36443251879779837, -10.00000000000000000 ) ) ;
#9517 = B_SPLINE_CURVE_WITH_KNOTS ( 'NONE', 3,
 ( #49937, #96587, #57024, #65629, #65137, #66135, #11469, #27151, #3846, #96085, #35234, #4854, #20053, #12452 ),
 .UNSPECIFIED., .F., .F.,
 ( 4, 2, 2, 2, 2, 2, 4 ),
 ( 0.001120812635800888610, 0.001358725036700777480, 0.001596637437600666133, 0.001834549838500555002, 0.002072462239400443655, 0.002548287041200175858, 0.003024111842999908061 ),
 .UNSPECIFIED. ) ;
#9518 = DIRECTION ( 'NONE',  ( -0.6793907169778431454, 0.000000000000000000, -0.7337767056021416989 ) ) ;
#9519 = CARTESIAN_POINT ( 'NONE',  ( 73.81716743588172847, 56.51341352178555866, -16.05755937095091923 ) ) ;
#9520 = CARTESIAN_POINT ( 'NONE',  ( -12.69762320744227502, 170.1427522451419350, -10.00000000000009592 ) ) ;
#9521 = CARTESIAN_POINT ( 'NONE',  ( 34.76219959342768107, 197.0024278399161233, 9.188101187500095079 ) ) ;
#9522 = CARTESIAN_POINT ( 'NONE',  ( 77.03509876804180578, 63.43842436480252900, -15.45738776637924516 ) ) ;
#9523 = VECTOR ( 'NONE', #84866, 1000.000000000000000 ) ;
#9524 = CARTESIAN_POINT ( 'NONE',  ( 59.87693630317638593, 211.5024278399160949, -9.188101187500093303 ) ) ;
#9525 = FACE_OUTER_BOUND ( 'NONE', #52660, .T. ) ;
#9526 = CARTESIAN_POINT ( 'NONE',  ( 88.29618083833925368, 44.15377159048836830, 0.4144604853962327584 ) ) ;
#9527 = CIRCLE ( 'NONE', #58100, 60.00000000000002132 ) ;
#9528 = CARTESIAN_POINT ( 'NONE',  ( 83.31851016613751426, 49.62898418713007231, -13.46204844297379388 ) ) ;
#9530 = LINE ( 'NONE', #92648, #42504 ) ;
#9529 = FACE_OUTER_BOUND ( 'NONE', #15122, .T. ) ;
#9531 = VECTOR ( 'NONE', #87413, 1000.000000000000227 ) ;
#9532 = CARTESIAN_POINT ( 'NONE',  ( 196.8111907360481609, 268.4516160315483830, -10.82598805925545626 ) ) ;
#9533 = CARTESIAN_POINT ( 'NONE',  ( 29.64435718874111458, 29.06628583063843152, -9.188101187500006262 ) ) ;
#9534 = CARTESIAN_POINT ( 'NONE',  ( 41.08847453908118297, 182.9824982072973967, 3.021315404115420679E-15 ) ) ;
#9535 = CARTESIAN_POINT ( 'NONE',  ( 78.55537653917157570, 48.00561504237174404, -13.97647359956260082 ) ) ;
#9536 = ORIENTED_EDGE ( 'NONE', *, *, #67306, .F. ) ;
#9537 = CARTESIAN_POINT ( 'NONE',  ( 11.76515913632831101, 28.83396525600389282, -2.839279412974133887 ) ) ;
#9538 = CARTESIAN_POINT ( 'NONE',  ( 58.09093245575348874, 204.3458772461660544, 9.188101187500095079 ) ) ;
#9539 = FACE_OUTER_BOUND ( 'NONE', #81835, .T. ) ;
#9540 = DIRECTION ( 'NONE',  ( 0.02977611660965746518, -0.9995565931350001154, 0.000000000000000000 ) ) ;
#9541 = VECTOR ( 'NONE', #73604, 1000.000000000000000 ) ;
#9542 = CARTESIAN_POINT ( 'NONE',  ( 198.5612432604688991, 286.7288335892616260, 18.30793681285053509 ) ) ;
#9543 = CARTESIAN_POINT ( 'NONE',  ( 74.10110473074108484, 67.08709595610132226, 12.20209729311798341 ) ) ;
#9544 = CARTESIAN_POINT ( 'NONE',  ( 153.8017027926681521, 264.2546318029277472, 18.09987928383549516 ) ) ;
#9545 = ORIENTED_EDGE ( 'NONE', *, *, #43878, .T. ) ;
#9547 = CARTESIAN_POINT ( 'NONE',  ( 87.48880955142448101, 44.86412769470708639, -6.596395727433105094 ) ) ;
#9546 = AXIS2_PLACEMENT_3D ( 'NONE', #63378, #15764, #48176 ) ;
#9548 = CARTESIAN_POINT ( 'NONE',  ( 130.4311169673963775, 236.1115022471901739, -5.000000000000041744 ) ) ;
#9549 = CARTESIAN_POINT ( 'NONE',  ( 165.0156970625405108, 244.8314239717225007, -1.890480716182876719 ) ) ;
#9550 = ORIENTED_EDGE ( 'NONE', *, *, #21528, .F. ) ;
#9551 = CARTESIAN_POINT ( 'NONE',  ( 86.36237991899166389, 47.04137177816882343, 10.01663566065926325 ) ) ;
#9552 = CARTESIAN_POINT ( 'NONE',  ( 188.2373216092262282, 273.3416365267268588, 15.62028696804763683 ) ) ;
#9553 = EDGE_LOOP ( 'NONE', ( #45729, #11598, #50195, #69957 ) ) ;
#9554 = CARTESIAN_POINT ( 'NONE',  ( 206.2809287719926488, 273.3579460648492159, -10.70911012174624588 ) ) ;
#9555 = CARTESIAN_POINT ( 'NONE',  ( -30.04356256989597185, 94.88921800892812541, 45.19948692389422717 ) ) ;
#9556 = CARTESIAN_POINT ( 'NONE',  ( 67.42721094069274557, 68.56443353946191621, -5.087393618767618975 ) ) ;
#9557 = VERTEX_POINT ( 'NONE', #63072 ) ;
#9558 = CARTESIAN_POINT ( 'NONE',  ( 177.0689902789707730, 252.6641302495915511, -0.2682384293953795629 ) ) ;
#9559 = EDGE_LOOP ( 'NONE', ( #67347, #82118, #10949, #76829 ) ) ;
#9560 = DIRECTION ( 'NONE',  ( 0.5000000000000013323, -0.8660254037844378194, 0.000000000000000000 ) ) ;
#9561 = CARTESIAN_POINT ( 'NONE',  ( 170.5571078448917888, 250.3859201599777293, 3.400624622539324182 ) ) ;
#9562 = CARTESIAN_POINT ( 'NONE',  ( 148.7859755799365189, 273.9149749650962349, 8.803960254582356981 ) ) ;
#9563 = ORIENTED_EDGE ( 'NONE', *, *, #87191, .F. ) ;
#9564 = ADVANCED_FACE ( 'NONE', ( #85423 ), #68706, .F. ) ;
#9565 = CARTESIAN_POINT ( 'NONE',  ( 29.59504171901726366, 22.80170272979927759, 7.433330006724137462 ) ) ;
#9566 = CARTESIAN_POINT ( 'NONE',  ( 74.89653295760797391, 66.81943746227950953, -13.20645658646817999 ) ) ;
#9567 = CARTESIAN_POINT ( 'NONE',  ( 78.71043930997907978, 49.45733721402466898, -14.60309932591205317 ) ) ;
#9568 = ADVANCED_FACE ( 'NONE', ( #75428 ), #53108, .F. ) ;
#9569 = EDGE_LOOP ( 'NONE', ( #81376, #43308, #66224, #44522 ) ) ;
#9570 = DIRECTION ( 'NONE',  ( -0.000000000000000000, -0.000000000000000000, -1.000000000000000000 ) ) ;
#9571 = CARTESIAN_POINT ( 'NONE',  ( 159.5895502557670795, 254.2297859303815244, -16.92708575547316485 ) ) ;
#9572 = ORIENTED_EDGE ( 'NONE', *, *, #98923, .T. ) ;
#9573 = ORIENTED_EDGE ( 'NONE', *, *, #40056, .T. ) ;
#9574 = CARTESIAN_POINT ( 'NONE',  ( 185.4975199963478474, 297.4654133624536598, 1.032910119675109817 ) ) ;
#9575 = CARTESIAN_POINT ( 'NONE',  ( 194.8708600166808651, 293.1207648669033006, -14.79199694356877970 ) ) ;
#9576 = DIRECTION ( 'NONE',  ( 1.000000000000000000, 0.000000000000000000, 0.000000000000000000 ) ) ;
#9577 = CARTESIAN_POINT ( 'NONE',  ( 193.9966098916996771, 294.6350105018939871, 13.97117019253516013 ) ) ;
#9578 = CARTESIAN_POINT ( 'NONE',  ( 185.4470681627111901, 292.4290838876615908, -11.21142039403692259 ) ) ;
#9579 = CARTESIAN_POINT ( 'NONE',  ( 157.8239779013331372, 257.2878469527003062, -17.92251383114021479 ) ) ;
#9581 = ADVANCED_FACE ( 'NONE', ( #52105 ), #7497, .T. ) ;
#9580 = CARTESIAN_POINT ( 'NONE',  ( -14.83262083840143575, 124.7156766241961208, -21.50000000000003197 ) ) ;
#9582 = CARTESIAN_POINT ( 'NONE',  ( -52.76723787663020460, 95.88936769132961047, -10.00000000000000000 ) ) ;
#9583 = CARTESIAN_POINT ( 'NONE',  ( 179.3546098028610061, 287.2282261399536196, -13.91071825436259601 ) ) ;
#9584 = CARTESIAN_POINT ( 'NONE',  ( 92.13672968991174628, 217.8768266524159856, 9.188101187500098632 ) ) ;
#9585 = VERTEX_POINT ( 'NONE', #98234 ) ;
#9586 = CARTESIAN_POINT ( 'NONE',  ( 190.8094645593471341, 300.1553081486349015, 8.399847186519689757 ) ) ;
#9587 = CARTESIAN_POINT ( 'NONE',  ( 8.106622824862185439, 30.17147933776455204, -10.00000000000000000 ) ) ;
#9588 = CARTESIAN_POINT ( 'NONE',  ( -19.65312891409030271, 93.06504152958497400, 59.99999999999999289 ) ) ;
#9589 = VERTEX_POINT ( 'NONE', #67818 ) ;
#9590 = CARTESIAN_POINT ( 'NONE',  ( 156.6856598554248023, 259.2594716433859503, -17.52902947127937949 ) ) ;
#9591 = ORIENTED_EDGE ( 'NONE', *, *, #59323, .T. ) ;
#9592 = CARTESIAN_POINT ( 'NONE',  ( 189.0689802957956260, 269.8288687927027354, -15.50864081522695415 ) ) ;
#9593 = CARTESIAN_POINT ( 'NONE',  ( -19.65312891409030271, 93.06504152958497400, 10.00000000000000888 ) ) ;
#9594 = EDGE_CURVE ( 'NONE', #35100, #44921, #94800, .T. ) ;
#9595 = CARTESIAN_POINT ( 'NONE',  ( 191.7187529716733820, 298.5803744197520473, -8.487597704798396592 ) ) ;
#9596 = DIRECTION ( 'NONE',  ( 0.5000000000000048850, -0.8660254037844358210, 0.000000000000000000 ) ) ;
#9597 = CARTESIAN_POINT ( 'NONE',  ( 82.14160159532623595, 47.93221979345100436, -12.80134787886038161 ) ) ;
#9598 = CARTESIAN_POINT ( 'NONE',  ( 162.6419541827858950, 248.9428672435623184, 10.30167521348375459 ) ) ;
#9599 = EDGE_CURVE ( 'NONE', #91585, #32767, #2936, .T. ) ;
#9600 = CARTESIAN_POINT ( 'NONE',  ( 89.86341300497758766, 216.5643266524160140, 9.188101187500095079 ) ) ;
#9601 = VERTEX_POINT ( 'NONE', #28819 ) ;
#9602 = ORIENTED_EDGE ( 'NONE', *, *, #69648, .F. ) ;
#9603 = CARTESIAN_POINT ( 'NONE',  ( 123.3405339703633672, 232.0177522451417929, 5.000000000000051514 ) ) ;
#9604 = CARTESIAN_POINT ( 'NONE',  ( 163.3473224498206093, 247.7211335670114352, -10.00320358166632850 ) ) ;
#9605 = AXIS2_PLACEMENT_3D ( 'NONE', #51637, #20748, #53122 ) ;
#9606 = ORIENTED_EDGE ( 'NONE', *, *, #7091, .F. ) ;
#9607 = VECTOR ( 'NONE', #45303, 1000.000000000000000 ) ;
#9608 = CARTESIAN_POINT ( 'NONE',  ( -22.42236680055709641, 157.8615022471902591, 0.000000000000000000 ) ) ;
#9609 = CARTESIAN_POINT ( 'NONE',  ( 165.1340499804484523, 285.1150614822342391, 0.5054430236558116185 ) ) ;
#9610 = CARTESIAN_POINT ( 'NONE',  ( 101.3470971569689141, 235.9865022471903160, 10.00000000000009415 ) ) ;
#9611 = CARTESIAN_POINT ( 'NONE',  ( 88.00768034709845722, 44.38581256804975794, 4.745967170566630422 ) ) ;
#9612 = AXIS2_PLACEMENT_3D ( 'NONE', #95245, #25814, #12098 ) ;
#9613 = EDGE_LOOP ( 'NONE', ( #48193, #75501, #54470, #86242 ) ) ;
#9614 = CARTESIAN_POINT ( 'NONE',  ( 85.17088969497783069, 43.77888550337738138, -6.018426280060992895 ) ) ;
#9615 = CARTESIAN_POINT ( 'NONE',  ( 160.6168281341388422, 275.7216313598870556, 14.06045084403267609 ) ) ;
#9616 = EDGE_CURVE ( 'NONE', #50075, #72450, #48853, .T. ) ;
#9617 = CARTESIAN_POINT ( 'NONE',  ( 206.8659638600981623, 272.3446355680395641, -10.26115277030573125 ) ) ;
#9618 = CARTESIAN_POINT ( 'NONE',  ( 19.98788723728717898, 104.4047874917408336, 22.50000000000002132 ) ) ;
#9619 = CARTESIAN_POINT ( 'NONE',  ( 176.8429236348229381, 284.5432036437209717, 13.07041713469269162 ) ) ;
#9620 = CARTESIAN_POINT ( 'NONE',  ( 106.8860512984590088, 232.5177522451418781, -10.00000000000009592 ) ) ;
#9621 = CARTESIAN_POINT ( 'NONE',  ( 195.4522889637296146, 279.6111606360764767, -17.26969813293585787 ) ) ;
#9622 = ORIENTED_EDGE ( 'NONE', *, *, #84564, .T. ) ;
#9623 = CARTESIAN_POINT ( 'NONE',  ( 8.774901663922227257, 164.3262482093457777, 3.021315404115420679E-15 ) ) ;
#9624 = VECTOR ( 'NONE', #54120, 1000.000000000000000 ) ;
#9625 = EDGE_CURVE ( 'NONE', #14882, #41928, #6398, .T. ) ;
#9626 = CARTESIAN_POINT ( 'NONE',  ( 161.1611771195837548, 251.5076483517112536, 14.17749514252127163 ) ) ;
#9627 = CARTESIAN_POINT ( 'NONE',  ( 85.22848849487193945, 43.87423014350909511, 6.205650761890156630 ) ) ;
#9628 = CARTESIAN_POINT ( 'NONE',  ( 188.1686623141184782, 265.7851399264815768, -13.17430125897227455 ) ) ;
#9629 = CARTESIAN_POINT ( 'NONE',  ( 83.17351638738638542, 52.27842989329151635, 14.84046717777660618 ) ) ;
#9630 = DIRECTION ( 'NONE',  ( -0.2877784213863818774, 0.9576970189910596343, 0.000000000000000000 ) ) ;
#9631 = DIRECTION ( 'NONE',  ( 1.000000000000000000, 0.000000000000000000, -0.000000000000000000 ) ) ;
#9632 = ORIENTED_EDGE ( 'NONE', *, *, #59835, .F. ) ;
#9633 = EDGE_CURVE ( 'NONE', #55257, #35007, #54297, .T. ) ;
#9634 = CIRCLE ( 'NONE', #50045, 17.82106496071138224 ) ;
#9635 = EDGE_CURVE ( 'NONE', #23644, #68477, #83789, .T. ) ;
#9636 = CARTESIAN_POINT ( 'NONE',  ( 72.40162949255979186, 64.46460395437595992, -13.26410053993346416 ) ) ;
#9637 = CARTESIAN_POINT ( 'NONE',  ( 73.98409239102026902, 55.09210739743019758, 16.60304204205536394 ) ) ;
#9638 = CARTESIAN_POINT ( 'NONE',  ( 69.84221642410084030, 62.80036841173330942, -13.30700940456985037 ) ) ;
#9639 = CARTESIAN_POINT ( 'NONE',  ( 28.71959338928917305, 24.78052372038641593, -10.00000000000000355 ) ) ;
#9640 = CARTESIAN_POINT ( 'NONE',  ( 99.25420243115659957, 218.1115022471901739, -5.000000000000041744 ) ) ;
#9641 = CARTESIAN_POINT ( 'NONE',  ( 168.8294252543820448, 272.9399934659655287, 15.96329185404338524 ) ) ;
#9642 = CARTESIAN_POINT ( 'NONE',  ( 180.5963630788930061, 273.1050420172064719, 16.83617887608246022 ) ) ;
#9643 = CYLINDRICAL_SURFACE ( 'NONE', #27497, 10.00000000000001066 ) ;
#9644 = CARTESIAN_POINT ( 'NONE',  ( 188.2974456734137902, 260.8608515763677360, 2.891147047799000447 ) ) ;
#9645 = CARTESIAN_POINT ( 'NONE',  ( 195.4288765293300401, 265.1666311804774523, -7.729559632884401843 ) ) ;
#9646 = CARTESIAN_POINT ( 'NONE',  ( -2.639098984630277922, 169.2833772461660828, -9.188101187500095079 ) ) ;
#9647 = CARTESIAN_POINT ( 'NONE',  ( 82.28096079332273405, 48.10700144346920837, 12.86989513579583999 ) ) ;
#9648 = VERTEX_POINT ( 'NONE', #47008 ) ;
#9649 = CARTESIAN_POINT ( 'NONE',  ( 161.2566224172725242, 253.0718664474237869, -14.99040694173076993 ) ) ;
#9650 = DIRECTION ( 'NONE',  ( -0.9932214622066116716, 0.1162373735601425623, 0.000000000000000000 ) ) ;
#9651 = DIRECTION ( 'NONE',  ( -0.7162481363636752363, 0.000000000000000000, -0.6978456900745050318 ) ) ;
#9652 = CARTESIAN_POINT ( 'NONE',  ( 71.94509386275791485, 72.64380087153907084, -0.7818115889975479904 ) ) ;
#9653 = CARTESIAN_POINT ( 'NONE',  ( 24.04513522159523475, 190.8149278399161233, 9.188101187500093303 ) ) ;
#9654 = DIRECTION ( 'NONE',  ( -0.8756465943326132706, -0.4829524219151362097, 0.000000000000000000 ) ) ;
#9655 = CARTESIAN_POINT ( 'NONE',  ( 31.97641226934276659, 34.16454794089043645, -10.00000000000000355 ) ) ;
#9656 = CARTESIAN_POINT ( 'NONE',  ( 178.5176923076055573, 291.6601484728420814, 5.967418820694346593 ) ) ;
#9657 = CARTESIAN_POINT ( 'NONE',  ( 196.3455846056825465, 290.5664669515812761, 16.75698796588176265 ) ) ;
#9658 = CARTESIAN_POINT ( 'NONE',  ( 133.4825598088814047, 236.3262482093457493, 3.021315404115420679E-15 ) ) ;
#9659 = CARTESIAN_POINT ( 'NONE',  ( 168.3557124657904467, 273.6222795104500278, 17.14480014634877136 ) ) ;
#9660 = CARTESIAN_POINT ( 'NONE',  ( 187.2709071308663056, 296.1806672229488413, -7.704019758776238902 ) ) ;
#9661 = CARTESIAN_POINT ( 'NONE',  ( 83.55704177478077099, 51.98730140788479304, 15.00998877770037865 ) ) ;
#9663 =( BOUNDED_CURVE ( )  B_SPLINE_CURVE ( 2, ( #96251, #42980, #72941, #74925, #57196, #73918, #4011, #5507, #34894 ),
 .UNSPECIFIED., .F., .T. ) 
 B_SPLINE_CURVE_WITH_KNOTS ( ( 3, 2, 2, 2, 3 ),
 ( 0.5362903225806451291, 0.5376344086021505042, 0.5403225806451612545, 0.5430107526881720048, 0.5443548387096773800 ),
 .UNSPECIFIED. ) 
 CURVE ( )  GEOMETRIC_REPRESENTATION_ITEM ( )  RATIONAL_B_SPLINE_CURVE ( ( 0.9330127018922194093, 0.9330127018922194093, 1.000000000000000000, 0.8660254037844387076, 1.000000000000000000, 0.8660254037844387076, 1.000000000000000000, 0.9330127018922194093, 0.9330127018922194093 ) ) 
 REPRESENTATION_ITEM ( '' )  );
#9662 = CARTESIAN_POINT ( 'NONE',  ( 65.47921168356343458, 208.6115022471902307, 10.00000000000009592 ) ) ;
#9664 = CARTESIAN_POINT ( 'NONE',  ( 165.2807093860638474, 245.9288570166273473, 0.7599370718198323882 ) ) ;
#9665 = CARTESIAN_POINT ( 'NONE',  ( 189.6738045434663320, 300.1223289962524063, 4.832295392723879424 ) ) ;
#9666 = DIRECTION ( 'NONE',  ( -0.000000000000000000, -0.000000000000000000, -1.000000000000000000 ) ) ;
#9667 = CARTESIAN_POINT ( 'NONE',  ( 33.92367135321775606, 181.2048013555409796, 4.594050593750051981 ) ) ;
#9668 = FACE_OUTER_BOUND ( 'NONE', #5609, .T. ) ;
#9669 = EDGE_CURVE ( 'NONE', #18151, #99635, #53663, .T. ) ;
#9670 = CARTESIAN_POINT ( 'NONE',  ( 66.70608100559137199, 215.9865022471902876, -10.00000000000009592 ) ) ;
#9671 = CARTESIAN_POINT ( 'NONE',  ( 205.7230952882032966, 269.3306732399635735, -3.168671107954665445 ) ) ;
#9672 = CARTESIAN_POINT ( 'NONE',  ( 67.11050834814496113, 66.80207709080652023, -9.015407947737315908 ) ) ;
#9673 = ORIENTED_EDGE ( 'NONE', *, *, #38121, .T. ) ;
#9674 = PLANE ( 'NONE',  #45900 ) ;
#9675 = CARTESIAN_POINT ( 'NONE',  ( 168.0327857633167241, 281.9162007134196415, -10.99116794043863976 ) ) ;
#9676 = CARTESIAN_POINT ( 'NONE',  ( 50.34596055286379368, 92.70800680107760172, -10.00000000000000000 ) ) ;
#9677 = CARTESIAN_POINT ( 'NONE',  ( 205.6976855946065825, 269.4214810134713503, -1.331547403361390325 ) ) ;
#9678 = CARTESIAN_POINT ( 'NONE',  ( 25.58005199048888656, 32.95586893147756768, 7.433330006724141015 ) ) ;
#9679 = CARTESIAN_POINT ( 'NONE',  ( 163.0309151244508712, 248.2691671304387739, 11.27270415168660200 ) ) ;
#9680 = CARTESIAN_POINT ( 'NONE',  ( 149.6564118588553924, 271.4344863124460971, -11.76165597393390172 ) ) ;
#9681 = CARTESIAN_POINT ( 'NONE',  ( 188.6600893746942802, 269.8527292173970409, -14.07731609263537997 ) ) ;
#9682 = ORIENTED_EDGE ( 'NONE', *, *, #87329, .F. ) ;
#9683 = CARTESIAN_POINT ( 'NONE',  ( 14.28983037092611319, 10.11110640527290627, -2.839279412974138328 ) ) ;
#9684 = CARTESIAN_POINT ( 'NONE',  ( 41.10966550219798421, 207.8207943907112565, -18.47570218321542868 ) ) ;
#9685 = CARTESIAN_POINT ( 'NONE',  ( 79.53422710701454434, 57.48121895429935080, -16.24767348339593553 ) ) ;
#9686 = DIRECTION ( 'NONE',  ( -0.9999580202055560196, -0.009162850352621043637, 0.000000000000000000 ) ) ;
#9687 = ORIENTED_EDGE ( 'NONE', *, *, #57791, .T. ) ;
#9688 = CARTESIAN_POINT ( 'NONE',  ( 72.21207746560659757, 71.58261399135965064, -5.866756630810175288 ) ) ;
#9689 = CARTESIAN_POINT ( 'NONE',  ( 82.87596643829704135, 41.15858874971023340, 0.1873015203630768732 ) ) ;
#9690 = DIRECTION ( 'NONE',  ( -0.000000000000000000, 0.000000000000000000, 1.000000000000000000 ) ) ;
#9691 = CARTESIAN_POINT ( 'NONE',  ( 190.6661865267473104, 300.4034729807058852, 4.523489664447863490 ) ) ;
#9692 = VERTEX_POINT ( 'NONE', #10518 ) ;
#9693 = CIRCLE ( 'NONE', #12956, 14.99999999999967493 ) ;
#9694 = ORIENTED_EDGE ( 'NONE', *, *, #52208, .T. ) ;
#9696 = CARTESIAN_POINT ( 'NONE',  ( 87.45625938901056884, 43.68296694889340870, -0.2840587573061720827 ) ) ;
#9695 = FACE_OUTER_BOUND ( 'NONE', #11570, .T. ) ;
#9697 = ORIENTED_EDGE ( 'NONE', *, *, #61318, .T. ) ;
#9698 = CARTESIAN_POINT ( 'NONE',  ( 43.28410984748890655, 30.15404122711137447, 8.090169943749479842 ) ) ;
#9699 = DIRECTION ( 'NONE',  ( 0.8660254037844373753, 0.5000000000000021094, 0.000000000000000000 ) ) ;
#9700 = CARTESIAN_POINT ( 'NONE',  ( 72.60665278519202559, 57.41384979935430977, -16.32120458462707546 ) ) ;
#9701 = CARTESIAN_POINT ( 'NONE',  ( 76.62156306105930526, 63.43458379359962152, 15.37592086074861619 ) ) ;
#9702 = CARTESIAN_POINT ( 'NONE',  ( 168.5910505471324257, 286.4687829538495976, 8.106709794022206594 ) ) ;
#9704 = ADVANCED_FACE ( 'NONE', ( #88076 ), #72337, .T. ) ;
#9703 = CARTESIAN_POINT ( 'NONE',  ( 102.2314250767153538, 220.6423013555409796, -4.594050593750043987 ) ) ;
#9705 = CARTESIAN_POINT ( 'NONE',  ( 196.2379679265050925, 290.7528645076583871, -16.93678934971137906 ) ) ;
#9706 = VECTOR ( 'NONE', #58487, 1000.000000000000114 ) ;
#9707 = CARTESIAN_POINT ( 'NONE',  ( -19.69918098444705379, 92.93090374423474032, 59.99999999999999289 ) ) ;
#9708 = ORIENTED_EDGE ( 'NONE', *, *, #66888, .T. ) ;
#9709 = CARTESIAN_POINT ( 'NONE',  ( 164.2647213391612979, 246.1321520798662164, -5.830872732487307530 ) ) ;
#9710 = EDGE_LOOP ( 'NONE', ( #48029, #67394 ) ) ;
#9711 = CARTESIAN_POINT ( 'NONE',  ( 35.44910642356613550, 21.26216523072496045, -2.296566073217252530E-15 ) ) ;
#9712 = CARTESIAN_POINT ( 'NONE',  ( 198.0006249058153003, 287.6998530631771587, 18.31850453277666801 ) ) ;
#9713 = CARTESIAN_POINT ( 'NONE',  ( 71.34900412968279682, 70.70430146466247834, -6.675603849584609506 ) ) ;
#9715 = VECTOR ( 'NONE', #15201, 1000.000000000000000 ) ;
#9714 = CARTESIAN_POINT ( 'NONE',  ( 56.95444766116892055, 197.5643266524159856, -9.188101187500093303 ) ) ;
#9716 = EDGE_CURVE ( 'NONE', #68082, #24137, #40048, .T. ) ;
#9717 = CARTESIAN_POINT ( 'NONE',  ( 74.39841895140679640, 68.21392270468032848, 11.45628786500076046 ) ) ;
#9718 = CARTESIAN_POINT ( 'NONE',  ( 190.8001679306945277, 300.1714103817999444, 7.815449226872675403 ) ) ;
#9719 = CARTESIAN_POINT ( 'NONE',  ( 150.2452556859942376, 270.4145788861182496, 14.49525683977126533 ) ) ;
#9720 = CARTESIAN_POINT ( 'NONE',  ( 175.1864013481757354, 272.4254438080928935, 16.55480563948633943 ) ) ;
#9721 = ADVANCED_FACE ( 'NONE', ( #88573 ), #27218, .T. ) ;
#9722 = VERTEX_POINT ( 'NONE', #3432 ) ;
#9723 = DIRECTION ( 'NONE',  ( 0.9981280818701453450, 0.06115825522547521653, 0.000000000000000000 ) ) ;
#9724 = CARTESIAN_POINT ( 'NONE',  ( 85.13042836612673625, 43.09392175677057679, -4.294211889271497995 ) ) ;
#9725 = CARTESIAN_POINT ( 'NONE',  ( 57.60966550219797000, 179.2419560658249225, 17.47570218321536117 ) ) ;
#9726 = LINE ( 'NONE', #26408, #72316 ) ;
#9727 = ORIENTED_EDGE ( 'NONE', *, *, #7528, .T. ) ;
#9728 = CARTESIAN_POINT ( 'NONE',  ( 175.4002342268021835, 261.2927254388914662, -14.34716763164142783 ) ) ;
#9729 = CARTESIAN_POINT ( 'NONE',  ( 71.49202448901485241, 69.85859178648415480, -7.429879959600643069 ) ) ;
#9730 = B_SPLINE_CURVE_WITH_KNOTS ( 'NONE', 3,
 ( #7014, #82581, #53605, #68312 ),
 .UNSPECIFIED., .F., .F.,
 ( 4, 4 ),
 ( 0.002571105401923278258, 0.005038221485946379335 ),
 .UNSPECIFIED. ) ;
#9731 = CARTESIAN_POINT ( 'NONE',  ( 146.5088695963383429, 276.8861894300958966, 0.09882562957467418141 ) ) ;
#9732 = CARTESIAN_POINT ( 'NONE',  ( 146.7944005049231180, 276.3916353892955726, -4.243051111306586520 ) ) ;
#9733 = CARTESIAN_POINT ( 'NONE',  ( 190.7222376050763444, 300.3063896652212179, 3.365789908110941475 ) ) ;
#9734 = CARTESIAN_POINT ( 'NONE',  ( 178.5543832690894703, 270.1946074348090292, 16.14052137089361949 ) ) ;
#9735 = CARTESIAN_POINT ( 'NONE',  ( 66.36268096397610350, 69.44190093015801324, 9.875986171954755521E-07 ) ) ;
#9736 = CARTESIAN_POINT ( 'NONE',  ( 67.37958206400872996, 66.94879931957503061, 9.026884747259803277 ) ) ;
#9737 = CARTESIAN_POINT ( 'NONE',  ( 154.4594390210350809, 264.0928981614183044, -16.94021933189004514 ) ) ;
#9738 = DIRECTION ( 'NONE',  ( 1.000000000000000000, 0.000000000000000000, 0.000000000000000000 ) ) ;
#9739 = CARTESIAN_POINT ( 'NONE',  ( 111.1617914095948692, 244.1744531367911293, 4.594050593750047540 ) ) ;
#9740 = ORIENTED_EDGE ( 'NONE', *, *, #66562, .F. ) ;
#9741 = CARTESIAN_POINT ( 'NONE',  ( 146.7373254022577100, 276.4904923669593586, -0.7242168585908188572 ) ) ;
#9742 = CARTESIAN_POINT ( 'NONE',  ( 82.06353261700769508, 41.00057011406286733, -2.892018250819532454 ) ) ;
#9743 = CARTESIAN_POINT ( 'NONE',  ( 203.3740894404336927, 278.3927394765486838, -15.19753795879846869 ) ) ;
#9744 = DIRECTION ( 'NONE',  ( 0.5000000000000004441, -0.8660254037844383745, -0.000000000000000000 ) ) ;
#9745 = CARTESIAN_POINT ( 'NONE',  ( 83.72112933957373571, 51.48465111928251048, -14.37122866580464198 ) ) ;
#9746 = CARTESIAN_POINT ( 'NONE',  ( 175.6023453674955022, 252.6114453084666991, 5.260320833529300799 ) ) ;
#9747 = ORIENTED_EDGE ( 'NONE', *, *, #27443, .T. ) ;
#9748 = CARTESIAN_POINT ( 'NONE',  ( 80.60151911206874331, 57.21366011616830605, -16.23031521152326206 ) ) ;
#9749 = ADVANCED_FACE ( 'NONE', ( #58583 ), #19135, .F. ) ;
#9750 = CARTESIAN_POINT ( 'NONE',  ( 158.4848075976798327, 275.1236941057235299, -12.43667617850595875 ) ) ;
#9751 = CARTESIAN_POINT ( 'NONE',  ( 185.8714895211756755, 261.7232839879937956, 10.07181324648456311 ) ) ;
#9752 = FACE_OUTER_BOUND ( 'NONE', #12412, .T. ) ;
#9753 = CARTESIAN_POINT ( 'NONE',  ( 198.5201458116119397, 286.8000164587433005, -18.30276554821096013 ) ) ;
#9754 = CARTESIAN_POINT ( 'NONE',  ( 185.5176298084847417, 297.3635137698159383, 4.083851266084445264 ) ) ;
#9755 = DIRECTION ( 'NONE',  ( -0.5000000000000014433, 0.8660254037844377084, 0.000000000000000000 ) ) ;
#9756 = CARTESIAN_POINT ( 'NONE',  ( 60.33744616864313315, 196.4548013555410080, -4.594050593750042211 ) ) ;
#9757 = CARTESIAN_POINT ( 'NONE',  ( 85.44302523967576235, 48.29274922941779380, -11.75060226479814318 ) ) ;
#9758 = DIRECTION ( 'NONE',  ( -0.8660254037844378194, -0.5000000000000014433, -0.000000000000000000 ) ) ;
#9759 = EDGE_CURVE ( 'NONE', #12458, #43772, #86395, .T. ) ;
#9760 = CARTESIAN_POINT ( 'NONE',  ( 171.8127856075278430, 259.9554699241354569, 15.47650383583072653 ) ) ;
#9761 = CARTESIAN_POINT ( 'NONE',  ( 81.64018326908548318, 41.60497881960491640, 5.570940999012380601 ) ) ;
#9762 = CARTESIAN_POINT ( 'NONE',  ( 88.33748333995926316, 44.07075497373335793, -2.898134731201826852 ) ) ;
#9763 = FACE_OUTER_BOUND ( 'NONE', #60638, .T. ) ;
#9764 = CARTESIAN_POINT ( 'NONE',  ( 157.2286243502475429, 270.8137009750436732, -14.73200381606329223 ) ) ;
#9765 = CARTESIAN_POINT ( 'NONE',  ( 126.8768043691498377, 237.3927522451418213, 10.00000000000009592 ) ) ;
#9766 = B_SPLINE_SURFACE_WITH_KNOTS ( 'NONE', 3, 1, ( 
 ( #94632, #2927 ),
 ( #12381, #9512 ),
 ( #79939, #40376 ),
 ( #26203, #72322 ),
 ( #71817, #48505 ),
 ( #20480, #10498 ),
 ( #57082, #79443 ),
 ( #32788, #18103 ),
 ( #56071, #82319 ),
 ( #5269, #10008 ),
 ( #74691, #40871 ),
 ( #43247, #64194 ),
 ( #28551, #47980 ),
 ( #49005, #78925 ),
 ( #41382, #33817 ),
 ( #64704, #4781 ),
 ( #66564, #97491 ),
 ( #28056, #58931 ),
 ( #51353, #12890 ),
 ( #43747, #36148 ),
 ( #67052, #97975 ),
 ( #75669, #29074 ),
 ( #68051, #22939 ),
 ( #68545, #6757 ),
 ( #38640, #98973 ),
 ( #90911, #91388 ),
 ( #22450, #21950 ),
 ( #82808, #99471 ),
 ( #99970, #92392 ),
 ( #29558, #152 ),
 ( #53828, #98483 ),
 ( #61438, #83292 ),
 ( #84788, #60431 ),
 ( #37151, #61928 ) ),
 .UNSPECIFIED., .T., .F., .F.,
 ( 4, 2, 2, 2, 2, 2, 2, 2, 2, 2, 2, 2, 2, 2, 2, 2, 4 ),
 ( 2, 2 ),
 ( 0.000000000000000000, 0.06250000000000000000, 0.1250000000000000000, 0.1875000000000000000, 0.2500000000000000000, 0.3125000000000000000, 0.3750000000000000000, 0.4375000000000000000, 0.5000000000000000000, 0.5625000000000000000, 0.6250000000000000000, 0.6875000000000000000, 0.7500000000000000000, 0.8125000000000000000, 0.8750000000000000000, 0.9375000000000000000, 1.000000000000000000 ),
 ( 0.000000000000000000, 1.000000000000000000 ),
 .UNSPECIFIED. ) ;
#9767 = CARTESIAN_POINT ( 'NONE',  ( 76.51423634175225175, 53.18905479164092043, -15.93784919710639691 ) ) ;
#9768 = ORIENTED_EDGE ( 'NONE', *, *, #82806, .T. ) ;
#9769 = CARTESIAN_POINT ( 'NONE',  ( 163.4004183463084416, 247.6291687766210146, 10.19167732382099345 ) ) ;
#9770 = CARTESIAN_POINT ( 'NONE',  ( 87.51647913336857698, 44.56403561216112053, 4.883618514853080406 ) ) ;
#9771 = CARTESIAN_POINT ( 'NONE',  ( 49.16021902710897251, 193.0643266524159856, -9.188101187500093303 ) ) ;
#9772 = CARTESIAN_POINT ( 'NONE',  ( 11.36960171514096452, 30.65659080271450065, -1.878358725466461243E-16 ) ) ;
#9773 = CARTESIAN_POINT ( 'NONE',  ( -48.41313092940755070, 109.7198701005979302, -10.00000000000000000 ) ) ;
#9774 = LINE ( 'NONE', #48253, #45224 ) ;
#9775 = CARTESIAN_POINT ( 'NONE',  ( 177.1262862392189845, 269.6057104283654553, 17.56656865388298172 ) ) ;
#9776 = CARTESIAN_POINT ( 'NONE',  ( 66.45568218898124258, 67.84274271466240691, -6.745522493097580785 ) ) ;
#9778 = CARTESIAN_POINT ( 'NONE',  ( 58.31645990288169656, 211.1427522451419065, 10.00000000000009237 ) ) ;
#9777 = CARTESIAN_POINT ( 'NONE',  ( 1.830000459568766003, 24.55466486950697202, 1.000260061240931054E-15 ) ) ;
#9779 = CARTESIAN_POINT ( 'NONE',  ( 171.6130448281033125, 286.7680181827872730, 7.456980690989077232 ) ) ;
#9780 = CARTESIAN_POINT ( 'NONE',  ( 183.3475561009241233, 257.5467204516681363, 1.327541498361791694 ) ) ;
#9781 = CARTESIAN_POINT ( 'NONE',  ( 204.9658583905037688, 275.6357147811169170, -12.57240504404813564 ) ) ;
#9782 = CARTESIAN_POINT ( 'NONE',  ( -27.42236680055714260, 166.5217562850347406, 1.224646799147364892E-15 ) ) ;
#9783 = ORIENTED_EDGE ( 'NONE', *, *, #46979, .F. ) ;
#9784 = ADVANCED_FACE ( 'NONE', ( #35799 ), #36291, .T. ) ;
#9785 = CARTESIAN_POINT ( 'NONE',  ( 161.8086887434684797, 267.2572688397011689, 16.48344843794798820 ) ) ;
#9786 = CARTESIAN_POINT ( 'NONE',  ( 24.41517378745133371, 178.2365022471902307, 10.00000000000009592 ) ) ;
#9787 = CARTESIAN_POINT ( 'NONE',  ( 198.2505066714982149, 285.2670451491296149, 0.000000000000000000 ) ) ;
#9788 = CARTESIAN_POINT ( 'NONE',  ( -169.5327448629461742, 46.94652375874896677, 30.52142883766498827 ) ) ;
#9789 = CARTESIAN_POINT ( 'NONE',  ( -13.19395714113563045, 169.3149278399160949, -9.188101187500095079 ) ) ;
#9790 = CARTESIAN_POINT ( 'NONE',  ( 41.95273645663377238, 27.14754757982093381, -5.678558825948276656 ) ) ;
#9792 = EDGE_CURVE ( 'NONE', #39443, #96352, #19062, .T. ) ;
#9791 = CARTESIAN_POINT ( 'NONE',  ( 170.2708277436370565, 263.6177537115055429, 15.82973544656882403 ) ) ;
#9793 = CARTESIAN_POINT ( 'NONE',  ( 33.17822050123679389, 178.4155109091895781, 2.679491924311254714 ) ) ;
#9794 = CARTESIAN_POINT ( 'NONE',  ( 35.39919958817179690, 22.29860640527294535, -2.839279412974138328 ) ) ;
#9795 = CARTESIAN_POINT ( 'NONE',  ( 206.3505875407052486, 273.2372935382459787, 11.62318091048137880 ) ) ;
#9796 = CARTESIAN_POINT ( 'NONE',  ( 183.1752028583183574, 257.7612102956644549, -2.166713690560386762 ) ) ;
#9797 = CARTESIAN_POINT ( 'NONE',  ( 66.04046446033240159, 68.57277501975208622, 1.949611298710725915 ) ) ;
#9798 = VERTEX_POINT ( 'NONE', #51495 ) ;
#9799 = CARTESIAN_POINT ( 'NONE',  ( 80.66987298107778770, 24.99999999999998579, 10.00000000000000178 ) ) ;
#9800 = CARTESIAN_POINT ( 'NONE',  ( 150.1530336415601710, 271.4893706449333877, -12.31841913146343082 ) ) ;
#9801 = SHAPE_REPRESENTATION_RELATIONSHIP ( 'NONE' , 'NONE' ,  #87244, #17532 ) ;
#9802 = CARTESIAN_POINT ( 'NONE',  ( 6.007877864960585512, 21.65586893147753855, -7.433330006724137462 ) ) ;
#9803 = CARTESIAN_POINT ( 'NONE',  ( 168.3660592861385226, 287.3002883228049313, 0.5084154714863498015 ) ) ;
#9804 = CARTESIAN_POINT ( 'NONE',  ( 17.52000153575897912, 22.06628583063841020, -9.188101187500006262 ) ) ;
#9805 = CARTESIAN_POINT ( 'NONE',  ( 207.2299632185859650, 271.7141701852165738, 8.357384014234831682 ) ) ;
#9806 = CARTESIAN_POINT ( 'NONE',  ( 84.63209989742584582, 49.90680382888324118, -13.65945482025744795 ) ) ;
#9807 = CARTESIAN_POINT ( 'NONE',  ( 159.2536436069973718, 254.8115933126508992, -15.76697951715411250 ) ) ;
#9808 = CARTESIAN_POINT ( 'NONE',  ( 63.45052750612631343, 195.8932355074535678, -2.679491924311248496 ) ) ;
#9809 = ORIENTED_EDGE ( 'NONE', *, *, #4460, .T. ) ;
#9810 = CARTESIAN_POINT ( 'NONE',  ( 29.85625172820832418, 25.43677371833803136, -10.00000000000000355 ) ) ;
#9811 = CARTESIAN_POINT ( 'NONE',  ( 207.5338226493333025, 271.1878702128032614, 6.432541580693135863 ) ) ;
#9812 = CARTESIAN_POINT ( 'NONE',  ( 104.0173421519710217, 220.8615022471902023, 5.000000000000051514 ) ) ;
#9813 = CARTESIAN_POINT ( 'NONE',  ( 87.87588256303088485, 45.05834245088314560, 6.537532970176366476 ) ) ;
#9814 = LINE ( 'NONE', #47768, #90489 ) ;
#9815 = VERTEX_POINT ( 'NONE', #59577 ) ;
#9816 = EDGE_LOOP ( 'NONE', ( #49184, #3581, #17309, #59304 ) ) ;
#9817 = CARTESIAN_POINT ( 'NONE',  ( 86.10128179547638183, 47.01522930412664181, 10.71950609365847384 ) ) ;
#9818 = CARTESIAN_POINT ( 'NONE',  ( 86.02805406347464157, 47.65264056766959300, 10.87896026205523370 ) ) ;
#9819 = ORIENTED_EDGE ( 'NONE', *, *, #4205, .F. ) ;
#9820 = CARTESIAN_POINT ( 'NONE',  ( 78.12080843744404035, 59.88224619964616835, 16.03904967186319297 ) ) ;
#9821 = CARTESIAN_POINT ( 'NONE',  ( 188.9790587790324992, 297.2113717040124925, 7.911450463245256692 ) ) ;
#9822 = ORIENTED_EDGE ( 'NONE', *, *, #94621, .T. ) ;
#9823 = CARTESIAN_POINT ( 'NONE',  ( 5.968649350820482979, 188.6868197944959320, -37.49999999999994316 ) ) ;
#9824 = CARTESIAN_POINT ( 'NONE',  ( 79.18684305567126103, 59.44391592844134919, -16.53590917749602340 ) ) ;
#9825 = CARTESIAN_POINT ( 'NONE',  ( 12.38042018312781067, 30.08080186712591697, -3.090169943749475845 ) ) ;
#9826 = ORIENTED_EDGE ( 'NONE', *, *, #15394, .F. ) ;
#9827 = CARTESIAN_POINT ( 'NONE',  ( 175.0917972779528213, 268.1668903562270430, 16.25173907998583900 ) ) ;
#9828 = CARTESIAN_POINT ( 'NONE',  ( -35.89898968889472997, 24.97633462685643124, 10.00000000000000000 ) ) ;
#9829 = CARTESIAN_POINT ( 'NONE',  ( 151.4361976351029000, 268.3518069213970421, 15.15218985681980612 ) ) ;
#9830 = CARTESIAN_POINT ( 'NONE',  ( 149.0959704726320751, 273.8919761871559331, -8.765438422576197652 ) ) ;
#9831 = ORIENTED_EDGE ( 'NONE', *, *, #57284, .F. ) ;
#9832 = CARTESIAN_POINT ( 'NONE',  ( 173.4125187911463684, 257.0454188278081915, -11.72670941500022757 ) ) ;
#9833 = CARTESIAN_POINT ( 'NONE',  ( 202.9685995779611858, 279.0950685203052899, 16.84977534244423580 ) ) ;
#9834 = ORIENTED_EDGE ( 'NONE', *, *, #89614, .T. ) ;
#9835 = EDGE_CURVE ( 'NONE', #43311, #42198, #51341, .T. ) ;
#9836 = ORIENTED_EDGE ( 'NONE', *, *, #78555, .T. ) ;
#9837 = DIRECTION ( 'NONE',  ( 0.000000000000000000, 0.000000000000000000, 1.000000000000000000 ) ) ;
#9838 = VERTEX_POINT ( 'NONE', #75819 ) ;
#9839 = EDGE_CURVE ( 'NONE', #38656, #89858, #78934, .T. ) ;
#9840 = CARTESIAN_POINT ( 'NONE',  ( 161.1595886466168679, 271.1349891283304601, 16.19772519489564999 ) ) ;
#9841 = ORIENTED_EDGE ( 'NONE', *, *, #23026, .T. ) ;
#9842 = CARTESIAN_POINT ( 'NONE',  ( 83.70835292455117838, 51.17077017971526232, 14.19597355579030484 ) ) ;
#9843 = EDGE_CURVE ( 'NONE', #80773, #11356, #20614, .T. ) ;
#9844 = CARTESIAN_POINT ( 'NONE',  ( -13.11024591527734628, 6.000000000000000000, -32.50000000000000000 ) ) ;
#9845 = CARTESIAN_POINT ( 'NONE',  ( 69.13686587061594935, 64.31895405193962745, 11.99662287724232357 ) ) ;
#9846 = EDGE_CURVE ( 'NONE', #33352, #92124, #99612, .T. ) ;
#9847 = CARTESIAN_POINT ( 'NONE',  ( -50.34886203176066033, 29.86533669878861375, 10.00000000000000000 ) ) ;
#9848 = B_SPLINE_CURVE_WITH_KNOTS ( 'NONE', 3,
 ( #75280, #83395, #67658, #12992, #66661, #74301, #81907, #37250, #42840, #89524, #51460, #5864, #36253, #59538, #52450, #28163, #36749, #97116, #19601, #5370, #98588, #4883, #27181, #35765, #89051, #29171, #67156, #59033, #90004, #58068, #75780, #13478, #20085, #98077, #91005, #44349, #81411, #60039, #73778, #28655, #20579, #43851, #21567, #90517, #82426, #68149, #74792, #50461, #11984, #44843 ),
 .UNSPECIFIED., .F., .F.,
 ( 4, 2, 2, 2, 2, 2, 2, 2, 2, 2, 2, 2, 2, 2, 2, 2, 2, 2, 2, 2, 2, 2, 2, 2, 4 ),
 ( 0.0005508003809566546210, 0.0009892564418127341736, 0.001208484472240721041, 0.001318098487454664276, 0.001427712502668604042, 0.001537326517882543807, 0.001646940533096483356, 0.001866168563524404521, 0.002304624624380174208, 0.003181536746091786876, 0.004058448867803400410, 0.004935360989515013945, 0.005373817050370783416, 0.005593045080798705014, 0.005702659096012628950, 0.005757466103619628649, 0.005812273111226628347, 0.005867080118833628913, 0.005921887126440628611, 0.006031501141654588109, 0.006250729172082574760, 0.006689185232938636531, 0.007127641293794699170, 0.007346869324222742199, 0.007566097354650785228 ),
 .UNSPECIFIED. ) ;
#9849 = CARTESIAN_POINT ( 'NONE',  ( 174.6745456591689845, 289.9937384206305637, 6.288497583336834396 ) ) ;
#9850 = CARTESIAN_POINT ( 'NONE',  ( 154.2853090730916676, 265.4170011543745886, 17.16471700533586642 ) ) ;
#9851 = ORIENTED_EDGE ( 'NONE', *, *, #23401, .F. ) ;
#9852 = CARTESIAN_POINT ( 'NONE',  ( 169.6445766797212116, 289.2987616194045017, 1.143403053474568054 ) ) ;
#9853 = CARTESIAN_POINT ( 'NONE',  ( 21.45440292344354916, 18.10170272979926764, -7.433330006724141015 ) ) ;
#9854 = CARTESIAN_POINT ( 'NONE',  ( 191.3122624219907664, 298.1811694523752863, -9.332778507267013524 ) ) ;
#9856 = ORIENTED_EDGE ( 'NONE', *, *, #72713, .T. ) ;
#9855 = CARTESIAN_POINT ( 'NONE',  ( 198.0006249058153003, 287.6998530631771587, 18.31850453277666801 ) ) ;
#9857 = ORIENTED_EDGE ( 'NONE', *, *, #47408, .T. ) ;
#9858 = CARTESIAN_POINT ( 'NONE',  ( 147.4604237891675780, 275.2380492219603525, -3.488979611022138716 ) ) ;
#9859 = CARTESIAN_POINT ( 'NONE',  ( 168.3813732014777145, 257.2211975074816905, -14.37470435435323424 ) ) ;
#9860 = CARTESIAN_POINT ( 'NONE',  ( 159.2186641046529303, 254.8721795879351646, -15.96198087403305443 ) ) ;
#9861 = DIRECTION ( 'NONE',  ( -0.8660254037844377084, -0.5000000000000014433, -0.000000000000000000 ) ) ;
#9862 = CARTESIAN_POINT ( 'NONE',  ( 200.7079229450794173, 283.0106753079404029, 16.90512463913211505 ) ) ;
#9863 = CARTESIAN_POINT ( 'NONE',  ( 72.02064175744285990, 59.20208988331167888, 15.86477473724754184 ) ) ;
#9864 = VERTEX_POINT ( 'NONE', #30189 ) ;
#9865 = DIRECTION ( 'NONE',  ( 0.4999999999999998890, -0.8660254037844385966, 0.000000000000000000 ) ) ;
#9866 = CARTESIAN_POINT ( 'NONE',  ( 8.323093432028223049, 20.50829794293878905, -10.00000000000000355 ) ) ;
#9867 = EDGE_CURVE ( 'NONE', #34967, #85106, #91038, .T. ) ;
#9868 = FACE_OUTER_BOUND ( 'NONE', #5921, .T. ) ;
#9869 = DIRECTION ( 'NONE',  ( -1.000000000000000000, -4.892646582057337723E-14, 0.000000000000000000 ) ) ;
#9870 = CARTESIAN_POINT ( 'NONE',  ( 10.82940026203495520, 190.3927522451419634, 2.944929066748280225E-16 ) ) ;
#9871 = CARTESIAN_POINT ( 'NONE',  ( 80.33678646758374953, 223.3149278399160664, -9.188101187500095079 ) ) ;
#9872 = CARTESIAN_POINT ( 'NONE',  ( 82.11422868418486587, 40.75191158806642022, -0.7887125810678616844 ) ) ;
#9873 = CARTESIAN_POINT ( 'NONE',  ( 84.81058727987682744, 50.28540220845615494, 13.39370648373574824 ) ) ;
#9874 = CARTESIAN_POINT ( 'NONE',  ( 208.0148989748639394, 270.3546215746652592, 3.138818306258006618 ) ) ;
#9876 = FACE_OUTER_BOUND ( 'NONE', #63988, .T. ) ;
#9875 = CARTESIAN_POINT ( 'NONE',  ( 0.6624493194153854292, 177.3149278399160664, 9.188101187500093303 ) ) ;
#9877 = CARTESIAN_POINT ( 'NONE',  ( 178.7600897929267774, 254.1784503161647706, 4.743017227330367014 ) ) ;
#9878 = ORIENTED_EDGE ( 'NONE', *, *, #38578, .T. ) ;
#9880 = VERTEX_POINT ( 'NONE', #38271 ) ;
#9879 = UNCERTAINTY_MEASURE_WITH_UNIT (LENGTH_MEASURE( 1.000000000000000082E-05 ), #84711, 'distance_accuracy_value', 'NONE');
#9881 = CARTESIAN_POINT ( 'NONE',  ( 200.9077156035369001, 267.7919832835530656, -3.066172851167955127 ) ) ;
#9882 = CARTESIAN_POINT ( 'NONE',  ( 79.90694551766156906, 47.07889366225261085, -13.03716703668656685 ) ) ;
#9883 = CARTESIAN_POINT ( 'NONE',  ( 83.85717419902768199, 43.35873368085128021, 6.682989616040957870 ) ) ;
#9884 = DIRECTION ( 'NONE',  ( 0.2194785493951409983, -0.9756173257765590190, 0.000000000000000000 ) ) ;
#9885 = CARTESIAN_POINT ( 'NONE',  ( 41.54549712337441747, 24.39040679176986615, -6.890680421881970419E-14 ) ) ;
#9886 = CARTESIAN_POINT ( 'NONE',  ( 88.67874521539408761, 45.12822637883663646, 1.911324073694122932E-15 ) ) ;
#9887 = CARTESIAN_POINT ( 'NONE',  ( 30.62142885764206568, 197.6744531367911293, 4.594050593750047540 ) ) ;
#9888 = CARTESIAN_POINT ( 'NONE',  ( 92.14326550588401687, 235.5530062829863027, -4.648177544792955347E-16 ) ) ;
#9889 = ORIENTED_EDGE ( 'NONE', *, *, #15394, .T. ) ;
#9890 = CARTESIAN_POINT ( 'NONE',  ( 82.04598463251571161, 43.24397476211455427, 8.160383678059524470 ) ) ;
#9891 = CARTESIAN_POINT ( 'NONE',  ( 168.1589593212097498, 275.9390298053305628, -16.40258036402506647 ) ) ;
#9892 = ADVANCED_FACE ( 'NONE', ( #92047 ), #69182, .T. ) ;
#9893 = CARTESIAN_POINT ( 'NONE',  ( -12.86919761471646773, 169.5024278399161233, -9.188101187500093303 ) ) ;
#9894 = CARTESIAN_POINT ( 'NONE',  ( 68.85868628182136320, 64.71584314351879641, -12.20120022179425234 ) ) ;
#9895 = CARTESIAN_POINT ( 'NONE',  ( 36.25628400652970384, 53.06077264917335867, 10.00000000000000000 ) ) ;
#9896 = CARTESIAN_POINT ( 'NONE',  ( 147.9133274879049793, 274.4535970048112290, -9.359166267164972908 ) ) ;
#9897 = CARTESIAN_POINT ( 'NONE',  ( 71.71377818447290053, 68.16592558100862220, -10.55737487113105821 ) ) ;
#9898 = CARTESIAN_POINT ( 'NONE',  ( 204.5831314780710954, 276.2986172388744421, 13.28075685133257089 ) ) ;
#9899 = CARTESIAN_POINT ( 'NONE',  ( 191.7741832257749195, 298.4843664033717801, -8.615487418695501276 ) ) ;
#9900 = CARTESIAN_POINT ( 'NONE',  ( 190.5444288681022442, 300.6143634316900943, -1.000014190476072873 ) ) ;
#9901 = EDGE_LOOP ( 'NONE', ( #30638, #98275, #41587, #40548 ) ) ;
#9902 = CARTESIAN_POINT ( 'NONE',  ( 163.9910908123517288, 246.6060940548019289, -7.333295033952830444 ) ) ;
#9903 = CARTESIAN_POINT ( 'NONE',  ( 135.1739027599712131, 260.3967562850347122, -4.648177544792955347E-16 ) ) ;
#9904 = CARTESIAN_POINT ( 'NONE',  ( 118.4422513298640638, 233.0643266524159856, 9.188101187500095079 ) ) ;
#9905 = CARTESIAN_POINT ( 'NONE',  ( 23.27484393518965788, 15.29860640527292226, -2.839279412974138328 ) ) ;
#9906 = CARTESIAN_POINT ( 'NONE',  ( 75.26135223891184012, 66.78369140784673164, 12.92241541316169773 ) ) ;
#9907 = CARTESIAN_POINT ( 'NONE',  ( 48.32408078245682503, 82.80331927372955647, -10.00000000000000000 ) ) ;
#9909 = DIRECTION ( 'NONE',  ( -0.5891075386695773242, -0.8080546441192405505, 0.000000000000000000 ) ) ;
#9908 = CARTESIAN_POINT ( 'NONE',  ( 157.6335212189247557, 257.6177276032722716, 16.76495363836117036 ) ) ;
#9910 = CARTESIAN_POINT ( 'NONE',  ( 191.2176660212971626, 299.4482824768133469, -7.870254471783424854 ) ) ;
#9911 = CARTESIAN_POINT ( 'NONE',  ( 77.00910850481051284, 63.69207575539577704, -14.97815254220547487 ) ) ;
#9912 = CARTESIAN_POINT ( 'NONE',  ( 196.2878005184348353, 290.6665519265632724, -16.69183432842427806 ) ) ;
#9913 = DIRECTION ( 'NONE',  ( -0.2925570654631174383, 0.000000000000000000, -0.9562480658530030375 ) ) ;
#9914 = CARTESIAN_POINT ( 'NONE',  ( 173.3685877188761424, 289.8321177535186735, -1.072859328093765052 ) ) ;
#9915 = CARTESIAN_POINT ( 'NONE',  ( 81.45669997382150029, 55.98862135975877408, -16.04303691645969110 ) ) ;
#9916 = ORIENTED_EDGE ( 'NONE', *, *, #22330, .T. ) ;
#9917 = CARTESIAN_POINT ( 'NONE',  ( 188.9872881452310196, 265.7805097164244330, 11.31253184319408156 ) ) ;
#9918 = CARTESIAN_POINT ( 'NONE',  ( 19.85205661636063112, 27.16454794089041869, -10.00000000000000355 ) ) ;
#9919 = CARTESIAN_POINT ( 'NONE',  ( 168.8883095508243457, 271.9124168116484270, -17.04002696021108676 ) ) ;
#9920 = ORIENTED_EDGE ( 'NONE', *, *, #18204, .F. ) ;
#9921 = CARTESIAN_POINT ( 'NONE',  ( 185.2570508126727873, 282.0811717828997303, -17.42469797758589678 ) ) ;
#9922 = CARTESIAN_POINT ( 'NONE',  ( 83.90707806624753573, 51.69617421279772174, -14.41620133319961106 ) ) ;
#9923 = DIRECTION ( 'NONE',  ( 1.000000000000000000, 0.000000000000000000, 0.000000000000000000 ) ) ;
#9924 = CARTESIAN_POINT ( 'NONE',  ( 74.95533196993615377, 53.16522946876935407, -16.03279857048111978 ) ) ;
#9925 = CARTESIAN_POINT ( 'NONE',  ( 192.6773196027083372, 296.9200883123592689, 11.15745042875121484 ) ) ;
#9926 = EDGE_LOOP ( 'NONE', ( #66352, #68980, #94718, #21660 ) ) ;
#9927 = FACE_OUTER_BOUND ( 'NONE', #34276, .T. ) ;
#9928 = CARTESIAN_POINT ( 'NONE',  ( 42.23901261427005949, 30.10170272979930672, -7.433330006724141015 ) ) ;
#9929 = CARTESIAN_POINT ( 'NONE',  ( 173.7927290169602372, 272.7279150489933386, -16.36119466774314191 ) ) ;
#9930 = ORIENTED_EDGE ( 'NONE', *, *, #23524, .T. ) ;
#9931 = CARTESIAN_POINT ( 'NONE',  ( 163.7939465169801281, 279.4726423028532167, 12.28070329374801517 ) ) ;
#9932 = CARTESIAN_POINT ( 'NONE',  ( -19.65312891409034179, 93.06504152958504505, 0.000000000000000000 ) ) ;
#9933 = DIRECTION ( 'NONE',  ( -1.000000000000000000, 0.000000000000000000, 0.000000000000000000 ) ) ;
#9934 = ORIENTED_EDGE ( 'NONE', *, *, #92492, .F. ) ;
#9935 = CARTESIAN_POINT ( 'NONE',  ( 86.55406513359314147, 47.25665231443431935, -10.69898602647501562 ) ) ;
#9936 = CARTESIAN_POINT ( 'NONE',  ( 188.1760652356224739, 292.9042221405367741, 12.45412430059673170 ) ) ;
#9937 = CARTESIAN_POINT ( 'NONE',  ( 28.24009562160082609, 16.70852965304480264, 1.583844403245364907 ) ) ;
#9938 = CARTESIAN_POINT ( 'NONE',  ( 79.30008114732019919, 51.60973947141255280, -15.28311722500239966 ) ) ;
#9939 = CARTESIAN_POINT ( 'NONE',  ( 202.8874463667715133, 279.2356300052831557, -15.29930322226033468 ) ) ;
#9940 = ORIENTED_EDGE ( 'NONE', *, *, #85926, .F. ) ;
#9941 = ORIENTED_EDGE ( 'NONE', *, *, #6347, .T. ) ;
#9942 = EDGE_CURVE ( 'NONE', #59130, #95735, #36804, .T. ) ;
#9943 = CARTESIAN_POINT ( 'NONE',  ( 175.0547837195394152, 258.6252918682578752, 12.74266989511996151 ) ) ;
#9944 = ORIENTED_EDGE ( 'NONE', *, *, #80337, .F. ) ;
#9945 = CARTESIAN_POINT ( 'NONE',  ( 77.31770070113016402, 49.73547290843352897, -14.99761632544347911 ) ) ;
#9946 = ORIENTED_EDGE ( 'NONE', *, *, #31896, .T. ) ;
#9947 = EDGE_CURVE ( 'NONE', #12823, #82885, #37288, .T. ) ;
#9948 = CYLINDRICAL_SURFACE ( 'NONE', #29810, 10.00000000000010658 ) ;
#9949 = CARTESIAN_POINT ( 'NONE',  ( 79.54765903714830699, 55.27048800625036762, 16.06385255412505231 ) ) ;
#9951 = ORIENTED_EDGE ( 'NONE', *, *, #34755, .F. ) ;
#9950 =( BOUNDED_CURVE ( )  B_SPLINE_CURVE ( 2, ( #3704, #34582, #65482, #84706, #68958, #83207, #67972, #68460, #54237, #8172, #52753, #99880, #22367 ),
 .UNSPECIFIED., .F., .F. ) 
 B_SPLINE_CURVE_WITH_KNOTS ( ( 3, 2, 2, 2, 2, 2, 3 ),
 ( 0.4874999999999999889, 0.4899999999999999911, 0.4949999999999999956, 0.5000000000000000000, 0.5050000000000000044, 0.5100000000000000089, 0.5125000000000000666 ),
 .UNSPECIFIED. ) 
 CURVE ( )  GEOMETRIC_REPRESENTATION_ITEM ( )  RATIONAL_B_SPLINE_CURVE ( ( 0.9755282581475768211, 0.9755282581475768211, 1.000000000000000000, 0.9510565162951535312, 1.000000000000000000, 0.9510565162951535312, 1.000000000000000000, 0.9510565162951535312, 1.000000000000000000, 0.9510565162951535312, 1.000000000000000000, 0.9755282581475761550, 0.9755282581475767101 ) ) 
 REPRESENTATION_ITEM ( '' )  );
#9952 = CARTESIAN_POINT ( 'NONE',  ( 185.9234121912444948, 282.2675293692463470, -16.62240104205559632 ) ) ;
#9953 = CARTESIAN_POINT ( 'NONE',  ( 25.48331929688331599, 38.21091486745862653, 7.012934429366973338E-14 ) ) ;
#9954 = CARTESIAN_POINT ( 'NONE',  ( 70.62624074450191358, 71.35313954103614265, 3.953306911768213361 ) ) ;
#9955 = CARTESIAN_POINT ( 'NONE',  ( 196.0802517080272764, 284.4438967393610938, -17.76628030232408761 ) ) ;
#9956 = CARTESIAN_POINT ( 'NONE',  ( 146.9422184197532317, 276.1356072505412840, -5.063317562214876943 ) ) ;
#9957 = CARTESIAN_POINT ( 'NONE',  ( 201.1679199471075492, 282.2139371290980989, -16.62385308864941535 ) ) ;
#9958 = EDGE_CURVE ( 'NONE', #66829, #65714, #44384, .T. ) ;
#9959 = CARTESIAN_POINT ( 'NONE',  ( 157.9535068807132348, 281.0419050908307099, 2.461037685683107323 ) ) ;
#9960 = B_SPLINE_CURVE_WITH_KNOTS ( 'NONE', 3,
 ( #93625, #1405, #24193, #32285, #63188, #24686, #94627, #25184, #7482, #30799 ),
 .UNSPECIFIED., .F., .F.,
 ( 4, 2, 2, 2, 4 ),
 ( 0.000000000000000000, 0.0002622400424273497836, 0.0005244800848546995672, 0.0007867201272820493509, 0.001048960169709399134 ),
 .UNSPECIFIED. ) ;
#9961 = CARTESIAN_POINT ( 'NONE',  ( 125.9117204375048544, 237.3768266524159856, 9.188101187500098632 ) ) ;
#9962 = CARTESIAN_POINT ( 'NONE',  ( 70.65498028500805106, 61.41543102928405062, -14.81213469601333266 ) ) ;
#9963 = ORIENTED_EDGE ( 'NONE', *, *, #29406, .T. ) ;
#9965 = ORIENTED_EDGE ( 'NONE', *, *, #66203, .F. ) ;
#9964 = CARTESIAN_POINT ( 'NONE',  ( 85.74281436412356072, 48.57633205417285893, -12.30481470458759219 ) ) ;
#9966 = CARTESIAN_POINT ( 'NONE',  ( 203.5888783976779735, 276.1984687194538424, 13.33151786231322156 ) ) ;
#9967 = CARTESIAN_POINT ( 'NONE',  ( 172.5942616442810333, 282.2509914604344203, 14.60726632573390305 ) ) ;
#9968 = CARTESIAN_POINT ( 'NONE',  ( 173.1155682512793419, 289.1052356982697233, -4.667333446098393068 ) ) ;
#9969 = CARTESIAN_POINT ( 'NONE',  ( 146.7466845547833429, 276.4742818392692243, 3.855766036253278184 ) ) ;
#9970 = CARTESIAN_POINT ( 'NONE',  ( 73.05415939173641959, 65.68351150362803992, 12.75436733280234236 ) ) ;
#9971 = DIRECTION ( 'NONE',  ( 1.000000000000000000, 0.000000000000000000, 0.000000000000000000 ) ) ;
#9972 = CARTESIAN_POINT ( 'NONE',  ( 78.30344819242883148, 51.70502438984931359, 15.92195105728979421 ) ) ;
#9973 =( BOUNDED_CURVE ( )  B_SPLINE_CURVE ( 2, ( #34232, #49425, #17018, #79876, #71751, #71247, #65620, #10948, #41818 ),
 .UNSPECIFIED., .F., .T. ) 
 B_SPLINE_CURVE_WITH_KNOTS ( ( 3, 2, 2, 2, 3 ),
 ( 0.6975806451612903691, 0.6989247311827957443, 0.7016129032258064946, 0.7043010752688172449, 0.7056451612903226200 ),
 .UNSPECIFIED. ) 
 CURVE ( )  GEOMETRIC_REPRESENTATION_ITEM ( )  RATIONAL_B_SPLINE_CURVE ( ( 0.9330127018922194093, 0.9330127018922194093, 1.000000000000000000, 0.8660254037844387076, 1.000000000000000000, 0.8660254037844387076, 1.000000000000000000, 0.9330127018922194093, 0.9330127018922194093 ) ) 
 REPRESENTATION_ITEM ( '' )  );
#9974 = CARTESIAN_POINT ( 'NONE',  ( 9.911560002841389050, 164.9824982072973967, 3.021315404115420679E-15 ) ) ;
#9975 = VECTOR ( 'NONE', #45768, 1000.000000000000000 ) ;
#9976 = CARTESIAN_POINT ( 'NONE',  ( 177.1886485508865974, 256.0379014559142092, -7.297321842872941389 ) ) ;
#9977 = ORIENTED_EDGE ( 'NONE', *, *, #39458, .F. ) ;
#9978 = LINE ( 'NONE', #93086, #65565 ) ;
#9979 = CARTESIAN_POINT ( 'NONE',  ( 196.3249884498792994, 275.2518087180711177, 16.06659936265807431 ) ) ;
#9980 = EDGE_LOOP ( 'NONE', ( #28608, #77947, #56522 ) ) ;
#9981 = FACE_OUTER_BOUND ( 'NONE', #79409, .T. ) ;
#9982 = CARTESIAN_POINT ( 'NONE',  ( 157.6514191749160716, 276.9937859392390465, 10.24612596229098038 ) ) ;
#9983 = CARTESIAN_POINT ( 'NONE',  ( 151.8090328414793930, 267.7060374011022077, -15.68750330915316660 ) ) ;
#9984 = CARTESIAN_POINT ( 'NONE',  ( 149.1856130393175306, 272.2499337880290682, 11.44243872309708188 ) ) ;
#9985 = CARTESIAN_POINT ( 'NONE',  ( 163.3543347837650686, 247.7089878483399730, 10.92686688779373405 ) ) ;
#9987 = CARTESIAN_POINT ( 'NONE',  ( 151.6065062536777646, 275.0711347837637959, -8.632019726508788793 ) ) ;
#9986 = CARTESIAN_POINT ( 'NONE',  ( 153.3527095124072162, 270.2041312749430517, 14.05198471302335328 ) ) ;
#9988 = CARTESIAN_POINT ( 'NONE',  ( 199.9757505641556747, 267.6639986697646805, 6.164811578842619433 ) ) ;
#9989 = ORIENTED_EDGE ( 'NONE', *, *, #46060, .T. ) ;
#9990 = CARTESIAN_POINT ( 'NONE',  ( 164.4821770989429695, 280.3560663856659971, -11.24245345476798086 ) ) ;
#9991 = CARTESIAN_POINT ( 'NONE',  ( 73.49855677914850105, 61.97002789810530743, -14.76944323329657216 ) ) ;
#9992 = LINE ( 'NONE', #32770, #17278 ) ;
#9993 = CARTESIAN_POINT ( 'NONE',  ( 76.50299338235490154, 221.6427522451419065, 10.00000000000009415 ) ) ;
#9994 = CARTESIAN_POINT ( 'NONE',  ( 75.03295173686203157, 65.04298178550190812, -13.86991885877484698 ) ) ;
#9995 = CARTESIAN_POINT ( 'NONE',  ( 85.51202090377952914, 48.04672559930133957, 11.47155550240170818 ) ) ;
#9996 = CARTESIAN_POINT ( 'NONE',  ( 13.90996860267861024, 31.52903772873356303, -1.583844403245363575 ) ) ;
#9997 = CARTESIAN_POINT ( 'NONE',  ( -4.099453989059914427, 156.8932355074535963, -2.679491924311252493 ) ) ;
#9998 = CARTESIAN_POINT ( 'NONE',  ( -74.33658418421376268, 48.94984639172533747, -10.00000000000000000 ) ) ;
#9999 = CARTESIAN_POINT ( 'NONE',  ( -5.778093977583854013, 155.2202760586659451, -5.415160957724236172E-17 ) ) ;
#10000 = CARTESIAN_POINT ( 'NONE',  ( 91.86592320334659689, 223.8458772461660544, 9.188101187500095079 ) ) ;
#10001 = CARTESIAN_POINT ( 'NONE',  ( 88.00202013401596446, 44.76312363537992667, -4.611939438784355971 ) ) ;
#10002 = CARTESIAN_POINT ( 'NONE',  ( 147.7395812515338491, 275.4447818272566337, 3.760927250875937489 ) ) ;
#10003 = DIRECTION ( 'NONE',  ( -0.8660254037844387076, -0.4999999999999998890, -0.000000000000000000 ) ) ;
#10004 = EDGE_CURVE ( 'NONE', #64385, #49158, #36788, .T. ) ;
#10005 = CYLINDRICAL_SURFACE ( 'NONE', #94275, 10.00000000000010658 ) ;
#10006 = CARTESIAN_POINT ( 'NONE',  ( 164.2057239597426985, 284.2837641608711579, 5.838786750481579801 ) ) ;
#10008 = CARTESIAN_POINT ( 'NONE',  ( 162.9111474110223412, 248.4766108952035211, -9.702990628959184960 ) ) ;
#10007 = CARTESIAN_POINT ( 'NONE',  ( 67.43106664880183132, 66.97720493292270305, 9.028648563732053489 ) ) ;
#10009 = CARTESIAN_POINT ( 'NONE',  ( 161.8690507138996395, 250.2815753210195737, 12.79467889464216945 ) ) ;
#10010 = CARTESIAN_POINT ( 'NONE',  ( 166.1309782654906257, 249.2029336093187339, -9.347746458946922132 ) ) ;
#10011 = CARTESIAN_POINT ( 'NONE',  ( 82.47021907082941539, 53.30441442868470858, -15.33472904691311456 ) ) ;
#10012 = DIRECTION ( 'NONE',  ( -0.8660254037844387076, -0.4999999999999998890, -0.000000000000000000 ) ) ;
#10013 = ADVANCED_FACE ( 'NONE', ( #76789 ), #52989, .T. ) ;
#10014 = CARTESIAN_POINT ( 'NONE',  ( 73.65729962767426287, 69.49757902785614760, 9.740712345197145794 ) ) ;
#10015 = CARTESIAN_POINT ( 'NONE',  ( 33.21950506899538880, 199.1744531367911293, 4.594050593750047540 ) ) ;
#10016 = CARTESIAN_POINT ( 'NONE',  ( 77.06427544118604089, 63.50113506902185634, -15.44174958657458951 ) ) ;
#10017 = EDGE_CURVE ( 'NONE', #61038, #43732, #25762, .T. ) ;
#10018 = CARTESIAN_POINT ( 'NONE',  ( 60.74296170696083408, 212.0024278399160949, 9.188101187500095079 ) ) ;
#10019 = CARTESIAN_POINT ( 'NONE',  ( 161.2488013048736377, 251.3558788108169040, -13.10044423494716170 ) ) ;
#10020 = CARTESIAN_POINT ( 'NONE',  ( 77.59354443008750479, 52.93461377476350549, -16.27594883185225072 ) ) ;
#10021 = CARTESIAN_POINT ( 'NONE',  ( 165.5574043327790150, 259.0627220984302426, 15.59678351321189638 ) ) ;
#10023 = CARTESIAN_POINT ( 'NONE',  ( 151.7165138354984038, 267.8662850201268952, 16.09268003789171431 ) ) ;
#10022 = CARTESIAN_POINT ( 'NONE',  ( 198.7246006328481087, 286.0324930241461630, -17.02257870953173224 ) ) ;
#10024 = CARTESIAN_POINT ( 'NONE',  ( 173.9772233185703669, 268.6891927935771491, -16.30485447805711274 ) ) ;
#10025 = CARTESIAN_POINT ( 'NONE',  ( 28.93108252874724684, 32.10171378149919263, 9.188101187500008038 ) ) ;
#10026 = CARTESIAN_POINT ( 'NONE',  ( 77.93017357788673394, 184.0458036431182052, 21.50000000000000000 ) ) ;
#10027 = CARTESIAN_POINT ( 'NONE',  ( 149.0598351764325002, 272.4677874370131576, -11.59078276432863674 ) ) ;
#10028 = ORIENTED_EDGE ( 'NONE', *, *, #69900, .F. ) ;
#10029 = CARTESIAN_POINT ( 'NONE',  ( 21.25954720759204974, 17.98920272979926338, 7.433330006724137462 ) ) ;
#10030 = CARTESIAN_POINT ( 'NONE',  ( 79.63366147065640632, 204.5327760586659451, 1.948934522072302763E-15 ) ) ;
#10031 = CARTESIAN_POINT ( 'NONE',  ( 76.65872121159138430, 63.56238613867309795, 15.33801735844474834 ) ) ;
#10032 = CARTESIAN_POINT ( 'NONE',  ( 169.6880240292687176, 288.1769740498922374, -1.088266952603743842 ) ) ;
#10033 = CARTESIAN_POINT ( 'NONE',  ( 187.1412927779018673, 261.9835105880691231, -10.20549468610707322 ) ) ;
#10034 = CARTESIAN_POINT ( 'NONE',  ( 153.6752087927504533, 264.4737258376377440, 16.52473746413441091 ) ) ;
#10035 = ORIENTED_EDGE ( 'NONE', *, *, #72159, .F. ) ;
#10036 = CARTESIAN_POINT ( 'NONE',  ( 86.27668453731669729, 47.22199995466520761, 10.82669603042141304 ) ) ;
#10037 = PLANE ( 'NONE',  #29912 ) ;
#10038 = CARTESIAN_POINT ( 'NONE',  ( 118.8119427999550624, 252.7365022471903444, 2.944929066748280225E-16 ) ) ;
#10039 = CARTESIAN_POINT ( 'NONE',  ( 161.8948331661419218, 250.2369188037922356, 13.64419044796309777 ) ) ;
#10040 = CARTESIAN_POINT ( 'NONE',  ( 75.18595658870128773, 53.28276008698350097, 16.02925223909795349 ) ) ;
#10041 = ORIENTED_EDGE ( 'NONE', *, *, #22958, .F. ) ;
#10042 = CARTESIAN_POINT ( 'NONE',  ( 187.7720937987822083, 273.1901695715338292, 15.64266941918570097 ) ) ;
#10043 = ORIENTED_EDGE ( 'NONE', *, *, #16457, .T. ) ;
#10044 = CARTESIAN_POINT ( 'NONE',  ( 163.0309151244508712, 248.2691671304387739, 11.27270415168660200 ) ) ;
#10045 = LINE ( 'NONE', #71856, #7709 ) ;
#10046 = CARTESIAN_POINT ( 'NONE',  ( 68.48697530863641703, 68.75015293434431385, -6.119310236332025532 ) ) ;
#10047 = VERTEX_POINT ( 'NONE', #5408 ) ;
#10048 = CARTESIAN_POINT ( 'NONE',  ( 177.2167214159767070, 253.2638437126931592, -0.2615130296398746612 ) ) ;
#10049 = ORIENTED_EDGE ( 'NONE', *, *, #20714, .T. ) ;
#10050 = CARTESIAN_POINT ( 'NONE',  ( 79.43604583212312775, 46.39531899247212010, -12.74396782343451484 ) ) ;
#10051 = CARTESIAN_POINT ( 'NONE',  ( 167.5688045394477967, 247.4305784569795605, 3.634624977922704669 ) ) ;
#10052 = DIRECTION ( 'NONE',  ( 0.000000000000000000, -0.000000000000000000, 1.000000000000000000 ) ) ;
#10053 = ORIENTED_EDGE ( 'NONE', *, *, #37368, .T. ) ;
#10054 = CARTESIAN_POINT ( 'NONE',  ( 31.23567208480136514, 20.96004757982091604, -5.678558825948275768 ) ) ;
#10055 = CARTESIAN_POINT ( 'NONE',  ( 75.04096107751729505, 66.95220489134599973, -13.17375343603500149 ) ) ;
#10056 = CARTESIAN_POINT ( 'NONE',  ( 84.04052627411616072, 48.12394913304956390, -12.17804820212080052 ) ) ;
#10057 = ADVANCED_FACE ( 'NONE', ( #69683 ), #39755, .T. ) ;
#10058 = CARTESIAN_POINT ( 'NONE',  ( 163.1218343930725894, 256.2508100442478849, -16.13596270478102923 ) ) ;
#10059 = DIRECTION ( 'NONE',  ( 0.4999999999999992784, -0.8660254037844390407, 0.000000000000000000 ) ) ;
#10060 = ORIENTED_EDGE ( 'NONE', *, *, #52016, .F. ) ;
#10061 = ORIENTED_EDGE ( 'NONE', *, *, #19856, .T. ) ;
#10062 = CARTESIAN_POINT ( 'NONE',  ( 183.1143161927901133, 295.7630023993714872, 0.8723711145391563893 ) ) ;
#10064 = CARTESIAN_POINT ( 'NONE',  ( 8.162811221194553823, 28.21091486745858745, -1.111400068045478839E-16 ) ) ;
#10063 = CARTESIAN_POINT ( 'NONE',  ( 163.0627400685409327, 284.1756707159956932, -2.513755478446318747 ) ) ;
#10065 = DIRECTION ( 'NONE',  ( 0.4525327339300069251, -0.8917477921037054722, 0.000000000000000000 ) ) ;
#10066 = CARTESIAN_POINT ( 'NONE',  ( 194.4165969972361552, 293.9075714965812267, 14.23342188338008718 ) ) ;
#10067 = CARTESIAN_POINT ( 'NONE',  ( 70.10520353637093649, 71.60267056347754533, -0.2412377010744407302 ) ) ;
#10068 = CARTESIAN_POINT ( 'NONE',  ( 70.96429761875693032, 61.15374941679502996, 14.99935025239129871 ) ) ;
#10069 = CARTESIAN_POINT ( 'NONE',  ( 164.7591420166619400, 245.2757903461224203, 4.883783760312801370 ) ) ;
#10070 = ADVANCED_FACE ( 'NONE', ( #38778 ), #288, .T. ) ;
#10071 = CARTESIAN_POINT ( 'NONE',  ( 77.55707599997003854, 60.86793710643906508, -16.22826185297084578 ) ) ;
#10072 = DIRECTION ( 'NONE',  ( 0.1378186779084994706, -0.2387089523694924387, -0.9612616959383186721 ) ) ;
#10073 = CARTESIAN_POINT ( 'NONE',  ( 85.20852645963621796, 213.8768266524159856, -9.188101187500091527 ) ) ;
#10074 = EDGE_LOOP ( 'NONE', ( #30260, #11587, #30906, #80828 ) ) ;
#10075 = CARTESIAN_POINT ( 'NONE',  ( 191.0170959869219303, 299.7956799668270946, 7.353346939903929069 ) ) ;
#10076 = DIRECTION ( 'NONE',  ( 1.000000000000000000, 0.000000000000000000, -5.984665299743594308E-16 ) ) ;
#10077 = ORIENTED_EDGE ( 'NONE', *, *, #78563, .F. ) ;
#10078 = VECTOR ( 'NONE', #703, 1000.000000000000000 ) ;
#10079 = CARTESIAN_POINT ( 'NONE',  ( 167.6704087901883895, 266.8335129934314978, -16.83350944486469913 ) ) ;
#10080 = ORIENTED_EDGE ( 'NONE', *, *, #55972, .F. ) ;
#10081 = CARTESIAN_POINT ( 'NONE',  ( 79.90425123310397737, 44.57332524593454082, -11.10618635266240162 ) ) ;
#10082 = LINE ( 'NONE', #47070, #75361 ) ;
#10084 = B_SPLINE_SURFACE_WITH_KNOTS ( 'NONE', 3, 1, ( 
 ( #84621, #91219 ),
 ( #6088, #14687 ),
 ( #69381, #99798 ),
 ( #14194, #45569 ),
 ( #68379, #83630 ),
 ( #45079, #23771 ),
 ( #38968, #4213 ),
 ( #29883, #30885 ),
 ( #76498, #30384 ),
 ( #77501, #98815 ),
 ( #85119, #60757 ),
 ( #36981, #7076 ),
 ( #46061, #61269 ),
 ( #92239, #67893 ),
 ( #29394, #22788 ),
 ( #15164, #92718 ),
 ( #8094, #61771 ),
 ( #23267, #54158 ),
 ( #69874, #487 ),
 ( #31374, #62258 ),
 ( #54662, #63780 ),
 ( #94223, #79015 ),
 ( #39958, #986 ),
 ( #33381, #40955 ),
 ( #41464, #63280 ),
 ( #47573, #8590 ),
 ( #24775, #26290 ),
 ( #1990, #79531 ),
 ( #64285, #85637 ),
 ( #16185, #62768 ),
 ( #78502, #71401 ),
 ( #93726, #9086 ),
 ( #47078, #80022 ),
 ( #87159, #24287 ) ),
 .UNSPECIFIED., .T., .F., .F.,
 ( 4, 2, 2, 2, 2, 2, 2, 2, 2, 2, 2, 2, 2, 2, 2, 2, 4 ),
 ( 2, 2 ),
 ( 0.000000000000000000, 0.06250000000000000000, 0.1250000000000000000, 0.1875000000000000000, 0.2500000000000000000, 0.3125000000000000000, 0.3750000000000000000, 0.4375000000000000000, 0.5000000000000000000, 0.5625000000000000000, 0.6250000000000000000, 0.6875000000000000000, 0.7500000000000000000, 0.8125000000000000000, 0.8750000000000000000, 0.9375000000000000000, 1.000000000000000000 ),
 ( 0.000000000000000000, 1.000000000000000000 ),
 .UNSPECIFIED. ) ;
#10083 = CARTESIAN_POINT ( 'NONE',  ( -13.03140383004354241, 163.2833772461660544, -9.188101187500095079 ) ) ;
#10085 = CARTESIAN_POINT ( 'NONE',  ( 27.25975761432448152, 39.23654200823204263, 1.583844403245397769 ) ) ;
#10086 = CARTESIAN_POINT ( 'NONE',  ( 79.97104311170529911, 48.47299295313705159, -13.83239755450518871 ) ) ;
#10087 = CARTESIAN_POINT ( 'NONE',  ( 208.0148989748639394, 270.3546215746652592, 3.138818306258006618 ) ) ;
#10088 = CARTESIAN_POINT ( 'NONE',  ( 90.72943840876202160, 217.0643266524159571, -9.188101187500093303 ) ) ;
#10089 = ORIENTED_EDGE ( 'NONE', *, *, #75425, .T. ) ;
#10090 = EDGE_LOOP ( 'NONE', ( #76602, #16388, #28224, #81739 ) ) ;
#10091 = DIRECTION ( 'NONE',  ( 0.5000000000000005551, -0.8660254037844382635, -3.965082230804119373E-16 ) ) ;
#10092 = DIRECTION ( 'NONE',  ( -0.5000000000000015543, 0.8660254037844377084, 0.000000000000000000 ) ) ;
#10093 = VERTEX_POINT ( 'NONE', #71209 ) ;
#10094 = CARTESIAN_POINT ( 'NONE',  ( -4.170157060006060235, 26.08383846222962887, 10.00000000000000000 ) ) ;
#10095 = CARTESIAN_POINT ( 'NONE',  ( 77.55626133878482165, 49.73613333205595666, 14.95107568548285037 ) ) ;
#10096 = CARTESIAN_POINT ( 'NONE',  ( -4.903394573382245269, 154.6427522451417644, 1.119607411625061291E-15 ) ) ;
#10097 = CARTESIAN_POINT ( 'NONE',  ( 88.24418735786636603, 44.41312371456485408, 4.416884733071428037 ) ) ;
#10098 = ORIENTED_EDGE ( 'NONE', *, *, #87110, .F. ) ;
#10099 = CARTESIAN_POINT ( 'NONE',  ( 156.9652392049574132, 258.7752260052484985, 18.40175728539550448 ) ) ;
#10100 = CARTESIAN_POINT ( 'NONE',  ( 160.0124400273076333, 275.3606515527212650, 12.84424831609223716 ) ) ;
#10101 = DIRECTION ( 'NONE',  ( 0.8660254037844382635, 0.5000000000000005551, 0.000000000000000000 ) ) ;
#10102 = CARTESIAN_POINT ( 'NONE',  ( 189.0767002963758330, 269.5454149288324857, 14.97099974568435066 ) ) ;
#10103 = CARTESIAN_POINT ( 'NONE',  ( 175.4995246435592833, 283.9138537061506327, 13.23358799048017076 ) ) ;
#10104 = CARTESIAN_POINT ( 'NONE',  ( 78.36279588851795097, 47.41043415324340771, -13.73196331463247688 ) ) ;
#10105 = CARTESIAN_POINT ( 'NONE',  ( 163.8070446421170629, 255.0663642890118581, -15.42060242571707818 ) ) ;
#10106 = ORIENTED_EDGE ( 'NONE', *, *, #51770, .F. ) ;
#10107 = CARTESIAN_POINT ( 'NONE',  ( 200.4116241316243645, 283.5238799070667142, 18.37703770054986663 ) ) ;
#10108 = CARTESIAN_POINT ( 'NONE',  ( 42.65610334793076674, 64.00004027534475881, -10.00000000000000000 ) ) ;
#10109 = CARTESIAN_POINT ( 'NONE',  ( 168.2952158864145531, 250.3176572863741285, 6.948728081753761110 ) ) ;
#10110 = CARTESIAN_POINT ( 'NONE',  ( 77.98425798866018965, 61.79443237021894930, 16.07418881765925178 ) ) ;
#10111 = CARTESIAN_POINT ( 'NONE',  ( 178.7002874096667426, 291.6869041091368899, -6.125093610568141500 ) ) ;
#10112 = CARTESIAN_POINT ( 'NONE',  ( 202.7367043553907990, 279.4967228278296716, -16.72422094393309777 ) ) ;
#10113 = EDGE_LOOP ( 'NONE', ( #31331, #22240, #86098, #30978 ) ) ;
#10114 = CARTESIAN_POINT ( 'NONE',  ( 38.68775240272602645, 99.32300362076651368, 59.99999999999999289 ) ) ;
#10115 = ADVANCED_FACE ( 'NONE', ( #782 ), #1297, .F. ) ;
#10116 = CARTESIAN_POINT ( 'NONE',  ( 206.9258336080761183, 272.2409381227055292, 6.776000910836894597 ) ) ;
#10117 = CARTESIAN_POINT ( 'NONE',  ( 181.9374065758725862, 264.0954804722510971, 13.73142499530935723 ) ) ;
#10118 = CARTESIAN_POINT ( 'NONE',  ( 79.64960764401185145, 54.33444549161213644, 16.32474502074725820 ) ) ;
#10119 = EDGE_CURVE ( 'NONE', #83740, #21633, #16485, .T. ) ;
#10120 = CARTESIAN_POINT ( 'NONE',  ( 31.15975419450677819, 23.15404122711134960, 8.090169943749479842 ) ) ;
#10121 = CARTESIAN_POINT ( 'NONE',  ( 152.8522706834672533, 265.8990964544007056, 17.63080661522264947 ) ) ;
#10122 = CARTESIAN_POINT ( 'NONE',  ( 171.8837275538034532, 274.9715841211527163, 17.02018998718227749 ) ) ;
#10123 = CARTESIAN_POINT ( 'NONE',  ( -61.61048871844075592, 38.59675092633816007, 10.00000000000000000 ) ) ;
#10124 = DIRECTION ( 'NONE',  ( -0.000000000000000000, -0.000000000000000000, -1.000000000000000000 ) ) ;
#10125 = CARTESIAN_POINT ( 'NONE',  ( 188.4962938548358409, 260.9679252005893773, 2.869700643444213828 ) ) ;
#10126 = CARTESIAN_POINT ( 'NONE',  ( 2.064617007569734319, 27.83817977871672511, -10.00000000000000000 ) ) ;
#10127 = CARTESIAN_POINT ( 'NONE',  ( 3.856091543753019213, 173.0333772461660828, 9.188101187500095079 ) ) ;
#10128 = CARTESIAN_POINT ( 'NONE',  ( 83.00132175467911111, 51.24136005855328335, 14.42644208312803578 ) ) ;
#10129 = ORIENTED_EDGE ( 'NONE', *, *, #58254, .T. ) ;
#10130 = EDGE_CURVE ( 'NONE', #52745, #8972, #25885, .T. ) ;
#10131 = CARTESIAN_POINT ( 'NONE',  ( 178.8388798781788296, 256.8338936803557431, 8.575590808577006285 ) ) ;
#10132 = B_SPLINE_CURVE_WITH_KNOTS ( 'NONE', 3,
 ( #56395, #71120, #87390, #63999 ),
 .UNSPECIFIED., .F., .F.,
 ( 4, 4 ),
 ( 0.009125246467023215291, 0.01512799987379969541 ),
 .UNSPECIFIED. ) ;
#10133 = CARTESIAN_POINT ( 'NONE',  ( 32.18369500442691589, 26.78052372038641948, -10.00000000000000355 ) ) ;
#10134 = CARTESIAN_POINT ( 'NONE',  ( 72.07700700168975061, 72.29913914755536553, -0.9446506882752414569 ) ) ;
#10135 = CARTESIAN_POINT ( 'NONE',  ( 26.15589859543730000, 198.1589784336661353, -6.496448406907676862E-16 ) ) ;
#10136 = VECTOR ( 'NONE', #65571, 1000.000000000000000 ) ;
#10137 = AXIS2_PLACEMENT_3D ( 'NONE', #55969, #78817, #72736 ) ;
#10138 = CARTESIAN_POINT ( 'NONE',  ( 161.1238074876215478, 251.5723744529297505, 13.42537408252843179 ) ) ;
#10139 = DIRECTION ( 'NONE',  ( 0.5000000000000002220, -0.8660254037844384856, 0.000000000000000000 ) ) ;
#10140 = CARTESIAN_POINT ( 'NONE',  ( 29.52096178950397842, 38.81751292744057480, -6.180339887498951690 ) ) ;
#10141 = CARTESIAN_POINT ( 'NONE',  ( 181.5900847557695670, 293.9353123765011446, 6.270096989977908208 ) ) ;
#10142 = CARTESIAN_POINT ( 'NONE',  ( 173.2748909899069076, 273.4713738435106620, -17.11406341994456781 ) ) ;
#10143 = CARTESIAN_POINT ( 'NONE',  ( 149.7132193248854435, 271.3360928950326638, 12.70265921103533380 ) ) ;
#10144 = CARTESIAN_POINT ( 'NONE',  ( 81.15053981873714406, 56.17130680763398942, 16.10758762198818417 ) ) ;
#10145 = CARTESIAN_POINT ( 'NONE',  ( 14.64478397084458550, 10.58380873178785642, 6.180339887498953466 ) ) ;
#10146 = CARTESIAN_POINT ( 'NONE',  ( 190.0660857974371822, 298.8038670201426044, -8.153583364850311099 ) ) ;
#10148 = ADVANCED_FACE ( 'NONE', ( #53967 ), #25078, .T. ) ;
#10147 = VECTOR ( 'NONE', #99506, 1000.000000000000000 ) ;
#10149 = CARTESIAN_POINT ( 'NONE',  ( 83.90995141641640487, 51.89037297248786729, 14.88406197085303972 ) ) ;
#10150 = ADVANCED_FACE ( 'NONE', ( #62564 ), #85438, .T. ) ;
#10151 = CARTESIAN_POINT ( 'NONE',  ( 77.09838585100465025, 221.9865022471902876, -10.00000000000009415 ) ) ;
#10152 = CARTESIAN_POINT ( 'NONE',  ( 69.61982051209052713, 66.78800749460349095, -10.00191460643801022 ) ) ;
#10153 = CARTESIAN_POINT ( 'NONE',  ( 203.3655854462036530, 270.0990294040706772, 6.133038700129080922 ) ) ;
#10154 = CARTESIAN_POINT ( 'NONE',  ( 43.28705038798948124, 204.9869531367911293, 4.594050593750046652 ) ) ;
#10155 = CARTESIAN_POINT ( 'NONE',  ( 159.4574711498080433, 254.4585536525209477, 16.86100557095418395 ) ) ;
#10156 = ORIENTED_EDGE ( 'NONE', *, *, #36707, .T. ) ;
#10157 = CARTESIAN_POINT ( 'NONE',  ( -5.552095647868114270, 82.17113873493018161, 13.38795332614766309 ) ) ;
#10158 = CARTESIAN_POINT ( 'NONE',  ( 190.1752790837055045, 301.2537496138681945, -5.177773110520776711 ) ) ;
#10159 = LINE ( 'NONE', #78061, #24040 ) ;
#10160 = ORIENTED_EDGE ( 'NONE', *, *, #34297, .F. ) ;
#10161 = CIRCLE ( 'NONE', #23075, 0.1418229129680828593 ) ;
#10162 = CARTESIAN_POINT ( 'NONE',  ( 156.6812872898450735, 261.2670451491295012, 0.000000000000000000 ) ) ;
#10163 = CARTESIAN_POINT ( 'NONE',  ( 159.5180972751518595, 279.0588588540967976, -11.03979334413982016 ) ) ;
#10164 = CARTESIAN_POINT ( 'NONE',  ( 203.1858896750085535, 273.4118621242805602, 12.47033584857523003 ) ) ;
#10165 = CARTESIAN_POINT ( 'NONE',  ( 24.28583178621855865, 34.99752408145591431, 5.678558825948277544 ) ) ;
#10166 = CARTESIAN_POINT ( 'NONE',  ( 203.0507839702407580, 278.9527209772879814, 16.21318481136342626 ) ) ;
#10167 = CARTESIAN_POINT ( 'NONE',  ( -17.33262083840143930, 129.0458036431182904, 21.50000000000006750 ) ) ;
#10168 = CARTESIAN_POINT ( 'NONE',  ( 171.4451181911705930, 255.5540518477252760, 12.38484697617079178 ) ) ;
#10169 = VERTEX_POINT ( 'NONE', #46887 ) ;
#10170 = CARTESIAN_POINT ( 'NONE',  ( 12.71236424662705566, 15.84335787977761179, 9.188101187500006262 ) ) ;
#10171 = CARTESIAN_POINT ( 'NONE',  ( -0.1018587248682858715, 159.2012482093460051, 2.708621480571796156E-14 ) ) ;
#10172 = CARTESIAN_POINT ( 'NONE',  ( 171.6833113595534712, 252.4132807094040061, 8.718741680673185002 ) ) ;
#10173 = FACE_OUTER_BOUND ( 'NONE', #34481, .T. ) ;
#10174 = EDGE_CURVE ( 'NONE', #37839, #84449, #78305, .T. ) ;
#10175 = VERTEX_POINT ( 'NONE', #9907 ) ;
#10176 = CARTESIAN_POINT ( 'NONE',  ( 72.36468543301930367, 71.15458895874081691, -6.079547378801656521 ) ) ;
#10177 = CYLINDRICAL_SURFACE ( 'NONE', #69382, 16.60714546451156792 ) ;
#10178 = FACE_OUTER_BOUND ( 'NONE', #22012, .T. ) ;
#10179 = DIRECTION ( 'NONE',  ( -0.8660254037844375974, -0.5000000000000016653, 0.000000000000000000 ) ) ;
#10180 = VERTEX_POINT ( 'NONE', #47868 ) ;
#10181 = VERTEX_POINT ( 'NONE', #78805 ) ;
#10182 = ADVANCED_FACE ( 'NONE', ( #32684 ), #24581, .T. ) ;
#10184 =( NAMED_UNIT ( * ) SI_UNIT ( $, .STERADIAN. ) SOLID_ANGLE_UNIT ( ) );
#10183 = CARTESIAN_POINT ( 'NONE',  ( 189.4877677241300944, 274.7371391580670092, -16.41815265926193845 ) ) ;
#10185 = ORIENTED_EDGE ( 'NONE', *, *, #68824, .F. ) ;
#10186 = CARTESIAN_POINT ( 'NONE',  ( 152.8721808860877616, 265.8646109718731623, -17.65676496037632504 ) ) ;
#10187 = DIRECTION ( 'NONE',  ( -0.4831861483251663203, -0.8755176446346986108, 0.000000000000000000 ) ) ;
#10188 = CARTESIAN_POINT ( 'NONE',  ( 72.60433822694926675, 57.21714546342739283, -16.35209281813967763 ) ) ;
#10189 = CARTESIAN_POINT ( 'NONE',  ( 76.63523979702124223, 63.50111620409151669, 15.35509843086873438 ) ) ;
#10190 = CARTESIAN_POINT ( 'NONE',  ( 205.2660270307054304, 275.1158074454486382, -13.97598661256119179 ) ) ;
#10191 = ADVANCED_FACE ( 'NONE', ( #61577 ), #86953, .F. ) ;
#10192 = CARTESIAN_POINT ( 'NONE',  ( 110.3772162092389948, 234.5333772461660828, 9.188101187500095079 ) ) ;
#10193 = EDGE_CURVE ( 'NONE', #91972, #8803, #5798, .T. ) ;
#10194 = CARTESIAN_POINT ( 'NONE',  ( 181.0943051178491885, 287.1835064078692312, -13.38063930454047323 ) ) ;
#10195 = ORIENTED_EDGE ( 'NONE', *, *, #5255, .F. ) ;
#10196 = CARTESIAN_POINT ( 'NONE',  ( 164.4698008747318738, 245.7769439046653019, -6.272955660526681854 ) ) ;
#10197 = EDGE_LOOP ( 'NONE', ( #29543, #15514, #73978, #5112 ) ) ;
#10198 = EDGE_CURVE ( 'NONE', #33624, #79062, #80847, .T. ) ;
#10199 = CARTESIAN_POINT ( 'NONE',  ( 23.84800118292001159, 31.95586893147756058, 7.433330006724141015 ) ) ;
#10200 = CARTESIAN_POINT ( 'NONE',  ( 157.3467993828755880, 258.5604024866626673, 16.83275751048395108 ) ) ;
#10201 = CARTESIAN_POINT ( 'NONE',  ( 78.14732411849692539, 47.76060378147906960, -13.97190537733660243 ) ) ;
#10202 = EDGE_CURVE ( 'NONE', #32950, #66029, #9634, .T. ) ;
#10203 = CARTESIAN_POINT ( 'NONE',  ( 60.74296170696083408, 212.0024278399160949, 9.188101187500095079 ) ) ;
#10204 = CARTESIAN_POINT ( 'NONE',  ( 74.35260113823048300, 68.48135296369000002, 11.20560402319359561 ) ) ;
#10205 = CARTESIAN_POINT ( 'NONE',  ( 191.3375250863502970, 299.2406804863936145, 8.828791580707859410 ) ) ;
#10206 = CARTESIAN_POINT ( 'NONE',  ( 1.764981905019474828, 67.65273034797039031, -10.00000000000000000 ) ) ;
#10207 = CARTESIAN_POINT ( 'NONE',  ( 173.8797520427797849, 271.6693953237884784, 16.43749877907051982 ) ) ;
#10208 = ORIENTED_EDGE ( 'NONE', *, *, #66550, .T. ) ;
#10209 = CARTESIAN_POINT ( 'NONE',  ( 75.01041914018598789, 58.43539866323090592, -15.92242282427785938 ) ) ;
#10210 = CARTESIAN_POINT ( 'NONE',  ( 177.9856817937294124, 288.6971931234167528, 10.88127348114070259 ) ) ;
#10211 = CARTESIAN_POINT ( 'NONE',  ( 78.36958359800738094, 55.49686521012768026, 16.55473436304751900 ) ) ;
#10212 = VERTEX_POINT ( 'NONE', #33189 ) ;
#10213 = CARTESIAN_POINT ( 'NONE',  ( 175.4379314651181119, 261.1390654822758393, -14.58016465811829576 ) ) ;
#10214 = CARTESIAN_POINT ( 'NONE',  ( 174.2802897980567138, 277.2551486598794099, -15.61713791557879993 ) ) ;
#10215 = CARTESIAN_POINT ( 'NONE',  ( 161.4143265314674522, 251.0691807084224365, -12.94469757303959234 ) ) ;
#10216 = CARTESIAN_POINT ( 'NONE',  ( 206.9349434189263661, 269.8064106017384916, 1.784245431258210113 ) ) ;
#10217 = CARTESIAN_POINT ( 'NONE',  ( 149.6676065383367416, 271.4150965588098074, 11.80358707172367261 ) ) ;
#10218 = CARTESIAN_POINT ( 'NONE',  ( 177.2917107194376740, 269.5050067700457816, 16.10103962328780369 ) ) ;
#10219 = CARTESIAN_POINT ( 'NONE',  ( 206.3505875407052486, 273.2372935382459787, 11.62318091048137880 ) ) ;
#10220 = CARTESIAN_POINT ( 'NONE',  ( 75.78378987240938613, 65.61208117828051911, 13.82073902662707354 ) ) ;
#10221 = CARTESIAN_POINT ( 'NONE',  ( 167.8085051679049116, 256.1148727468539619, 13.55799742952848419 ) ) ;
#10222 = PLANE ( 'NONE',  #83643 ) ;
#10223 = CARTESIAN_POINT ( 'NONE',  ( 120.4179585561885659, 231.1423013555409796, -4.594050593750043987 ) ) ;
#10224 = ORIENTED_EDGE ( 'NONE', *, *, #50258, .T. ) ;
#10225 = CARTESIAN_POINT ( 'NONE',  ( 191.8453338867844877, 298.3611298435110371, -9.039024722281077118 ) ) ;
#10226 = CARTESIAN_POINT ( 'NONE',  ( 84.54753597202504523, 42.62579540220287555, 3.803055962842035953 ) ) ;
#10227 = FACE_OUTER_BOUND ( 'NONE', #36232, .T. ) ;
#10228 = DIRECTION ( 'NONE',  ( -0.8082118706970123911, -0.5888918169447047157, 0.000000000000000000 ) ) ;
#10229 = CARTESIAN_POINT ( 'NONE',  ( 83.57459526254079663, 51.48179996603089137, -14.40656865850368717 ) ) ;
#10230 = CARTESIAN_POINT ( 'NONE',  ( 174.7959030193343608, 252.7028669189593870, 5.110487748453643064 ) ) ;
#10231 = ORIENTED_EDGE ( 'NONE', *, *, #508, .T. ) ;
#10232 = CARTESIAN_POINT ( 'NONE',  ( 80.56382388659234550, 57.17170686835115845, -16.22950384588643402 ) ) ;
#10233 = CARTESIAN_POINT ( 'NONE',  ( 155.4293395016508725, 273.5175306886564499, -12.86640682340763320 ) ) ;
#10235 = CARTESIAN_POINT ( 'NONE',  ( 185.9187572292423170, 261.7931673995647657, 10.04575878863954941 ) ) ;
#10234 = CARTESIAN_POINT ( 'NONE',  ( 72.85283338774588913, 70.95119525769652569, 7.785565881738502725 ) ) ;
#10236 = CARTESIAN_POINT ( 'NONE',  ( 42.87860686303043423, 124.5258428655388769, 177.5919119679930134 ) ) ;
#10237 = CARTESIAN_POINT ( 'NONE',  ( 133.7867050834633460, 257.2369531367911009, -4.594050593750048428 ) ) ;
#10238 = CARTESIAN_POINT ( 'NONE',  ( 189.7697392812929138, 294.5961115088648512, -12.48438950990594698 ) ) ;
#10239 = VECTOR ( 'NONE', #45877, 1000.000000000000000 ) ;
#10240 = DIRECTION ( 'NONE',  ( -0.8944271909999158554, 0.000000000000000000, -0.4472135954999578722 ) ) ;
#10241 = CARTESIAN_POINT ( 'NONE',  ( 72.69493809724967548, 71.16443809380129437, -7.267007365939463170 ) ) ;
#10242 = CARTESIAN_POINT ( 'NONE',  ( 62.15025298811053034, 212.8149278399160949, -9.188101187500095079 ) ) ;
#10243 = CARTESIAN_POINT ( 'NONE',  ( 207.6477529416552557, 270.9905371579805546, 7.447146952410988341 ) ) ;
#10244 = CARTESIAN_POINT ( 'NONE',  ( 193.6967711697749905, 268.4383357953667542, 12.84685063220190671 ) ) ;
#10245 = CARTESIAN_POINT ( 'NONE',  ( 71.88059653590643450, 71.08635078533735907, -5.573730649155103301 ) ) ;
#10246 = CARTESIAN_POINT ( 'NONE',  ( 173.4606779374792325, 267.5814416807811540, -17.58000433512257032 ) ) ;
#10247 = CARTESIAN_POINT ( 'NONE',  ( 155.3426119516925610, 279.6488991376975264, -1.568138233356304534 ) ) ;
#10248 = PLANE ( 'NONE',  #41810 ) ;
#10249 = CARTESIAN_POINT ( 'NONE',  ( 203.3205561747472814, 278.4854618126124706, -15.14439614831292147 ) ) ;
#10250 = CARTESIAN_POINT ( 'NONE',  ( 193.0673971409008232, 289.3950934321782142, 16.62649702710665522 ) ) ;
#10251 =( BOUNDED_CURVE ( )  B_SPLINE_CURVE ( 2, ( #17864, #70036, #94880, #87332, #71067, #8257, #9256, #72063, #33554, #77671, #62942, #23434, #54321 ),
 .UNSPECIFIED., .F., .T. ) 
 B_SPLINE_CURVE_WITH_KNOTS ( ( 3, 2, 2, 2, 2, 2, 3 ),
 ( 0.2124999999999999944, 0.2149999999999999967, 0.2200000000000000011, 0.2250000000000000056, 0.2300000000000000100, 0.2349999999999999867, 0.2374999999999999889 ),
 .UNSPECIFIED. ) 
 CURVE ( )  GEOMETRIC_REPRESENTATION_ITEM ( )  RATIONAL_B_SPLINE_CURVE ( ( 0.9755282581475768211, 0.9755282581475768211, 1.000000000000000000, 0.9510565162951535312, 1.000000000000000000, 0.9510565162951535312, 1.000000000000000000, 0.9510565162951535312, 1.000000000000000000, 0.9510565162951535312, 1.000000000000000000, 0.9755282581475768211, 0.9755282581475768211 ) ) 
 REPRESENTATION_ITEM ( '' )  );
#10252 = CARTESIAN_POINT ( 'NONE',  ( 125.1447535615809414, 236.3927522451417929, -10.00000000000009059 ) ) ;
#10253 = CARTESIAN_POINT ( 'NONE',  ( 81.31123310220682754, 51.67285451222524983, -14.93676299417988318 ) ) ;
#10254 = VERTEX_POINT ( 'NONE', #73694 ) ;
#10255 = EDGE_CURVE ( 'NONE', #76205, #76868, #56176, .T. ) ;
#10256 = CARTESIAN_POINT ( 'NONE',  ( 65.02584505343169496, 219.8967562850346837, -4.648177544792955347E-16 ) ) ;
#10257 = CARTESIAN_POINT ( 'NONE',  ( -18.01139699756907930, 172.6589784336661353, -6.496448406907676862E-16 ) ) ;
#10258 = CARTESIAN_POINT ( 'NONE',  ( 38.41565749170202082, 202.1744531367911293, 4.594050593750047540 ) ) ;
#10259 = CARTESIAN_POINT ( 'NONE',  ( 22.25607796093117230, 24.80066082961421969, 10.00000000000000533 ) ) ;
#10260 = CARTESIAN_POINT ( 'NONE',  ( 68.27244882330454345, 65.69410988500804649, -10.30841495897560023 ) ) ;
#10261 = DIRECTION ( 'NONE',  ( -0.9042435392811277728, -0.4270171210482543445, 0.000000000000000000 ) ) ;
#10262 = CARTESIAN_POINT ( 'NONE',  ( 147.4368675721658519, 275.2788497866417288, 5.050119523016719292 ) ) ;
#10263 = CARTESIAN_POINT ( 'NONE',  ( 74.00705488591727033, 54.85690809062158024, -16.13415776006375424 ) ) ;
#10265 = CARTESIAN_POINT ( 'NONE',  ( 59.25465409031482977, 215.0177522451419065, 5.000000000000046185 ) ) ;
#10264 = CARTESIAN_POINT ( 'NONE',  ( 171.6654525870716554, 267.7842514992769907, 17.73500564707179095 ) ) ;
#10266 = DIRECTION ( 'NONE',  ( -0.8660254037844387076, -0.4999999999999998890, -0.000000000000000000 ) ) ;
#10267 = CARTESIAN_POINT ( 'NONE',  ( 180.8260447606230912, 256.2909217566163989, 1.374377561445572438 ) ) ;
#10268 = EDGE_CURVE ( 'NONE', #59479, #35906, #4782, .T. ) ;
#10269 = CARTESIAN_POINT ( 'NONE',  ( 157.6668627405778409, 257.5599783937680058, -16.78811156090270629 ) ) ;
#10270 = CARTESIAN_POINT ( 'NONE',  ( 162.1264656378374696, 252.0740353423958595, -13.51783732343398903 ) ) ;
#10271 = EDGE_CURVE ( 'NONE', #28238, #40468, #33706, .T. ) ;
#10272 = CARTESIAN_POINT ( 'NONE',  ( 44.69460199273694911, 186.6115022471902023, -5.000000000000041744 ) ) ;
#10273 = CARTESIAN_POINT ( 'NONE',  ( 149.2944063396847412, 250.8768266524159856, 9.188101187500098632 ) ) ;
#10274 = CARTESIAN_POINT ( 'NONE',  ( 162.6774150396764469, 248.8814472377480911, 10.88033986792731689 ) ) ;
#10275 = CARTESIAN_POINT ( 'NONE',  ( 3.531332017333847606, 172.8458772461660828, 9.188101187500095079 ) ) ;
#10276 = CARTESIAN_POINT ( 'NONE',  ( 34.84050961144773595, 32.06628583063844218, -9.188101187500006262 ) ) ;
#10278 = CARTESIAN_POINT ( 'NONE',  ( 170.3916841401598958, 263.6555044952191906, 15.81889653756881131 ) ) ;
#10277 = CARTESIAN_POINT ( 'NONE',  ( -27.15312891409035601, 106.0554225863516109, 0.000000000000000000 ) ) ;
#10279 = CARTESIAN_POINT ( 'NONE',  ( 192.7259387352017939, 296.8358775046606297, 11.24705370801146209 ) ) ;
#10280 = CARTESIAN_POINT ( 'NONE',  ( 28.84929788977513709, 34.84336893147758474, -7.433330006724137462 ) ) ;
#10281 = CARTESIAN_POINT ( 'NONE',  ( 165.0087721269838710, 244.8434183119457543, 2.604344609212914108 ) ) ;
#10282 = CARTESIAN_POINT ( 'NONE',  ( 186.8350843013657823, 259.3184771713918053, -2.377127750769511660 ) ) ;
#10283 = CARTESIAN_POINT ( 'NONE',  ( 80.86506773606531340, 42.95500482456080249, -9.556183558881794937 ) ) ;
#10284 = CARTESIAN_POINT ( 'NONE',  ( 149.2223635749290622, 272.1862799931444670, -12.97307652490353647 ) ) ;
#10285 = DIRECTION ( 'NONE',  ( 0.000000000000000000, 0.000000000000000000, 1.000000000000000000 ) ) ;
#10286 = CARTESIAN_POINT ( 'NONE',  ( 8.860943796042899834, 20.51421378149916919, -9.188101187500004485 ) ) ;
#10287 = CARTESIAN_POINT ( 'NONE',  ( 165.7255960892794349, 285.4442248579660486, 0.4815049898957938779 ) ) ;
#10288 = CARTESIAN_POINT ( 'NONE',  ( 14.99289142922413021, 26.84336893147755276, -7.433330006724137462 ) ) ;
#10289 = CARTESIAN_POINT ( 'NONE',  ( -13.76211276271272865, 162.8615022471902307, 0.000000000000000000 ) ) ;
#10290 = CLOSED_SHELL ( 'NONE', ( #99146, #17233, #42355, #7788, #32345, #25198, #64168, #20836, #38012, #4843, #7461, #23647, #47207, #58681, #48831, #29101, #62125, #99445, #19783, #31770, #44757, #76174, #44827, #71010, #95613, #31885, #77143, #65931, #22488, #66205, #73309, #54693, #94780, #22651, #64753, #51910 ) ) ;
#10291 = CARTESIAN_POINT ( 'NONE',  ( 153.3433014850764096, 275.0156552373531440, 10.59304337032270915 ) ) ;
#10292 = CARTESIAN_POINT ( 'NONE',  ( 206.8775514429320026, 272.3245652858344670, -9.838455694836268250 ) ) ;
#10293 = ORIENTED_EDGE ( 'NONE', *, *, #15197, .F. ) ;
#10294 = CARTESIAN_POINT ( 'NONE',  ( 153.1745822862813498, 265.3408363824576668, 16.18092354043443493 ) ) ;
#10295 = CARTESIAN_POINT ( 'NONE',  ( 164.6649740431187183, 245.4388940607451843, -1.430729255012818557 ) ) ;
#10296 = LINE ( 'NONE', #33088, #46090 ) ;
#10297 = CARTESIAN_POINT ( 'NONE',  ( 87.65336964024139377, 45.10687245489099695, 6.884500160062607677 ) ) ;
#10298 = CARTESIAN_POINT ( 'NONE',  ( 194.3562588153086779, 294.0120802933159325, 14.11474987148825200 ) ) ;
#10299 = ORIENTED_EDGE ( 'NONE', *, *, #31863, .F. ) ;
#10300 = ORIENTED_EDGE ( 'NONE', *, *, #63793, .T. ) ;
#10301 = ADVANCED_FACE ( 'NONE', ( #11906 ), #18503, .T. ) ;
#10302 = DIRECTION ( 'NONE',  ( 0.000000000000000000, 0.000000000000000000, 1.000000000000000000 ) ) ;
#10303 = VECTOR ( 'NONE', #2317, 1000.000000000000000 ) ;
#10304 = CARTESIAN_POINT ( 'NONE',  ( 85.95939684119618107, 47.60785808554223308, 10.87377621121526339 ) ) ;
#10305 = ORIENTED_EDGE ( 'NONE', *, *, #57742, .F. ) ;
#10306 = CARTESIAN_POINT ( 'NONE',  ( 77.53002750585342540, 56.25820219453329685, 16.17037978242485607 ) ) ;
#10307 = FACE_OUTER_BOUND ( 'NONE', #41949, .T. ) ;
#10308 = ORIENTED_EDGE ( 'NONE', *, *, #90259, .T. ) ;
#10309 = CARTESIAN_POINT ( 'NONE',  ( 78.38752765249786592, 61.22447296964845975, -15.89000806468494531 ) ) ;
#10310 = CARTESIAN_POINT ( 'NONE',  ( -10.80656490723494123, 24.88181024604956804, 10.00000000000000000 ) ) ;
#10311 = VECTOR ( 'NONE', #654, 1000.000000000000114 ) ;
#10312 = EDGE_CURVE ( 'NONE', #48468, #65117, #65086, .T. ) ;
#10313 = DIRECTION ( 'NONE',  ( 0.9994538543569184696, -0.03304531753667278721, 0.000000000000000000 ) ) ;
#10314 = CARTESIAN_POINT ( 'NONE',  ( 21.02495994229494514, 13.10801979619928304, 3.090169943749476733 ) ) ;
#10315 = ORIENTED_EDGE ( 'NONE', *, *, #97417, .T. ) ;
#10316 = CARTESIAN_POINT ( 'NONE',  ( 161.5875797534026219, 250.7690973254556468, 12.95526170413129030 ) ) ;
#10317 = CARTESIAN_POINT ( 'NONE',  ( 168.9356066370792462, 275.9063550870135373, -15.42059771712085059 ) ) ;
#10318 = CARTESIAN_POINT ( 'NONE',  ( 42.76202708541288899, 64.24573752441608576, 10.00000000000000000 ) ) ;
#10319 = LINE ( 'NONE', #26024, #94712 ) ;
#10320 = PRODUCT_DEFINITION_SHAPE ( 'NONE', 'NONE',  #100303 ) ;
#10321 = ORIENTED_EDGE ( 'NONE', *, *, #79862, .F. ) ;
#10322 = EDGE_CURVE ( 'NONE', #60097, #48601, #19521, .T. ) ;
#10323 = CARTESIAN_POINT ( 'NONE',  ( 170.7128543530930926, 255.6187006993503985, -11.59851742352739912 ) ) ;
#10324 = CARTESIAN_POINT ( 'NONE',  ( -10.54235908185773418, 24.92402704602492847, -10.00000000000000000 ) ) ;
#10325 = ORIENTED_EDGE ( 'NONE', *, *, #34755, .T. ) ;
#10326 = ORIENTED_EDGE ( 'NONE', *, *, #9487, .T. ) ;
#10327 = CARTESIAN_POINT ( 'NONE',  ( 80.20857538925844210, 44.21345027839175401, -11.30608575764590107 ) ) ;
#10328 = EDGE_LOOP ( 'NONE', ( #4813, #23791, #92118, #38673 ) ) ;
#10329 = CYLINDRICAL_SURFACE ( 'NONE', #50854, 10.00000000000010658 ) ;
#10330 = ORIENTED_EDGE ( 'NONE', *, *, #13954, .F. ) ;
#10331 = CARTESIAN_POINT ( 'NONE',  ( 159.2431593014864575, 259.5309889387258409, 16.68740487222246216 ) ) ;
#10332 = CARTESIAN_POINT ( 'NONE',  ( 168.7305174143800741, 272.8130231889026049, 15.98073601715322845 ) ) ;
#10333 = CARTESIAN_POINT ( 'NONE',  ( 147.6685936899311287, 274.8774883772312592, 5.860645049887598823 ) ) ;
#10334 = CARTESIAN_POINT ( 'NONE',  ( 177.4997901991728781, 288.9581381731804299, -9.329869128273438506 ) ) ;
#10335 = CARTESIAN_POINT ( 'NONE',  ( 70.17933292656275057, 66.80308542599925659, 10.34396498317840596 ) ) ;
#10336 = CARTESIAN_POINT ( 'NONE',  ( 192.7787710433387360, 295.2766471658688943, 13.34619424850646752 ) ) ;
#10337 = DIRECTION ( 'NONE',  ( 0.000000000000000000, 0.000000000000000000, 1.000000000000000000 ) ) ;
#10338 = CARTESIAN_POINT ( 'NONE',  ( -19.65312891409030271, 93.06504152958497400, -10.00000000000000888 ) ) ;
#10339 = ORIENTED_EDGE ( 'NONE', *, *, #28353, .T. ) ;
#10340 = CARTESIAN_POINT ( 'NONE',  ( 183.6498318386265396, 256.3252116762061519, 1.424693195823348635 ) ) ;
#10341 = CARTESIAN_POINT ( 'NONE',  ( 16.26188567080226477, 32.49540643055187417, 3.479690158560446702E-15 ) ) ;
#10342 = CARTESIAN_POINT ( 'NONE',  ( 164.4573439719129340, 245.7985198932525748, 1.541132361166968501 ) ) ;
#10343 = CARTESIAN_POINT ( 'NONE',  ( 164.7762319088960794, 245.2461897844768828, 2.994040459560653122 ) ) ;
#10345 = EDGE_LOOP ( 'NONE', ( #76741, #15276, #27131, #45942, #31110, #99138, #10299, #26392 ) ) ;
#10344 = CARTESIAN_POINT ( 'NONE',  ( -47.78078991586326651, 28.96484896693080913, 10.00000000000000000 ) ) ;
#10346 = ORIENTED_EDGE ( 'NONE', *, *, #79852, .T. ) ;
#10347 = CYLINDRICAL_SURFACE ( 'NONE', #51380, 17.82106496071139645 ) ;
#10348 = CARTESIAN_POINT ( 'NONE',  ( 171.5826572751710160, 259.5044536903516246, -13.90678447660475925 ) ) ;
#10349 = FACE_OUTER_BOUND ( 'NONE', #24863, .T. ) ;
#10350 = CARTESIAN_POINT ( 'NONE',  ( 10.35730516091175701, 49.35094346172001423, 59.99999999999999289 ) ) ;
#10351 = EDGE_CURVE ( 'NONE', #75738, #63237, #50381, .T. ) ;
#10352 = CARTESIAN_POINT ( 'NONE',  ( 161.4726291907278721, 250.9681975403669867, 14.52346149734912117 ) ) ;
#10353 = CARTESIAN_POINT ( 'NONE',  ( 191.1149281592727789, 262.1737860021522692, -0.7454788891368452353 ) ) ;
#10354 = ORIENTED_EDGE ( 'NONE', *, *, #72324, .F. ) ;
#10355 = CARTESIAN_POINT ( 'NONE',  ( 179.9804556880129383, 273.2999562016793789, -17.78099266527076949 ) ) ;
#10356 = CARTESIAN_POINT ( 'NONE',  ( 81.62382999622622037, 59.34769798152620268, 0.4414737964294616623 ) ) ;
#10357 = CARTESIAN_POINT ( 'NONE',  ( 51.59680478827888805, 189.0494855054051868, -2.679491924311248496 ) ) ;
#10359 = EDGE_CURVE ( 'NONE', #22179, #32899, #66088, .T. ) ;
#10358 = CARTESIAN_POINT ( 'NONE',  ( -40.42249077443059235, 27.53003111760058630, -10.00000000000000000 ) ) ;
#10360 = CARTESIAN_POINT ( 'NONE',  ( 18.47929132879751890, 188.1427522451419350, -10.00000000000009415 ) ) ;
#10361 = CARTESIAN_POINT ( 'NONE',  ( 93.32716752435031538, 230.8149278399160949, -9.188101187500095079 ) ) ;
#10362 = CARTESIAN_POINT ( 'NONE',  ( 82.36066395365664050, 40.35653381656560867, -0.9401641086475391873 ) ) ;
#10363 = CARTESIAN_POINT ( 'NONE',  ( 84.67479249306344968, 50.56977290030206262, 13.61422284357908197 ) ) ;
#10364 = CARTESIAN_POINT ( 'NONE',  ( 162.6076392040105816, 249.0023025302617725, 11.70000256607044165 ) ) ;
#10365 = CARTESIAN_POINT ( 'NONE',  ( 23.96437920969670898, 175.4548013555409796, -4.594050593750042211 ) ) ;
#10366 = CARTESIAN_POINT ( 'NONE',  ( -5.122212653107841795, 179.3967562850347406, 2.649461200531984646E-14 ) ) ;
#10367 = VERTEX_POINT ( 'NONE', #49389 ) ;
#10368 = VERTEX_POINT ( 'NONE', #49888 ) ;
#10369 = CARTESIAN_POINT ( 'NONE',  ( 200.9615411070818425, 267.7048942554176847, -3.403220809365973931 ) ) ;
#10370 = CARTESIAN_POINT ( 'NONE',  ( 79.65783702838581348, 47.13130848700988906, -13.15621609857660523 ) ) ;
#10371 = CARTESIAN_POINT ( 'NONE',  ( 82.71995705146288458, 41.94179129365014802, 4.898035795836064743 ) ) ;
#10372 = CARTESIAN_POINT ( 'NONE',  ( 194.0465404961993556, 264.4183967981790602, -4.354813327397827116 ) ) ;
#10373 = AXIS2_PLACEMENT_3D ( 'NONE', #16530, #91571, #335 ) ;
#10374 = CARTESIAN_POINT ( 'NONE',  ( 161.2977680094314223, 251.2710659906439616, -13.03191437619249982 ) ) ;
#10375 = CARTESIAN_POINT ( 'NONE',  ( 182.6041507127388002, 284.2934025591197269, 14.95852815553201864 ) ) ;
#10376 = CARTESIAN_POINT ( 'NONE',  ( 74.21864607481936105, 68.58553829006309854, -11.54532566021463502 ) ) ;
#10377 = CARTESIAN_POINT ( 'NONE',  ( 25.42527643493543366, 194.6744531367911293, 4.594050593750047540 ) ) ;
#10378 = CARTESIAN_POINT ( 'NONE',  ( 77.44118756978804186, 225.5177522451419350, 5.000000000000046185 ) ) ;
#10379 = ORIENTED_EDGE ( 'NONE', *, *, #88321, .T. ) ;
#10380 = CARTESIAN_POINT ( 'NONE',  ( 79.31967116076749846, 59.78699023733837237, -16.51284638439522112 ) ) ;
#10382 = EDGE_CURVE ( 'NONE', #8334, #67265, #97034, .T. ) ;
#10381 = VECTOR ( 'NONE', #76819, 1000.000000000000000 ) ;
#10383 = CARTESIAN_POINT ( 'NONE',  ( 178.7980240951186488, 259.0421912297024392, -10.14286040655596288 ) ) ;
#10384 = CARTESIAN_POINT ( 'NONE',  ( -10.94779052401099051, 173.6744531367911293, 4.594050593750047540 ) ) ;
#10385 = FACE_OUTER_BOUND ( 'NONE', #58845, .T. ) ;
#10386 = CARTESIAN_POINT ( 'NONE',  ( 198.9225589249066957, 286.1030165008847916, -17.03502353404871883 ) ) ;
#10387 = DIRECTION ( 'NONE',  ( 0.4999999999999992784, -0.8660254037844390407, 0.000000000000000000 ) ) ;
#10388 = CARTESIAN_POINT ( 'NONE',  ( 147.5851099763508216, 275.0220864107570264, -4.372720440640867956 ) ) ;
#10389 = CARTESIAN_POINT ( 'NONE',  ( -11.77978294824862893, 175.5530062829863311, 1.347971487989956912E-14 ) ) ;
#10390 = CARTESIAN_POINT ( 'NONE',  ( 163.9149533033796047, 246.7379680887036670, 7.273005089308705706 ) ) ;
#10391 = EDGE_CURVE ( 'NONE', #49538, #76828, #41647, .T. ) ;
#10392 = CARTESIAN_POINT ( 'NONE',  ( 191.7187529716733820, 298.5803744197520473, -8.487597704798396592 ) ) ;
#10393 = CARTESIAN_POINT ( 'NONE',  ( 206.9408877595175511, 272.2148635675444552, 6.707071080545934372 ) ) ;
#10394 = ADVANCED_FACE ( 'NONE', ( #96530 ), #92169, .F. ) ;
#10395 = CARTESIAN_POINT ( 'NONE',  ( 151.2701135660092007, 248.9548013555409796, -4.594050593750042211 ) ) ;
#10396 = CARTESIAN_POINT ( 'NONE',  ( 7.752142999874299001, 186.8297689869269220, -2.679491924311252493 ) ) ;
#10397 = CARTESIAN_POINT ( 'NONE',  ( 111.5140480995885497, 229.0643266524159856, -9.188101187500093303 ) ) ;
#10398 = CARTESIAN_POINT ( 'NONE',  ( 13.67041502465407277, 29.93396525600389424, 2.839279412974139660 ) ) ;
#10399 = CARTESIAN_POINT ( 'NONE',  ( 75.03253579078814539, 67.12707870640632279, 13.05283704309126414 ) ) ;
#10400 = DIRECTION ( 'NONE',  ( -0.8660254037844387076, -0.4999999999999998890, -0.000000000000000000 ) ) ;
#10402 = CARTESIAN_POINT ( 'NONE',  ( 162.1596889173749787, 251.8569052447999184, -14.10774048472399222 ) ) ;
#10401 = CARTESIAN_POINT ( 'NONE',  ( 180.3268137483904354, 258.1330830615356149, 10.30874540274224849 ) ) ;
#10403 = CARTESIAN_POINT ( 'NONE',  ( 191.3193808042797741, 299.2721073048064682, -6.832536527061075837 ) ) ;
#10404 = ORIENTED_EDGE ( 'NONE', *, *, #7917, .F. ) ;
#10405 = CARTESIAN_POINT ( 'NONE',  ( 191.6416599777803071, 263.0665572907887508, -4.349148431717937413 ) ) ;
#10406 = CARTESIAN_POINT ( 'NONE',  ( 196.2630260332681189, 290.7094625936034049, -17.43112004684450866 ) ) ;
#10407 = CARTESIAN_POINT ( 'NONE',  ( 190.5500884410106153, 299.9961840195823015, 4.185962364582526796 ) ) ;
#10408 = CARTESIAN_POINT ( 'NONE',  ( 173.2992799364793655, 289.7901017517768878, -1.077829072056774473 ) ) ;
#10409 = CARTESIAN_POINT ( 'NONE',  ( 81.36199125831662116, 55.41608345602817565, -16.32668456146281244 ) ) ;
#10410 = ORIENTED_EDGE ( 'NONE', *, *, #10623, .T. ) ;
#10411 = FACE_OUTER_BOUND ( 'NONE', #10804, .T. ) ;
#10412 = CARTESIAN_POINT ( 'NONE',  ( 176.4230820045180224, 279.0088413606695781, 15.48324227125391239 ) ) ;
#10413 = CARTESIAN_POINT ( 'NONE',  ( 196.8708119716154954, 268.3476497963631573, -11.07389558091716708 ) ) ;
#10414 = B_SPLINE_CURVE_WITH_KNOTS ( 'NONE', 3,
 ( #91126, #59157, #5493, #90129, #98714, #21691, #28790, #37863, #22186, #97713, #36376, #21204, #52571, #67281, #20703, #35884, #98207, #59670, #51591, #14090, #6494, #90644, #75913, #37372, #53080, #84033, #6980, #14592, #45471, #68772, #99696 ),
 .UNSPECIFIED., .F., .F.,
 ( 4, 3, 3, 3, 3, 3, 3, 3, 3, 3, 4 ),
 ( 0.000000000000000000, 0.1333490885032329043, 0.3007194338854160542, 0.4699862290244992691, 0.5844252810809290599, 0.6686540514502579136, 0.7354980260655432645, 0.8028463152565632477, 0.8633854507757217078, 0.9437142632667381292, 1.000000000000000000 ),
 .UNSPECIFIED. ) ;
#10415 = CARTESIAN_POINT ( 'NONE',  ( 80.04281669451169989, 53.86981617844637782, 15.76102994265571411 ) ) ;
#10416 = CARTESIAN_POINT ( 'NONE',  ( 83.76063610407190652, 51.49572955327540313, -14.36612422999478866 ) ) ;
#10417 = CARTESIAN_POINT ( 'NONE',  ( 70.15559162998948750, 71.15866369468874097, 0.8108420958401643119 ) ) ;
#10418 = CARTESIAN_POINT ( 'NONE',  ( 148.5240811353718016, 275.0344138590257330, 7.425379614582615417 ) ) ;
#10419 = EDGE_CURVE ( 'NONE', #79111, #86732, #84317, .T. ) ;
#10420 = CARTESIAN_POINT ( 'NONE',  ( 191.2272277623841035, 280.2561453075193754, 17.73953484063011388 ) ) ;
#10421 = CARTESIAN_POINT ( 'NONE',  ( 41.44395331530407844, 35.87878583063845639, -9.188101187500006262 ) ) ;
#10422 = CARTESIAN_POINT ( 'NONE',  ( 173.8066869025494441, 272.5896278189234181, -16.38874741603444107 ) ) ;
#10423 = VERTEX_POINT ( 'NONE', #83816 ) ;
#10424 = CARTESIAN_POINT ( 'NONE',  ( 77.78993031024410243, 61.70844822385715389, 16.06828208845739780 ) ) ;
#10425 = CARTESIAN_POINT ( 'NONE',  ( 194.9819925439454664, 292.9282776833073285, -15.33279721168237586 ) ) ;
#10426 = DIRECTION ( 'NONE',  ( 0.4999999999999998890, -0.8660254037844385966, 0.000000000000000000 ) ) ;
#10427 = ORIENTED_EDGE ( 'NONE', *, *, #3975, .F. ) ;
#10428 = CARTESIAN_POINT ( 'NONE',  ( 78.88256717313477395, 59.65579592159198086, 16.50129574805686161 ) ) ;
#10429 = CARTESIAN_POINT ( 'NONE',  ( 76.77731254116881132, 64.09355814141257213, -15.16545583891343263 ) ) ;
#10430 = CARTESIAN_POINT ( 'NONE',  ( 87.99887978206298556, 43.75530803335438890, -2.234124107031381534 ) ) ;
#10431 = PLANE ( 'NONE',  #98626 ) ;
#10432 = CARTESIAN_POINT ( 'NONE',  ( 84.72693717884534692, 49.96098312850357104, -13.65910992477957819 ) ) ;
#10433 = CARTESIAN_POINT ( 'NONE',  ( -45.72565977301701423, 72.45571923938835823, -10.00000000000000000 ) ) ;
#10434 = ORIENTED_EDGE ( 'NONE', *, *, #88822, .F. ) ;
#10435 = ORIENTED_EDGE ( 'NONE', *, *, #49730, .T. ) ;
#10436 = PLANE ( 'NONE',  #91855 ) ;
#10437 = ORIENTED_EDGE ( 'NONE', *, *, #100044, .T. ) ;
#10438 = DIRECTION ( 'NONE',  ( 0.5000000000000014433, -0.8660254037844378194, 0.000000000000000000 ) ) ;
#10439 = B_SPLINE_CURVE_WITH_KNOTS ( 'NONE', 3,
 ( #12330, #6709, #37587, #43194, #66513, #82763, #97439, #44192, #67501, #86258, #31487, #23890, #77622, #69989 ),
 .UNSPECIFIED., .F., .F.,
 ( 4, 2, 2, 2, 2, 2, 4 ),
 ( 0.0009839635007110013321, 0.001239636163184778313, 0.001495308825658555512, 0.001750981488132332493, 0.002006654150606109691, 0.002517999475553669292, 0.003029344800501229326 ),
 .UNSPECIFIED. ) ;
#10440 = AXIS2_PLACEMENT_3D ( 'NONE', #96147, #27217, #2942 ) ;
#10441 = ORIENTED_EDGE ( 'NONE', *, *, #73824, .T. ) ;
#10442 = CARTESIAN_POINT ( 'NONE',  ( 74.38298257480929010, 55.99886258023348518, 16.10773052095676405 ) ) ;
#10443 = CARTESIAN_POINT ( 'NONE',  ( 77.95436975687957215, 48.11784896437987413, 14.20357318872345331 ) ) ;
#10444 = ORIENTED_EDGE ( 'NONE', *, *, #81227, .T. ) ;
#10445 = DIRECTION ( 'NONE',  ( -0.3715724127386920705, 0.6435822975543701308, -0.6691306063588670083 ) ) ;
#10446 = CARTESIAN_POINT ( 'NONE',  ( 189.9165526381299571, 301.7018769628665495, 2.876435567632701584 ) ) ;
#10447 = DIRECTION ( 'NONE',  ( -0.5000000000000082157, 0.8660254037844338226, 0.000000000000000000 ) ) ;
#10448 = CARTESIAN_POINT ( 'NONE',  ( 192.4743214706506365, 297.2716913909250707, -12.17804856100553046 ) ) ;
#10449 = LINE ( 'NONE', #94576, #83548 ) ;
#10450 = CARTESIAN_POINT ( 'NONE',  ( 81.30818518503046732, 58.89441083166271085, 0.000000000000000000 ) ) ;
#10451 = AXIS2_PLACEMENT_3D ( 'NONE', #32928, #63832, #95790 ) ;
#10452 = CARTESIAN_POINT ( 'NONE',  ( 153.8556153531656321, 279.8124448561599706, 2.207844972829135166 ) ) ;
#10453 = CARTESIAN_POINT ( 'NONE',  ( 130.5662598870812019, 252.3149278399160664, 9.188101187500093303 ) ) ;
#10454 = ORIENTED_EDGE ( 'NONE', *, *, #41133, .F. ) ;
#10455 = CARTESIAN_POINT ( 'NONE',  ( 88.02796755599807454, 43.59779901362369259, -1.172627947537940913E-07 ) ) ;
#10456 = EDGE_CURVE ( 'NONE', #55671, #93478, #90434, .T. ) ;
#10457 = ORIENTED_EDGE ( 'NONE', *, *, #81456, .T. ) ;
#10459 = ORIENTED_EDGE ( 'NONE', *, *, #63681, .F. ) ;
#10458 = CARTESIAN_POINT ( 'NONE',  ( 30.82187231905848535, 18.76426979415091267, 3.090169943749476733 ) ) ;
#10460 = CARTESIAN_POINT ( 'NONE',  ( 203.5517807763935991, 276.4131063546051337, 14.32831804246049678 ) ) ;
#10461 = CYLINDRICAL_SURFACE ( 'NONE', #5936, 17.82106496071139645 ) ;
#10462 = CARTESIAN_POINT ( 'NONE',  ( 75.99750771566300500, 65.44421971917601866, -13.95497799904430458 ) ) ;
#10463 = CARTESIAN_POINT ( 'NONE',  ( 146.6727924462101669, 276.6022667255962801, 3.481050673020940511 ) ) ;
#10464 = CARTESIAN_POINT ( 'NONE',  ( 153.4235286554718130, 276.8959503085853839, 7.157280695494672607 ) ) ;
#10465 = CARTESIAN_POINT ( 'NONE',  ( 163.4927498574098763, 249.4692459082536686, 11.48939803020791750 ) ) ;
#10466 = DIRECTION ( 'NONE',  ( -0.8143688203140631021, 0.5803476755362091399, 0.000000000000000000 ) ) ;
#10467 = CARTESIAN_POINT ( 'NONE',  ( 171.1570684511148102, 280.6390554436904949, 13.86101101377389533 ) ) ;
#10468 = FACE_OUTER_BOUND ( 'NONE', #40606, .T. ) ;
#10469 = CARTESIAN_POINT ( 'NONE',  ( 177.3728554691246018, 255.8828027512285530, -8.252538712637369045 ) ) ;
#10470 = EDGE_LOOP ( 'NONE', ( #42659, #6542, #89818, #48063 ) ) ;
#10471 = CARTESIAN_POINT ( 'NONE',  ( -19.65312891409030271, 93.06504152958497400, 10.00000000000000888 ) ) ;
#10472 = CARTESIAN_POINT ( 'NONE',  ( 10.82940026203503336, 170.3927522451417929, -10.00000000000009237 ) ) ;
#10473 = VERTEX_POINT ( 'NONE', #43266 ) ;
#10474 = DIRECTION ( 'NONE',  ( -0.8503781557569302096, 0.05328141121993809626, -0.5234673661555743207 ) ) ;
#10475 = CARTESIAN_POINT ( 'NONE',  ( 204.6703448838256918, 269.2340485566120947, -2.958164987615520936 ) ) ;
#10476 = CARTESIAN_POINT ( 'NONE',  ( 191.4657099001964866, 299.0186578760529983, -10.61565110258011480 ) ) ;
#10477 = CARTESIAN_POINT ( 'NONE',  ( 149.0761751337341821, 272.4394858007734683, 11.56094486755886130 ) ) ;
#10478 = CARTESIAN_POINT ( 'NONE',  ( 163.2442700311756596, 247.8996255919473697, 11.14021925110252020 ) ) ;
#10480 = CARTESIAN_POINT ( 'NONE',  ( 152.5863647195084809, 275.6253943308787484, -8.621472240177467938 ) ) ;
#10479 = CARTESIAN_POINT ( 'NONE',  ( 22.96769398916923777, 37.53608102203546792, -10.00000000000000000 ) ) ;
#10481 = FACE_OUTER_BOUND ( 'NONE', #20029, .T. ) ;
#10482 = VERTEX_POINT ( 'NONE', #21481 ) ;
#10483 = CARTESIAN_POINT ( 'NONE',  ( 72.34523945420380642, 62.27941420626569169, -14.34989103246101827 ) ) ;
#10484 = CARTESIAN_POINT ( 'NONE',  ( 193.2812998533557618, 275.8456789399431273, -16.80650560145133809 ) ) ;
#10485 = CARTESIAN_POINT ( 'NONE',  ( 73.08007996217260427, 65.63861575768015655, -12.79487007168413015 ) ) ;
#10486 = CARTESIAN_POINT ( 'NONE',  ( 85.05511982866016751, 46.74444827917869816, 10.44744734522612717 ) ) ;
#10487 = CARTESIAN_POINT ( 'NONE',  ( 80.78918961562681034, 43.20779693872438543, -9.098606657379754381 ) ) ;
#10488 = CARTESIAN_POINT ( 'NONE',  ( 67.55525932531482169, 69.43178850908184074, 2.233867015644889431 ) ) ;
#10489 = CARTESIAN_POINT ( 'NONE',  ( -0.2032289886040369309, 164.5643266524160140, -9.188101187500093303 ) ) ;
#10490 = CARTESIAN_POINT ( 'NONE',  ( 100.4182711614829486, 216.5327760586659451, 1.948934522072303157E-15 ) ) ;
#10491 = CARTESIAN_POINT ( 'NONE',  ( 155.6048174803203210, 261.1315455520403361, -17.38645169541727498 ) ) ;
#10492 = CARTESIAN_POINT ( 'NONE',  ( 146.9129474150286683, 276.1863061179126930, -5.016087650759920358 ) ) ;
#10493 = FACE_OUTER_BOUND ( 'NONE', #72429, .T. ) ;
#10494 = CARTESIAN_POINT ( 'NONE',  ( -4.163664537435148638, 161.7365022471902307, 10.00000000000009948 ) ) ;
#10495 = CARTESIAN_POINT ( 'NONE',  ( 74.24029763082349120, 55.47955095029949746, -16.12046342301015756 ) ) ;
#10496 = CARTESIAN_POINT ( 'NONE',  ( 164.2093793230265817, 284.1672360007073053, 5.801580848943813429 ) ) ;
#10498 = CARTESIAN_POINT ( 'NONE',  ( 163.2742264920156572, 247.8477394797576778, -9.850275379362519956 ) ) ;
#10497 = CARTESIAN_POINT ( 'NONE',  ( 190.3965342815112933, 300.3990912182416650, -0.9262266978771579451 ) ) ;
#10499 = CARTESIAN_POINT ( 'NONE',  ( 207.4561410457603472, 271.3224186970049914, 4.887894857253799685 ) ) ;
#10500 = LINE ( 'NONE', #88559, #63731 ) ;
#10501 = DIRECTION ( 'NONE',  ( -0.8660254037844387076, -0.4999999999999998890, -0.000000000000000000 ) ) ;
#10502 = EDGE_CURVE ( 'NONE', #57260, #55973, #29576, .T. ) ;
#10503 = CARTESIAN_POINT ( 'NONE',  ( 77.09103540138860922, 55.43591893971357365, -16.15323720810845742 ) ) ;
#10504 = CARTESIAN_POINT ( 'NONE',  ( 79.22212042028705525, 45.73389709458791685, -12.98434876985491115 ) ) ;
#10505 = VECTOR ( 'NONE', #41595, 1000.000000000000114 ) ;
#10506 = B_SPLINE_CURVE_WITH_KNOTS ( 'NONE', 3,
 ( #24159, #32253, #55044, #8459 ),
 .UNSPECIFIED., .F., .F.,
 ( 4, 4 ),
 ( 0.009739077263292133385, 0.01805476430672628765 ),
 .UNSPECIFIED. ) ;
#10507 = CARTESIAN_POINT ( 'NONE',  ( 90.56794795857862823, 211.5494855054051584, -2.679491924311248496 ) ) ;
#10509 = EDGE_CURVE ( 'NONE', #10212, #78334, #45043, .T. ) ;
#10508 = CARTESIAN_POINT ( 'NONE',  ( 73.60600985167290844, 69.76719088550383674, 9.400953274917574376 ) ) ;
#10510 = CARTESIAN_POINT ( 'NONE',  ( 46.72434903108273119, 197.7833772461660828, -9.188101187500095079 ) ) ;
#10512 = EDGE_CURVE ( 'NONE', #78854, #81228, #37655, .T. ) ;
#10511 = CARTESIAN_POINT ( 'NONE',  ( 77.07143086693146472, 63.53409821367920784, -15.43182057973166188 ) ) ;
#10513 = EDGE_CURVE ( 'NONE', #3234, #18286, #87369, .T. ) ;
#10514 = CARTESIAN_POINT ( 'NONE',  ( 69.94482871793547929, 205.0643266524159856, -9.188101187500093303 ) ) ;
#10515 = CARTESIAN_POINT ( 'NONE',  ( 161.3145230519951951, 251.2420454056404822, -14.44869077440025151 ) ) ;
#10517 = CARTESIAN_POINT ( 'NONE',  ( 88.06269261788010283, 43.61796610520789841, 0.05835779599787579291 ) ) ;
#10516 = VECTOR ( 'NONE', #18118, 1000.000000000000000 ) ;
#10518 = CARTESIAN_POINT ( 'NONE',  ( 163.4927498574098763, 249.4692459082536686, 11.48939803020791750 ) ) ;
#10520 = CARTESIAN_POINT ( 'NONE',  ( 200.3107031111897243, 283.6986802420111644, 17.10973405491822419 ) ) ;
#10519 = DIRECTION ( 'NONE',  ( -1.000000000000000000, 0.000000000000000000, 0.000000000000000000 ) ) ;
#10521 = B_SPLINE_CURVE_WITH_KNOTS ( 'NONE', 3,
 ( #47818, #78756, #9343, #71162 ),
 .UNSPECIFIED., .F., .F.,
 ( 4, 4 ),
 ( 0.01197369137472301809, 0.01810739594695707014 ),
 .UNSPECIFIED. ) ;
#10522 = CARTESIAN_POINT ( 'NONE',  ( 17.25242200676959570, 180.7677522451418497, 10.00000000000009592 ) ) ;
#10523 = CARTESIAN_POINT ( 'NONE',  ( 37.13125039574066477, 23.29860640527294535, -2.839279412974138328 ) ) ;
#10524 = CARTESIAN_POINT ( 'NONE',  ( 82.56061938396526045, 50.68218938071114366, 14.69501007283553307 ) ) ;
#10525 = FACE_OUTER_BOUND ( 'NONE', #41837, .T. ) ;
#10526 = EDGE_LOOP ( 'NONE', ( #58229, #26025, #78330, #8554, #64602, #47909, #72766, #96977, #46188, #29430, #77336, #33155, #68915, #98031, #36335, #71659, #4846, #10951, #25302, #331, #43335, #98823, #18782, #85278, #65640, #89263, #25789, #37698, #80257, #88003, #29709, #72495, #46012, #20778, #28661, #4245, #89965, #63132, #14454, #18543, #73176, #39298, #42103, #7819, #65321, #68510, #52177, #20182, #94043, #28992, #65122, #52930, #77214, #34539, #37417, #45231, #70251, #56767, #31169, #85243, #2568, #22810, #70988, #85626, #96809, #50453, #4067, #97171, #79464, #32579, #86350, #70097, #30886, #35828, #84878, #95698, #38571, #79751, #82722, #98922, #26054, #25379, #71016, #51682, #34708, #17123, #62956, #22878, #68832, #51917, #74507, #75390, #11829, #31358, #74717, #56895, #10599, #54487, #23782, #6943, #50632, #15782, #72133, #11454, #96963, #31096, #37705, #41934, #16970, #24500, #10669, #17502, #31097, #39063, #93455, #53618, #76453, #67998, #38699, #98654, #42754, #27240, #1991, #5438, #14373, #5047, #52281 ) ) ;
#10527 = CARTESIAN_POINT ( 'NONE',  ( 13.49720994389718598, 29.83396525600389637, -2.839279412974133887 ) ) ;
#10528 = CARTESIAN_POINT ( 'NONE',  ( 70.81050702595493362, 217.8149278399160949, 9.188101187500093303 ) ) ;
#10529 = CARTESIAN_POINT ( 'NONE',  ( 89.29491028763546012, 232.3615022471903160, 5.000000000000046185 ) ) ;
#10530 = CARTESIAN_POINT ( 'NONE',  ( 159.4889735931715222, 254.4039898200529706, 16.88104032092801887 ) ) ;
#10531 = FACE_OUTER_BOUND ( 'NONE', #76117, .T. ) ;
#10532 = CARTESIAN_POINT ( 'NONE',  ( 201.7913750587587458, 281.1340811994797946, 17.83190890278124741 ) ) ;
#10533 = ORIENTED_EDGE ( 'NONE', *, *, #97782, .F. ) ;
#10534 = LINE ( 'NONE', #50023, #37268 ) ;
#10535 = CARTESIAN_POINT ( 'NONE',  ( 193.5431251303248530, 288.4874559808632171, 16.06641325508723384 ) ) ;
#10536 = CARTESIAN_POINT ( 'NONE',  ( 12.50963621419470329, 166.4824982072973967, 3.021315404115420679E-15 ) ) ;
#10538 =( BOUNDED_CURVE ( )  B_SPLINE_CURVE ( 2, ( #69431, #22334, #28950, #6646, #44616, #60313, #92283, #45128, #98361 ),
 .UNSPECIFIED., .F., .T. ) 
 B_SPLINE_CURVE_WITH_KNOTS ( ( 3, 2, 2, 2, 3 ),
 ( 0.4959677419354838745, 0.4973118279569892497, 0.5000000000000000000, 0.5026881720430107503, 0.5040322580645161255 ),
 .UNSPECIFIED. ) 
 CURVE ( )  GEOMETRIC_REPRESENTATION_ITEM ( )  RATIONAL_B_SPLINE_CURVE ( ( 0.9330127018922194093, 0.9330127018922194093, 1.000000000000000000, 0.8660254037844387076, 1.000000000000000000, 0.8660254037844387076, 1.000000000000000000, 0.9330127018922194093, 0.9330127018922194093 ) ) 
 REPRESENTATION_ITEM ( '' )  );
#10537 = CARTESIAN_POINT ( 'NONE',  ( 127.4000280541508516, 234.3615022471901739, 5.000000000000051514 ) ) ;
#10539 = CARTESIAN_POINT ( 'NONE',  ( 20.08504676852914628, 175.7365022471902307, -10.00000000000009237 ) ) ;
#10540 = CARTESIAN_POINT ( 'NONE',  ( 28.28448313147312021, 16.73415679381822230, 1.333680081654574804E-15 ) ) ;
#10541 = ORIENTED_EDGE ( 'NONE', *, *, #69760, .T. ) ;
#10542 = CARTESIAN_POINT ( 'NONE',  ( 184.9257308103695436, 271.4024368688196205, 16.03004893721198343 ) ) ;
#10543 = VERTEX_POINT ( 'NONE', #59959 ) ;
#10544 = CARTESIAN_POINT ( 'NONE',  ( 202.2603678735342214, 280.3217618159037556, 16.49712126737133744 ) ) ;
#10545 = LINE ( 'NONE', #73347, #19101 ) ;
#10546 = CARTESIAN_POINT ( 'NONE',  ( 150.0694502760089222, 271.4680435213315945, -12.17790201236558545 ) ) ;
#10547 = ORIENTED_EDGE ( 'NONE', *, *, #63113, .T. ) ;
#10548 = LINE ( 'NONE', #65720, #48362 ) ;
#10549 = ORIENTED_EDGE ( 'NONE', *, *, #25802, .T. ) ;
#10550 = LINE ( 'NONE', #95701, #3741 ) ;
#10551 = CARTESIAN_POINT ( 'NONE',  ( 170.7055562504701527, 250.3708107612802110, 3.163906886382704009 ) ) ;
#10552 = DIRECTION ( 'NONE',  ( 0.000000000000000000, 1.000000000000000000, 0.000000000000000000 ) ) ;
#10553 = ORIENTED_EDGE ( 'NONE', *, *, #33693, .T. ) ;
#10554 = CARTESIAN_POINT ( 'NONE',  ( 46.69726203620875538, 27.36477965099643583, 1.583844403245330712 ) ) ;
#10555 = AXIS2_PLACEMENT_3D ( 'NONE', #9408, #17504, #57490 ) ;
#10556 = CARTESIAN_POINT ( 'NONE',  ( 33.05914333415502426, 24.80170272979928470, 7.433330006724137462 ) ) ;
#10557 = CARTESIAN_POINT ( 'NONE',  ( 84.88550499454136400, 50.14668325075617616, -13.29646903481718745 ) ) ;
#10558 = CARTESIAN_POINT ( 'NONE',  ( 85.29133164726557936, 47.82314596797873918, -11.37170031403014114 ) ) ;
#10559 = CARTESIAN_POINT ( 'NONE',  ( 167.3614853001860752, 276.6147906615189527, 15.78902546434338561 ) ) ;
#10560 = CYLINDRICAL_SURFACE ( 'NONE', #4465, 70.00000000000002842 ) ;
#10561 = EDGE_LOOP ( 'NONE', ( #82408, #57906, #86639, #7103 ) ) ;
#10562 = ORIENTED_EDGE ( 'NONE', *, *, #27206, .F. ) ;
#10563 = CARTESIAN_POINT ( 'NONE',  ( 186.2060483959004102, 298.7711416952031414, 1.080402104957500331 ) ) ;
#10564 = B_SPLINE_CURVE_WITH_KNOTS ( 'NONE', 3,
 ( #58999, #60008, #43818, #27146 ),
 .UNSPECIFIED., .F., .F.,
 ( 4, 4 ),
 ( 0.04343396320418384943, 0.04853114605566435924 ),
 .UNSPECIFIED. ) ;
#10566 = CARTESIAN_POINT ( 'NONE',  ( 148.0637215040603394, 274.1931069276759558, -7.795633835291665648 ) ) ;
#10565 = CARTESIAN_POINT ( 'NONE',  ( 204.6780326111993986, 276.1342436545999703, 14.85609018352459287 ) ) ;
#10567 = CARTESIAN_POINT ( 'NONE',  ( 81.77537817921462704, 55.54508588803495428, -15.95796652904217439 ) ) ;
#10568 = CARTESIAN_POINT ( 'NONE',  ( 155.5888570658010508, 261.1591898008976500, 17.34682632352454945 ) ) ;
#10569 = CARTESIAN_POINT ( 'NONE',  ( 154.8332767207531901, 280.7459370637686220, -0.9958211956073632631 ) ) ;
#10570 = CARTESIAN_POINT ( 'NONE',  ( 70.33074575655678018, 61.13420976129943796, 14.85339103883890566 ) ) ;
#10571 = CARTESIAN_POINT ( 'NONE',  ( 207.4143746336561094, 271.3947602448195084, -4.799001228152785181 ) ) ;
#10572 = CARTESIAN_POINT ( 'NONE',  ( 169.0547802094920371, 266.9661960260407909, 17.74255763397777130 ) ) ;
#10573 = CARTESIAN_POINT ( 'NONE',  ( 79.57595289148407858, 59.38824344631919416, 16.55667218292645515 ) ) ;
#10574 = CARTESIAN_POINT ( 'NONE',  ( 84.34250105585179824, 213.3768266524160140, 9.188101187500098632 ) ) ;
#10575 = ORIENTED_EDGE ( 'NONE', *, *, #46602, .T. ) ;
#10576 = DIRECTION ( 'NONE',  ( -0.000000000000000000, 0.000000000000000000, -1.000000000000000000 ) ) ;
#10577 = CARTESIAN_POINT ( 'NONE',  ( 163.6377088202057166, 277.2438325465888056, -14.42846884688455589 ) ) ;
#10578 = EDGE_CURVE ( 'NONE', #40485, #47191, #60958, .T. ) ;
#10579 = VERTEX_POINT ( 'NONE', #28574 ) ;
#10580 = CARTESIAN_POINT ( 'NONE',  ( 167.9757358556196039, 266.9719029692253116, -17.65027412328727152 ) ) ;
#10581 = ORIENTED_EDGE ( 'NONE', *, *, #84432, .F. ) ;
#10582 = CARTESIAN_POINT ( 'NONE',  ( 201.3053657339852691, 274.7141922394133076, -14.27644254562359372 ) ) ;
#10583 = DIRECTION ( 'NONE',  ( 0.6123724356957949144, 0.3535533905933026522, -0.7071067811865326957 ) ) ;
#10584 = CARTESIAN_POINT ( 'NONE',  ( 146.7434471017767521, 276.4798892723637209, 0.7354350123930684102 ) ) ;
#10585 = CARTESIAN_POINT ( 'NONE',  ( 84.15416455708074750, 41.95829577234375307, -1.425225784223129732 ) ) ;
#10586 = CARTESIAN_POINT ( 'NONE',  ( 206.8317058779879574, 272.4039721336197317, -10.41591514895975834 ) ) ;
#10587 = CARTESIAN_POINT ( 'NONE',  ( 208.1303038335461224, 270.1547344959873840, 3.060743731163897863 ) ) ;
#10588 = CARTESIAN_POINT ( 'NONE',  ( 96.08779704679574252, 226.2833772461660260, -9.188101187500095079 ) ) ;
#10589 = ORIENTED_EDGE ( 'NONE', *, *, #82041, .F. ) ;
#10590 = VECTOR ( 'NONE', #44667, 1000.000000000000000 ) ;
#10591 = DIRECTION ( 'NONE',  ( 0.8660254037844378194, 0.5000000000000016653, 0.000000000000000000 ) ) ;
#10592 = VERTEX_POINT ( 'NONE', #91917 ) ;
#10593 = EDGE_CURVE ( 'NONE', #4283, #49899, #22473, .T. ) ;
#10594 = CARTESIAN_POINT ( 'NONE',  ( 76.10709454405099450, 64.72268328886903532, -14.35831925167281398 ) ) ;
#10595 = CARTESIAN_POINT ( 'NONE',  ( 164.9656603750091506, 286.4677819567733650, 1.164111042001980678 ) ) ;
#10596 = CARTESIAN_POINT ( 'NONE',  ( 87.51070308547132015, 44.87157588833125033, -6.586006751413206572 ) ) ;
#10597 = CARTESIAN_POINT ( 'NONE',  ( -3.965200385949115169, 158.5177522451418213, 5.000000000000051514 ) ) ;
#10598 = CARTESIAN_POINT ( 'NONE',  ( 87.78141208182009336, 44.24254441107329683, 4.709165031671993518 ) ) ;
#10599 = ORIENTED_EDGE ( 'NONE', *, *, #13600, .F. ) ;
#10600 = CARTESIAN_POINT ( 'NONE',  ( 87.23971111752899787, 44.08784344967020274, -3.737494627976594597 ) ) ;
#10601 = B_SPLINE_CURVE_WITH_KNOTS ( 'NONE', 3,
 ( #36839, #97674, #6933, #90089, #28747, #37822, #59627, #99654, #52047, #44926, #82985, #13561, #75366, #30240, #5946, #67748, #98672, #60121, #91084, #72127, #79261, #9832, #2732, #10820, #61622, #33620, #48824, #64516, #86873, #56403, #2229, #17406, #10323, #65016, #40693, #48316, #41697, #16901, #49807, #69229, #87879, #7429, #47790, #38322, #95473, #57398, #72642, #33109, #94949, #18426, #87397, #94446, #3239, #26026 ),
 .UNSPECIFIED., .F., .F.,
 ( 4, 2, 2, 2, 2, 2, 2, 2, 2, 2, 2, 2, 2, 2, 2, 2, 2, 2, 2, 2, 2, 2, 2, 2, 2, 2, 4 ),
 ( 0.001822495010402024659, 0.002272902490822721697, 0.002498106231033042461, 0.002723309971243363659, 0.002835911841348543773, 0.002948513711453724321, 0.003061115581558904435, 0.003173717451664084983, 0.003398921191874445646, 0.003624124932084806308, 0.004074532412505526766, 0.004524939892926247223, 0.005425754853767611810, 0.006326569814608976397, 0.006776977295029658691, 0.007227384775450340984, 0.007339986645555551456, 0.007396287580608187917, 0.007452588515660822643, 0.007565190385766093831, 0.007677792255871365018, 0.007902995996081869229, 0.008128199736292375174, 0.008353403476502881120, 0.008578607216713385331, 0.008803810956923891276, 0.009029014697134397222 ),
 .UNSPECIFIED. ) ;
#10602 = CARTESIAN_POINT ( 'NONE',  ( 81.16146148815955996, 46.97546385808738734, 12.48307154572201938 ) ) ;
#10603 = CARTESIAN_POINT ( 'NONE',  ( 159.7132918459648181, 254.0154592091499239, -16.90058287995827158 ) ) ;
#10604 = CARTESIAN_POINT ( 'NONE',  ( 191.0627567933567548, 271.2378347160873204, 14.18540690319008135 ) ) ;
#10605 = CARTESIAN_POINT ( 'NONE',  ( 174.6143879786744151, 283.7077023516287682, 13.57591769828411543 ) ) ;
#10606 = FACE_OUTER_BOUND ( 'NONE', #8343, .T. ) ;
#10607 = CARTESIAN_POINT ( 'NONE',  ( 139.0246627140281248, 262.6199935810940360, 2.679491924311251605 ) ) ;
#10608 = ORIENTED_EDGE ( 'NONE', *, *, #43490, .T. ) ;
#10609 = CARTESIAN_POINT ( 'NONE',  ( 3.125382611083852957, 172.6115022471902591, 10.00000000000009592 ) ) ;
#10610 = CARTESIAN_POINT ( 'NONE',  ( 200.4775477985258760, 283.4096967665721536, 16.80647240730505487 ) ) ;
#10611 = CARTESIAN_POINT ( 'NONE',  ( 83.59213118347814486, 42.01539464043647598, 3.571310749328834522 ) ) ;
#10612 = CARTESIAN_POINT ( 'NONE',  ( 167.6039016024858768, 249.9644671705272287, 7.137948275192514735 ) ) ;
#10613 = CARTESIAN_POINT ( 'NONE',  ( 83.14954596509920748, 52.21800694492112882, 14.82118944672224714 ) ) ;
#10614 = CARTESIAN_POINT ( 'NONE',  ( 178.7802048856326849, 291.7431450991714428, -6.108826784319776770 ) ) ;
#10615 = CARTESIAN_POINT ( 'NONE',  ( 163.2175214641260652, 247.9459554691067638, -11.09782983415651181 ) ) ;
#10616 = ORIENTED_EDGE ( 'NONE', *, *, #56292, .F. ) ;
#10617 = CARTESIAN_POINT ( 'NONE',  ( 36.39373221054007246, 21.41603393254327159, -1.583844403245362020 ) ) ;
#10618 = CIRCLE ( 'NONE', #51026, 11.89249999999999652 ) ;
#10619 = CARTESIAN_POINT ( 'NONE',  ( 74.33967961526438728, 63.91161072895079798, -14.20272303067961950 ) ) ;
#10621 = CARTESIAN_POINT ( 'NONE',  ( 185.4835256528986633, 266.2441379785080358, 13.04562320151002908 ) ) ;
#10620 = CARTESIAN_POINT ( 'NONE',  ( 180.6242511116918763, 266.9822466815605253, -14.84429364384706496 ) ) ;
#10622 = CARTESIAN_POINT ( 'NONE',  ( 69.58400947765115063, 62.48688437104875248, -13.40551765113508331 ) ) ;
#10623 = EDGE_CURVE ( 'NONE', #81988, #23533, #93541, .T. ) ;
#10624 = CARTESIAN_POINT ( 'NONE',  ( 34.95497629653712579, 28.38052372038643156, 10.00000000000000533 ) ) ;
#10625 = CARTESIAN_POINT ( 'NONE',  ( 152.7531861616124615, 266.0707158804971186, 17.45453282433162556 ) ) ;
#10626 = CARTESIAN_POINT ( 'NONE',  ( 81.55388316527243830, 43.41730979745093322, -9.640312318338271069 ) ) ;
#10627 = DIRECTION ( 'NONE',  ( -0.000000000000000000, -0.000000000000000000, 1.000000000000000000 ) ) ;
#10628 = CARTESIAN_POINT ( 'NONE',  ( 71.70264960794062858, 59.22880258761407646, -15.30490172258937953 ) ) ;
#10629 = VECTOR ( 'NONE', #69501, 1000.000000000000114 ) ;
#10630 = CARTESIAN_POINT ( 'NONE',  ( 156.6084421796713002, 261.3932165810376205, -17.82046942966612590 ) ) ;
#10631 = CARTESIAN_POINT ( 'NONE',  ( 207.1007598919583472, 271.9379569114424271, -6.086525981869248092 ) ) ;
#10632 = CARTESIAN_POINT ( 'NONE',  ( 11.29875767934929520, 168.1423013555409796, -4.594050593750043987 ) ) ;
#10633 = CARTESIAN_POINT ( 'NONE',  ( 81.25623871648237184, 45.26464092063801559, 11.05715119619013187 ) ) ;
#10634 = ORIENTED_EDGE ( 'NONE', *, *, #76967, .F. ) ;
#10635 = EDGE_CURVE ( 'NONE', #2437, #48869, #23325, .T. ) ;
#10636 = CARTESIAN_POINT ( 'NONE',  ( 87.13739461745468873, 46.26069895958453060, 8.495900850489460865 ) ) ;
#10637 = B_SPLINE_CURVE_WITH_KNOTS ( 'NONE', 3,
 ( #57123, #96182, #19168, #18656, #39913, #40915 ),
 .UNSPECIFIED., .F., .F.,
 ( 4, 2, 4 ),
 ( 0.01970985617426966596, 0.02425325239201692878, 0.02879664860976419161 ),
 .UNSPECIFIED. ) ;
#10638 = LINE ( 'NONE', #56722, #37010 ) ;
#10639 = DIRECTION ( 'NONE',  ( -0.7911563084720435457, -0.6116140086401625764, 0.000000000000000000 ) ) ;
#10640 = CARTESIAN_POINT ( 'NONE',  ( 35.84507844392322085, 185.3768266524159856, -9.188101187500093303 ) ) ;
#10641 = CARTESIAN_POINT ( 'NONE',  ( 161.5504728662519369, 250.8333683393111926, 12.94300825113363373 ) ) ;
#10642 = LINE ( 'NONE', #71447, #37753 ) ;
#10643 = CARTESIAN_POINT ( 'NONE',  ( 30.42216059839860165, 41.65659080271453973, -1.878358725466461243E-16 ) ) ;
#10644 = CARTESIAN_POINT ( 'NONE',  ( 200.0629734989200301, 267.3250638936581822, -6.802650431247307061 ) ) ;
#10645 = CARTESIAN_POINT ( 'NONE',  ( 176.7349755076185716, 291.6822743229055277, 2.566495134243914400 ) ) ;
#10647 = CARTESIAN_POINT ( 'NONE',  ( 149.0581491015862241, 272.4707078043124966, 11.78139744831781321 ) ) ;
#10646 = AXIS2_PLACEMENT_3D ( 'NONE', #77050, #99382, #85725 ) ;
#10648 = CARTESIAN_POINT ( 'NONE',  ( 180.2906925969918177, 272.3403866223749787, 17.68789668772514290 ) ) ;
#10649 = CARTESIAN_POINT ( 'NONE',  ( 3.113790753877909712, 26.87087736965101570, 10.00000000000000000 ) ) ;
#10650 = CARTESIAN_POINT ( 'NONE',  ( 84.07138645536940658, 51.57118087273712348, 14.70185406139690976 ) ) ;
#10651 = CARTESIAN_POINT ( 'NONE',  ( 81.50068165357551209, 227.8615022471903160, 5.000000000000046185 ) ) ;
#10652 = CARTESIAN_POINT ( 'NONE',  ( 8.754547735682661980, 185.8615022471903160, 5.000000000000046185 ) ) ;
#10653 = CARTESIAN_POINT ( 'NONE',  ( -36.26652983198114555, 26.35523046909639788, -10.00000000000000000 ) ) ;
#10654 = CARTESIAN_POINT ( 'NONE',  ( 54.70828104404427705, 193.2048013555409796, 4.594050593750051981 ) ) ;
#10655 = CARTESIAN_POINT ( 'NONE',  ( 198.1230806404959139, 287.4877535090322453, 17.00698319228197164 ) ) ;
#10656 = ORIENTED_EDGE ( 'NONE', *, *, #75850, .F. ) ;
#10657 = CARTESIAN_POINT ( 'NONE',  ( -5.341514567247151568, 81.77868734245731730, 13.39505696618104302 ) ) ;
#10658 = CARTESIAN_POINT ( 'NONE',  ( 190.9586609929293104, 299.8968923453624598, -4.970176667899034229 ) ) ;
#10659 = CARTESIAN_POINT ( 'NONE',  ( 67.02216205416458195, 66.98564243900641202, -8.693011569217512502 ) ) ;
#10660 = ORIENTED_EDGE ( 'NONE', *, *, #93453, .F. ) ;
#10661 = CARTESIAN_POINT ( 'NONE',  ( 170.4597437522810424, 286.1127027945369719, 7.473822327501647322 ) ) ;
#10662 = CARTESIAN_POINT ( 'NONE',  ( 164.7243055739305078, 245.3361288348881999, -1.445094907380085170 ) ) ;
#10663 = CARTESIAN_POINT ( 'NONE',  ( 193.3082004299502046, 295.8273706660551738, 13.84301442133521043 ) ) ;
#10664 = CARTESIAN_POINT ( 'NONE',  ( 70.66235305853896875, 64.93978938733117445, 12.81966862783717964 ) ) ;
#10665 = CARTESIAN_POINT ( 'NONE',  ( 27.58754685475307156, 27.87878583063842797, -9.188101187500006262 ) ) ;
#10666 = CARTESIAN_POINT ( 'NONE',  ( 202.6070187115982719, 279.7213449518906145, 15.56322169823762280 ) ) ;
#10667 = CARTESIAN_POINT ( 'NONE',  ( 149.0164813726494799, 272.5428784278667536, -11.67305721329070423 ) ) ;
#10668 = CARTESIAN_POINT ( 'NONE',  ( 173.4136195317119018, 256.7516932182500113, 11.26842845872458376 ) ) ;
#10669 = ORIENTED_EDGE ( 'NONE', *, *, #55561, .F. ) ;
#10670 = CARTESIAN_POINT ( 'NONE',  ( 15.73863525846626032, 14.80170272979925272, 7.433330006724137462 ) ) ;
#10671 = DIRECTION ( 'NONE',  ( -0.6123724356957797044, -0.3535533905932748411, 0.7071067811865598962 ) ) ;
#10672 = DIRECTION ( 'NONE',  ( -0.03487823687206607903, 0.06041087834084090530, 0.9975640502598237536 ) ) ;
#10673 = VERTEX_POINT ( 'NONE', #76675 ) ;
#10674 = CARTESIAN_POINT ( 'NONE',  ( 72.19109158906037749, 71.10838548458626462, -5.953967166465981897 ) ) ;
#10675 = CARTESIAN_POINT ( 'NONE',  ( 190.8443993347725325, 300.0947993426467519, 8.522468760355437212 ) ) ;
#10676 = CARTESIAN_POINT ( 'NONE',  ( 177.5792917427869497, 255.5367556796404074, -6.834657972258073144 ) ) ;
#10677 = CARTESIAN_POINT ( 'NONE',  ( 67.86860378221429357, 65.58690806574966814, -10.91583492536020472 ) ) ;
#10678 = ORIENTED_EDGE ( 'NONE', *, *, #71015, .T. ) ;
#10680 = CYLINDRICAL_SURFACE ( 'NONE', #16790, 17.82106496071139645 ) ;
#10679 = CARTESIAN_POINT ( 'NONE',  ( 207.2167723318516153, 271.7370174712370954, -6.606038862010207957 ) ) ;
#10681 = CARTESIAN_POINT ( 'NONE',  ( 196.9098758191317700, 289.5890858996224324, -16.54412079817003800 ) ) ;
#10682 = VERTEX_POINT ( 'NONE', #78689 ) ;
#10683 = CARTESIAN_POINT ( 'NONE',  ( 200.8147387322574957, 282.8256649374973790, -18.02438097732020239 ) ) ;
#10684 = CARTESIAN_POINT ( 'NONE',  ( 72.04989860578065475, 72.29315785138345518, -3.506402493552649435 ) ) ;
#10685 = CARTESIAN_POINT ( 'NONE',  ( 73.11398337492714461, 57.41976801426039856, -15.88230524335126148 ) ) ;
#10686 = CARTESIAN_POINT ( 'NONE',  ( 78.21052395450516315, 61.02929962668400066, -15.90929906019731099 ) ) ;
#10687 = CARTESIAN_POINT ( 'NONE',  ( 205.4029933437358295, 274.8785748323546159, -13.50815392427034922 ) ) ;
#10688 = CARTESIAN_POINT ( 'NONE',  ( 117.9006383567337792, 245.0024278399160949, 9.188101187500095079 ) ) ;
#10689 = CARTESIAN_POINT ( 'NONE',  ( 196.4170778717353585, 290.4426369823788718, -17.78762421190030452 ) ) ;
#10690 = CARTESIAN_POINT ( 'NONE',  ( 183.7819271391472853, 288.5527987327671440, -13.16916153635029829 ) ) ;
#10692 = EDGE_CURVE ( 'NONE', #98414, #77450, #66245, .T. ) ;
#10691 = CIRCLE ( 'NONE', #28460, 50.00000000000000711 ) ;
#10693 = ORIENTED_EDGE ( 'NONE', *, *, #87886, .T. ) ;
#10694 = CARTESIAN_POINT ( 'NONE',  ( 207.5408646414791178, 271.1756731246201753, 3.050859480894625886 ) ) ;
#10695 = VERTEX_POINT ( 'NONE', #69062 ) ;
#10696 = CARTESIAN_POINT ( 'NONE',  ( 28.38624132378439313, 39.49540643055189548, 3.479690158560446702E-15 ) ) ;
#10697 = CARTESIAN_POINT ( 'NONE',  ( 198.2114954873088948, 287.3346145022089786, 18.52864136173620935 ) ) ;
#10698 = CARTESIAN_POINT ( 'NONE',  ( 78.22897022588638549, 47.73976331551912011, -14.48630821629448384 ) ) ;
#10699 = EDGE_CURVE ( 'NONE', #14070, #29175, #41940, .T. ) ;
#10700 = CARTESIAN_POINT ( 'NONE',  ( 62.15060008387555968, 200.5643266524159856, -9.188101187500093303 ) ) ;
#10701 = CARTESIAN_POINT ( 'NONE',  ( 73.91288345017510153, 68.57868192222672121, 11.39134523673512511 ) ) ;
#10702 = CARTESIAN_POINT ( 'NONE',  ( 190.9907605556751093, 299.8412942717858414, 8.799173206188184437 ) ) ;
#10703 = CARTESIAN_POINT ( 'NONE',  ( 198.6859012307616581, 286.5129196511462624, 18.23225590904412030 ) ) ;
#10704 = VECTOR ( 'NONE', #12962, 1000.000000000000227 ) ;
#10705 = CARTESIAN_POINT ( 'NONE',  ( 172.6048621181717806, 271.8561855147940491, 17.03490788493881425 ) ) ;
#10706 = ORIENTED_EDGE ( 'NONE', *, *, #91364, .T. ) ;
#10707 = CARTESIAN_POINT ( 'NONE',  ( 78.29659894437797618, 57.29271133927426263, -16.19830913213783319 ) ) ;
#10708 = CARTESIAN_POINT ( 'NONE',  ( 199.1041333440138317, 265.1832257255362038, 0.2027868546939186056 ) ) ;
#10709 = DIRECTION ( 'NONE',  ( -0.8600446134263897147, -0.5102188382608503492, 0.000000000000000000 ) ) ;
#10710 = ORIENTED_EDGE ( 'NONE', *, *, #91820, .T. ) ;
#10711 = CARTESIAN_POINT ( 'NONE',  ( 173.1855788362566955, 260.3541085725848916, -13.89348164722228240 ) ) ;
#10712 = CARTESIAN_POINT ( 'NONE',  ( 174.2579852878230895, 277.3140177265087800, -15.60830308234947061 ) ) ;
#10713 = EDGE_CURVE ( 'NONE', #41328, #59881, #29766, .T. ) ;
#10714 = CARTESIAN_POINT ( 'NONE',  ( 161.7938256150359848, 259.1648011204742375, -16.40003089747464671 ) ) ;
#10715 = CARTESIAN_POINT ( 'NONE',  ( 206.8889038998294723, 269.8868643644167378, 1.765609235721585568 ) ) ;
#10716 = CARTESIAN_POINT ( 'NONE',  ( 190.0550686570564949, 301.4619601804237732, 4.203010638620038542 ) ) ;
#10717 = CARTESIAN_POINT ( 'NONE',  ( 177.1677292396067287, 269.5601071575461560, 16.13534633437323507 ) ) ;
#10718 = CARTESIAN_POINT ( 'NONE',  ( 186.3805605339445606, 261.9022306725897238, 10.64329021816346454 ) ) ;
#10719 = PLANE ( 'NONE',  #41218 ) ;
#10720 = CARTESIAN_POINT ( 'NONE',  ( 194.9471474500919896, 290.9886311562445371, 16.55118206508679890 ) ) ;
#10721 = CARTESIAN_POINT ( 'NONE',  ( 208.1876422586379647, 270.0554214305024630, 3.377638779759113863 ) ) ;
#10722 = CARTESIAN_POINT ( 'NONE',  ( 124.6666353716822186, 242.7833772461660544, -9.188101187500095079 ) ) ;
#10723 = EDGE_LOOP ( 'NONE', ( #84176, #16172 ) ) ;
#10724 = CIRCLE ( 'NONE', #83497, 70.00000000000001421 ) ;
#10725 = CARTESIAN_POINT ( 'NONE',  ( 86.56107662385767298, 44.24251769246640720, -5.392801405849540153 ) ) ;
#10726 = DIRECTION ( 'NONE',  ( 0.000000000000000000, 0.000000000000000000, 1.000000000000000000 ) ) ;
#10727 = CARTESIAN_POINT ( 'NONE',  ( 155.1601726304954809, 261.9016930232608615, -18.56587418422714464 ) ) ;
#10728 = EDGE_CURVE ( 'NONE', #71229, #84849, #96910, .T. ) ;
#10729 = VECTOR ( 'NONE', #70029, 1000.000000000000227 ) ;
#10730 = CARTESIAN_POINT ( 'NONE',  ( 79.49833928707691655, 59.53565285605930768, -16.19549232290340157 ) ) ;
#10731 = CARTESIAN_POINT ( 'NONE',  ( -10.31836507581447471, 176.3967562850347406, -4.648177544792955347E-16 ) ) ;
#10732 = CARTESIAN_POINT ( 'NONE',  ( 177.7461146735995214, 255.2454472211425127, 4.878792714415012277 ) ) ;
#10733 = ORIENTED_EDGE ( 'NONE', *, *, #83221, .T. ) ;
#10734 = CARTESIAN_POINT ( 'NONE',  ( 80.27314967653323663, 57.13666510169645107, -16.23447001446601590 ) ) ;
#10735 = CARTESIAN_POINT ( 'NONE',  ( 158.5161628873921131, 275.0455875265674308, -12.48876142424470714 ) ) ;
#10737 = CARTESIAN_POINT ( 'NONE',  ( 182.5145075214082340, 260.7231217271532273, 9.500621738068392830 ) ) ;
#10736 = CARTESIAN_POINT ( 'NONE',  ( 147.6238900292995879, 275.3621543041489872, 3.125955112918928691 ) ) ;
#10738 = CARTESIAN_POINT ( 'NONE',  ( 140.4447960187037552, 242.7048013555409796, 4.594050593750051981 ) ) ;
#10739 = CARTESIAN_POINT ( 'NONE',  ( -32.70869837084711662, 94.07384053862010376, 43.88975835780059498 ) ) ;
#10740 = LINE ( 'NONE', #3645, #74192 ) ;
#10741 = CARTESIAN_POINT ( 'NONE',  ( 68.13167480270307408, 200.9548013555409796, -4.594050593750042211 ) ) ;
#10742 = CARTESIAN_POINT ( 'NONE',  ( 157.8239779013331372, 257.2878469527003062, -17.92251383114021479 ) ) ;
#10743 = CARTESIAN_POINT ( 'NONE',  ( 170.6659753671055171, 250.4757724785690698, 3.524607026314700242 ) ) ;
#10744 = ADVANCED_FACE ( 'NONE', ( #2186 ), #49276, .T. ) ;
#10745 = CARTESIAN_POINT ( 'NONE',  ( 15.75562222995320560, 27.83478043621387599, -8.090169943749479842 ) ) ;
#10746 = CARTESIAN_POINT ( 'NONE',  ( 190.8072577185990610, 300.1591305089344814, 3.698484652594827171 ) ) ;
#10747 = CARTESIAN_POINT ( 'NONE',  ( 155.2672715809540591, 279.9936962574083736, -0.9937612457601998628 ) ) ;
#10748 = CARTESIAN_POINT ( 'NONE',  ( 168.9333898618331489, 285.8808315938983924, -9.126212950214783959 ) ) ;
#10749 = CARTESIAN_POINT ( 'NONE',  ( 197.8809552785519656, 287.9071269377202498, 17.61728046362068412 ) ) ;
#10750 = FACE_OUTER_BOUND ( 'NONE', #57380, .T. ) ;
#10751 = ADVANCED_FACE ( 'NONE', ( #42643 ), #53341, .F. ) ;
#10752 = CARTESIAN_POINT ( 'NONE',  ( 113.8142545287344802, 246.5177522451419065, 5.000000000000046185 ) ) ;
#10753 = CARTESIAN_POINT ( 'NONE',  ( 82.15503656874240335, 51.38971310115279323, -14.65386453280463819 ) ) ;
#10754 = ORIENTED_EDGE ( 'NONE', *, *, #16214, .F. ) ;
#10755 = EDGE_CURVE ( 'NONE', #50031, #77129, #51146, .T. ) ;
#10756 = CARTESIAN_POINT ( 'NONE',  ( 159.9924463476198753, 283.3850188831759169, -3.371971149216307140 ) ) ;
#10757 = CARTESIAN_POINT ( 'NONE',  ( -5.561934722402757991, 167.5958772461660544, -9.188101187500095079 ) ) ;
#10758 = VECTOR ( 'NONE', #96320, 1000.000000000000000 ) ;
#10759 = CARTESIAN_POINT ( 'NONE',  ( 41.69040282370318096, 201.0024278399160664, -9.188101187500093303 ) ) ;
#10760 = CARTESIAN_POINT ( 'NONE',  ( 25.28119919123577475, 178.7365022471902023, -10.00000000000009237 ) ) ;
#10761 = CARTESIAN_POINT ( 'NONE',  ( 18.12000580879176681, 26.16454794089041513, -10.00000000000000355 ) ) ;
#10762 = CARTESIAN_POINT ( 'NONE',  ( 85.93449727955278661, 48.41344338607260767, 12.08598331734388509 ) ) ;
#10763 = DIRECTION ( 'NONE',  ( 0.000000000000000000, -0.000000000000000000, 1.000000000000000000 ) ) ;
#10765 = VECTOR ( 'NONE', #25144, 1000.000000000000000 ) ;
#10764 = CARTESIAN_POINT ( 'NONE',  ( 72.24659094707693896, 72.05232748221199301, -3.244599947448891797 ) ) ;
#10766 = CARTESIAN_POINT ( 'NONE',  ( 190.7403173041394950, 300.2750747078583800, -4.254144485856557800 ) ) ;
#10767 = CARTESIAN_POINT ( 'NONE',  ( 73.97864017645115098, 55.44741841079105882, -16.11550171815304111 ) ) ;
#10768 = EDGE_CURVE ( 'NONE', #22014, #68457, #58167, .T. ) ;
#10770 = CARTESIAN_POINT ( 'NONE',  ( 62.64658692180396571, 193.6427522451417644, 1.119607411625061291E-15 ) ) ;
#10769 = CARTESIAN_POINT ( 'NONE',  ( -19.65312891409030271, 93.06504152958497400, 10.00000000000000888 ) ) ;
#10771 = CARTESIAN_POINT ( 'NONE',  ( 180.8099474207024286, 256.2767700812191265, 1.456173454511005660 ) ) ;
#10772 = CARTESIAN_POINT ( 'NONE',  ( 157.1269483542914998, 258.4951375425532092, -17.15328932028234377 ) ) ;
#10773 = CARTESIAN_POINT ( 'NONE',  ( 80.61430232155159104, 228.8967562850347122, -4.648177544792955347E-16 ) ) ;
#10774 = AXIS2_PLACEMENT_3D ( 'NONE', #13457, #83372, #68621 ) ;
#10775 = CARTESIAN_POINT ( 'NONE',  ( 47.29267820409027934, 188.1115022471902023, -5.000000000000041744 ) ) ;
#10776 = DIRECTION ( 'NONE',  ( 0.000000000000000000, 0.000000000000000000, 1.000000000000000000 ) ) ;
#10777 = CARTESIAN_POINT ( 'NONE',  ( 163.1332433029523372, 248.0919295262283981, 11.24052392390482957 ) ) ;
#10778 = CARTESIAN_POINT ( 'NONE',  ( 4.289451341410244645, 161.0327760586659451, 1.948934522072303157E-15 ) ) ;
#10779 = CARTESIAN_POINT ( 'NONE',  ( 40.22068564906490451, 26.14754757982093381, -5.678558825948276656 ) ) ;
#10780 = CARTESIAN_POINT ( 'NONE',  ( -74.33658418421376268, 48.94984639172533747, 10.00000000000000000 ) ) ;
#10781 = CARTESIAN_POINT ( 'NONE',  ( 192.1859061758433143, 297.7712413352111298, 11.15082371775444336 ) ) ;
#10782 = CARTESIAN_POINT ( 'NONE',  ( 35.11595366814305663, 25.98920272979928470, 7.433330006724137462 ) ) ;
#10783 = CARTESIAN_POINT ( 'NONE',  ( 77.09838585100463604, 221.9865022471902876, -10.00000000000009592 ) ) ;
#10784 = CARTESIAN_POINT ( 'NONE',  ( 183.1758135086024595, 257.7755843168840784, -2.206437414030474109 ) ) ;
#10785 = DIRECTION ( 'NONE',  ( -0.1239754375649672058, -0.9922852870422774751, 0.000000000000000000 ) ) ;
#10786 = CARTESIAN_POINT ( 'NONE',  ( 176.4797194055593934, 260.2797452624257630, -13.51627001118733773 ) ) ;
#10787 =( NAMED_UNIT ( * ) SI_UNIT ( $, .STERADIAN. ) SOLID_ANGLE_UNIT ( ) );
#10788 = CARTESIAN_POINT ( 'NONE',  ( 3.501222095392049649, 22.99752408145588944, 5.678558825948277544 ) ) ;
#10789 = CARTESIAN_POINT ( 'NONE',  ( 154.4302508464143102, 278.3454869111918697, -5.206030047134956540 ) ) ;
#10790 = CARTESIAN_POINT ( 'NONE',  ( 13.78045586392592092, 26.14336893147754282, 7.433330006724141015 ) ) ;
#10791 = CARTESIAN_POINT ( 'NONE',  ( 72.49386282319785835, 57.57572440859879492, 15.80166580940835885 ) ) ;
#10792 = CIRCLE ( 'NONE', #23694, 70.00000000000001421 ) ;
#10793 = LINE ( 'NONE', #3696, #64571 ) ;
#10794 = CIRCLE ( 'NONE', #83564, 70.00000000000001421 ) ;
#10795 = CARTESIAN_POINT ( 'NONE',  ( 84.55537670905214043, 50.62155581810768012, -14.09136642048690291 ) ) ;
#10796 = B_SPLINE_CURVE_WITH_KNOTS ( 'NONE', 3,
 ( #75775, #51456, #36250, #90001 ),
 .UNSPECIFIED., .F., .F.,
 ( 4, 4 ),
 ( 0.02733452390982080843, 0.03654861343160081127 ),
 .UNSPECIFIED. ) ;
#10797 = CARTESIAN_POINT ( 'NONE',  ( 87.83899792242847582, 44.00541668311378629, -1.848955303085625390 ) ) ;
#10798 = ORIENTED_EDGE ( 'NONE', *, *, #29598, .T. ) ;
#10799 = CARTESIAN_POINT ( 'NONE',  ( 152.8522706834672533, 265.8990964544007056, 17.63080661522264947 ) ) ;
#10800 = CARTESIAN_POINT ( 'NONE',  ( 207.2824254892180704, 271.6233028670009162, 6.274396967990798046 ) ) ;
#10801 = CARTESIAN_POINT ( 'NONE',  ( 66.08271157691945064, 68.62646445644681137, 4.299565650807243067 ) ) ;
#10802 = CARTESIAN_POINT ( 'NONE',  ( 116.8713438767135813, 249.8297689869268936, -2.679491924311252493 ) ) ;
#10803 = VERTEX_POINT ( 'NONE', #67448 ) ;
#10804 = EDGE_LOOP ( 'NONE', ( #67134, #91478, #90398, #20320 ) ) ;
#10805 = CARTESIAN_POINT ( 'NONE',  ( 30.84500111113854004, 63.18596212086494290, 59.99999999999999289 ) ) ;
#10806 = CARTESIAN_POINT ( 'NONE',  ( 86.15223587325151300, 47.11913640227773925, 10.79538652562921541 ) ) ;
#10807 = ORIENTED_EDGE ( 'NONE', *, *, #38391, .F. ) ;
#10808 = CARTESIAN_POINT ( 'NONE',  ( 76.54141439059615948, 51.80385272469369795, 15.68951548868696300 ) ) ;
#10809 = CARTESIAN_POINT ( 'NONE',  ( 169.8880101891228378, 248.5302279630965927, 2.598380334187264218 ) ) ;
#10810 = ORIENTED_EDGE ( 'NONE', *, *, #81375, .F. ) ;
#10811 = LINE ( 'NONE', #9823, #16722 ) ;
#10812 = CARTESIAN_POINT ( 'NONE',  ( 78.28735576227695958, 50.40689703484141404, -15.06222486931144111 ) ) ;
#10813 = CARTESIAN_POINT ( 'NONE',  ( 43.35468487962021555, 120.5828561944265687, -10.00000000000000000 ) ) ;
#10814 = CARTESIAN_POINT ( 'NONE',  ( 21.31189239132533331, 12.70852965304479198, 1.583844403245364907 ) ) ;
#10815 = ORIENTED_EDGE ( 'NONE', *, *, #56923, .T. ) ;
#10816 = CARTESIAN_POINT ( 'NONE',  ( 161.8016137473484548, 250.3983795733946636, 14.25000412375400316 ) ) ;
#10817 = CARTESIAN_POINT ( 'NONE',  ( 166.2792040466741526, 273.7071925000096826, -16.00520433647330520 ) ) ;
#10818 = CARTESIAN_POINT ( 'NONE',  ( -107.5954152546898257, 65.38554960527383741, 36.50000000000000000 ) ) ;
#10819 = ORIENTED_EDGE ( 'NONE', *, *, #85203, .F. ) ;
#10820 = CARTESIAN_POINT ( 'NONE',  ( 172.8704676289727047, 256.8043734995969771, -11.66604796816862866 ) ) ;
#10821 = DIRECTION ( 'NONE',  ( -0.9874733399847778204, -0.1577859398657163181, 0.000000000000000000 ) ) ;
#10822 = ORIENTED_EDGE ( 'NONE', *, *, #48500, .F. ) ;
#10823 = EDGE_LOOP ( 'NONE', ( #18399, #13420, #28629, #54661 ) ) ;
#10824 = CARTESIAN_POINT ( 'NONE',  ( 157.0122940985184528, 266.1029671896999389, -16.89663335517050768 ) ) ;
#10825 = ORIENTED_EDGE ( 'NONE', *, *, #17598, .F. ) ;
#10826 = CARTESIAN_POINT ( 'NONE',  ( 49.07456115661582174, 91.13648234292965356, 10.00000000000000000 ) ) ;
#10827 = EDGE_LOOP ( 'NONE', ( #589, #87160 ) ) ;
#10828 = CARTESIAN_POINT ( 'NONE',  ( 147.9411595194912934, 274.4053905120259742, 6.673340298825284123 ) ) ;
#10829 = CARTESIAN_POINT ( 'NONE',  ( 180.5607909224531227, 291.5613472329837350, -9.815939981736717002 ) ) ;
#10830 = CARTESIAN_POINT ( 'NONE',  ( 190.4083125682826392, 267.3722578230377280, -13.56112132691750105 ) ) ;
#10831 = CARTESIAN_POINT ( 'NONE',  ( -13.11024591527734451, 15.00000000000000000, 40.00000000000000000 ) ) ;
#10832 = EDGE_CURVE ( 'NONE', #21633, #81790, #98376, .T. ) ;
#10833 = DIRECTION ( 'NONE',  ( -0.000000000000000000, -0.000000000000000000, -1.000000000000000000 ) ) ;
#10834 = CARTESIAN_POINT ( 'NONE',  ( 197.1145765276632460, 289.2345338721006556, -16.80523350695997564 ) ) ;
#10835 = VERTEX_POINT ( 'NONE', #13749 ) ;
#10836 = CARTESIAN_POINT ( 'NONE',  ( 41.97168754484824404, 36.18347333012635403, -9.594050593750004907 ) ) ;
#10837 = CARTESIAN_POINT ( 'NONE',  ( 26.24098094315136009, 17.01110640527292972, 2.839279412974134775 ) ) ;
#10838 = VECTOR ( 'NONE', #68363, 1000.000000000000000 ) ;
#10839 = CARTESIAN_POINT ( 'NONE',  ( 164.2572333502590709, 246.1451216570909253, 2.155809084027023204 ) ) ;
#10841 = DIRECTION ( 'NONE',  ( 0.4999999999999998890, -0.8660254037844385966, 0.000000000000000000 ) ) ;
#10840 = CARTESIAN_POINT ( 'NONE',  ( 196.4808189786114951, 290.3322341467384717, -17.84817245450773271 ) ) ;
#10843 = ORIENTED_EDGE ( 'NONE', *, *, #17691, .T. ) ;
#10842 = CARTESIAN_POINT ( 'NONE',  ( 85.69563749947228359, 42.25122789774620458, -8.045052972278457832E-08 ) ) ;
#10844 = CIRCLE ( 'NONE', #57740, 0.1418229129684298040 ) ;
#10845 = ORIENTED_EDGE ( 'NONE', *, *, #58080, .F. ) ;
#10846 = CARTESIAN_POINT ( 'NONE',  ( 190.3269285683297198, 300.9910850015572805, 5.981691054164898880 ) ) ;
#10847 = CARTESIAN_POINT ( 'NONE',  ( 171.5510444326116613, 259.6073805218057942, -14.00194690452766189 ) ) ;
#10848 = CARTESIAN_POINT ( 'NONE',  ( 164.0005577228977529, 247.4545569590189587, 7.324775775061132421 ) ) ;
#10849 = ADVANCED_FACE ( 'NONE', ( #75563, #6152 ), #37045, .F. ) ;
#10850 = CARTESIAN_POINT ( 'NONE',  ( 25.98835327777827686, 41.64452202306098627, -10.00000000000000000 ) ) ;
#10851 = EDGE_CURVE ( 'NONE', #34369, #74676, #35497, .T. ) ;
#10852 = CARTESIAN_POINT ( 'NONE',  ( 199.4035972599234867, 285.2698336642472441, -18.06228912948296284 ) ) ;
#10853 = CARTESIAN_POINT ( 'NONE',  ( 148.6048294702719375, 273.2558804378169839, -10.20107683747840888 ) ) ;
#10854 = EDGE_LOOP ( 'NONE', ( #26739, #88446, #95814, #1454 ) ) ;
#10855 = CYLINDRICAL_SURFACE ( 'NONE', #91491, 14.99999999999968381 ) ;
#10856 = AXIS2_PLACEMENT_3D ( 'NONE', #59281, #90260, #20830 ) ;
#10857 =( BOUNDED_CURVE ( )  B_SPLINE_CURVE ( 2, ( #51508, #74839, #13037, #12529, #4413, #59081, #58593, #14012, #83445, #44891, #90052, #66221, #21134 ),
 .UNSPECIFIED., .F., .T. ) 
 B_SPLINE_CURVE_WITH_KNOTS ( ( 3, 2, 2, 2, 2, 2, 3 ),
 ( 0.1125000000000000028, 0.1150000000000000050, 0.1199999999999999956, 0.1250000000000000000, 0.1300000000000000044, 0.1350000000000000089, 0.1375000000000000111 ),
 .UNSPECIFIED. ) 
 CURVE ( )  GEOMETRIC_REPRESENTATION_ITEM ( )  RATIONAL_B_SPLINE_CURVE ( ( 0.9755282581475768211, 0.9755282581475768211, 1.000000000000000000, 0.9510565162951535312, 1.000000000000000000, 0.9510565162951535312, 1.000000000000000000, 0.9510565162951535312, 1.000000000000000000, 0.9510565162951535312, 1.000000000000000000, 0.9755282581475768211, 0.9755282581475768211 ) ) 
 REPRESENTATION_ITEM ( '' )  );
#10858 = CARTESIAN_POINT ( 'NONE',  ( 43.23318412030271674, 205.7677522451419350, -5.000000000000047962 ) ) ;
#10859 = VECTOR ( 'NONE', #20112, 1000.000000000000114 ) ;
#10860 = CARTESIAN_POINT ( 'NONE',  ( -104.9999999999999858, 93.06504152958497400, 54.99999999999999289 ) ) ;
#10861 = CARTESIAN_POINT ( 'NONE',  ( 23.81978131880161342, 177.8927522451418213, -10.00000000000009059 ) ) ;
#10862 = CARTESIAN_POINT ( 'NONE',  ( 104.0717290597573026, 221.7048013555409796, 4.594050593750051981 ) ) ;
#10863 = CARTESIAN_POINT ( 'NONE',  ( 180.7931344147162349, 294.0809750825963533, -2.761424145458095225 ) ) ;
#10864 = CARTESIAN_POINT ( 'NONE',  ( 12.22230530498201873, 30.55466486950698624, -1.111400068045478839E-16 ) ) ;
#10865 = CARTESIAN_POINT ( 'NONE',  ( 207.5603179267596374, 271.1419790461399089, 2.162348062361596490 ) ) ;
#10866 = CARTESIAN_POINT ( 'NONE',  ( 22.50244069716294959, 192.9869531367911293, 4.594050593750046652 ) ) ;
#10867 = CARTESIAN_POINT ( 'NONE',  ( 200.6129772034685175, 283.1751261563724142, 18.36811917402039640 ) ) ;
#10868 = ORIENTED_EDGE ( 'NONE', *, *, #66377, .T. ) ;
#10869 = AXIS2_PLACEMENT_3D ( 'NONE', #92828, #40073, #85240 ) ;
#10870 = ORIENTED_EDGE ( 'NONE', *, *, #37336, .T. ) ;
#10871 = CARTESIAN_POINT ( 'NONE',  ( 185.9634666876222866, 260.4317438331094081, -5.811366535968028657 ) ) ;
#10872 = CARTESIAN_POINT ( 'NONE',  ( 180.4448332398771129, 260.5583812017072205, 12.70931349753900008 ) ) ;
#10873 = CARTESIAN_POINT ( 'NONE',  ( 194.3204549332184001, 264.5487851543980469, -4.361261795965002186 ) ) ;
#10874 = CARTESIAN_POINT ( 'NONE',  ( 183.0847682432378463, 284.5747524302673241, 14.98238360739832764 ) ) ;
#10875 = CARTESIAN_POINT ( 'NONE',  ( 168.0462690533684338, 251.4142709888886884, 10.74789308012043954 ) ) ;
#10876 = EDGE_CURVE ( 'NONE', #78230, #64662, #38022, .T. ) ;
#10877 = CARTESIAN_POINT ( 'NONE',  ( 48.78150646083578579, 186.7202760586659736, -5.415160957724236172E-17 ) ) ;
#10878 = CARTESIAN_POINT ( 'NONE',  ( 84.80240350195582266, 219.7677522451418497, 10.00000000000009592 ) ) ;
#10879 = B_SPLINE_CURVE_WITH_KNOTS ( 'NONE', 3,
 ( #22100, #52996, #61084, #5416 ),
 .UNSPECIFIED., .F., .F.,
 ( 4, 4 ),
 ( 0.02303826909059158295, 0.03226139655626733549 ),
 .UNSPECIFIED. ) ;
#10880 = ORIENTED_EDGE ( 'NONE', *, *, #93051, .F. ) ;
#10881 = CARTESIAN_POINT ( 'NONE',  ( 83.93631839880838186, 47.12607340849465487, 11.39547821726712051 ) ) ;
#10882 = EDGE_CURVE ( 'NONE', #96562, #91318, #68933, .T. ) ;
#10883 = EDGE_CURVE ( 'NONE', #20265, #19444, #24349, .T. ) ;
#10884 = CARTESIAN_POINT ( 'NONE',  ( 158.2696483452693030, 282.4806668385787134, -1.679042238831097489 ) ) ;
#10885 = CARTESIAN_POINT ( 'NONE',  ( 6.724974241671477060, 168.5643266524160424, 9.188101187500095079 ) ) ;
#10886 = EDGE_CURVE ( 'NONE', #16870, #13446, #1051, .T. ) ;
#10887 = CARTESIAN_POINT ( 'NONE',  ( 68.70336459149662289, 64.02807437409755664, -12.02912010802727316 ) ) ;
#10888 = CARTESIAN_POINT ( 'NONE',  ( 151.4428545556028780, 268.3402767968688067, -15.03309903163500749 ) ) ;
#10889 = CARTESIAN_POINT ( 'NONE',  ( -22.42236680055709641, 157.8615022471902591, 0.000000000000000000 ) ) ;
#10890 = CARTESIAN_POINT ( 'NONE',  ( 193.0065576635309412, 296.3498312632291913, -11.90044991639595295 ) ) ;
#10891 = CARTESIAN_POINT ( 'NONE',  ( 169.3986711591969367, 265.8083199790463027, 17.66272553310151494 ) ) ;
#10892 = CARTESIAN_POINT ( 'NONE',  ( 204.1793240545508752, 276.9980322128846524, 14.17550310845996187 ) ) ;
#10893 = CARTESIAN_POINT ( 'NONE',  ( 191.0862225170008628, 299.6759493045793192, -9.402218231374108726 ) ) ;
#10894 = CARTESIAN_POINT ( 'NONE',  ( 206.9258336080761183, 272.2409381227055292, 6.776000910836894597 ) ) ;
#10895 = EDGE_LOOP ( 'NONE', ( #61637, #32246, #11883, #4466 ) ) ;
#10896 = CARTESIAN_POINT ( 'NONE',  ( 0.5273063997305368344, 171.1115022471902591, 10.00000000000009592 ) ) ;
#10897 = CARTESIAN_POINT ( 'NONE',  ( -71.61465314115659453, 63.06504152958490295, 203.6502102582797420 ) ) ;
#10898 = MANIFOLD_SOLID_BREP ( 'Chamfer4', #10290 ) ;
#10899 = CARTESIAN_POINT ( 'NONE',  ( 124.1257165900819359, 230.2202760586659736, -5.415160957724236172E-17 ) ) ;
#10900 = CARTESIAN_POINT ( 'NONE',  ( 18.53877768333398990, 26.10171378149918198, 9.188101187500008038 ) ) ;
#10901 = B_SPLINE_CURVE_WITH_KNOTS ( 'NONE', 3,
 ( #44256, #51880, #59444, #14856 ),
 .UNSPECIFIED., .F., .F.,
 ( 4, 4 ),
 ( 0.04471951162845413247, 0.04887066958154934887 ),
 .UNSPECIFIED. ) ;
#10902 = CARTESIAN_POINT ( 'NONE',  ( 75.07027850253338386, 67.11046765588916685, 13.07895222455245232 ) ) ;
#10903 = CARTESIAN_POINT ( 'NONE',  ( 151.1920263787787349, 270.5503660113284923, 14.04656984271712439 ) ) ;
#10905 = LINE ( 'NONE', #72727, #21490 ) ;
#10904 = CARTESIAN_POINT ( 'NONE',  ( 195.7617614321055157, 291.5776783508526364, 16.33009124109666033 ) ) ;
#10906 = CARTESIAN_POINT ( 'NONE',  ( 190.7283810415139271, 300.2957489211784718, -7.863702551849829803 ) ) ;
#10907 = VERTEX_POINT ( 'NONE', #7642 ) ;
#10908 = CARTESIAN_POINT ( 'NONE',  ( 189.9271880503060572, 261.0444523307733675, -4.592131172855204113 ) ) ;
#10909 = CARTESIAN_POINT ( 'NONE',  ( 196.7130436017243653, 289.9300093007386749, -16.33278734947153765 ) ) ;
#10910 = VECTOR ( 'NONE', #94141, 1000.000000000000114 ) ;
#10911 = CARTESIAN_POINT ( 'NONE',  ( 190.2911366393398680, 300.0106470811841177, 4.501196058731199656 ) ) ;
#10912 = CARTESIAN_POINT ( 'NONE',  ( 176.3606141446090874, 292.2811541075674313, -1.103747915900352705 ) ) ;
#10913 = CARTESIAN_POINT ( 'NONE',  ( 81.56748776902772136, 55.16552677673315941, -15.91734106113700342 ) ) ;
#10914 = ORIENTED_EDGE ( 'NONE', *, *, #90879, .T. ) ;
#10915 = CARTESIAN_POINT ( 'NONE',  ( 189.0809633534686043, 265.6194490791910994, 11.75540354764823547 ) ) ;
#10916 = CYLINDRICAL_SURFACE ( 'NONE', #99310, 17.82106496071139645 ) ;
#10917 = VECTOR ( 'NONE', #14864, 1000.000000000000000 ) ;
#10918 = CARTESIAN_POINT ( 'NONE',  ( 168.6645287092987360, 271.8237458140437752, -17.23257543817958037 ) ) ;
#10919 = CARTESIAN_POINT ( 'NONE',  ( 72.08176305907363712, 72.32341480998664451, 0.8068646397873169285 ) ) ;
#10920 = B_SPLINE_SURFACE_WITH_KNOTS ( 'NONE', 3, 1, ( 
 ( #48697, #10196 ),
 ( #77604, #1606 ),
 ( #32490, #63383 ),
 ( #24878, #55752 ),
 ( #17279, #41061 ),
 ( #48183, #9709 ),
 ( #71998, #15772 ),
 ( #81618, #3123 ),
 ( #95839, #42560 ),
 ( #64893, #72514 ),
 ( #11210, #18299 ),
 ( #49677, #96827 ),
 ( #88246, #4580 ),
 ( #4077, #74506 ),
 ( #10694, #27390 ),
 ( #82129, #96322 ),
 ( #20289, #12191 ),
 ( #73009, #58273 ),
 ( #33491, #89248 ),
 ( #58758, #43050 ),
 ( #19799, #65379 ),
 ( #26393, #51166 ),
 ( #50666, #73494 ),
 ( #34008, #3601 ),
 ( #73995, #18795 ),
 ( #49196, #57271 ),
 ( #56777, #35475 ),
 ( #19317, #66379 ),
 ( #80633, #80131 ),
 ( #97309, #34968 ),
 ( #87760, #50180 ),
 ( #27876, #42077 ),
 ( #88744, #34480 ),
 ( #26891, #89728 ) ),
 .UNSPECIFIED., .T., .F., .F.,
 ( 4, 2, 2, 2, 2, 2, 2, 2, 2, 2, 2, 2, 2, 2, 2, 2, 4 ),
 ( 2, 2 ),
 ( 0.000000000000000000, 0.06250000000000000000, 0.1250000000000000000, 0.1875000000000000000, 0.2500000000000000000, 0.3125000000000000000, 0.3750000000000000000, 0.4375000000000000000, 0.5000000000000000000, 0.5625000000000000000, 0.6250000000000000000, 0.6875000000000000000, 0.7500000000000000000, 0.8125000000000000000, 0.8750000000000000000, 0.9375000000000000000, 1.000000000000000000 ),
 ( 0.000000000000000000, 1.000000000000000000 ),
 .UNSPECIFIED. ) ;
#10921 = CARTESIAN_POINT ( 'NONE',  ( 196.3917908427449106, 270.9162700290431758, 12.02664507717766895 ) ) ;
#10922 = CARTESIAN_POINT ( 'NONE',  ( 156.7442704525034571, 261.1579551113846378, 17.82061976529222846 ) ) ;
#10923 = CARTESIAN_POINT ( 'NONE',  ( 177.9342434413450746, 262.3724634088865173, 14.97940413522559311 ) ) ;
#10924 = CARTESIAN_POINT ( 'NONE',  ( 148.2612186747170711, 275.6732389230651847, 6.000192647976810179 ) ) ;
#10925 = AXIS2_PLACEMENT_3D ( 'NONE', #55046, #78378, #18578 ) ;
#10926 = ORIENTED_EDGE ( 'NONE', *, *, #77533, .F. ) ;
#10927 = CARTESIAN_POINT ( 'NONE',  ( 190.8747839792335412, 280.8223637028987127, 16.64593989182785805 ) ) ;
#10928 = CARTESIAN_POINT ( 'NONE',  ( 7.283862947486897887, 19.90829794293878408, 10.00000000000000355 ) ) ;
#10929 = CARTESIAN_POINT ( 'NONE',  ( 195.0281415497474882, 290.0432247540097705, -16.40372058219452356 ) ) ;
#10930 = ORIENTED_EDGE ( 'NONE', *, *, #86734, .F. ) ;
#10931 = CARTESIAN_POINT ( 'NONE',  ( 77.73453021100772276, 61.59708935479353897, 16.08607222837813566 ) ) ;
#10932 = EDGE_CURVE ( 'NONE', #25358, #30622, #12929, .T. ) ;
#10933 = CARTESIAN_POINT ( 'NONE',  ( 194.6310785344323904, 293.5360785768717165, -14.54510914272505495 ) ) ;
#10934 = CARTESIAN_POINT ( 'NONE',  ( 165.1399196574946018, 246.6162641258139843, 5.603258891903981187 ) ) ;
#10935 = ORIENTED_EDGE ( 'NONE', *, *, #45369, .T. ) ;
#10936 = CARTESIAN_POINT ( 'NONE',  ( 78.86219776201926379, 59.55369065033507070, 16.50996775951928441 ) ) ;
#10937 = CARTESIAN_POINT ( 'NONE',  ( -17.42236680055705023, 149.2012482093457777, 0.000000000000000000 ) ) ;
#10938 = CARTESIAN_POINT ( 'NONE',  ( 88.10271290040205372, 43.80081590334129515, -2.139902876137079080 ) ) ;
#10939 = DIRECTION ( 'NONE',  ( -0.8660254037844379305, -0.5000000000000014433, -0.000000000000000000 ) ) ;
#10940 = AXIS2_PLACEMENT_3D ( 'NONE', #40598, #71536, #78634 ) ;
#10941 = B_SPLINE_CURVE_WITH_KNOTS ( 'NONE', 3,
 ( #84965, #15509, #61115, #22637, #62105, #16523, #31219, #23607, #46928, #94070, #328, #45421, #15016, #55503 ),
 .UNSPECIFIED., .F., .F.,
 ( 4, 2, 2, 2, 2, 2, 4 ),
 ( 0.0009227269066335377912, 0.001449417115908541165, 0.001712762220546040250, 0.001976107325183539334, 0.002239452429821038419, 0.002502797534458537504, 0.003029487743733528735 ),
 .UNSPECIFIED. ) ;
#10942 = CARTESIAN_POINT ( 'NONE',  ( 73.47309087361824709, 69.99741330878467238, -9.625970422713120200 ) ) ;
#10943 = CARTESIAN_POINT ( 'NONE',  ( 84.63209989742584582, 49.90680382888324118, -13.65945482025744795 ) ) ;
#10944 = CARTESIAN_POINT ( 'NONE',  ( 155.4661767250933622, 261.3716783840932294, -17.10192542004562810 ) ) ;
#10945 = ORIENTED_EDGE ( 'NONE', *, *, #59166, .T. ) ;
#10946 = ORIENTED_EDGE ( 'NONE', *, *, #17964, .T. ) ;
#10947 = B_SPLINE_CURVE_WITH_KNOTS ( 'NONE', 3,
 ( #67965, #29463, #21860, #52744 ),
 .UNSPECIFIED., .F., .F.,
 ( 4, 4 ),
 ( 0.03703073727535406701, 0.04566479234050394020 ),
 .UNSPECIFIED. ) ;
#10948 = CARTESIAN_POINT ( 'NONE',  ( 105.9243544191296422, 220.4155109091896065, 2.679491924311254714 ) ) ;
#10949 = ORIENTED_EDGE ( 'NONE', *, *, #95172, .F. ) ;
#10950 = PLANE ( 'NONE',  #80582 ) ;
#10951 = ORIENTED_EDGE ( 'NONE', *, *, #60800, .F. ) ;
#10952 = CARTESIAN_POINT ( 'NONE',  ( 173.3453504041607971, 270.5580986211186314, 17.57651758220006855 ) ) ;
#10953 = CARTESIAN_POINT ( 'NONE',  ( 203.3205561747472814, 278.4854618126124706, -15.14439614831292147 ) ) ;
#10954 = ORIENTED_EDGE ( 'NONE', *, *, #161, .T. ) ;
#10955 = VECTOR ( 'NONE', #26355, 1000.000000000000114 ) ;
#10956 = CARTESIAN_POINT ( 'NONE',  ( 82.40463100666525520, 40.71042483417762980, 3.199549863589999266 ) ) ;
#10957 = CARTESIAN_POINT ( 'NONE',  ( 161.6049555880495063, 255.0146571223070282, -15.06743769531358623 ) ) ;
#10958 = CARTESIAN_POINT ( 'NONE',  ( 161.9909766791130608, 277.5219621271734241, -13.08164419582714721 ) ) ;
#10959 = CARTESIAN_POINT ( 'NONE',  ( 146.9129474150286683, 276.1863061179126930, -5.016087650759920358 ) ) ;
#10960 = CARTESIAN_POINT ( 'NONE',  ( 200.9445292274600092, 282.6008612054670266, -16.62830946367346741 ) ) ;
#10961 = LINE ( 'NONE', #33238, #87412 ) ;
#10962 = EDGE_CURVE ( 'NONE', #6447, #42087, #89299, .T. ) ;
#10963 = CARTESIAN_POINT ( 'NONE',  ( 157.4545252365239776, 280.7287273452560612, 2.083561193472878603 ) ) ;
#10964 = CARTESIAN_POINT ( 'NONE',  ( 132.2983106946500982, 253.3149278399160949, -9.188101187500095079 ) ) ;
#10965 = CARTESIAN_POINT ( 'NONE',  ( 70.93212201657662774, 61.12454710469379648, -14.47427800527280795 ) ) ;
#10966 = B_SPLINE_CURVE_WITH_KNOTS ( 'NONE', 3,
 ( #24197, #93124, #55078, #1905, #94630, #23675, #47486, #17594, #78411, #54567, #8992, #32786, #16092, #70800, #63694, #86554, #1409, #48503, #32290, #25187, #63191, #17086, #56069, #47978 ),
 .UNSPECIFIED., .F., .F.,
 ( 4, 2, 2, 2, 2, 2, 2, 2, 2, 2, 2, 4 ),
 ( 0.000000000000000000, 0.1250000000000144884, 0.2500000000000289768, 0.3750000000000434652, 0.4375000000000391354, 0.5000000000000348610, 0.5625000000000305311, 0.6250000000000262013, 0.6875000000000219824, 0.7500000000000176525, 0.8750000000000087708, 1.000000000000000000 ),
 .UNSPECIFIED. ) ;
#10967 = CARTESIAN_POINT ( 'NONE',  ( 45.07042791025775585, 28.94754757982093452, 5.678558825948272215 ) ) ;
#10968 = ORIENTED_EDGE ( 'NONE', *, *, #80428, .T. ) ;
#10970 = VERTEX_POINT ( 'NONE', #10536 ) ;
#10969 = CARTESIAN_POINT ( 'NONE',  ( 85.90518370574052653, 43.58569018707092368, -5.829448724985482500 ) ) ;
#10971 = CARTESIAN_POINT ( 'NONE',  ( 13.67211979723576931, 32.92651376809308772, -10.00000000000000000 ) ) ;
#10972 = CARTESIAN_POINT ( 'NONE',  ( 162.7561251957091031, 248.7451172484279027, 11.07313294959361194 ) ) ;
#10973 = CARTESIAN_POINT ( 'NONE',  ( 120.7221038307704788, 252.0530062829862743, -4.648177544792955347E-16 ) ) ;
#10974 = CARTESIAN_POINT ( 'NONE',  ( -71.61465314115659453, 63.06504152958490295, -40.00000000000000711 ) ) ;
#10975 = CARTESIAN_POINT ( 'NONE',  ( 152.7626916759926985, 277.8440032964028887, 6.837158938718278733 ) ) ;
#10976 = EDGE_CURVE ( 'NONE', #84127, #59353, #14903, .T. ) ;
#10977 = CARTESIAN_POINT ( 'NONE',  ( 153.1627746953036535, 265.3612877299463548, -17.72069958822647351 ) ) ;
#10978 = CARTESIAN_POINT ( 'NONE',  ( 78.12943550715658603, 47.76092654452022401, 14.52429885557054057 ) ) ;
#10979 = CARTESIAN_POINT ( 'NONE',  ( 170.9811431790156462, 280.9458665424763240, 14.82329785628973440 ) ) ;
#10980 = EDGE_CURVE ( 'NONE', #40695, #50208, #3926, .T. ) ;
#10981 = CARTESIAN_POINT ( 'NONE',  ( 76.31143563843063760, 51.61816296641098489, -15.67522282572066850 ) ) ;
#10982 = CARTESIAN_POINT ( 'NONE',  ( 15.77038241084232517, 34.14663330942826747, 10.00000000000000000 ) ) ;
#10983 = ORIENTED_EDGE ( 'NONE', *, *, #13269, .T. ) ;
#10984 = CARTESIAN_POINT ( 'NONE',  ( 184.7187487274096327, 272.8151481436858035, -17.12587133286889696 ) ) ;
#10985 = CARTESIAN_POINT ( 'NONE',  ( 76.01432959614969320, 61.89104940659418475, -15.35760132559815005 ) ) ;
#10986 = ORIENTED_EDGE ( 'NONE', *, *, #62898, .T. ) ;
#10987 = AXIS2_PLACEMENT_3D ( 'NONE', #28190, #59066, #20610 ) ;
#10989 = CARTESIAN_POINT ( 'NONE',  ( -19.65312891409030271, 93.06504152958497400, 59.99999999999999289 ) ) ;
#10988 = B_SPLINE_CURVE_WITH_KNOTS ( 'NONE', 3,
 ( #56662, #77979, #71886, #93707 ),
 .UNSPECIFIED., .F., .F.,
 ( 4, 4 ),
 ( 0.03198279863331025819, 0.04097217294255945524 ),
 .UNSPECIFIED. ) ;
#10990 = CARTESIAN_POINT ( 'NONE',  ( 156.7543839089325957, 276.7182480148175046, 10.07123213494488212 ) ) ;
#10991 = CARTESIAN_POINT ( 'NONE',  ( 152.1196796635681494, 267.1679813220347910, -17.00838471677149144 ) ) ;
#10992 = CARTESIAN_POINT ( 'NONE',  ( -86.81108781737714253, -8.000000000000000000, 0.000000000000000000 ) ) ;
#10993 = VECTOR ( 'NONE', #26656, 1000.000000000000000 ) ;
#10994 = CARTESIAN_POINT ( 'NONE',  ( 202.9689790241539242, 279.0944113002206564, 15.85114608332523289 ) ) ;
#10996 = CARTESIAN_POINT ( 'NONE',  ( 87.80273158879131756, 44.12514266115443462, 2.714529260603524286 ) ) ;
#10995 = CARTESIAN_POINT ( 'NONE',  ( 42.76202708541288899, 64.24573752441608576, -10.00000000000000000 ) ) ;
#10997 = CARTESIAN_POINT ( 'NONE',  ( -18.15312891409030627, 78.77562236714182120, 52.49999999999999289 ) ) ;
#10998 = ORIENTED_EDGE ( 'NONE', *, *, #46067, .F. ) ;
#10999 = CIRCLE ( 'NONE', #38427, 70.00000000000001421 ) ;
#11000 = CARTESIAN_POINT ( 'NONE',  ( 2.096977440541873516, 182.0177522451419350, 5.000000000000046185 ) ) ;
#11001 = DIRECTION ( 'NONE',  ( -0.6384778167143363437, 0.7696402260561061581, 0.000000000000000000 ) ) ;
#11002 = CARTESIAN_POINT ( 'NONE',  ( 75.45848158068072564, 64.88927211188989475, -14.08658606194572727 ) ) ;
#11003 = DIRECTION ( 'NONE',  ( -0.2575544297740129385, 0.9662637919863205083, 0.000000000000000000 ) ) ;
#11004 = VECTOR ( 'NONE', #21742, 1000.000000000000000 ) ;
#11005 = CARTESIAN_POINT ( 'NONE',  ( 80.96872438510855829, 43.68017817554169113, -9.540616427834850199 ) ) ;
#11006 = DIRECTION ( 'NONE',  ( -0.8660254037844387076, -0.4999999999999998890, -0.000000000000000000 ) ) ;
#11007 = EDGE_CURVE ( 'NONE', #75397, #49368, #11371, .T. ) ;
#11008 = CARTESIAN_POINT ( 'NONE',  ( 162.8789161433191452, 248.5324370884573568, 9.731756914259689140 ) ) ;
#11009 = CARTESIAN_POINT ( 'NONE',  ( 6.724974241671478836, 168.5643266524160140, 9.188101187500095079 ) ) ;
#11010 = CARTESIAN_POINT ( 'NONE',  ( 102.2582280487598609, 229.8458772461660544, 9.188101187500095079 ) ) ;
#11011 = CARTESIAN_POINT ( 'NONE',  ( 88.11801461435689475, 44.35549720747543745, -4.463913325698415591 ) ) ;
#11012 = CARTESIAN_POINT ( 'NONE',  ( 180.0322305761642383, 254.9176317891389090, -2.436366251733914190 ) ) ;
#11013 = CYLINDRICAL_SURFACE ( 'NONE', #7561, 16.60714546451156792 ) ;
#11014 = VECTOR ( 'NONE', #31568, 1000.000000000000000 ) ;
#11015 = LINE ( 'NONE', #42373, #81487 ) ;
#11016 = CARTESIAN_POINT ( 'NONE',  ( 172.5994563415556513, 290.7548730510699784, 2.767649011580872731 ) ) ;
#11017 = CARTESIAN_POINT ( 'NONE',  ( 164.2149278243714150, 284.2439244671650727, 5.824652686812012981 ) ) ;
#11018 = FACE_OUTER_BOUND ( 'NONE', #49428, .T. ) ;
#11019 = CARTESIAN_POINT ( 'NONE',  ( 178.1946494622069395, 290.5425167686889267, 9.940919530699707352 ) ) ;
#11020 = EDGE_CURVE ( 'NONE', #98801, #63065, #24597, .T. ) ;
#11021 = CARTESIAN_POINT ( 'NONE',  ( 205.5756302247097267, 274.5795589832478640, -13.28165401105990640 ) ) ;
#11022 = DIRECTION ( 'NONE',  ( 0.8660254037844384856, 0.5000000000000002220, -5.782411586589354927E-17 ) ) ;
#11023 = CARTESIAN_POINT ( 'NONE',  ( 80.06011714963352688, 53.70964243608271005, -16.15649400312684492 ) ) ;
#11024 = CARTESIAN_POINT ( 'NONE',  ( 176.0325359971707542, 265.4089874483971130, -16.36978886597187355 ) ) ;
#11025 = CARTESIAN_POINT ( 'NONE',  ( 79.20030167299918844, 216.5333772461660544, 9.188101187500095079 ) ) ;
#11026 = CARTESIAN_POINT ( 'NONE',  ( 207.1770866921659717, 271.8057550155037347, -5.569195235244989384 ) ) ;
#11027 = DIRECTION ( 'NONE',  ( -0.9946578707245747886, -0.1032265479692855564, 0.000000000000000000 ) ) ;
#11028 = CARTESIAN_POINT ( 'NONE',  ( 163.4176914027354997, 257.9558872812714299, 15.60721039003836808 ) ) ;
#11029 = CARTESIAN_POINT ( 'NONE',  ( 83.16599801226564637, 42.97050380912442336, -7.691725848249192588 ) ) ;
#11030 = EDGE_CURVE ( 'NONE', #43292, #8402, #65223, .T. ) ;
#11031 = CARTESIAN_POINT ( 'NONE',  ( 176.3672203485075727, 269.8998402218351202, -17.39506173205459305 ) ) ;
#11032 = CARTESIAN_POINT ( 'NONE',  ( 34.51455378690028652, 28.43085787977765477, -9.188101187500008038 ) ) ;
#11033 = CARTESIAN_POINT ( 'NONE',  ( 83.70644011242923455, 48.17923023345559841, -12.88485594781891841 ) ) ;
#11034 = CARTESIAN_POINT ( 'NONE',  ( 14.42807667092211865, 8.734156793818204534, -7.779800476318352071E-15 ) ) ;
#11035 = EDGE_LOOP ( 'NONE', ( #76855, #93072, #13158, #90200 ) ) ;
#11036 = CARTESIAN_POINT ( 'NONE',  ( 21.36958804686389612, 14.19860640527291906, 2.839279412974134775 ) ) ;
#11037 = CARTESIAN_POINT ( 'NONE',  ( 67.72511797709034909, 222.1589784336661637, -6.496448406907676862E-16 ) ) ;
#11038 = CARTESIAN_POINT ( 'NONE',  ( 75.28650001057751240, 66.67572118895704136, 13.44401380721711270 ) ) ;
#11039 = CARTESIAN_POINT ( 'NONE',  ( 169.4352824855270399, 288.1566314908686763, -1.095578661510785423 ) ) ;
#11040 = CARTESIAN_POINT ( 'NONE',  ( 192.5076277540105423, 297.2140032159341558, -13.10094381206144298 ) ) ;
#11041 = CARTESIAN_POINT ( 'NONE',  ( 200.1233510698300222, 282.0231834965481994, 17.42297826929840809 ) ) ;
#11042 = DIRECTION ( 'NONE',  ( 0.000000000000000000, -0.000000000000000000, -1.000000000000000000 ) ) ;
#11043 = CARTESIAN_POINT ( 'NONE',  ( 190.0370014622527322, 286.8089957100377205, 16.96978714573610247 ) ) ;
#11044 = CARTESIAN_POINT ( 'NONE',  ( 72.45903907735083749, 71.58914108862926184, 5.178295322198071204 ) ) ;
#11045 = CARTESIAN_POINT ( 'NONE',  ( 128.3382222415839919, 238.2365022471902307, 10.00000000000009592 ) ) ;
#11046 = CARTESIAN_POINT ( 'NONE',  ( 157.1850763439666139, 258.3944569110938687, -16.98181238659443437 ) ) ;
#11047 = CARTESIAN_POINT ( 'NONE',  ( 19.10612102538523160, 34.52903772873358434, -1.583844403245329602 ) ) ;
#11048 = VERTEX_POINT ( 'NONE', #34326 ) ;
#11049 = AXIS2_PLACEMENT_3D ( 'NONE', #65578, #50871, #42267 ) ;
#11050 = CARTESIAN_POINT ( 'NONE',  ( 169.5996950482089574, 248.5186537671148699, -1.940243715008109993 ) ) ;
#11051 = VERTEX_POINT ( 'NONE', #96166 ) ;
#11052 = CARTESIAN_POINT ( 'NONE',  ( 163.0683798854284703, 248.2042762609320903, 11.26611642476872710 ) ) ;
#11053 = DIRECTION ( 'NONE',  ( 0.4755282581475757664, -0.8236391035463335175, -0.3090169943749448977 ) ) ;
#11054 = EDGE_CURVE ( 'NONE', #87622, #37700, #66227, .T. ) ;
#11055 = DIRECTION ( 'NONE',  ( 1.000000000000000000, 0.000000000000000000, 0.000000000000000000 ) ) ;
#11056 = VERTEX_POINT ( 'NONE', #28215 ) ;
#11057 = CARTESIAN_POINT ( 'NONE',  ( 1.023347710557721113, 26.18841396516314646, -10.00000000000000000 ) ) ;
#11058 = ORIENTED_EDGE ( 'NONE', *, *, #46785, .F. ) ;
#11059 = CARTESIAN_POINT ( 'NONE',  ( 71.96464922262767061, 71.55750601381073750, 5.589292941210044496 ) ) ;
#11060 = CARTESIAN_POINT ( 'NONE',  ( 171.2741013746033332, 249.3936815359432728, 2.927055546763141169 ) ) ;
#11061 = CARTESIAN_POINT ( 'NONE',  ( 194.1631857443810816, 280.7988080397683461, -17.36965744553461377 ) ) ;
#11062 = CARTESIAN_POINT ( 'NONE',  ( 206.7927593038066618, 270.4714295788825780, 5.070506503021109168 ) ) ;
#11063 = AXIS2_PLACEMENT_3D ( 'NONE', #80681, #74039, #58315 ) ;
#11064 = EDGE_LOOP ( 'NONE', ( #22865, #36521, #70219, #25050 ) ) ;
#11065 = CARTESIAN_POINT ( 'NONE',  ( 101.5149374161625815, 240.9637435831424739, 2.679491924311251605 ) ) ;
#11066 = VECTOR ( 'NONE', #18068, 1000.000000000000000 ) ;
#11067 = CARTESIAN_POINT ( 'NONE',  ( 31.37760429443828869, 33.51421378149921537, -9.188101187500004485 ) ) ;
#11068 = CARTESIAN_POINT ( 'NONE',  ( -32.04500338604975695, 25.44370296803429810, -10.00000000000000000 ) ) ;
#11069 = CARTESIAN_POINT ( 'NONE',  ( 79.14312167556931854, 57.64441083166269664, 0.000000000000000000 ) ) ;
#11070 = DIRECTION ( 'NONE',  ( -0.8660254037844387076, -0.4999999999999998890, -0.000000000000000000 ) ) ;
#11071 = ORIENTED_EDGE ( 'NONE', *, *, #38649, .T. ) ;
#11072 = ORIENTED_EDGE ( 'NONE', *, *, #42172, .T. ) ;
#11073 = CARTESIAN_POINT ( 'NONE',  ( 40.82928596147627331, 60.38352576601455723, -10.00000000000000000 ) ) ;
#11074 = VECTOR ( 'NONE', #17874, 1000.000000000000000 ) ;
#11076 = CARTESIAN_POINT ( 'NONE',  ( 148.3874010092782498, 273.6324775792697892, -8.328854486678444857 ) ) ;
#11075 = CARTESIAN_POINT ( 'NONE',  ( 204.2799274532736433, 276.8237820148827950, 13.55359442435934803 ) ) ;
#11077 = CARTESIAN_POINT ( 'NONE',  ( 85.44439542427645051, 48.29040533209811059, -11.74811922390697738 ) ) ;
#11078 = CARTESIAN_POINT ( 'NONE',  ( 86.18027666378026197, 49.75620593066997799, 22.50000000000002842 ) ) ;
#11079 = CARTESIAN_POINT ( 'NONE',  ( 147.5263885827495471, 275.7695129196879975, 0.5021707157977391978 ) ) ;
#11080 = CARTESIAN_POINT ( 'NONE',  ( 42.87900647455834502, 24.75620593066997444, 1.732050807568941364 ) ) ;
#11081 = CARTESIAN_POINT ( 'NONE',  ( 208.1506335189424988, 270.1195224479792500, -4.283595630760618889 ) ) ;
#11082 = CARTESIAN_POINT ( 'NONE',  ( 165.9965283720889033, 265.7099112032472021, 16.66492205199346444 ) ) ;
#11083 = AXIS2_PLACEMENT_3D ( 'NONE', #9221, #71039, #62914 ) ;
#11084 = CARTESIAN_POINT ( 'NONE',  ( 79.58917286194427732, 59.33460254692537461, 16.56081879078485741 ) ) ;
#11085 = CARTESIAN_POINT ( 'NONE',  ( 91.59511671678144751, 229.8149278399160664, 9.188101187500093303 ) ) ;
#11086 = ORIENTED_EDGE ( 'NONE', *, *, #45199, .T. ) ;
#11087 = CARTESIAN_POINT ( 'NONE',  ( 23.46864935082055581, 158.3759306620404743, -30.52142883766493853 ) ) ;
#11088 = CARTESIAN_POINT ( 'NONE',  ( 164.1573742157265201, 276.8569001291454015, -13.59881056395027521 ) ) ;
#11089 = ORIENTED_EDGE ( 'NONE', *, *, #76838, .T. ) ;
#11090 = VERTEX_POINT ( 'NONE', #57611 ) ;
#11091 = VERTEX_POINT ( 'NONE', #88590 ) ;
#11092 = CARTESIAN_POINT ( 'NONE',  ( 79.93734396971494505, 44.49601230399111529, -11.01925363558071069 ) ) ;
#11093 = CARTESIAN_POINT ( 'NONE',  ( 179.9534164099970042, 293.6013641453405967, -2.637859770436314921 ) ) ;
#11094 = FACE_OUTER_BOUND ( 'NONE', #21180, .T. ) ;
#11095 = CARTESIAN_POINT ( 'NONE',  ( 159.6288139302610887, 254.1617792512662675, -15.32287760493869477 ) ) ;
#11096 = EDGE_CURVE ( 'NONE', #35869, #75897, #34808, .T. ) ;
#11097 = CARTESIAN_POINT ( 'NONE',  ( 207.2158346629843493, 271.3235102996118826, -3.977316185394199177 ) ) ;
#11098 = CARTESIAN_POINT ( 'NONE',  ( 92.54224522822943300, 233.4244531367911009, -4.594050593750046652 ) ) ;
#11099 = EDGE_LOOP ( 'NONE', ( #60262, #82910, #446, #66097, #39169, #34849, #52077, #60581, #17316, #67597, #82421, #61851, #9223, #22280, #88432, #71999, #81239, #32873, #2258, #51299, #94115 ) ) ;
#11100 = EDGE_CURVE ( 'NONE', #84216, #83863, #42404, .T. ) ;
#11101 = AXIS2_PLACEMENT_3D ( 'NONE', #42422, #57628, #35334 ) ;
#11102 = ORIENTED_EDGE ( 'NONE', *, *, #87841, .T. ) ;
#11103 = CARTESIAN_POINT ( 'NONE',  ( 73.67824366217406862, 55.52431661998091528, 16.58293631993679540 ) ) ;
#11105 = ADVANCED_FACE ( 'NONE', ( #95688 ), #4940, .F. ) ;
#11104 = CARTESIAN_POINT ( 'NONE',  ( 207.5886452961740076, 271.0929146030698007, -1.661373005306138184 ) ) ;
#11106 = VERTEX_POINT ( 'NONE', #20136 ) ;
#11107 = EDGE_CURVE ( 'NONE', #75907, #20062, #8028, .T. ) ;
#11108 = CARTESIAN_POINT ( 'NONE',  ( 75.79167905567804553, 65.12415201610325255, -14.46789148266619485 ) ) ;
#11109 = CARTESIAN_POINT ( 'NONE',  ( 95.19470834736904408, 235.7677522451419065, -5.000000000000047962 ) ) ;
#11110 = AXIS2_PLACEMENT_3D ( 'NONE', #69782, #8004, #391 ) ;
#11111 = CARTESIAN_POINT ( 'NONE',  ( 68.98939262229419001, 69.25400323834284677, -5.717648734987297310 ) ) ;
#11113 = CARTESIAN_POINT ( 'NONE',  ( 87.58100233665301459, 44.90480556695516867, -6.571228966301012164 ) ) ;
#11112 = CARTESIAN_POINT ( 'NONE',  ( 131.1886288721100300, 255.7369531367911293, -4.594050593750048428 ) ) ;
#11114 = CARTESIAN_POINT ( 'NONE',  ( -6.130263895410211994, 157.2677522451417929, -5.000000000000041744 ) ) ;
#11115 = CARTESIAN_POINT ( 'NONE',  ( 81.29539683296886210, 43.25976067974499273, 9.624898955577574355 ) ) ;
#11116 = EDGE_LOOP ( 'NONE', ( #24283, #72862, #51165, #6672, #98904, #71218, #82952, #53057, #53051, #11072, #53929, #70254, #84830, #842, #34249, #72255, #12174, #63011, #22868, #52043, #63053 ) ) ;
#11117 = CARTESIAN_POINT ( 'NONE',  ( 156.7786475906069938, 259.0984121615696836, 17.12081851550279055 ) ) ;
#11118 = CARTESIAN_POINT ( 'NONE',  ( 160.7433166061900920, 275.5038296165459997, 13.74271022849526780 ) ) ;
#11119 = CARTESIAN_POINT ( 'NONE',  ( 159.9770824720811220, 253.5585604421560788, -16.42166711341322483 ) ) ;
#11120 = CARTESIAN_POINT ( 'NONE',  ( 191.9985291012005462, 271.7866236224816703, 14.17061973602814007 ) ) ;
#11121 = CARTESIAN_POINT ( 'NONE',  ( 71.55517591705296354, 59.48308490877587928, -15.70938992770603093 ) ) ;
#11122 = CARTESIAN_POINT ( 'NONE',  ( 187.4676533354318906, 272.4601757945604845, -16.88503403312462936 ) ) ;
#11123 = CARTESIAN_POINT ( 'NONE',  ( -19.65312891409030271, 93.06504152958497400, 177.5919119679930134 ) ) ;
#11124 = DIRECTION ( 'NONE',  ( 0.000000000000000000, 0.000000000000000000, 1.000000000000000000 ) ) ;
#11125 = CARTESIAN_POINT ( 'NONE',  ( 161.8662906133268393, 250.2863559554455719, 14.03735902266321744 ) ) ;
#11126 = CARTESIAN_POINT ( 'NONE',  ( -3.216670782107629911, 25.02209300385174373, 10.00000000000000000 ) ) ;
#11127 = FACE_OUTER_BOUND ( 'NONE', #15410, .T. ) ;
#11128 = CARTESIAN_POINT ( 'NONE',  ( 78.28176711274900867, 61.66836085159184933, 15.77706035593199196 ) ) ;
#11129 = FACE_OUTER_BOUND ( 'NONE', #2455, .T. ) ;
#11130 = FACE_OUTER_BOUND ( 'NONE', #95496, .T. ) ;
#11131 = VECTOR ( 'NONE', #49638, 1000.000000000000114 ) ;
#11132 = AXIS2_PLACEMENT_3D ( 'NONE', #66020, #10833, #4732 ) ;
#11133 = VECTOR ( 'NONE', #13188, 1000.000000000000114 ) ;
#11134 = CARTESIAN_POINT ( 'NONE',  ( 165.0437781805843258, 244.7827860485373606, -2.050141714668513693 ) ) ;
#11135 = CARTESIAN_POINT ( 'NONE',  ( 183.3360699033760568, 264.4351057451253837, 14.27812921404662383 ) ) ;
#11136 = LINE ( 'NONE', #51089, #90303 ) ;
#11137 = CARTESIAN_POINT ( 'NONE',  ( 31.01755306704832194, 42.00034080476293497, -1.878358725466461243E-16 ) ) ;
#11138 = CARTESIAN_POINT ( 'NONE',  ( 78.23911696424225681, 47.73527672355887574, 13.93191159841320825 ) ) ;
#11139 = DIRECTION ( 'NONE',  ( 0.5000000000000001110, -0.8660254037844384856, -0.000000000000000000 ) ) ;
#11140 = CARTESIAN_POINT ( 'NONE',  ( 58.31414817410232843, 216.0217562850347690, 5.155647304959626021E-14 ) ) ;
#11142 = CARTESIAN_POINT ( 'NONE',  ( 71.85273313970169795, 59.31805131066353454, -15.30413012561420771 ) ) ;
#11141 = B_SPLINE_CURVE_WITH_KNOTS ( 'NONE', 3,
 ( #21509, #43792, #20521, #59983, #68095, #52890, #52394, #66108, #21029, #74238, #83842, #82852, #67596, #74735, #58492, #60476 ),
 .UNSPECIFIED., .F., .F.,
 ( 4, 1, 2, 2, 2, 1, 2, 2, 4 ),
 ( 0.000000000000000000, 0.1250000000000008604, 0.1875000000000018596, 0.2500000000000028311, 0.5000000000000042188, 0.6250000000000045519, 0.6875000000000034417, 0.7500000000000022204, 1.000000000000000000 ),
 .UNSPECIFIED. ) ;
#11143 = DIRECTION ( 'NONE',  ( -0.2588190451025115801, -0.9659258262890707547, -2.299878683274414842E-16 ) ) ;
#11144 = VECTOR ( 'NONE', #5905, 999.9999999999998863 ) ;
#11145 =( BOUNDED_CURVE ( )  B_SPLINE_CURVE ( 2, ( #49700, #32514, #18322, #87783, #95859, #86264, #25925, #3143, #24900 ),
 .UNSPECIFIED., .F., .T. ) 
 B_SPLINE_CURVE_WITH_KNOTS ( ( 3, 2, 2, 2, 3 ),
 ( 0.3104838709677419373, 0.3118279569892473124, 0.3145161290322580627, 0.3172043010752688130, 0.3185483870967741882 ),
 .UNSPECIFIED. ) 
 CURVE ( )  GEOMETRIC_REPRESENTATION_ITEM ( )  RATIONAL_B_SPLINE_CURVE ( ( 0.9330127018922194093, 0.9330127018922194093, 1.000000000000000000, 0.8660254037844387076, 1.000000000000000000, 0.8660254037844387076, 1.000000000000000000, 0.9330127018922194093, 0.9330127018922194093 ) ) 
 REPRESENTATION_ITEM ( '' )  );
#11146 = CARTESIAN_POINT ( 'NONE',  ( 18.14551070619625150, 181.2833772461660544, -9.188101187500095079 ) ) ;
#11147 = DIRECTION ( 'NONE',  ( 0.000000000000000000, 0.000000000000000000, 1.000000000000000000 ) ) ;
#11148 = ORIENTED_EDGE ( 'NONE', *, *, #20412, .F. ) ;
#11149 = CARTESIAN_POINT ( 'NONE',  ( 86.58136378248637754, 46.32108903705595537, 9.037364168832199951 ) ) ;
#11150 = CARTESIAN_POINT ( 'NONE',  ( 24.22498904768565353, 14.39040679176983062, 1.333680081654574804E-15 ) ) ;
#11151 = CARTESIAN_POINT ( 'NONE',  ( 207.9622466093905189, 270.4458181468041289, 3.586592550214158681 ) ) ;
#11152 = CARTESIAN_POINT ( 'NONE',  ( 81.94607988216938566, 41.18096579325325024, 5.530507272723311551 ) ) ;
#11153 = CARTESIAN_POINT ( 'NONE',  ( 31.35205101814392847, 201.1589784336661353, -6.496448406907676862E-16 ) ) ;
#11154 = EDGE_CURVE ( 'NONE', #90765, #41961, #66713, .T. ) ;
#11155 = VECTOR ( 'NONE', #1281, 1000.000000000000114 ) ;
#11156 = CARTESIAN_POINT ( 'NONE',  ( 200.8432122835317841, 282.7763473000181307, 17.15137370990203891 ) ) ;
#11157 = CARTESIAN_POINT ( 'NONE',  ( 190.1693911629507738, 301.2639477917662703, -5.112716700269980485 ) ) ;
#11158 = CARTESIAN_POINT ( 'NONE',  ( 30.83758659773572575, 40.73705186507756082, -3.090169943749475845 ) ) ;
#11159 = CARTESIAN_POINT ( 'NONE',  ( 178.2476854491459903, 292.1019644849587849, 5.583694897891509967 ) ) ;
#11160 = CARTESIAN_POINT ( 'NONE',  ( 191.1687199697037443, 299.5330595250031820, -8.491751560014430211 ) ) ;
#11161 = CARTESIAN_POINT ( 'NONE',  ( 157.7255603307123408, 268.5163524934444013, 16.86592485641857309 ) ) ;
#11162 = B_SPLINE_SURFACE_WITH_KNOTS ( 'NONE', 3, 1, ( 
 ( #8399, #45389 ),
 ( #53486, #46892 ),
 ( #14983, #24585 ),
 ( #73211, #9398 ),
 ( #55471, #26105 ),
 ( #64604, #72731 ),
 ( #72218, #2822 ),
 ( #71214, #47873 ),
 ( #87478, #26603 ),
 ( #71722, #55964 ),
 ( #94035, #3321 ),
 ( #57478, #95559 ),
 ( #32689, #56979 ),
 ( #42277, #87965 ),
 ( #63089, #1805 ),
 ( #18509, #88461 ),
 ( #78811, #19021 ),
 ( #94531, #56491 ),
 ( #10909, #96044 ),
 ( #63590, #2314 ),
 ( #40272, #18012 ),
 ( #25083, #49895 ),
 ( #49395, #80853 ),
 ( #80342, #86958 ),
 ( #9912, #33194 ),
 ( #41785, #40770 ),
 ( #17494, #48905 ),
 ( #48399, #34202 ),
 ( #10406, #79345 ),
 ( #11425, #32187 ),
 ( #65092, #64095 ),
 ( #95040, #25604 ),
 ( #79840, #86457 ),
 ( #41276, #16982 ) ),
 .UNSPECIFIED., .T., .F., .F.,
 ( 4, 2, 2, 2, 2, 2, 2, 2, 2, 2, 2, 2, 2, 2, 2, 2, 4 ),
 ( 2, 2 ),
 ( 0.000000000000000000, 0.06250000000000000000, 0.1250000000000000000, 0.1875000000000000000, 0.2500000000000000000, 0.3125000000000000000, 0.3750000000000000000, 0.4375000000000000000, 0.5000000000000000000, 0.5625000000000000000, 0.6250000000000000000, 0.6875000000000000000, 0.7500000000000000000, 0.8125000000000000000, 0.8750000000000000000, 0.9375000000000000000, 1.000000000000000000 ),
 ( 0.000000000000000000, 1.000000000000000000 ),
 .UNSPECIFIED. ) ;
#11163 = CARTESIAN_POINT ( 'NONE',  ( 166.0171423212046022, 257.5822672037136272, -15.03208011136822009 ) ) ;
#11164 = CARTESIAN_POINT ( 'NONE',  ( 83.38731009417298878, 51.80618739314797949, 14.97569794390972397 ) ) ;
#11165 = CARTESIAN_POINT ( 'NONE',  ( 82.29453827371126806, 224.9865022471902876, -10.00000000000009415 ) ) ;
#11166 = CARTESIAN_POINT ( 'NONE',  ( 19.05118110555104849, 170.2592609112379876, 2.679491924311254714 ) ) ;
#11167 = CARTESIAN_POINT ( 'NONE',  ( 161.5827144264378887, 267.7246213421781249, -17.17800402044808195 ) ) ;
#11168 = CARTESIAN_POINT ( 'NONE',  ( 45.10055139898691579, 196.8458772461660544, 9.188101187500095079 ) ) ;
#11169 = EDGE_CURVE ( 'NONE', #49174, #86134, #22085, .T. ) ;
#11170 = ORIENTED_EDGE ( 'NONE', *, *, #29935, .T. ) ;
#11171 = CARTESIAN_POINT ( 'NONE',  ( -7.323307257743949528, 84.15769153094232990, 13.64793647583705294 ) ) ;
#11172 = CARTESIAN_POINT ( 'NONE',  ( 150.8168331730346949, 269.4245776381016526, -15.71017957295074652 ) ) ;
#11173 = B_SPLINE_CURVE_WITH_KNOTS ( 'NONE', 3,
 ( #20113, #18615, #80449, #3426, #19627, #34301, #96143, #57586, #50002, #79448, #50485, #42868, #73802, #44379, #66688, #67690, #98619, #13993, #91032, #51488, #76307, #13019, #12511, #28690, #82457, #68178, #83427, #4910, #14494, #75811, #28188, #90546, #21116, #59570, #92037, #51994 ),
 .UNSPECIFIED., .F., .F.,
 ( 4, 2, 2, 2, 2, 2, 2, 2, 2, 2, 2, 2, 2, 2, 2, 2, 2, 4 ),
 ( 0.003351528275103934310, 0.003542274814850215284, 0.003637648084723309801, 0.003733021354596404318, 0.003923767894342636287, 0.004114514434088867821, 0.004496007513581369922, 0.004877500593073871155, 0.005640486752058733975, 0.006403472911043596796, 0.007929445229013240906, 0.008120191768759348408, 0.008167878403695857936, 0.008215565038632367464, 0.008310938308505362235, 0.008692431387997369072, 0.009073924467489377643, 0.009455417546981384480 ),
 .UNSPECIFIED. ) ;
#11174 = LINE ( 'NONE', #19278, #11131 ) ;
#11175 = EDGE_LOOP ( 'NONE', ( #78678, #26737, #85639, #24474 ) ) ;
#11176 = CARTESIAN_POINT ( 'NONE',  ( 167.3544567060031056, 285.1758971363884712, 7.850027993811327320 ) ) ;
#11177 = CARTESIAN_POINT ( 'NONE',  ( 207.3502731283117555, 271.5057873089173768, 6.280625384230454245 ) ) ;
#11178 = FACE_OUTER_BOUND ( 'NONE', #26047, .T. ) ;
#11179 = CARTESIAN_POINT ( 'NONE',  ( 32.96772289237024012, 21.96004757982091959, -5.678558825948276656 ) ) ;
#11180 = CARTESIAN_POINT ( 'NONE',  ( 72.96724880819495240, 70.75172224442833624, -7.458605312651823915 ) ) ;
#11181 = CARTESIAN_POINT ( 'NONE',  ( -69.85371643402891095, 44.28081239092799848, -10.00000000000000000 ) ) ;
#11182 = CARTESIAN_POINT ( 'NONE',  ( 172.8753696232004415, 256.4781477760785720, 11.23930794150890478 ) ) ;
#11183 = ORIENTED_EDGE ( 'NONE', *, *, #65141, .T. ) ;
#11184 = CARTESIAN_POINT ( 'NONE',  ( 18.60133699236122240, 19.24335787977762990, -9.188101187500008038 ) ) ;
#11185 = CARTESIAN_POINT ( 'NONE',  ( 171.8846141982767222, 252.9912589899345221, 8.488787739703381519 ) ) ;
#11186 = LINE ( 'NONE', #50159, #65098 ) ;
#11187 = ORIENTED_EDGE ( 'NONE', *, *, #60172, .F. ) ;
#11188 = CARTESIAN_POINT ( 'NONE',  ( 72.06693479607845632, 71.51559350784613400, -5.828149303013867133 ) ) ;
#11189 = CARTESIAN_POINT ( 'NONE',  ( -22.42236680055709641, 157.8615022471902591, 0.000000000000000000 ) ) ;
#11190 = CARTESIAN_POINT ( 'NONE',  ( -19.65312891409030271, 93.06504152958497400, 203.6502102582797420 ) ) ;
#11191 = CARTESIAN_POINT ( 'NONE',  ( 71.42110848219473951, 65.04516533590125960, -13.05791646362531466 ) ) ;
#11192 = ORIENTED_EDGE ( 'NONE', *, *, #66881, .F. ) ;
#11193 = ORIENTED_EDGE ( 'NONE', *, *, #37375, .F. ) ;
#11195 = CARTESIAN_POINT ( 'NONE',  ( 150.9847884352320762, 269.5419465100882803, -13.76858632224513279 ) ) ;
#11194 = CARTESIAN_POINT ( 'NONE',  ( 207.1211793645798878, 271.9025893473983047, -6.294110402770905388 ) ) ;
#11196 = CARTESIAN_POINT ( 'NONE',  ( 188.2520712372829621, 265.6420100395978920, -13.17850047611677766 ) ) ;
#11197 = ORIENTED_EDGE ( 'NONE', *, *, #64448, .T. ) ;
#11198 = CARTESIAN_POINT ( 'NONE',  ( 41.71240375114938814, 62.05720181600818108, 10.00000000000000000 ) ) ;
#11199 = VECTOR ( 'NONE', #47948, 1000.000000000000000 ) ;
#11200 = FACE_OUTER_BOUND ( 'NONE', #439, .T. ) ;
#11201 = CARTESIAN_POINT ( 'NONE',  ( 72.26191451101281871, 71.91445694603925176, -5.118044210176695863 ) ) ;
#11202 = CARTESIAN_POINT ( 'NONE',  ( 78.09292022067579353, 61.02350456329286033, -15.89647179981830405 ) ) ;
#11203 = CARTESIAN_POINT ( 'NONE',  ( 157.0978663001774862, 258.5455091378672137, -17.31223197570816552 ) ) ;
#11204 = CARTESIAN_POINT ( 'NONE',  ( 119.9849458542963561, 230.8923013555409796, 4.594050593750050204 ) ) ;
#11205 = AXIS2_PLACEMENT_3D ( 'NONE', #87615, #72365, #11055 ) ;
#11206 = DIRECTION ( 'NONE',  ( -0.5000000000000013323, 0.8660254037844379305, 0.000000000000000000 ) ) ;
#11207 = AXIS2_PLACEMENT_3D ( 'NONE', #41992, #58187, #72929 ) ;
#11208 = DIRECTION ( 'NONE',  ( -0.8660254037844387076, -0.4999999999999998890, -0.000000000000000000 ) ) ;
#11209 = ORIENTED_EDGE ( 'NONE', *, *, #82172, .T. ) ;
#11210 = CARTESIAN_POINT ( 'NONE',  ( 207.7655736232174206, 270.7864657513322300, 3.530742899761726949 ) ) ;
#11211 = ORIENTED_EDGE ( 'NONE', *, *, #342, .F. ) ;
#11212 = CARTESIAN_POINT ( 'NONE',  ( 31.85034293892215018, 41.49540643055189548, 3.479690158560446702E-15 ) ) ;
#11213 = FACE_BOUND ( 'NONE', #49786, .T. ) ;
#11214 = CARTESIAN_POINT ( 'NONE',  ( 78.50112015865835247, 48.01465776021366594, -13.99615223866804570 ) ) ;
#11215 = CARTESIAN_POINT ( 'NONE',  ( 72.70511114461589841, 212.7833772461660544, -9.188101187500095079 ) ) ;
#11216 = CARTESIAN_POINT ( 'NONE',  ( -31.49991166888935368, 96.34225309604657639, 12.27547638658930218 ) ) ;
#11217 = CARTESIAN_POINT ( 'NONE',  ( 150.8757650385446993, 269.3225046528533539, 14.31332712971473953 ) ) ;
#11218 = DIRECTION ( 'NONE',  ( 0.000000000000000000, 0.000000000000000000, 1.000000000000000000 ) ) ;
#11219 = CARTESIAN_POINT ( 'NONE',  ( 174.2807072416181597, 277.7764784826417213, 15.50750675594299643 ) ) ;
#11220 = EDGE_LOOP ( 'NONE', ( #42178, #82154, #19072, #44529 ) ) ;
#11221 = CIRCLE ( 'NONE', #24134, 1.449999999999993072 ) ;
#11222 = CARTESIAN_POINT ( 'NONE',  ( 80.28198526002465485, 56.49958842488598521, -16.15443186264643316 ) ) ;
#11223 = CARTESIAN_POINT ( 'NONE',  ( 147.6220714307702622, 274.9580672937808572, 8.392894244419288441 ) ) ;
#11224 = ORIENTED_EDGE ( 'NONE', *, *, #54772, .T. ) ;
#11225 = CARTESIAN_POINT ( 'NONE',  ( 195.5106104057018968, 292.0126846889568810, 15.81382758565595736 ) ) ;
#11226 = CARTESIAN_POINT ( 'NONE',  ( 173.8661040448295694, 278.0172980323289380, -16.69473935971507572 ) ) ;
#11227 = CARTESIAN_POINT ( 'NONE',  ( 160.7200862735817850, 258.4377271483461413, -16.74603599744149918 ) ) ;
#11228 = EDGE_CURVE ( 'NONE', #92184, #79500, #20632, .T. ) ;
#11229 = CARTESIAN_POINT ( 'NONE',  ( 206.4737064409647189, 270.6076388844679173, 2.372787432230063942 ) ) ;
#11230 = CARTESIAN_POINT ( 'NONE',  ( 149.4491471355718772, 271.7934793437897270, 11.43912701239353780 ) ) ;
#11231 = B_SPLINE_CURVE_WITH_KNOTS ( 'NONE', 3,
 ( #5105, #39335, #91222, #29397, #21789, #67896, #89746, #28904, #36987, #59781, #82151, #28387, #363, #31250, #35984, #66889 ),
 .UNSPECIFIED., .F., .F.,
 ( 4, 2, 2, 2, 2, 2, 2, 4 ),
 ( 0.000000000000000000, 0.0003786681000626568642, 0.0007573362001253137283, 0.001136004300187970538, 0.001514672400250627457, 0.001893340500313284158, 0.002272008600375941077, 0.003029344800501280934 ),
 .UNSPECIFIED. ) ;
#11232 = CARTESIAN_POINT ( 'NONE',  ( 179.4402317224691501, 270.6826544746222112, 16.24075135540241988 ) ) ;
#11233 = VECTOR ( 'NONE', #57472, 1000.000000000000000 ) ;
#11234 = CARTESIAN_POINT ( 'NONE',  ( 206.0627831668701901, 273.7357853363691902, 10.14454147593459687 ) ) ;
#11235 = CARTESIAN_POINT ( 'NONE',  ( -167.0327448629461742, 42.61639673982675447, 30.52142883766498116 ) ) ;
#11236 = CARTESIAN_POINT ( 'NONE',  ( 166.6284335572192958, 255.9663351304055539, 13.75844111390426683 ) ) ;
#11237 = ORIENTED_EDGE ( 'NONE', *, *, #9305, .F. ) ;
#11238 = CARTESIAN_POINT ( 'NONE',  ( 208.3057440179679531, 269.8508631828800617, 2.969924427282375046 ) ) ;
#11239 = CARTESIAN_POINT ( 'NONE',  ( 127.7791744883563183, 235.3923013555409796, 4.594050593750050204 ) ) ;
#11240 = ORIENTED_EDGE ( 'NONE', *, *, #12101, .T. ) ;
#11241 = CARTESIAN_POINT ( 'NONE',  ( 86.21802580015948081, 44.21772915329312070, -5.774872143548296144 ) ) ;
#11242 = CARTESIAN_POINT ( 'NONE',  ( 46.50192534792603283, 74.36443251879779837, 10.00000000000000000 ) ) ;
#11243 = CARTESIAN_POINT ( 'NONE',  ( 78.60735446187599962, 47.91558663937576057, -14.46554739992950189 ) ) ;
#11244 = CARTESIAN_POINT ( 'NONE',  ( 164.4936379324916516, 245.7356569095223051, 6.719479797016231437 ) ) ;
#11245 = LINE ( 'NONE', #35005, #35285 ) ;
#11246 = CARTESIAN_POINT ( 'NONE',  ( 76.30616544034060666, 50.97262258187969763, -15.53540872755634439 ) ) ;
#11247 = ORIENTED_EDGE ( 'NONE', *, *, #16841, .T. ) ;
#11248 = CARTESIAN_POINT ( 'NONE',  ( 80.44110801039052205, 57.53904330600535388, -16.59063950305211677 ) ) ;
#11249 = CARTESIAN_POINT ( 'NONE',  ( 157.9297271802291220, 276.0988248505941556, -12.89341868665208679 ) ) ;
#11251 = CARTESIAN_POINT ( 'NONE',  ( 207.0571114767778624, 269.8739652884199245, 1.758464922131628860 ) ) ;
#11250 = DIRECTION ( 'NONE',  ( -0.9303772761487891785, -0.3666034970181814012, 0.000000000000000000 ) ) ;
#11252 = CARTESIAN_POINT ( 'NONE',  ( 206.4839639422192192, 273.0062788342933118, -11.22308919026441210 ) ) ;
#11253 = CARTESIAN_POINT ( 'NONE',  ( 148.2390246527636748, 247.2048013555409511, 4.594050593750051981 ) ) ;
#11254 = DIRECTION ( 'NONE',  ( -0.5000000000000013323, 0.8660254037844380415, -0.000000000000000000 ) ) ;
#11255 = CARTESIAN_POINT ( 'NONE',  ( 29.55951135474875358, 176.3262482093457777, 3.021315404115420679E-15 ) ) ;
#11256 = CARTESIAN_POINT ( 'NONE',  ( 67.85514785513115044, 68.63529022595450613, 5.540876512699765222 ) ) ;
#11257 = CARTESIAN_POINT ( 'NONE',  ( 65.53359859134977228, 199.4548013555410080, -4.594050593750042211 ) ) ;
#11258 = CARTESIAN_POINT ( 'NONE',  ( 157.6668627405778409, 257.5599783937680058, -16.78811156090270629 ) ) ;
#11259 = CARTESIAN_POINT ( 'NONE',  ( 172.5875758667829984, 251.5272254664457989, 3.418950794502710000 ) ) ;
#11260 = CARTESIAN_POINT ( 'NONE',  ( 19.55501378379531019, 16.45404122711132899, -8.090169943749478065 ) ) ;
#11261 = CARTESIAN_POINT ( 'NONE',  ( 149.0323968763055689, 272.5153119669064949, 11.64231532207353403 ) ) ;
#11262 = CARTESIAN_POINT ( 'NONE',  ( 154.9461157776194966, 279.4417561161487242, -1.582898759582469284 ) ) ;
#11263 = CARTESIAN_POINT ( 'NONE',  ( 170.6705325584632931, 285.9596063569311468, -7.984020550193259069 ) ) ;
#11264 = DIRECTION ( 'NONE',  ( 0.000000000000000000, 0.000000000000000000, 1.000000000000000000 ) ) ;
#11265 = CARTESIAN_POINT ( 'NONE',  ( 149.0242096487241383, 274.5281563735073860, 9.114748174487145249 ) ) ;
#11266 = CARTESIAN_POINT ( 'NONE',  ( 135.3927208396967785, 255.6427522451419065, -10.00000000000009415 ) ) ;
#11267 = CARTESIAN_POINT ( 'NONE',  ( 17.41189581114303309, 28.79103043416549212, 8.090169943749478065 ) ) ;
#11268 = VERTEX_POINT ( 'NONE', #75840 ) ;
#11269 = AXIS2_PLACEMENT_3D ( 'NONE', #94150, #18116, #18626 ) ;
#11270 = CARTESIAN_POINT ( 'NONE',  ( 66.79965368539949111, 67.34049316045133082, -6.934348251617318049 ) ) ;
#11271 = CARTESIAN_POINT ( 'NONE',  ( 148.1672759425158290, 274.0137453789218398, 7.847779094015780110 ) ) ;
#11272 = CARTESIAN_POINT ( 'NONE',  ( -9.188242552867590618, 159.3768266524160140, 9.188101187500096856 ) ) ;
#11273 = EDGE_CURVE ( 'NONE', #35906, #13323, #84945, .T. ) ;
#11274 = CARTESIAN_POINT ( 'NONE',  ( 40.49996498926459765, 188.0643266524160140, 9.188101187500095079 ) ) ;
#11275 = VECTOR ( 'NONE', #38525, 1000.000000000000114 ) ;
#11276 = CARTESIAN_POINT ( 'NONE',  ( 179.3158450784500246, 274.1411853107688898, -17.71003609510279730 ) ) ;
#11277 = CARTESIAN_POINT ( 'NONE',  ( 21.19599769036394576, 20.43677371833801004, -10.00000000000000355 ) ) ;
#11278 = DIRECTION ( 'NONE',  ( 0.7492053821868994712, 0.6623377501714527993, 0.000000000000000000 ) ) ;
#11279 = CARTESIAN_POINT ( 'NONE',  ( 205.0716081116550527, 275.4525508911965517, -12.57761053684872188 ) ) ;
#11280 = CARTESIAN_POINT ( 'NONE',  ( 192.6160155272557688, 292.3720383156061757, -14.34532783140716106 ) ) ;
#11281 = CARTESIAN_POINT ( 'NONE',  ( 190.2287563641723978, 301.1611242470490311, -4.521471513871881953 ) ) ;
#11282 = CARTESIAN_POINT ( 'NONE',  ( 73.84183722536076289, 55.07373432386307144, -16.12662324738414910 ) ) ;
#11284 = CARTESIAN_POINT ( 'NONE',  ( 52.25428207639063061, 207.6427522451419350, -10.00000000000009415 ) ) ;
#11283 = CARTESIAN_POINT ( 'NONE',  ( 168.9800899256908053, 257.3656399283672727, 13.71095777019204576 ) ) ;
#11285 = CARTESIAN_POINT ( 'NONE',  ( 75.02164697668396798, 67.17574075851680959, 12.57494967656429985 ) ) ;
#11286 = CARTESIAN_POINT ( 'NONE',  ( 26.07214984898741150, 33.79103043416550634, 8.090169943749478065 ) ) ;
#11287 = CARTESIAN_POINT ( 'NONE',  ( 162.1789081252419464, 251.9841321976889503, -13.95467832899616845 ) ) ;
#11288 = EDGE_CURVE ( 'NONE', #14234, #2713, #77731, .T. ) ;
#11289 = CIRCLE ( 'NONE', #82482, 0.1418229129680828593 ) ;
#11290 = CARTESIAN_POINT ( 'NONE',  ( 32.13723363786251497, 199.3615022471903160, 5.000000000000046185 ) ) ;
#11291 = DIRECTION ( 'NONE',  ( 0.4999999999999998890, -0.8660254037844387076, 0.000000000000000000 ) ) ;
#11292 = CARTESIAN_POINT ( 'NONE',  ( 203.0507839702407580, 278.9527209772879814, 16.21318481136342626 ) ) ;
#11293 = CARTESIAN_POINT ( 'NONE',  ( -3.911334118262431936, 177.7369531367911293, -4.594050593750048428 ) ) ;
#11294 = CARTESIAN_POINT ( 'NONE',  ( 30.99092310034283315, 39.93396525600392977, 2.839279412974139660 ) ) ;
#11296 = EDGE_CURVE ( 'NONE', #48810, #80286, #67213, .T. ) ;
#11295 = CARTESIAN_POINT ( 'NONE',  ( 164.8761197389183906, 246.7675571797174428, 5.899305509596029395 ) ) ;
#11297 = CARTESIAN_POINT ( 'NONE',  ( 192.8132846206021611, 296.6845899933152850, 11.53748932578252351 ) ) ;
#11298 = CARTESIAN_POINT ( 'NONE',  ( 30.66313333631613247, 33.10171378149921395, 9.188101187500008038 ) ) ;
#11299 = B_SPLINE_CURVE_WITH_KNOTS ( 'NONE', 3,
 ( #23719, #63739, #63236, #9558, #32334, #94178, #94674, #55119, #39910, #24729, #78456, #10048, #40421, #55613, #86596, #71354, #93168, #1946, #25231, #87109, #17647, #62720, #8541, #25755, #71859, #86105, #64235, #38924, #54613, #85597, #48545, #79485, #2456, #16632, #95185, #31818, #77455, #85072, #15619, #440, #46518, #31329, #16137, #47035, #77952, #39413, #70328, #93677, #24242, #18653, #80485, #50521 ),
 .UNSPECIFIED., .F., .F.,
 ( 4, 2, 2, 2, 2, 2, 2, 2, 2, 2, 2, 2, 2, 2, 2, 2, 2, 2, 2, 2, 2, 2, 2, 2, 2, 4 ),
 ( 0.001762225997650664847, 0.002214759945835987828, 0.002667293894021311243, 0.002780427381067715822, 0.002893560868114120836, 0.003006694355160525849, 0.003119827842206930428, 0.003346094816299740454, 0.003572361790392550480, 0.004024895738578136706, 0.004477429686763722064, 0.005382497583134956097, 0.006287565479506190130, 0.006740099427691806713, 0.007192633375877425031, 0.007305766862923767160, 0.007362333606446948633, 0.007418900349970128372, 0.007532033837016489583, 0.007645167324062849060, 0.007871434298155587095, 0.008097701272248325130, 0.008323968246341063165, 0.008550235220433801200, 0.008776502194526539236, 0.009002769168619277271 ),
 .UNSPECIFIED. ) ;
#11300 = CARTESIAN_POINT ( 'NONE',  ( 25.36820930315042943, 19.81029122506294726, 8.090169943749479842 ) ) ;
#11301 = CARTESIAN_POINT ( 'NONE',  ( 179.3456124633583499, 277.5962114444210442, 17.35945876020667100 ) ) ;
#11302 = CARTESIAN_POINT ( 'NONE',  ( 80.93613592869992601, 42.95327845849681836, -9.503115154567232992 ) ) ;
#11303 = FACE_OUTER_BOUND ( 'NONE', #13525, .T. ) ;
#11304 = CARTESIAN_POINT ( 'NONE',  ( 179.5567261186911594, 262.6765698908865829, -12.85373963981448497 ) ) ;
#11305 = DIRECTION ( 'NONE',  ( 0.000000000000000000, 0.000000000000000000, 1.000000000000000000 ) ) ;
#11306 = CARTESIAN_POINT ( 'NONE',  ( 6.965323710529800927, 24.99752408145590366, 5.678558825948277544 ) ) ;
#11307 = CARTESIAN_POINT ( 'NONE',  ( 125.9386101817166974, 233.5177522451417929, 5.000000000000051514 ) ) ;
#11308 = CARTESIAN_POINT ( 'NONE',  ( 21.54279312762077936, 14.29860640527291871, -2.839279412974138328 ) ) ;
#11309 = VECTOR ( 'NONE', #90063, 1000.000000000000114 ) ;
#11310 = CARTESIAN_POINT ( 'NONE',  ( 158.9661858079439298, 259.3592988854380224, 16.70105242487986530 ) ) ;
#11311 = PLANE ( 'NONE',  #20905 ) ;
#11312 = CARTESIAN_POINT ( 'NONE',  ( 111.0177141658951854, 228.2365022471901739, -10.00000000000009237 ) ) ;
#11313 = CARTESIAN_POINT ( 'NONE',  ( 81.18465792105908463, 42.40984018312481396, 7.627542571750448808 ) ) ;
#11314 = CARTESIAN_POINT ( 'NONE',  ( 48.05312180239142350, 111.8345470171556428, 10.00000000000000000 ) ) ;
#11315 = ORIENTED_EDGE ( 'NONE', *, *, #75108, .T. ) ;
#11316 = DIRECTION ( 'NONE',  ( 0.000000000000000000, 0.000000000000000000, 1.000000000000000000 ) ) ;
#11317 = CARTESIAN_POINT ( 'NONE',  ( 207.4285356523023154, 271.3702326410368642, 7.833982582429932506 ) ) ;
#11318 = DIRECTION ( 'NONE',  ( -0.4924038765061016787, 0.8528685319524424990, -0.1736481776669404342 ) ) ;
#11319 = CARTESIAN_POINT ( 'NONE',  ( 87.56358751521999295, 45.50810825807865712, 6.913240104252196261 ) ) ;
#11320 = ORIENTED_EDGE ( 'NONE', *, *, #66082, .T. ) ;
#11321 = ORIENTED_EDGE ( 'NONE', *, *, #30086, .T. ) ;
#11323 = DIRECTION ( 'NONE',  ( 1.000000000000000000, 0.000000000000000000, 0.000000000000000000 ) ) ;
#11322 = CARTESIAN_POINT ( 'NONE',  ( 159.6251152260277308, 278.4128260634272465, -9.785471751044605426 ) ) ;
#11324 = CARTESIAN_POINT ( 'NONE',  ( 86.13530110067358692, 47.09369226531615737, 10.77952153921811096 ) ) ;
#11325 = ORIENTED_EDGE ( 'NONE', *, *, #80665, .F. ) ;
#11326 = LINE ( 'NONE', #41682, #36992 ) ;
#11327 = DIRECTION ( 'NONE',  ( -1.000000000000000000, 0.000000000000000000, 0.000000000000000000 ) ) ;
#11328 = ORIENTED_EDGE ( 'NONE', *, *, #19494, .T. ) ;
#11329 = CARTESIAN_POINT ( 'NONE',  ( 69.12672858200174630, 64.33651235087042153, -11.97836756590942997 ) ) ;
#11330 = CARTESIAN_POINT ( 'NONE',  ( 85.25577013208754806, 208.4824982072973967, 3.021315404115420679E-15 ) ) ;
#11331 = CARTESIAN_POINT ( 'NONE',  ( 149.6564118588553924, 271.4344863124460971, -11.76165597393390172 ) ) ;
#11332 = CARTESIAN_POINT ( 'NONE',  ( 43.80257615421894712, 184.5494855054052152, -2.679491924311248496 ) ) ;
#11333 = ORIENTED_EDGE ( 'NONE', *, *, #66938, .T. ) ;
#11334 = CARTESIAN_POINT ( 'NONE',  ( 161.8662906133268393, 250.2863559554455719, 14.03735902266321744 ) ) ;
#11335 = CARTESIAN_POINT ( 'NONE',  ( 166.0972222936661638, 274.0867323433699880, -15.20829511115417887 ) ) ;
#11336 = DIRECTION ( 'NONE',  ( -1.000000000000000000, -9.785293164091215354E-14, 0.000000000000000000 ) ) ;
#11337 = ORIENTED_EDGE ( 'NONE', *, *, #6965, .F. ) ;
#11338 = EDGE_CURVE ( 'NONE', #48833, #89111, #90574, .T. ) ;
#11339 = EDGE_CURVE ( 'NONE', #98279, #100024, #98644, .T. ) ;
#11340 = CARTESIAN_POINT ( 'NONE',  ( 174.6263263390559928, 276.7176742049951486, -16.26821278762835732 ) ) ;
#11341 = CARTESIAN_POINT ( 'NONE',  ( 163.4260108471723640, 247.5848412648317662, 10.45113099391573108 ) ) ;
#11342 = VERTEX_POINT ( 'NONE', #91060 ) ;
#11343 = CARTESIAN_POINT ( 'NONE',  ( 159.4451596000803306, 268.2047196561628084, -16.33042910166371442 ) ) ;
#11344 = ORIENTED_EDGE ( 'NONE', *, *, #66396, .F. ) ;
#11345 = LINE ( 'NONE', #19448, #76745 ) ;
#11346 = ORIENTED_EDGE ( 'NONE', *, *, #91621, .F. ) ;
#11347 = CARTESIAN_POINT ( 'NONE',  ( 168.8123838728505177, 272.7757763755409997, 16.00497778368365331 ) ) ;
#11348 = CARTESIAN_POINT ( 'NONE',  ( 147.1674053649995528, 275.7455720201731424, 6.878590988502374159 ) ) ;
#11349 = CARTESIAN_POINT ( 'NONE',  ( 177.3345340752408674, 288.7672428955659711, -10.08588367977367461 ) ) ;
#11350 = CARTESIAN_POINT ( 'NONE',  ( 70.79402339348382611, 68.13029754943326566, 9.272317926153396783 ) ) ;
#11351 = CARTESIAN_POINT ( 'NONE',  ( 193.5315086250829211, 294.9135581674226501, 13.30815287220877607 ) ) ;
#11353 = CARTESIAN_POINT ( 'NONE',  ( 87.57621950688576362, 43.92368059598960883, 2.290041065490416194 ) ) ;
#11352 = CIRCLE ( 'NONE', #22592, 15.50000000000000000 ) ;
#11354 = EDGE_CURVE ( 'NONE', #71188, #54504, #41461, .T. ) ;
#11355 = CARTESIAN_POINT ( 'NONE',  ( 197.0726333729855639, 289.3071815470320303, -18.06554324141507095 ) ) ;
#11356 = VERTEX_POINT ( 'NONE', #39773 ) ;
#11357 = CARTESIAN_POINT ( 'NONE',  ( 100.3908607700757472, 218.7677522451417644, -5.000000000000041744 ) ) ;
#11358 = CARTESIAN_POINT ( 'NONE',  ( 29.50362127723248662, 19.96004757982091604, -5.678558825948276656 ) ) ;
#11359 = CARTESIAN_POINT ( 'NONE',  ( 164.3022921857394749, 246.0670774647090582, 1.862798784958315856 ) ) ;
#11361 = CARTESIAN_POINT ( 'NONE',  ( 206.4943150373521803, 272.9883502116088039, 11.34100825923693101 ) ) ;
#11360 = CARTESIAN_POINT ( 'NONE',  ( 77.53640704328023503, 49.75990552807767386, -14.96334311224574165 ) ) ;
#11363 = ORIENTED_EDGE ( 'NONE', *, *, #96502, .F. ) ;
#11362 = CARTESIAN_POINT ( 'NONE',  ( 198.6562788533279615, 286.5642271139020636, 17.47134757795404525 ) ) ;
#11364 = VERTEX_POINT ( 'NONE', #85976 ) ;
#11365 = EDGE_CURVE ( 'NONE', #94954, #80395, #62087, .T. ) ;
#11366 = CARTESIAN_POINT ( 'NONE',  ( 190.3324536135930600, 300.9815153424474374, 5.885744744784173754 ) ) ;
#11367 = CARTESIAN_POINT ( 'NONE',  ( 171.5022402205397611, 259.7078029901424543, -14.90461411186678475 ) ) ;
#11368 = EDGE_CURVE ( 'NONE', #35356, #52194, #32702, .T. ) ;
#11369 = CARTESIAN_POINT ( 'NONE',  ( 72.04811769650321196, 71.35602353065118564, 5.168332083721268511 ) ) ;
#11370 = CARTESIAN_POINT ( 'NONE',  ( 119.8042635715768540, 246.6427522451419065, -10.00000000000009592 ) ) ;
#11371 = B_SPLINE_CURVE_WITH_KNOTS ( 'NONE', 3,
 ( #81960, #74353, #89574, #12037 ),
 .UNSPECIFIED., .F., .F.,
 ( 4, 4 ),
 ( 0.01060329708585674990, 0.01613402798502076851 ),
 .UNSPECIFIED. ) ;
#11372 = CARTESIAN_POINT ( 'NONE',  ( 160.5669369365265027, 252.5369025406650678, -14.88991766242778247 ) ) ;
#11373 = CARTESIAN_POINT ( 'NONE',  ( 148.6789780052693004, 273.1274514078948528, -9.289896596434795484 ) ) ;
#11374 = AXIS2_PLACEMENT_3D ( 'NONE', #37260, #99085, #91499 ) ;
#11375 = VERTEX_POINT ( 'NONE', #7922 ) ;
#11376 = LINE ( 'NONE', #80287, #25139 ) ;
#11377 = CARTESIAN_POINT ( 'NONE',  ( 12.62681055351980497, 12.45404122711131656, -8.090169943749478065 ) ) ;
#11378 = DIRECTION ( 'NONE',  ( 0.4999999999999998890, -0.8660254037844385966, 0.000000000000000000 ) ) ;
#11379 = CARTESIAN_POINT ( 'NONE',  ( -8.406493707509316238, 25.24382671950691304, -10.00000000000000000 ) ) ;
#11380 = CARTESIAN_POINT ( 'NONE',  ( 41.14028939449039513, 187.8927522451418213, 10.00000000000009592 ) ) ;
#11381 = CARTESIAN_POINT ( 'NONE',  ( 99.93095832397169431, 222.3768266524160140, 9.188101187500096856 ) ) ;
#11382 = CARTESIAN_POINT ( 'NONE',  ( 82.53545809363272667, 41.02697948193551269, -1.178820010245875682 ) ) ;
#11383 = CARTESIAN_POINT ( 'NONE',  ( 183.6498318386265396, 256.3252116762061519, 1.424693195823348635 ) ) ;
#11384 = CARTESIAN_POINT ( 'NONE',  ( 161.3981413584396876, 253.0972142504356270, -15.11937522241654719 ) ) ;
#11385 = CARTESIAN_POINT ( 'NONE',  ( 19.90436448580963713, 191.4869531367911293, 4.594050593750046652 ) ) ;
#11386 = CARTESIAN_POINT ( 'NONE',  ( -4.170157060006060235, 26.08383846222962887, 10.00000000000000000 ) ) ;
#11387 = EDGE_LOOP ( 'NONE', ( #83839, #16448, #80694, #92794 ) ) ;
#11388 = VERTEX_POINT ( 'NONE', #310 ) ;
#11389 = CARTESIAN_POINT ( 'NONE',  ( 185.5167381441177099, 260.1903814095311986, -5.802878996917316456 ) ) ;
#11390 = CARTESIAN_POINT ( 'NONE',  ( 66.88838894469625984, 68.52338324295652683, 4.302485449169815013 ) ) ;
#11391 = CARTESIAN_POINT ( 'NONE',  ( 193.2033031094106263, 263.3857463355129198, -3.783757748560594880 ) ) ;
#11392 = CARTESIAN_POINT ( 'NONE',  ( 207.2167723318516153, 271.7370174712370954, -6.606038862010207957 ) ) ;
#11393 = CARTESIAN_POINT ( 'NONE',  ( 181.8935795008488867, 285.0832480758294309, 15.32078685669571882 ) ) ;
#11394 = CARTESIAN_POINT ( 'NONE',  ( 168.1183126599903517, 251.5151909822113225, 10.70881076761038031 ) ) ;
#11395 = CARTESIAN_POINT ( 'NONE',  ( 51.37958267218910180, 188.2202760586659451, -5.415160957724236172E-17 ) ) ;
#11396 = CARTESIAN_POINT ( 'NONE',  ( 80.97745796857449818, 230.8927522451419350, 2.944929066748280225E-16 ) ) ;
#11397 = CARTESIAN_POINT ( 'NONE',  ( -16.14350997085658435, 56.98620320469874656, 0.000000000000000000 ) ) ;
#11398 = CARTESIAN_POINT ( 'NONE',  ( 178.7556533234623544, 259.1617598374694467, -10.24969492202171750 ) ) ;
#11399 = EDGE_CURVE ( 'NONE', #52618, #31479, #39112, .T. ) ;
#11400 = CARTESIAN_POINT ( 'NONE',  ( -1.069254392388470976, 164.0643266524160140, 9.188101187500095079 ) ) ;
#11401 = CARTESIAN_POINT ( 'NONE',  ( 69.12006753439638373, 64.33743317121387406, -11.97457433615276123 ) ) ;
#11402 = CARTESIAN_POINT ( 'NONE',  ( 151.0013883899287066, 269.1049186256390726, -14.25461351222133466 ) ) ;
#11403 = LINE ( 'NONE', #51356, #53187 ) ;
#11404 = CARTESIAN_POINT ( 'NONE',  ( 147.5749551500760788, 275.0396750858066639, -4.254929048021584670 ) ) ;
#11405 = EDGE_CURVE ( 'NONE', #2950, #29361, #55482, .T. ) ;
#11406 = CARTESIAN_POINT ( 'NONE',  ( 179.4583960273904211, 270.4090523040318885, 17.47970616590194837 ) ) ;
#11407 = CARTESIAN_POINT ( 'NONE',  ( 204.9004517216375518, 275.7490024547470853, 14.55104398969427670 ) ) ;
#11408 = CARTESIAN_POINT ( 'NONE',  ( 73.27344031762339682, 213.1115022471902591, 10.00000000000009592 ) ) ;
#11409 = LINE ( 'NONE', #49879, #19166 ) ;
#11410 = VERTEX_POINT ( 'NONE', #31682 ) ;
#11411 = CARTESIAN_POINT ( 'NONE',  ( 207.6471633721571379, 270.9915583223058206, 2.196965492132801678 ) ) ;
#11412 = CARTESIAN_POINT ( 'NONE',  ( 0.02212491418958350761, 177.4865022471903160, 10.00000000000009237 ) ) ;
#11413 = CARTESIAN_POINT ( 'NONE',  ( 85.22110914792114045, 48.09116874191089153, 12.16284421431235785 ) ) ;
#11414 = CARTESIAN_POINT ( 'NONE',  ( 116.8724067376222706, 238.2833772461660544, -9.188101187500095079 ) ) ;
#11415 = CARTESIAN_POINT ( 'NONE',  ( 25.38156110457203241, 15.44966523072494624, -2.296566073217252530E-15 ) ) ;
#11417 = ADVANCED_FACE ( 'NONE', ( #63602 ), #86469, .T. ) ;
#11416 = CARTESIAN_POINT ( 'NONE',  ( 75.25260660042954441, 66.87649888114015084, 12.86011724376103338 ) ) ;
#11418 = AXIS2_PLACEMENT_3D ( 'NONE', #53449, #53935, #15953 ) ;
#11419 = DIRECTION ( 'NONE',  ( -0.5000000000000002220, 0.8660254037844384856, 1.387778780781440548E-15 ) ) ;
#11421 = CYLINDRICAL_SURFACE ( 'NONE', #61886, 17.82106496071139645 ) ;
#11420 = CARTESIAN_POINT ( 'NONE',  ( 196.4994169513186364, 290.3000215130921902, 16.82935102260526961 ) ) ;
#11422 = CARTESIAN_POINT ( 'NONE',  ( 190.7283684373172434, 300.2957707522874102, -6.596676114545077851 ) ) ;
#11423 = ORIENTED_EDGE ( 'NONE', *, *, #81877, .T. ) ;
#11424 = CARTESIAN_POINT ( 'NONE',  ( 151.3284628043366524, 268.5384091220288383, 14.49047510809488237 ) ) ;
#11425 = CARTESIAN_POINT ( 'NONE',  ( 196.3174919959537306, 290.6151247789487684, -17.61248417473235151 ) ) ;
#11426 = CARTESIAN_POINT ( 'NONE',  ( 190.4273386993099280, 300.1655951281246075, 3.362114210485594779 ) ) ;
#11427 = CARTESIAN_POINT ( 'NONE',  ( 173.0801454197684279, 289.8428614808497059, -1.592028862751424301 ) ) ;
#11428 = CARTESIAN_POINT ( 'NONE',  ( 81.62004238798716926, 55.61031524971931361, -16.33394531952002993 ) ) ;
#11429 = EDGE_LOOP ( 'NONE', ( #87997, #31954, #55015, #25919 ) ) ;
#11430 = CARTESIAN_POINT ( 'NONE',  ( 189.0071503145738632, 265.7560967367359694, 11.07595847811888135 ) ) ;
#11431 = CARTESIAN_POINT ( 'NONE',  ( 165.4151454494500513, 269.5741751986499253, -16.33037408709135008 ) ) ;
#11432 = EDGE_CURVE ( 'NONE', #36629, #21068, #382, .T. ) ;
#11433 = EDGE_CURVE ( 'NONE', #55151, #19809, #18518, .T. ) ;
#11434 = CARTESIAN_POINT ( 'NONE',  ( 85.24547482218825678, 44.72709687800012546, 7.712155500878341563 ) ) ;
#11435 = CARTESIAN_POINT ( 'NONE',  ( -9.055497838557604595, 23.87190447404379157, -10.00000000000000000 ) ) ;
#11436 = CARTESIAN_POINT ( 'NONE',  ( 83.88232353660403362, 51.62541775870871419, -14.39191172970312671 ) ) ;
#11437 = CARTESIAN_POINT ( 'NONE',  ( 71.66369827319218189, 72.02185750324218816, -1.551229696566573502 ) ) ;
#11438 = VECTOR ( 'NONE', #71915, 1000.000000000000000 ) ;
#11439 = CARTESIAN_POINT ( 'NONE',  ( 148.0764158854584593, 274.5517338476317946, 6.287425945023585427 ) ) ;
#11440 = CARTESIAN_POINT ( 'NONE',  ( 194.3471816728315673, 282.8997524079796904, 17.29725935490247579 ) ) ;
#11441 = CARTESIAN_POINT ( 'NONE',  ( 44.74566838383860556, 28.76004757982093807, 5.678558825948272215 ) ) ;
#11442 = CARTESIAN_POINT ( 'NONE',  ( 174.5819976565091736, 273.2228988371514333, -16.37309483920122943 ) ) ;
#11443 = ORIENTED_EDGE ( 'NONE', *, *, #54849, .F. ) ;
#11444 = CARTESIAN_POINT ( 'NONE',  ( 77.84925963432132789, 61.76067837358136359, 16.06420508523131119 ) ) ;
#11445 = CARTESIAN_POINT ( 'NONE',  ( 147.8819534105757043, 274.5079385007862811, -9.338341377131436971 ) ) ;
#11446 = CARTESIAN_POINT ( 'NONE',  ( 72.06470348997973474, 72.25603645428110156, 1.367373202405273602 ) ) ;
#11447 = ORIENTED_EDGE ( 'NONE', *, *, #26867, .T. ) ;
#11448 = CARTESIAN_POINT ( 'NONE',  ( 78.75376543412218666, 59.99366791223036444, 16.11417685114693299 ) ) ;
#11449 = CARTESIAN_POINT ( 'NONE',  ( 184.9969017503452164, 291.7732855071091649, 12.02731214230744428 ) ) ;
#11450 = VERTEX_POINT ( 'NONE', #85459 ) ;
#11451 = DIRECTION ( 'NONE',  ( -0.6123724356958050175, -0.3535533905932800591, -0.7071067811865352493 ) ) ;
#11452 = CARTESIAN_POINT ( 'NONE',  ( 84.55094438110296551, 49.89265462440669552, -13.67900519688966021 ) ) ;
#11453 = CARTESIAN_POINT ( 'NONE',  ( 185.0543182570741294, 259.9533911388629690, -5.863674189508556900 ) ) ;
#11454 = ORIENTED_EDGE ( 'NONE', *, *, #45369, .F. ) ;
#11455 = EDGE_CURVE ( 'NONE', #63771, #11090, #35570, .T. ) ;
#11457 = VERTEX_POINT ( 'NONE', #1819 ) ;
#11456 =( BOUNDED_CURVE ( )  B_SPLINE_CURVE ( 2, ( #56217, #25331, #87214, #34433, #64336, #42029, #17749, #48649, #79584, #10145, #41010, #18746, #87714 ),
 .UNSPECIFIED., .F., .T. ) 
 B_SPLINE_CURVE_WITH_KNOTS ( ( 3, 2, 2, 2, 2, 2, 3 ),
 ( 0.06250000000000000000, 0.06500000000000000222, 0.07000000000000000666, 0.07499999999999999722, 0.08000000000000000167, 0.08500000000000000611, 0.08750000000000000833 ),
 .UNSPECIFIED. ) 
 CURVE ( )  GEOMETRIC_REPRESENTATION_ITEM ( )  RATIONAL_B_SPLINE_CURVE ( ( 0.9755282581475768211, 0.9755282581475768211, 1.000000000000000000, 0.9510565162951535312, 1.000000000000000000, 0.9510565162951535312, 1.000000000000000000, 0.9510565162951535312, 1.000000000000000000, 0.9510565162951535312, 1.000000000000000000, 0.9755282581475767101, 0.9755282581475768211 ) ) 
 REPRESENTATION_ITEM ( '' )  );
#11458 = CARTESIAN_POINT ( 'NONE',  ( 175.8048057498829735, 259.3838861800913946, 12.42913708267750472 ) ) ;
#11459 = VERTEX_POINT ( 'NONE', #25095 ) ;
#11460 = FACE_BOUND ( 'NONE', #36476, .T. ) ;
#11461 = ORIENTED_EDGE ( 'NONE', *, *, #60254, .T. ) ;
#11462 = CARTESIAN_POINT ( 'NONE',  ( 74.79904262356255629, 57.81733164762822241, 15.98236516859485867 ) ) ;
#11463 = CARTESIAN_POINT ( 'NONE',  ( 203.4682009197399566, 278.2297336128146412, -15.36039508894693206 ) ) ;
#11464 = ORIENTED_EDGE ( 'NONE', *, *, #5199, .F. ) ;
#11465 = EDGE_CURVE ( 'NONE', #76337, #82333, #67898, .T. ) ;
#11466 = CARTESIAN_POINT ( 'NONE',  ( 182.9784873362611961, 280.4349440833490235, -16.11357538915770604 ) ) ;
#11467 =( BOUNDED_CURVE ( )  B_SPLINE_CURVE ( 2, ( #94288, #40028, #93794, #70968, #56237, #87230, #69936, #17764, #1570 ),
 .UNSPECIFIED., .F., .T. ) 
 B_SPLINE_CURVE_WITH_KNOTS ( ( 3, 2, 2, 2, 3 ),
 ( 0.6008064516129032473, 0.6021505376344086224, 0.6048387096774193727, 0.6075268817204301230, 0.6088709677419354982 ),
 .UNSPECIFIED. ) 
 CURVE ( )  GEOMETRIC_REPRESENTATION_ITEM ( )  RATIONAL_B_SPLINE_CURVE ( ( 0.9330127018922194093, 0.9330127018922194093, 1.000000000000000000, 0.8660254037844387076, 1.000000000000000000, 0.8660254037844387076, 1.000000000000000000, 0.9330127018922194093, 0.9330127018922194093 ) ) 
 REPRESENTATION_ITEM ( '' )  );
#11468 = CARTESIAN_POINT ( 'NONE',  ( 82.16908567409906539, 40.68835713038597390, 3.666464688308268993 ) ) ;
#11469 = CARTESIAN_POINT ( 'NONE',  ( 151.5020479237435609, 268.6693028843759521, 14.46568410587973652 ) ) ;
#11470 = CARTESIAN_POINT ( 'NONE',  ( 160.7509603171012031, 276.3162894764463431, -12.59630221962144958 ) ) ;
#11471 = CARTESIAN_POINT ( 'NONE',  ( 193.0065576635309412, 296.3498312632291913, -11.90044991639595295 ) ) ;
#11472 = CARTESIAN_POINT ( 'NONE',  ( 152.6621968174709991, 266.2283140474973493, -17.02835521334403168 ) ) ;
#11473 = CARTESIAN_POINT ( 'NONE',  ( 85.48084685767805979, 42.33396824294695904, -2.482615992588285803 ) ) ;
#11474 = CARTESIAN_POINT ( 'NONE',  ( 3.854092266844447501, 28.45370138451379560, -10.00000000000000000 ) ) ;
#11475 = EDGE_CURVE ( 'NONE', #121, #35007, #46389, .T. ) ;
#11476 = CARTESIAN_POINT ( 'NONE',  ( 144.5855667544892924, 242.0327760586659451, 1.948934522072303157E-15 ) ) ;
#11477 = CARTESIAN_POINT ( 'NONE',  ( 88.03957972502300322, 43.60450335154009593, 0.01945071491020158166 ) ) ;
#11478 = CARTESIAN_POINT ( 'NONE',  ( 10.98031343905817714, 14.84335787977761001, 9.188101187500006262 ) ) ;
#11479 = VERTEX_POINT ( 'NONE', #86973 ) ;
#11480 = EDGE_CURVE ( 'NONE', #46907, #88625, #17505, .T. ) ;
#11482 = EDGE_LOOP ( 'NONE', ( #47390, #93843, #95824, #39453, #50357 ) ) ;
#11481 = CARTESIAN_POINT ( 'NONE',  ( 85.45699573997251264, 48.32332763657781527, -12.23527099237750981 ) ) ;
#11483 = EDGE_CURVE ( 'NONE', #94973, #64873, #72785, .T. ) ;
#11484 = DIRECTION ( 'NONE',  ( 0.4999999999999992784, -0.8660254037844390407, 0.000000000000000000 ) ) ;
#11485 = CARTESIAN_POINT ( 'NONE',  ( 128.9696990949622659, 235.2677522451417929, -5.000000000000041744 ) ) ;
#11486 = CARTESIAN_POINT ( 'NONE',  ( 157.3343857493933058, 280.1478128481105045, -6.988461411397997480 ) ) ;
#11487 = CARTESIAN_POINT ( 'NONE',  ( 34.98558885611105751, 202.5530062829863027, -4.648177544792955347E-16 ) ) ;
#11488 = CARTESIAN_POINT ( 'NONE',  ( 176.2024152284932370, 253.2971236404176238, 6.345151448921726001 ) ) ;
#11489 = CARTESIAN_POINT ( 'NONE',  ( -110.0000000000000142, 15.00000000000000000, -9.212605237762117483 ) ) ;
#11490 = CARTESIAN_POINT ( 'NONE',  ( 88.11584858642071083, 44.14570234724004649, -1.721659289381729963 ) ) ;
#11491 = ORIENTED_EDGE ( 'NONE', *, *, #50591, .F. ) ;
#11492 = CARTESIAN_POINT ( 'NONE',  ( 184.3893518601747417, 272.5925419477008518, -17.24544351097261696 ) ) ;
#11493 = CARTESIAN_POINT ( 'NONE',  ( 65.83788420375942962, 69.13770088707153150, 0.1877971835443447424 ) ) ;
#11494 = ORIENTED_EDGE ( 'NONE', *, *, #31829, .F. ) ;
#11495 = CARTESIAN_POINT ( 'NONE',  ( 162.1283350843791311, 276.5786735129873932, 12.83412388560665285 ) ) ;
#11496 = B_SPLINE_CURVE_WITH_KNOTS ( 'NONE', 3,
 ( #44413, #67727, #73838, #98651, #44906, #4428, #37310, #8911, #92555, #30722 ),
 .UNSPECIFIED., .F., .F.,
 ( 4, 2, 2, 2, 4 ),
 ( 0.000000000000000000, 0.0002622400424273968922, 0.0005244800848547937844, 0.0007867201272821907308, 0.001048960169709587569 ),
 .UNSPECIFIED. ) ;
#11497 = CARTESIAN_POINT ( 'NONE',  ( 156.6021870925794133, 276.9767950607789544, 9.957507455165190535 ) ) ;
#11498 = DIRECTION ( 'NONE',  ( -0.000000000000000000, 0.000000000000000000, 1.000000000000000000 ) ) ;
#11499 = CARTESIAN_POINT ( 'NONE',  ( 149.6700657135140489, 271.4108371424580355, 12.58635654151485284 ) ) ;
#11500 = CARTESIAN_POINT ( 'NONE',  ( 162.9796882977680639, 248.3578945969637743, 9.683801903336119565 ) ) ;
#11502 = CARTESIAN_POINT ( 'NONE',  ( 88.16334560026523093, 43.89615744693332289, 2.509484348711646273 ) ) ;
#11501 = CARTESIAN_POINT ( 'NONE',  ( 171.7948998666937541, 269.4667684067869686, 17.81952346552377620 ) ) ;
#11503 = CARTESIAN_POINT ( 'NONE',  ( 67.06923665261433598, 197.9824982072973967, 3.021315404115420679E-15 ) ) ;
#11504 = ORIENTED_EDGE ( 'NONE', *, *, #52956, .F. ) ;
#11505 = CARTESIAN_POINT ( 'NONE',  ( 75.20678305874149316, 61.44858071201250027, -15.30768782187949029 ) ) ;
#11506 = DIRECTION ( 'NONE',  ( 1.000000000000000000, 0.000000000000000000, 0.000000000000000000 ) ) ;
#11507 = CARTESIAN_POINT ( 'NONE',  ( 72.59318785522671647, 65.75921281613393887, -12.50631930651069723 ) ) ;
#11508 = CARTESIAN_POINT ( 'NONE',  ( 192.7944000592152634, 296.7172990131160759, 11.44860011299869740 ) ) ;
#11509 = CARTESIAN_POINT ( 'NONE',  ( 80.93651615306337987, 43.67145026278060271, -9.552024319604889513 ) ) ;
#11510 = CARTESIAN_POINT ( 'NONE',  ( 110.3297989853572005, 246.0530062829863311, -4.648177544792955347E-16 ) ) ;
#11511 = CARTESIAN_POINT ( 'NONE',  ( 7.238742955462222461, 184.1744531367911293, 4.594050593750047540 ) ) ;
#11512 = CARTESIAN_POINT ( 'NONE',  ( 104.8563042601131770, 231.3458772461660544, 9.188101187500095079 ) ) ;
#11513 = CARTESIAN_POINT ( 'NONE',  ( 154.8545429534089237, 262.4310591522755089, -17.81746354318405778 ) ) ;
#11514 = CARTESIAN_POINT ( 'NONE',  ( 88.01192408641850307, 44.27121890238829138, -4.391744778743014166 ) ) ;
#11515 = CARTESIAN_POINT ( 'NONE',  ( 186.7639553457436534, 295.8781545368645425, -7.658116578984559553 ) ) ;
#11516 = CARTESIAN_POINT ( 'NONE',  ( -2.503782513514959174, 159.3615022471902023, 5.000000000000051514 ) ) ;
#11517 = LINE ( 'NONE', #81434, #36087 ) ;
#11518 = CARTESIAN_POINT ( 'NONE',  ( 163.4597682148788920, 284.3339965611676803, 5.988904932330388675 ) ) ;
#11519 = CARTESIAN_POINT ( 'NONE',  ( 194.4826705584825390, 293.7931287314651740, -16.11258321617245315 ) ) ;
#11520 = CARTESIAN_POINT ( 'NONE',  ( 181.8379482810746879, 291.5118755679804963, 9.487367419015216186 ) ) ;
#11521 = CARTESIAN_POINT ( 'NONE',  ( 164.7432774000302800, 245.3032686681709720, -5.267720626764685221 ) ) ;
#11522 = CARTESIAN_POINT ( 'NONE',  ( 75.67111234668428210, 55.92069150990298709, -16.15888377404129628 ) ) ;
#11523 = CARTESIAN_POINT ( 'NONE',  ( 79.57426776854913442, 46.24084366570346560, -13.18946159588284139 ) ) ;
#11524 = CARTESIAN_POINT ( 'NONE',  ( 172.9438399295877957, 262.8668947608421718, -16.49499919880818766 ) ) ;
#11525 = CARTESIAN_POINT ( 'NONE',  ( 86.99453030705913648, 221.0333772461660544, 9.188101187500095079 ) ) ;
#11526 = CARTESIAN_POINT ( 'NONE',  ( 207.8996209429610360, 270.5542889829179103, -5.987818313449536411 ) ) ;
#11528 = EDGE_CURVE ( 'NONE', #46236, #62365, #7340, .T. ) ;
#11527 = CARTESIAN_POINT ( 'NONE',  ( -112.5954152546897120, 74.04580364311804885, -30.52142883766498116 ) ) ;
#11529 = CARTESIAN_POINT ( 'NONE',  ( -16.75143828124104317, 104.0219442184326937, 12.69405866495271695 ) ) ;
#11530 = CARTESIAN_POINT ( 'NONE',  ( 195.6986305151803549, 291.6870243064952888, 16.84182339398051909 ) ) ;
#11531 = CARTESIAN_POINT ( 'NONE',  ( 151.0388915836658725, 269.0399611886400635, -14.24896787280406585 ) ) ;
#11532 = CARTESIAN_POINT ( 'NONE',  ( 173.1967572896427043, 268.2116334800467143, -16.29158950216322665 ) ) ;
#11533 = CARTESIAN_POINT ( 'NONE',  ( 32.39518414388500389, 34.10171378149921395, 9.188101187500008038 ) ) ;
#11534 = CARTESIAN_POINT ( 'NONE',  ( 128.5163324648304410, 256.5530062829863027, -4.648177544792955347E-16 ) ) ;
#11535 = CARTESIAN_POINT ( 'NONE',  ( 129.0599100780709421, 251.9865022471902876, -10.00000000000009592 ) ) ;
#11536 = ORIENTED_EDGE ( 'NONE', *, *, #43100, .F. ) ;
#11537 = CARTESIAN_POINT ( 'NONE',  ( 18.53877768333398990, 26.10171378149918198, 9.188101187500008038 ) ) ;
#11538 = CARTESIAN_POINT ( 'NONE',  ( 75.14063404487711750, 220.3149278399160664, -9.188101187500095079 ) ) ;
#11539 = CARTESIAN_POINT ( 'NONE',  ( 173.0274122914222517, 289.6322751625752403, -1.044431133429226000 ) ) ;
#11540 = CARTESIAN_POINT ( 'NONE',  ( -30.74734981195323158, 93.63450014558806345, 11.75270985346817909 ) ) ;
#11541 = CARTESIAN_POINT ( 'NONE',  ( 191.3058253459265075, 288.7823831380905517, -16.22814272653723933 ) ) ;
#11542 = EDGE_CURVE ( 'NONE', #82653, #2846, #66104, .T. ) ;
#11543 = EDGE_CURVE ( 'NONE', #23912, #41184, #48452, .T. ) ;
#11544 = CARTESIAN_POINT ( 'NONE',  ( 86.72415995732357885, 47.00718562526229505, 10.33097223407348686 ) ) ;
#11545 = CARTESIAN_POINT ( 'NONE',  ( 193.7119801207757064, 288.2734703750227823, 16.20783580877855456 ) ) ;
#11546 = CARTESIAN_POINT ( 'NONE',  ( 72.36540186540696595, 71.57331123994032396, 5.085634937608116246 ) ) ;
#11547 = CARTESIAN_POINT ( 'NONE',  ( 126.6061714340151241, 237.2365022471902023, -10.00000000000009059 ) ) ;
#11548 = FACE_BOUND ( 'NONE', #36641, .T. ) ;
#11549 = CARTESIAN_POINT ( 'NONE',  ( 75.10222324744135847, 53.09139496487031806, 16.49549906635234819 ) ) ;
#11550 = ORIENTED_EDGE ( 'NONE', *, *, #51791, .T. ) ;
#11551 = CARTESIAN_POINT ( 'NONE',  ( 165.5623119752849846, 246.9337586618608498, -1.855523153196440234 ) ) ;
#11552 = ORIENTED_EDGE ( 'NONE', *, *, #35650, .T. ) ;
#11553 = CARTESIAN_POINT ( 'NONE',  ( 202.2773826701151165, 280.2922913237452462, 16.62862787739668846 ) ) ;
#11554 = CARTESIAN_POINT ( 'NONE',  ( 110.0000000000000000, 15.00000000000003908, 59.99999999999999289 ) ) ;
#11555 = DIRECTION ( 'NONE',  ( 1.000000000000000000, 0.000000000000000000, 0.000000000000000000 ) ) ;
#11556 = ORIENTED_EDGE ( 'NONE', *, *, #10728, .T. ) ;
#11557 = FACE_OUTER_BOUND ( 'NONE', #50919, .T. ) ;
#11558 = VERTEX_POINT ( 'NONE', #12419 ) ;
#11559 = CARTESIAN_POINT ( 'NONE',  ( 188.9581516566892674, 290.6722666539587863, 14.45932873867149482 ) ) ;
#11560 = CARTESIAN_POINT ( 'NONE',  ( 5.287540158160898507, 21.79103043416546726, 8.090169943749478065 ) ) ;
#11561 = CARTESIAN_POINT ( 'NONE',  ( 143.8814004702669536, 260.0024278399161517, 9.188101187500095079 ) ) ;
#11562 = CARTESIAN_POINT ( 'NONE',  ( 87.77887691218910504, 44.16646017302762317, -4.484802941535585674 ) ) ;
#11563 = CARTESIAN_POINT ( 'NONE',  ( 201.6662765003921152, 274.8599008263099677, -14.23589684381435738 ) ) ;
#11564 = CARTESIAN_POINT ( 'NONE',  ( 32.07042461746583939, 33.91421378149920685, 9.188101187500008038 ) ) ;
#11565 = CYLINDRICAL_SURFACE ( 'NONE', #60723, 17.82106496071139645 ) ;
#11566 = CARTESIAN_POINT ( 'NONE',  ( 168.1726423428391399, 255.4859975196775963, 14.21197738914692366 ) ) ;
#11567 = CARTESIAN_POINT ( 'NONE',  ( 45.92147131476482969, 203.9865022471903160, -10.00000000000009592 ) ) ;
#11568 = EDGE_LOOP ( 'NONE', ( #35486, #53010, #99322, #26926 ) ) ;
#11569 = VECTOR ( 'NONE', #39557, 1000.000000000000000 ) ;
#11570 = EDGE_LOOP ( 'NONE', ( #15358, #60350, #81884, #54239 ) ) ;
#11571 = CARTESIAN_POINT ( 'NONE',  ( 184.2559797716583603, 296.4936185974571572, 1.018868464677917363 ) ) ;
#11572 = ADVANCED_FACE ( 'NONE', ( #50894 ), #27119, .F. ) ;
#11574 = CARTESIAN_POINT ( 'NONE',  ( 194.6310785344323904, 293.5360785768717165, -14.54510914272505495 ) ) ;
#11573 = CARTESIAN_POINT ( 'NONE',  ( 204.4781092559247782, 276.4805210635553863, 13.30606382016679490 ) ) ;
#11575 = CARTESIAN_POINT ( 'NONE',  ( 85.94639921072385391, 48.27664717140825701, 11.96740676232643352 ) ) ;
#11576 = CARTESIAN_POINT ( 'NONE',  ( 201.3394753198586500, 274.7605675011590733, -14.24554608861767946 ) ) ;
#11577 = CARTESIAN_POINT ( 'NONE',  ( 147.6453533338496129, 276.1788777465205840, 0.8289047639747788576 ) ) ;
#11578 = CARTESIAN_POINT ( 'NONE',  ( 157.7593757092099906, 257.3997412317380054, -18.08445832352326121 ) ) ;
#11579 = CARTESIAN_POINT ( 'NONE',  ( -27.42236680055714260, 166.5217562850347406, 1.224646799147364892E-15 ) ) ;
#11580 = CARTESIAN_POINT ( 'NONE',  ( 168.2018854272548083, 266.5653299185787546, 16.61820373829572617 ) ) ;
#11581 = CARTESIAN_POINT ( 'NONE',  ( 179.6412324868688302, 256.3037255040319451, 4.896461366237743640 ) ) ;
#11582 = EDGE_CURVE ( 'NONE', #85223, #20973, #65107, .T. ) ;
#11583 = CARTESIAN_POINT ( 'NONE',  ( 103.5572661544365332, 230.5958772461660260, -9.188101187500095079 ) ) ;
#11584 = ORIENTED_EDGE ( 'NONE', *, *, #12887, .T. ) ;
#11585 = CARTESIAN_POINT ( 'NONE',  ( 3.854092266844447501, 28.45370138451379560, -10.00000000000000000 ) ) ;
#11586 = CARTESIAN_POINT ( 'NONE',  ( 163.3044915899828879, 276.5565773319555660, -13.83122682706599704 ) ) ;
#11587 = ORIENTED_EDGE ( 'NONE', *, *, #77834, .T. ) ;
#11588 = ORIENTED_EDGE ( 'NONE', *, *, #4795, .T. ) ;
#11589 = CARTESIAN_POINT ( 'NONE',  ( 87.11651898459504650, 46.29685661633757832, -9.218154771921559743 ) ) ;
#11590 = EDGE_CURVE ( 'NONE', #33116, #9076, #56993, .T. ) ;
#11591 = CARTESIAN_POINT ( 'NONE',  ( 176.8027066500977469, 292.5242457368331657, -2.743196636303242730 ) ) ;
#11592 = CARTESIAN_POINT ( 'NONE',  ( 37.75007554933399234, 22.76426979415092333, 3.090169943749476733 ) ) ;
#11593 = CARTESIAN_POINT ( 'NONE',  ( 206.6298919378964740, 272.7535241315335384, -9.267551915974392429 ) ) ;
#11594 = CARTESIAN_POINT ( 'NONE',  ( 208.2995279947827783, 269.8616296508574237, 2.738519832864397152 ) ) ;
#11595 = CARTESIAN_POINT ( 'NONE',  ( 95.14032143958276322, 234.9244531367911009, -4.594050593750046652 ) ) ;
#11596 = ORIENTED_EDGE ( 'NONE', *, *, #70963, .T. ) ;
#11597 = B_SPLINE_CURVE_WITH_KNOTS ( 'NONE', 3,
 ( #72277, #55039, #55527, #87021, #86020, #2373, #17552, #54523, #85504, #70243, #33251, #64152, #95103, #848, #16546, #62127, #48459, #32746, #78371, #56547, #8454, #31241, #16051, #87534, #18066, #8952, #48962, #41337, #93075, #39819, #46952, #79401, #1862, #17044, #39326, #32248, #70751, #47442, #1364, #47935, #63148, #40333, #71272, #73265, #97099, #12975, #49955, #57539 ),
 .UNSPECIFIED., .F., .F.,
 ( 4, 2, 2, 2, 2, 2, 2, 2, 2, 2, 2, 2, 2, 2, 2, 2, 2, 2, 2, 2, 2, 2, 2, 4 ),
 ( 0.0002509531133599470203, 0.0007282208505926920017, 0.001205488587825436983, 0.001444122456441809419, 0.001563439390749959967, 0.001682756325058110732, 0.001802073259366261280, 0.001921390193674411828, 0.002160024062290898106, 0.002637291799524055409, 0.003114559536757212713, 0.004069095011223527319, 0.005023630485689842794, 0.005500898222923000097, 0.005739532091539544488, 0.005978165960156088012, 0.006037824427310304123, 0.006097482894464520235, 0.006216799828772952459, 0.006455433697389797824, 0.006932701434623462534, 0.007409969171857128112, 0.007648603040473891945, 0.007887236909090657513 ),
 .UNSPECIFIED. ) ;
#11598 = ORIENTED_EDGE ( 'NONE', *, *, #31216, .T. ) ;
#11599 = DIRECTION ( 'NONE',  ( -0.8951289669282589401, 0.4458072818673421422, 0.000000000000000000 ) ) ;
#11600 = CARTESIAN_POINT ( 'NONE',  ( 49.07419501245632176, 91.40403951869188859, -10.00000000000000000 ) ) ;
#11601 = ORIENTED_EDGE ( 'NONE', *, *, #80048, .T. ) ;
#11602 = CARTESIAN_POINT ( 'NONE',  ( 194.6936158627724751, 266.3821769738702869, -7.823464608937872988 ) ) ;
#11603 = DIRECTION ( 'NONE',  ( -0.8660254037844387076, -0.4999999999999998890, -0.000000000000000000 ) ) ;
#11604 = CARTESIAN_POINT ( 'NONE',  ( 68.91323701008126079, 69.24239215680682946, -5.639282044092864155 ) ) ;
#11606 = CARTESIAN_POINT ( 'NONE',  ( 69.48953819294759171, 62.61851694872117235, -13.86937595337403728 ) ) ;
#11605 = CARTESIAN_POINT ( 'NONE',  ( 134.5719744753492364, 242.3768266524159856, -9.188101187500091527 ) ) ;
#11607 = CARTESIAN_POINT ( 'NONE',  ( -16.52256874082355864, 171.2677522451419350, -5.000000000000047962 ) ) ;
#11608 = CARTESIAN_POINT ( 'NONE',  ( -56.16025090550425602, 33.03454289568183100, -10.00000000000000000 ) ) ;
#11609 = ORIENTED_EDGE ( 'NONE', *, *, #90867, .T. ) ;
#11610 = CARTESIAN_POINT ( 'NONE',  ( 204.3531539698473978, 276.6969499677158524, 13.47943239092699841 ) ) ;
#11611 = CARTESIAN_POINT ( 'NONE',  ( 160.7477323183478006, 275.4922477318379492, 13.14247883376535420 ) ) ;
#11612 = CARTESIAN_POINT ( 'NONE',  ( 82.16988580781558937, 40.62906898968385860, -3.430093734972964548 ) ) ;
#11613 = CARTESIAN_POINT ( 'NONE',  ( 189.3527614026753270, 269.6247310899153149, 15.08597367144959733 ) ) ;
#11614 = CARTESIAN_POINT ( 'NONE',  ( 178.5210264805825204, 285.2939240913069625, 14.13561587336957359 ) ) ;
#11615 = CARTESIAN_POINT ( 'NONE',  ( 65.88310562893973099, 69.02589174555536999, 1.996831191813060347 ) ) ;
#11616 = CARTESIAN_POINT ( 'NONE',  ( 188.3784916956350344, 286.3721210266486992, -16.81851773412965301 ) ) ;
#11617 = CARTESIAN_POINT ( 'NONE',  ( 123.8637576553643100, 248.9865022471902876, -10.00000000000009592 ) ) ;
#11618 = CARTESIAN_POINT ( 'NONE',  ( 161.6256441450323678, 250.7031678651938762, 14.48526717260977037 ) ) ;
#11619 = CARTESIAN_POINT ( 'NONE',  ( 70.42903375700203128, 70.52137667656469944, -4.659989608922488813 ) ) ;
#11620 = CARTESIAN_POINT ( 'NONE',  ( 206.8659638600981623, 272.3446355680395641, -10.26115277030573125 ) ) ;
#11621 = CARTESIAN_POINT ( 'NONE',  ( 83.39698567699524290, 51.83659370627650276, 14.98600084375454244 ) ) ;
#11622 = CARTESIAN_POINT ( 'NONE',  ( 163.2256942281324541, 247.9317998266098471, -9.780520296312531059 ) ) ;
#11623 = ADVANCED_FACE ( 'NONE', ( #96055 ), #19537, .T. ) ;
#11624 = DIRECTION ( 'NONE',  ( 0.000000000000000000, 0.000000000000000000, 1.000000000000000000 ) ) ;
#11625 = CARTESIAN_POINT ( 'NONE',  ( -11.26211276271278194, 158.5313752282681605, 5.249404841173988696E-14 ) ) ;
#11626 = CARTESIAN_POINT ( 'NONE',  ( 71.55914530767435622, 64.65954455392433431, -12.81547558104803031 ) ) ;
#11627 = CARTESIAN_POINT ( 'NONE',  ( 182.5610248314471846, 264.1229073254193622, 14.12000187221130609 ) ) ;
#11628 = CARTESIAN_POINT ( 'NONE',  ( 78.86178680068651659, 50.42561631414478285, 15.44278421312068694 ) ) ;
#11629 = CARTESIAN_POINT ( 'NONE',  ( 30.83975393042360480, 33.50829794293883168, -10.00000000000000355 ) ) ;
#11630 = CYLINDRICAL_SURFACE ( 'NONE', #87130, 10.00000000000010658 ) ;
#11631 = SURFACE_STYLE_USAGE ( .BOTH. , #72444 ) ;
#11632 = CARTESIAN_POINT ( 'NONE',  ( 157.6156715759294116, 270.9999693453487453, -14.72877181860486751 ) ) ;
#11633 = CARTESIAN_POINT ( 'NONE',  ( 86.67335767502150645, 43.67802127306630666, -3.448278313570464881 ) ) ;
#11634 = CIRCLE ( 'NONE', #5118, 15.50000000000000000 ) ;
#11635 = CARTESIAN_POINT ( 'NONE',  ( 161.0974665087481981, 251.6179983666593216, -13.69252715295363210 ) ) ;
#11636 = B_SPLINE_CURVE_WITH_KNOTS ( 'NONE', 3,
 ( #40660, #3207, #71597, #2193 ),
 .UNSPECIFIED., .F., .F.,
 ( 4, 4 ),
 ( 0.008328144461416385133, 0.01467133638754275146 ),
 .UNSPECIFIED. ) ;
#11637 = CARTESIAN_POINT ( 'NONE',  ( 11.37951369124782453, 183.5024278399160949, 9.188101187500095079 ) ) ;
#11638 = CARTESIAN_POINT ( 'NONE',  ( 41.52713374746741692, 206.3297689869269220, -2.679491924311252493 ) ) ;
#11639 = EDGE_LOOP ( 'NONE', ( #66708, #86996, #68038, #58250 ) ) ;
#11640 = CARTESIAN_POINT ( 'NONE',  ( 86.70078377113696888, 46.42938884419434942, 9.090660191201401119 ) ) ;
#11641 = LINE ( 'NONE', #66322, #79153 ) ;
#11642 = CARTESIAN_POINT ( 'NONE',  ( 163.8947349411736525, 246.7729873192901664, -5.868803394723933309 ) ) ;
#11643 = CARTESIAN_POINT ( 'NONE',  ( 81.94721816817228444, 41.71691344098891818, 5.409604974753337459 ) ) ;
#11644 = CARTESIAN_POINT ( 'NONE',  ( 36.00728465925030974, 191.5958772461660544, -9.188101187500095079 ) ) ;
#11645 = CARTESIAN_POINT ( 'NONE',  ( 86.94335770270596697, 46.00923847012510493, 8.969699243401572986 ) ) ;
#11646 = CARTESIAN_POINT ( 'NONE',  ( 190.8907028847385448, 300.0145992415348815, -5.421341690443150618 ) ) ;
#11647 = CARTESIAN_POINT ( 'NONE',  ( 31.26830227169403997, 36.79103043416551344, 8.090169943749478065 ) ) ;
#11648 = CARTESIAN_POINT ( 'NONE',  ( 199.5283806629861942, 267.5346968016396545, -6.617246389697492681 ) ) ;
#11649 = CARTESIAN_POINT ( 'NONE',  ( 178.8515547497951559, 293.8219541337840042, 2.692371752549619135 ) ) ;
#11650 = CARTESIAN_POINT ( 'NONE',  ( 179.1981449177366130, 278.3664918542738747, -16.54318165528815143 ) ) ;
#11651 = CARTESIAN_POINT ( 'NONE',  ( 72.08705432318760131, 67.71326266777748515, -10.59477395882420225 ) ) ;
#11652 = CARTESIAN_POINT ( 'NONE',  ( 166.9996108681188218, 257.9679880018421159, -15.33282310006317495 ) ) ;
#11653 = CARTESIAN_POINT ( 'NONE',  ( 83.63860429472313740, 52.00081728452853014, 14.99618877770984859 ) ) ;
#11654 = EDGE_CURVE ( 'NONE', #99059, #63734, #30315, .T. ) ;
#11655 = EDGE_CURVE ( 'NONE', #68082, #84967, #51906, .T. ) ;
#11656 = CARTESIAN_POINT ( 'NONE',  ( 75.36633504343573975, 220.9865022471902876, 10.00000000000009237 ) ) ;
#11657 = CARTESIAN_POINT ( 'NONE',  ( 75.40263629470850049, 53.17004129013850644, 16.48570774626835700 ) ) ;
#11658 = CARTESIAN_POINT ( 'NONE',  ( 37.49256495613256845, 26.81029122506297568, 8.090169943749479842 ) ) ;
#11659 = ORIENTED_EDGE ( 'NONE', *, *, #73090, .T. ) ;
#11660 = CARTESIAN_POINT ( 'NONE',  ( 35.05980905203730913, 200.2369531367911293, -4.594050593750048428 ) ) ;
#11661 = ORIENTED_EDGE ( 'NONE', *, *, #4696, .F. ) ;
#11662 = CARTESIAN_POINT ( 'NONE',  ( 162.6118520434669392, 263.2546530415788766, 17.62269466845149068 ) ) ;
#11663 = CARTESIAN_POINT ( 'NONE',  ( 150.6386650955079176, 269.7331738006648720, -15.06054658539322766 ) ) ;
#11664 = DIRECTION ( 'NONE',  ( 0.000000000000000000, 0.000000000000000000, 1.000000000000000000 ) ) ;
#11665 = ORIENTED_EDGE ( 'NONE', *, *, #5582, .F. ) ;
#11666 = B_SPLINE_CURVE_WITH_KNOTS ( 'NONE', 3,
 ( #15616, #92669, #939, #9035, #84576, #37912, #68822, #70840, #46514, #77452, #77949, #8048, #93674, #24238, #47525, #78453 ),
 .UNSPECIFIED., .F., .F.,
 ( 4, 2, 2, 2, 2, 2, 2, 4 ),
 ( 8.537055041414144432E-15, 0.0005636500808654369178, 0.0008454751212938848128, 0.001127300161722332708, 0.001409125202150780711, 0.001690950242579228715, 0.001972775283007676718, 0.002254600323436124504 ),
 .UNSPECIFIED. ) ;
#11667 = CARTESIAN_POINT ( 'NONE',  ( 171.2998820311650263, 286.5525287771079661, 7.511819249465659709 ) ) ;
#11668 = CARTESIAN_POINT ( 'NONE',  ( 207.1601050488701503, 271.8351680844880889, 6.320235450527015075 ) ) ;
#11669 = CARTESIAN_POINT ( 'NONE',  ( 159.7654401674316205, 278.6271376734871978, -10.85853086775617449 ) ) ;
#11670 = CARTESIAN_POINT ( 'NONE',  ( 29.31959766232195008, 28.87878583063843152, -9.188101187500006262 ) ) ;
#11671 = CARTESIAN_POINT ( 'NONE',  ( 189.0745626194224087, 265.5475558152633653, 10.70054544839699773 ) ) ;
#11672 = CARTESIAN_POINT ( 'NONE',  ( 154.0986224399686648, 280.1916420498395155, 2.233781007141098396 ) ) ;
#11673 = CARTESIAN_POINT ( 'NONE',  ( 171.3843415847181291, 255.6973737389273253, 11.29858615387269083 ) ) ;
#11675 = EDGE_LOOP ( 'NONE', ( #26368, #29342, #92404, #77047 ) ) ;
#11674 = VECTOR ( 'NONE', #13438, 999.9999999999998863 ) ;
#11676 = CARTESIAN_POINT ( 'NONE',  ( 16.48196734934595398, 24.91421378149918198, 9.188101187500008038 ) ) ;
#11677 = CARTESIAN_POINT ( 'NONE',  ( 69.03518170984699509, 64.49507618471645287, 12.45339560606362461 ) ) ;
#11678 = CARTESIAN_POINT ( 'NONE',  ( -44.55566051625979895, 47.72160670319654230, 59.99999999999999289 ) ) ;
#11679 = CYLINDRICAL_SURFACE ( 'NONE', #24591, 45.00000000000000000 ) ;
#11680 = VERTEX_POINT ( 'NONE', #91428 ) ;
#11681 = CARTESIAN_POINT ( 'NONE',  ( 72.25718139279801733, 71.61371966692031776, -5.855127513239330561 ) ) ;
#11682 = CARTESIAN_POINT ( 'NONE',  ( 191.5694459269389824, 298.8389818071599962, 7.944420692511652504 ) ) ;
#11683 = PLANE ( 'NONE',  #23754 ) ;
#11684 = ORIENTED_EDGE ( 'NONE', *, *, #80105, .T. ) ;
#11685 = VERTEX_POINT ( 'NONE', #29111 ) ;
#11686 = EDGE_CURVE ( 'NONE', #92439, #41192, #40701, .T. ) ;
#11688 = CARTESIAN_POINT ( 'NONE',  ( 150.9356804500963278, 270.2479074161392987, -13.67838782973983669 ) ) ;
#11687 = CARTESIAN_POINT ( 'NONE',  ( 161.0974665087481981, 251.6179983666593216, -13.69252715295363210 ) ) ;
#11689 = AXIS2_PLACEMENT_3D ( 'NONE', #82818, #75190, #5765 ) ;
#11690 = CARTESIAN_POINT ( 'NONE',  ( 179.4404154152157105, 291.3709498135804097, -10.08759257512885199 ) ) ;
#11691 = ORIENTED_EDGE ( 'NONE', *, *, #88127, .T. ) ;
#11692 = CARTESIAN_POINT ( 'NONE',  ( 66.15182308703052172, 68.59394279077463352, -2.211977090278242297 ) ) ;
#11693 = CARTESIAN_POINT ( 'NONE',  ( 159.2876523829509665, 254.7526883847961017, 15.64395448151312351 ) ) ;
#11694 = CARTESIAN_POINT ( 'NONE',  ( 73.02887634090247104, 57.43239839248311540, -15.87220953312935201 ) ) ;
#11695 = CARTESIAN_POINT ( 'NONE',  ( 78.03830882516994905, 61.03761899432888782, -15.88690189282890231 ) ) ;
#11696 = CARTESIAN_POINT ( 'NONE',  ( 157.1539462478114615, 258.4483758192793061, -17.96006278656275867 ) ) ;
#11697 = CARTESIAN_POINT ( 'NONE',  ( 115.9249311304092771, 246.9244531367911293, -4.594050593750046652 ) ) ;
#11698 = CARTESIAN_POINT ( 'NONE',  ( -51.42721978966704910, 42.16899896210637877, -10.00000000000000000 ) ) ;
#11699 = CARTESIAN_POINT ( 'NONE',  ( 184.1192235817496794, 260.9197926262456235, 11.00856571192608513 ) ) ;
#11700 = CARTESIAN_POINT ( 'NONE',  ( 201.4510510982464666, 281.3426432124285839, 16.26095448192928927 ) ) ;
#11701 = ORIENTED_EDGE ( 'NONE', *, *, #7264, .F. ) ;
#11702 = CARTESIAN_POINT ( 'NONE',  ( 30.77620441319551503, 35.95586893147757479, 7.433330006724141015 ) ) ;
#11703 = CARTESIAN_POINT ( 'NONE',  ( 159.9014600375868440, 253.6895423408921886, 15.57825579621527368 ) ) ;
#11704 = CARTESIAN_POINT ( 'NONE',  ( 194.6547327110108370, 291.6682678161738522, -16.14356736919946300 ) ) ;
#11705 = CARTESIAN_POINT ( 'NONE',  ( 72.19064823929512897, 221.6744531367911293, 4.594050593750047540 ) ) ;
#11706 = CARTESIAN_POINT ( 'NONE',  ( 169.3571508527084291, 283.0956279022483955, 12.63651818596384935 ) ) ;
#11707 = CARTESIAN_POINT ( 'NONE',  ( 191.4941427383744781, 298.9694107557253346, 8.584406880462095657 ) ) ;
#11708 = CARTESIAN_POINT ( 'NONE',  ( 150.6881537519499830, 269.6474569333088311, 15.31267828461696467 ) ) ;
#11709 = CARTESIAN_POINT ( 'NONE',  ( 172.1891475301837033, 276.7325189785484554, 15.90371275011163910 ) ) ;
#11710 = ORIENTED_EDGE ( 'NONE', *, *, #5964, .T. ) ;
#11711 = CARTESIAN_POINT ( 'NONE',  ( 74.39278055389422661, 58.62799419530674783, -15.82512888129269157 ) ) ;
#11712 = CARTESIAN_POINT ( 'NONE',  ( 88.08526958130826756, 44.05723934618831095, -0.5494347720344661123 ) ) ;
#11713 = FACE_OUTER_BOUND ( 'NONE', #15165, .T. ) ;
#11714 = ORIENTED_EDGE ( 'NONE', *, *, #44332, .T. ) ;
#11715 = CARTESIAN_POINT ( 'NONE',  ( 148.2459810799481943, 273.8774240820723662, 8.845211566752345433 ) ) ;
#11716 = CARTESIAN_POINT ( 'NONE',  ( 68.88217923695410150, 69.54816024699961474, -4.775671802712312619 ) ) ;
#11717 = CARTESIAN_POINT ( 'NONE',  ( 161.1750406344237661, 251.4836360396366501, -14.21198410781773802 ) ) ;
#11718 = CARTESIAN_POINT ( 'NONE',  ( 78.46959274033007148, 206.1115022471901739, -5.000000000000041744 ) ) ;
#11719 = CARTESIAN_POINT ( 'NONE',  ( 61.75705882612326292, 194.9155109091896634, 2.679491924311254714 ) ) ;
#11720 = ADVANCED_FACE ( 'NONE', ( #44286 ), #37962, .F. ) ;
#11721 = CARTESIAN_POINT ( 'NONE',  ( 164.3022921857394749, 246.0670774647090582, 1.862798784958315856 ) ) ;
#11722 = CARTESIAN_POINT ( 'NONE',  ( 151.7991800818630850, 269.5918300736246920, -14.34690986903463283 ) ) ;
#11723 = CARTESIAN_POINT ( 'NONE',  ( 134.6192181478005523, 236.9824982072973967, 3.021315404115420679E-15 ) ) ;
#11724 = CARTESIAN_POINT ( 'NONE',  ( 167.6123132579195953, 256.4410626529074761, 13.64026455462122911 ) ) ;
#11725 = CARTESIAN_POINT ( 'NONE',  ( 207.5195222358739784, 271.2126392554839640, 2.810970398613041432 ) ) ;
#11726 = CARTESIAN_POINT ( 'NONE',  ( 121.9063529450018137, 235.0643266524159856, -9.188101187500093303 ) ) ;
#11727 = ORIENTED_EDGE ( 'NONE', *, *, #98097, .T. ) ;
#11728 = CARTESIAN_POINT ( 'NONE',  ( 87.01675511858377376, 44.28642545908458317, -4.855627809373741499 ) ) ;
#11729 = DIRECTION ( 'NONE',  ( -0.8660254037844359321, -0.5000000000000051070, -0.000000000000000000 ) ) ;
#11730 = CARTESIAN_POINT ( 'NONE',  ( 161.6402223331288610, 284.6042864318112038, 1.832567169484626168 ) ) ;
#11731 = CARTESIAN_POINT ( 'NONE',  ( 164.0777181605478745, 246.4560510864015441, 5.763760713451748785 ) ) ;
#11732 = FACE_OUTER_BOUND ( 'NONE', #17928, .T. ) ;
#11733 = ORIENTED_EDGE ( 'NONE', *, *, #13718, .T. ) ;
#11734 = CARTESIAN_POINT ( 'NONE',  ( 80.35060322210587458, 57.11308289743137578, -16.23202674241575849 ) ) ;
#11735 =( BOUNDED_CURVE ( )  B_SPLINE_CURVE ( 2, ( #31620, #1248, #9345, #56437, #93480, #54413, #32640, #46317, #40725 ),
 .UNSPECIFIED., .F., .T. ) 
 B_SPLINE_CURVE_WITH_KNOTS ( ( 3, 2, 2, 2, 3 ),
 ( 0.9072580645161290036, 0.9086021505376343788, 0.9112903225806451291, 0.9139784946236558794, 0.9153225806451612545 ),
 .UNSPECIFIED. ) 
 CURVE ( )  GEOMETRIC_REPRESENTATION_ITEM ( )  RATIONAL_B_SPLINE_CURVE ( ( 0.9330127018922194093, 0.9330127018922194093, 1.000000000000000000, 0.8660254037844387076, 1.000000000000000000, 0.8660254037844387076, 1.000000000000000000, 0.9330127018922194093, 0.9330127018922194093 ) ) 
 REPRESENTATION_ITEM ( '' )  );
#11736 = CARTESIAN_POINT ( 'NONE',  ( 167.4300203585630413, 249.0882148589028304, -5.481496684248728712 ) ) ;
#11737 = CARTESIAN_POINT ( 'NONE',  ( 164.6027939175806125, 245.5465931973980105, -2.481135897876769913 ) ) ;
#11738 = DIRECTION ( 'NONE',  ( -0.000000000000000000, -0.000000000000000000, 1.000000000000000000 ) ) ;
#11739 = LINE ( 'NONE', #42603, #67264 ) ;
#11740 = B_SPLINE_CURVE_WITH_KNOTS ( 'NONE', 3,
 ( #76039, #52198, #91243, #6617, #99326, #45591, #29905, #91742, #22306, #76519, #22808, #7101, #30404, #53686, #84643, #46084, #55675, #32403, #46587, #70916, #55185, #23291, #17194, #93750, #69894, #16702, #70398, #2522, #31888, #86168, #47594, #25298, #86662, #48097, #78018, #24794, #506, #16204, #32895, #31395, #63300, #38989, #54680, #79038, #8608, #92737, #78522, #9628, #63802, #15692 ),
 .UNSPECIFIED., .F., .F.,
 ( 4, 2, 2, 2, 2, 2, 2, 2, 2, 2, 2, 2, 2, 2, 2, 2, 2, 2, 2, 2, 2, 2, 2, 2, 4 ),
 ( 0.0005200597963811503860, 0.001534264867450421416, 0.002041367402985044301, 0.002168143036868656979, 0.002294918670752269223, 0.002421694304635881468, 0.002548469938519494146, 0.002802021206286847439, 0.003055572474054200297, 0.003562675009589019639, 0.004576880080658723808, 0.005591085151728427544, 0.006098187687263286784, 0.006351738955030682143, 0.006605290222798075768, 0.006668678039739819874, 0.006732065856681563980, 0.006795453673623308086, 0.006858841490565051324, 0.007112392758331753662, 0.007619495293865116703, 0.007873046561631806897, 0.008126597829398497091, 0.008380149097165187286, 0.008633700364931875745 ),
 .UNSPECIFIED. ) ;
#11741 = PLANE ( 'NONE',  #20670 ) ;
#11742 = CARTESIAN_POINT ( 'NONE',  ( 69.07022550912036252, 70.00077902694121690, 3.705957357846692446 ) ) ;
#11743 = AXIS2_PLACEMENT_3D ( 'NONE', #44527, #83085, #61230 ) ;
#11744 = CARTESIAN_POINT ( 'NONE',  ( 157.3029956111992362, 258.1902147490555421, -18.22269824972649843 ) ) ;
#11745 = CARTESIAN_POINT ( 'NONE',  ( 174.1921478203586560, 252.1247383714452894, 3.477943671650291169 ) ) ;
#11746 = B_SPLINE_SURFACE_WITH_KNOTS ( 'NONE', 3, 1, ( 
 ( #66134, #96084 ),
 ( #58520, #89018 ),
 ( #19569, #87520 ),
 ( #11468, #18051 ),
 ( #27150, #50429 ),
 ( #26642, #35233 ),
 ( #2868, #43320 ),
 ( #74266, #57525 ),
 ( #80897, #97562 ),
 ( #34240, #11952 ),
 ( #42810, #18554 ),
 ( #73743, #42322 ),
 ( #97082, #88005 ),
 ( #4335, #73251 ),
 ( #80386, #88501 ),
 ( #19063, #41827 ),
 ( #3845, #89493 ),
 ( #20052, #50924 ),
 ( #10956, #81874 ),
 ( #49433, #12451 ),
 ( #35734, #41318 ),
 ( #66631, #72262 ),
 ( #72774, #33757 ),
 ( #95598, #3366 ),
 ( #26145, #57023 ),
 ( #21536, #53414 ),
 ( #90485, #29629 ),
 ( #98047, #99045 ),
 ( #82391, #84362 ),
 ( #21057, #37220 ),
 ( #52418, #74760 ) ),
 .UNSPECIFIED., .F., .F., .F.,
 ( 4, 3, 3, 3, 3, 3, 3, 3, 3, 3, 4 ),
 ( 2, 2 ),
 ( 0.000000000000000000, 0.1122669598086752790, 0.2243161639709619903, 0.3396355846219121233, 0.4553962076585190699, 0.5677860799922404000, 0.6749047109689705337, 0.7773884377078417174, 0.8775581155834378810, 0.9782364162378134331, 1.000000000000000000 ),
 ( 0.000000000000000000, 1.000000000000000000 ),
 .UNSPECIFIED. ) ;
#11747 = CARTESIAN_POINT ( 'NONE',  ( 22.51478983128357925, 15.12755873383625982, -6.180339887498949025 ) ) ;
#11748 = CARTESIAN_POINT ( 'NONE',  ( 190.0607312434325138, 301.4521522931182176, 3.538147641957853473 ) ) ;
#11749 = CARTESIAN_POINT ( 'NONE',  ( 154.4702041996320361, 279.2069854860779401, -1.587565366136612699 ) ) ;
#11750 = CARTESIAN_POINT ( 'NONE',  ( 169.3965326574621315, 285.1119705909437130, -8.078821750416475211 ) ) ;
#11751 = CARTESIAN_POINT ( 'NONE',  ( 198.2819808855875863, 287.2125302111982705, 18.53535247371401695 ) ) ;
#11752 = CARTESIAN_POINT ( 'NONE',  ( 157.4281126377775593, 271.2014885723156112, -14.63201430359713662 ) ) ;
#11753 = CARTESIAN_POINT ( 'NONE',  ( 125.1447535615808988, 256.3927522451419918, 2.944929066748280225E-16 ) ) ;
#11754 = B_SPLINE_CURVE_WITH_KNOTS ( 'NONE', 3,
 ( #79341, #34682, #65584, #96040 ),
 .UNSPECIFIED., .F., .F.,
 ( 4, 4 ),
 ( 0.0004588294438088373985, 0.008388525337162593826 ),
 .UNSPECIFIED. ) ;
#11755 = CARTESIAN_POINT ( 'NONE',  ( 25.95703985525452850, 15.39040679176983240, 1.333680081654574804E-15 ) ) ;
#11756 = ORIENTED_EDGE ( 'NONE', *, *, #76601, .T. ) ;
#11758 = CARTESIAN_POINT ( 'NONE',  ( 196.3720681610792553, 290.5205960880691691, 16.18360420724715354 ) ) ;
#11757 = VECTOR ( 'NONE', #65529, 1000.000000000000000 ) ;
#11759 = CARTESIAN_POINT ( 'NONE',  ( 148.3837145175834280, 273.6388627701866767, 8.841971351370922605 ) ) ;
#11760 = CARTESIAN_POINT ( 'NONE',  ( -0.5279885150232012103, 164.3768266524160140, -9.188101187500093303 ) ) ;
#11761 = EDGE_CURVE ( 'NONE', #48169, #49525, #24485, .T. ) ;
#11762 = CARTESIAN_POINT ( 'NONE',  ( 47.23881193640350062, 188.8923013555410080, 4.594050593750050204 ) ) ;
#11763 = CARTESIAN_POINT ( 'NONE',  ( 177.2703692633946844, 258.2913615668659304, -10.36463420540507308 ) ) ;
#11764 = CARTESIAN_POINT ( 'NONE',  ( 13.93250452138409479, 29.81751292744056059, -6.180339887498951690 ) ) ;
#11765 = DIRECTION ( 'NONE',  ( -0.8660254037844387076, -0.4999999999999998890, -0.000000000000000000 ) ) ;
#11766 = CARTESIAN_POINT ( 'NONE',  ( 157.1458804504438831, 258.4623461901232417, -17.08829597948888335 ) ) ;
#11767 = CARTESIAN_POINT ( 'NONE',  ( 189.2157573186698016, 290.5516144355429446, -14.57334616014404460 ) ) ;
#11768 = CARTESIAN_POINT ( 'NONE',  ( 146.8201187048455267, 276.3470901603510015, 4.112223577763169047 ) ) ;
#11769 = CARTESIAN_POINT ( 'NONE',  ( 74.14735107364549549, 55.49514332839016362, -16.11765820591672949 ) ) ;
#11771 = CARTESIAN_POINT ( 'NONE',  ( 79.17323837735700920, 206.5177522451417929, 5.000000000000051514 ) ) ;
#11770 = CARTESIAN_POINT ( 'NONE',  ( 169.7431851515004837, 257.7669204232371385, 13.75914435124215274 ) ) ;
#11772 = CARTESIAN_POINT ( 'NONE',  ( 76.76222887016557195, 59.42175249350923849, 16.38682359597675742 ) ) ;
#11773 = CARTESIAN_POINT ( 'NONE',  ( 157.1539462478114615, 258.4483758192793061, -17.96006278656275867 ) ) ;
#11774 = CARTESIAN_POINT ( 'NONE',  ( 91.91334042722833431, 212.3262482093457777, 3.021315404115420679E-15 ) ) ;
#11775 = ADVANCED_FACE ( 'NONE', ( #85333 ), #25100, .T. ) ;
#11776 = EDGE_CURVE ( 'NONE', #82130, #37468, #37438, .T. ) ;
#11777 = CARTESIAN_POINT ( 'NONE',  ( 43.32339510341159894, 182.4865022471901455, 1.119607411625061291E-15 ) ) ;
#11778 = DIRECTION ( 'NONE',  ( -0.9659258262890627611, 0.2588190451025410010, -1.722766911950497786E-15 ) ) ;
#11779 = CARTESIAN_POINT ( 'NONE',  ( 168.6156890688689884, 286.4116463664167895, -8.226575548882113509 ) ) ;
#11780 = EDGE_CURVE ( 'NONE', #71872, #5333, #92243, .T. ) ;
#11781 = CARTESIAN_POINT ( 'NONE',  ( 3.882894515797516988, 182.2369531367911009, -4.594050593750048428 ) ) ;
#11782 = CARTESIAN_POINT ( 'NONE',  ( 167.8073358443718064, 286.0487684481980182, 4.087165526909992685 ) ) ;
#11783 = B_SPLINE_CURVE_WITH_KNOTS ( 'NONE', 3,
 ( #29684, #13989, #44866, #91514, #53465, #45851, #99100, #53954, #92510, #23056, #273, #22080, #92032, #99592, #37277, #30175, #68173, #54445, #85422, #61062, #22578, #84415, #52977, #56470, #78790, #63570, #25067, #71196, #33691, #2296, #41256, #63071, #55944, #48886, #25584, #1283, #70668, #94014, #95021, #64585, #87946, #95537, #9378, #56959, #62550, #47364, #16468, #94513, #72198, #79327, #40256, #18490, #24566, #766 ),
 .UNSPECIFIED., .F., .F.,
 ( 4, 2, 2, 2, 2, 2, 2, 2, 2, 2, 2, 2, 2, 2, 2, 2, 2, 2, 2, 2, 2, 2, 2, 2, 2, 2, 4 ),
 ( 0.0006528422629810665513, 0.0008645749101140807850, 0.001076307557247095127, 0.001182173880813599479, 0.001288040204380103615, 0.001393906527946607750, 0.001499772851513112102, 0.001711505498646120373, 0.001923238145779129077, 0.002346703440045146052, 0.003193634028577111480, 0.004040564617109077342, 0.004887495205641041902, 0.005310960499907025484, 0.005522693147040058474, 0.005628559470606574536, 0.005681492632389832133, 0.005734425794173090597, 0.005787358955956349062, 0.005840292117739606659, 0.005946158441306171293, 0.006157891088439202548, 0.006369623735572234671, 0.006581356382705265927, 0.007004821676971320632, 0.007216554324104351888, 0.007428286971237384011 ),
 .UNSPECIFIED. ) ;
#11784 = CARTESIAN_POINT ( 'NONE',  ( 80.60685564337630638, 57.64637852931380024, -16.24314337822399779 ) ) ;
#11785 = ADVANCED_FACE ( 'NONE', ( #95940 ), #79363, .F. ) ;
#11786 = CARTESIAN_POINT ( 'NONE',  ( 153.4477557824949940, 264.8676860077344486, 17.16010094972647693 ) ) ;
#11787 = CARTESIAN_POINT ( 'NONE',  ( 34.84050961144773595, 32.06628583063844218, -9.188101187500006262 ) ) ;
#11788 = CARTESIAN_POINT ( 'NONE',  ( 83.66574516303668929, 209.1115022471902023, -5.000000000000041744 ) ) ;
#11789 = CARTESIAN_POINT ( 'NONE',  ( 179.3259839114000158, 277.6273404258797086, 17.12033975729926638 ) ) ;
#11790 = CARTESIAN_POINT ( 'NONE',  ( 154.9455285025717615, 262.2734675583710100, 18.28470720339922551 ) ) ;
#11791 = B_SPLINE_CURVE_WITH_KNOTS ( 'NONE', 3,
 ( #53418, #69619, #14915, #38713, #45804, #61999, #76728, #85895, #84367, #38200 ),
 .UNSPECIFIED., .F., .F.,
 ( 4, 3, 3, 4 ),
 ( 0.0005899778860174007163, 0.001498044977030944455, 0.004494154408253303763, 0.005834865480722558825 ),
 .UNSPECIFIED. ) ;
#11792 = CARTESIAN_POINT ( 'NONE',  ( 38.71056063283548809, 34.30066082961425167, -10.00000000000000533 ) ) ;
#11793 = B_SPLINE_CURVE_WITH_KNOTS ( 'NONE', 3,
 ( #97040, #74718, #28085, #42768 ),
 .UNSPECIFIED., .F., .F.,
 ( 4, 4 ),
 ( 0.008066038982947665303, 0.01417919469606437194 ),
 .UNSPECIFIED. ) ;
#11794 = CARTESIAN_POINT ( 'NONE',  ( 179.4170627276716345, 262.5904822696095380, -12.85500290294408288 ) ) ;
#11795 = CARTESIAN_POINT ( 'NONE',  ( 9.941082954516854642, 14.24335787977761036, -9.188101187500008038 ) ) ;
#11796 = CARTESIAN_POINT ( 'NONE',  ( 71.78242053751056062, 72.53632993589366151, 0.9980050652678106315 ) ) ;
#11797 = CARTESIAN_POINT ( 'NONE',  ( 19.96532700332172183, 20.03085787977762422, 9.188101187500006262 ) ) ;
#11798 = CARTESIAN_POINT ( 'NONE',  ( 159.1349094508772737, 259.4340307094828404, 16.68893039409465828 ) ) ;
#11799 = CARTESIAN_POINT ( 'NONE',  ( 154.8989000222956349, 262.3542304552891551, 17.41779271305265908 ) ) ;
#11800 = ORIENTED_EDGE ( 'NONE', *, *, #39155, .F. ) ;
#11801 = CARTESIAN_POINT ( 'NONE',  ( 154.9380580364485525, 275.5880567444434064, 10.35765824813548619 ) ) ;
#11802 = CARTESIAN_POINT ( 'NONE',  ( 159.9770824720811220, 253.5585604421560788, -16.42166711341322483 ) ) ;
#11803 = ORIENTED_EDGE ( 'NONE', *, *, #65619, .F. ) ;
#11804 = CARTESIAN_POINT ( 'NONE',  ( 192.2185419806677942, 297.7147144631093170, 12.45868041609393728 ) ) ;
#11805 = CARTESIAN_POINT ( 'NONE',  ( 207.3062152119541679, 271.5820978585240368, 7.879821064966149535 ) ) ;
#11806 = CARTESIAN_POINT ( 'NONE',  ( 181.4791476608088487, 255.0645862387702039, -1.457838961102627895 ) ) ;
#11807 = CARTESIAN_POINT ( 'NONE',  ( 87.77058453035330388, 45.11289234403164983, 6.766180878992238412 ) ) ;
#11808 = ORIENTED_EDGE ( 'NONE', *, *, #45491, .F. ) ;
#11809 = ORIENTED_EDGE ( 'NONE', *, *, #45398, .T. ) ;
#11811 = CARTESIAN_POINT ( 'NONE',  ( 204.5133713884061706, 276.4194452585140311, 14.87364779308245843 ) ) ;
#11810 = CARTESIAN_POINT ( 'NONE',  ( 159.6784519327069063, 278.7635212910759606, -9.544083088951406779 ) ) ;
#11812 = CARTESIAN_POINT ( 'NONE',  ( 152.6945189806187955, 266.1723304187151484, 16.62409282110771613 ) ) ;
#11813 = VERTEX_POINT ( 'NONE', #77586 ) ;
#11814 = DIRECTION ( 'NONE',  ( -0.2473641778533917646, -0.9689225787001330970, 0.000000000000000000 ) ) ;
#11815 = CARTESIAN_POINT ( 'NONE',  ( 175.8349158976987212, 262.9913934397512207, 14.38086816053275108 ) ) ;
#11816 = ORIENTED_EDGE ( 'NONE', *, *, #31520, .F. ) ;
#11817 = CARTESIAN_POINT ( 'NONE',  ( 37.75683693788968753, 23.92755873383628895, 6.180339887498953466 ) ) ;
#11818 = CARTESIAN_POINT ( 'NONE',  ( 76.43878283397967266, 226.4860189848784842, -2.679491924311252493 ) ) ;
#11819 = CIRCLE ( 'NONE', #68405, 70.00000000000001421 ) ;
#11820 = CARTESIAN_POINT ( 'NONE',  ( 81.29242433156768755, 43.25429275065669543, 9.620330362255517187 ) ) ;
#11821 = EDGE_LOOP ( 'NONE', ( #39278, #9037, #8808, #19989, #96576, #43587, #74254, #52410, #26033, #19655, #96496, #91414 ) ) ;
#11822 = CARTESIAN_POINT ( 'NONE',  ( 161.8289209813647176, 250.3510820566641257, 13.28523796267037937 ) ) ;
#11823 = FACE_OUTER_BOUND ( 'NONE', #47046, .T. ) ;
#11824 = FACE_OUTER_BOUND ( 'NONE', #16930, .T. ) ;
#11825 = ORIENTED_EDGE ( 'NONE', *, *, #95333, .F. ) ;
#11826 = CARTESIAN_POINT ( 'NONE',  ( 174.4652129899553472, 277.2261295425576577, -15.64854957247286471 ) ) ;
#11827 = CARTESIAN_POINT ( 'NONE',  ( 201.5074933251657399, 279.6257787853921286, 16.58790246189369100 ) ) ;
#11828 = VECTOR ( 'NONE', #46656, 1000.000000000000000 ) ;
#11829 = ORIENTED_EDGE ( 'NONE', *, *, #91560, .F. ) ;
#11830 = CARTESIAN_POINT ( 'NONE',  ( 156.8551930071947140, 266.3782999250777266, -16.34332614469098743 ) ) ;
#11831 = VERTEX_POINT ( 'NONE', #84707 ) ;
#11832 = CARTESIAN_POINT ( 'NONE',  ( 32.07560492619583670, 120.7590592525220075, 59.99999999999999289 ) ) ;
#11833 = VERTEX_POINT ( 'NONE', #31453 ) ;
#11834 = CARTESIAN_POINT ( 'NONE',  ( 82.93017357788673394, 175.3855496052738374, 21.50000000000000000 ) ) ;
#11835 = CARTESIAN_POINT ( 'NONE',  ( 82.99898243690306288, 53.45938235784409898, 15.65150354709845004 ) ) ;
#11836 = CARTESIAN_POINT ( 'NONE',  ( 19.05068821614582575, 13.12755873383625271, -6.180339887498949025 ) ) ;
#11837 = CARTESIAN_POINT ( 'NONE',  ( -0.06004842451780637025, 38.53370552223154988, 59.99999999999999289 ) ) ;
#11838 = CARTESIAN_POINT ( 'NONE',  ( 177.8017954917369252, 291.1815355444027205, 6.079021535780970709 ) ) ;
#11839 = CARTESIAN_POINT ( 'NONE',  ( 191.1192699377806719, 299.6187094927299199, -9.526914969203620132 ) ) ;
#11840 = AXIS2_PLACEMENT_3D ( 'NONE', #82972, #84465, #44910 ) ;
#11841 = ORIENTED_EDGE ( 'NONE', *, *, #42360, .F. ) ;
#11842 = LINE ( 'NONE', #48331, #7574 ) ;
#11843 = CARTESIAN_POINT ( 'NONE',  ( 27.77157046966360809, 18.96004757982091249, -5.678558825948276656 ) ) ;
#11844 = EDGE_CURVE ( 'NONE', #51674, #29855, #54747, .T. ) ;
#11845 = CARTESIAN_POINT ( 'NONE',  ( 22.66956910419568061, 38.88013629349136835, -10.00000000000000000 ) ) ;
#11846 = CARTESIAN_POINT ( 'NONE',  ( 206.3106310032756596, 273.3065002911688453, 10.17860425536756175 ) ) ;
#11847 = CARTESIAN_POINT ( 'NONE',  ( 198.5558597050348908, 286.7381581807989051, 17.16554469393394200 ) ) ;
#11848 = EDGE_LOOP ( 'NONE', ( #26565, #14154, #682, #65055 ) ) ;
#11849 = CARTESIAN_POINT ( 'NONE',  ( 187.5205457192285223, 277.0860194500085640, 16.99091369793140061 ) ) ;
#11850 = LINE ( 'NONE', #73640, #99872 ) ;
#11851 = CARTESIAN_POINT ( 'NONE',  ( 198.7408816115379864, 285.9624092822338071, -17.04496721243561197 ) ) ;
#11852 = CARTESIAN_POINT ( 'NONE',  ( 177.9661674680945112, 277.1853473926717015, -17.54411374166730297 ) ) ;
#11853 = EDGE_CURVE ( 'NONE', #92061, #14896, #73751, .T. ) ;
#11854 = CARTESIAN_POINT ( 'NONE',  ( 160.5165517222688436, 252.6241722917100390, -14.79882802290810595 ) ) ;
#11855 = CARTESIAN_POINT ( 'NONE',  ( 148.7168577282835713, 273.0618418030571206, -9.544069619348908518 ) ) ;
#11856 = ORIENTED_EDGE ( 'NONE', *, *, #73160, .T. ) ;
#11857 = CARTESIAN_POINT ( 'NONE',  ( 167.2812095546786679, 252.8454341180955680, -12.28570835557802177 ) ) ;
#11858 = CARTESIAN_POINT ( 'NONE',  ( 82.85336985908988083, 152.2760637034261890, 0.000000000000000000 ) ) ;
#11859 = CARTESIAN_POINT ( 'NONE',  ( 124.2065593741477301, 252.5177522451419350, 5.000000000000046185 ) ) ;
#11861 = EDGE_CURVE ( 'NONE', #1989, #34033, #86225, .T. ) ;
#11860 = CARTESIAN_POINT ( 'NONE',  ( 164.2672861321391053, 246.1277097281173667, -2.417001679502223777 ) ) ;
#11862 = CARTESIAN_POINT ( 'NONE',  ( 30.24280306353613312, 198.2677522451419350, -5.000000000000047962 ) ) ;
#11863 = CARTESIAN_POINT ( 'NONE',  ( 110.3232631693849441, 228.3768266524160140, 9.188101187500096856 ) ) ;
#11864 = CARTESIAN_POINT ( 'NONE',  ( 183.5927363050826955, 297.0638526922078313, -2.830836570955955978 ) ) ;
#11865 = CARTESIAN_POINT ( 'NONE',  ( 167.3110030245129281, 283.1034262774602439, -11.14282353764315303 ) ) ;
#11866 = CARTESIAN_POINT ( 'NONE',  ( 84.74456076088121392, 50.48706963223701649, 13.54072923514545757 ) ) ;
#11867 = CARTESIAN_POINT ( 'NONE',  ( 162.7894281526998839, 248.6874348348773651, 10.21811719309735622 ) ) ;
#11868 = CARTESIAN_POINT ( 'NONE',  ( 25.07406103223676652, 173.0327760586659451, 1.948934522072303157E-15 ) ) ;
#11869 = LINE ( 'NONE', #88928, #23628 ) ;
#11870 = ORIENTED_EDGE ( 'NONE', *, *, #35158, .T. ) ;
#11872 = ORIENTED_EDGE ( 'NONE', *, *, #61273, .F. ) ;
#11871 = B_SPLINE_CURVE_WITH_KNOTS ( 'NONE', 3,
 ( #97313, #73498, #67373, #74510 ),
 .UNSPECIFIED., .F., .F.,
 ( 4, 4 ),
 ( 0.005351796179668294809, 0.01338782376300005385 ),
 .UNSPECIFIED. ) ;
#11873 = CARTESIAN_POINT ( 'NONE',  ( 74.32474745866193189, 68.52230083288840490, 11.65590001247776364 ) ) ;
#11874 = CARTESIAN_POINT ( 'NONE',  ( 185.3920610038572647, 259.4640903649777783, -5.312017440010943226 ) ) ;
#11875 = DIRECTION ( 'NONE',  ( 0.1473778574936323582, 0.9890802632347824863, 0.000000000000000000 ) ) ;
#11876 = CARTESIAN_POINT ( 'NONE',  ( 190.6954410837624607, 300.3528026016029457, -5.728531842148099962 ) ) ;
#11877 = CARTESIAN_POINT ( 'NONE',  ( 193.0090100919386202, 263.8705414732962709, -4.314308890231003168 ) ) ;
#11878 = CARTESIAN_POINT ( 'NONE',  ( 161.0974665087481981, 251.6179983666593216, -13.69252715295363210 ) ) ;
#11879 = CARTESIAN_POINT ( 'NONE',  ( 185.8273812090706940, 286.4779426780396534, 15.58107062954017330 ) ) ;
#11880 = PLANE ( 'NONE',  #54755 ) ;
#11881 = CARTESIAN_POINT ( 'NONE',  ( 39.95835201613431309, 200.0024278399160949, 9.188101187500095079 ) ) ;
#11882 = CARTESIAN_POINT ( 'NONE',  ( 106.8138825148103450, 219.1427522451417644, 1.119607411625061291E-15 ) ) ;
#11883 = ORIENTED_EDGE ( 'NONE', *, *, #29502, .F. ) ;
#11884 = CARTESIAN_POINT ( 'NONE',  ( 79.13444159074371953, 60.15296345131729083, -16.46386276767551848 ) ) ;
#11885 = CARTESIAN_POINT ( 'NONE',  ( 179.1927739452798676, 258.3510491419078221, -10.08736568086201579 ) ) ;
#11886 = AXIS2_PLACEMENT_3D ( 'NONE', #16496, #30708, #85451 ) ;
#11887 = CARTESIAN_POINT ( 'NONE',  ( -4.696256414383327638, 180.3464784336661637, 1.353441290958777327E-15 ) ) ;
#11888 = CARTESIAN_POINT ( 'NONE',  ( 68.79203164621388567, 64.70631446037705814, -12.17797522407645516 ) ) ;
#11889 = CARTESIAN_POINT ( 'NONE',  ( 198.4344074287054696, 286.9485196940960918, -17.83642855442570152 ) ) ;
#11890 = DIRECTION ( 'NONE',  ( -0.8660254037844387076, -0.4999999999999998890, -0.000000000000000000 ) ) ;
#11891 = CARTESIAN_POINT ( 'NONE',  ( 192.5284579606305613, 297.1779242397361713, -13.15228012403107272 ) ) ;
#11892 = VECTOR ( 'NONE', #75559, 1000.000000000000114 ) ;
#11893 = CARTESIAN_POINT ( 'NONE',  ( 193.2494886543572363, 263.9923760144491780, 7.744585581713212541 ) ) ;
#11894 = CARTESIAN_POINT ( 'NONE',  ( 203.7436594101163507, 276.0772935449583656, 13.22569794353039363 ) ) ;
#11895 = CARTESIAN_POINT ( 'NONE',  ( 68.82480163077127600, 67.66752897612431639, 8.343174400127590928 ) ) ;
#11896 = CARTESIAN_POINT ( 'NONE',  ( 207.5686001603237116, 271.1276337968068333, 7.659944433763431704 ) ) ;
#11897 = ORIENTED_EDGE ( 'NONE', *, *, #47156, .T. ) ;
#11898 = CARTESIAN_POINT ( 'NONE',  ( 0.5273063997305784678, 161.1115022471902023, -5.000000000000041744 ) ) ;
#11899 = DIRECTION ( 'NONE',  ( 0.000000000000000000, 0.000000000000000000, 1.000000000000000000 ) ) ;
#11900 = VECTOR ( 'NONE', #9654, 1000.000000000000227 ) ;
#11901 = CARTESIAN_POINT ( 'NONE',  ( 120.4987145680870952, 246.5024278399160949, 9.188101187500095079 ) ) ;
#11902 = EDGE_CURVE ( 'NONE', #2005, #89249, #12213, .T. ) ;
#11903 = CARTESIAN_POINT ( 'NONE',  ( 17.68238808236222326, 31.18502408145591787, 5.678558825948277544 ) ) ;
#11904 = FACE_OUTER_BOUND ( 'NONE', #75285, .T. ) ;
#11905 = EDGE_CURVE ( 'NONE', #53889, #22875, #43592, .T. ) ;
#11906 = FACE_OUTER_BOUND ( 'NONE', #9216, .T. ) ;
#11907 = AXIS2_PLACEMENT_3D ( 'NONE', #72242, #95582, #27132 ) ;
#11909 = CARTESIAN_POINT ( 'NONE',  ( 74.89568429962641005, 67.14399892254596125, 12.98700472788359228 ) ) ;
#11908 = CARTESIAN_POINT ( 'NONE',  ( 82.04105866126801061, 41.84617809604260685, -5.590206233676478398 ) ) ;
#11910 = CARTESIAN_POINT ( 'NONE',  ( 190.6083555345403795, 300.5036391974608136, -6.894354067666211172 ) ) ;
#11911 = EDGE_LOOP ( 'NONE', ( #88743, #69038, #82164, #90521, #89357 ) ) ;
#11912 = CARTESIAN_POINT ( 'NONE',  ( 76.55433408466377898, 148.6393137034262111, 8.907468493598274475E-16 ) ) ;
#11913 = CARTESIAN_POINT ( 'NONE',  ( 163.3351346677209506, 247.7422434248393586, 8.151360907120263732 ) ) ;
#11914 = CARTESIAN_POINT ( 'NONE',  ( 195.4436462626574667, 265.1414692012189676, -7.795071168451356058 ) ) ;
#11915 = CARTESIAN_POINT ( 'NONE',  ( 173.0073966428915071, 268.1627966282908915, -16.30112163756558630 ) ) ;
#11916 = CARTESIAN_POINT ( 'NONE',  ( 81.59284463765364137, 55.17094835597973912, -15.91583639150689855 ) ) ;
#11917 = ORIENTED_EDGE ( 'NONE', *, *, #63440, .T. ) ;
#11918 = CARTESIAN_POINT ( 'NONE',  ( -27.42236680055714260, 166.5217562850347406, 1.224646799147364892E-15 ) ) ;
#11919 = CARTESIAN_POINT ( 'NONE',  ( 167.3709722853970163, 270.8926238990931665, -16.36061349221664329 ) ) ;
#11920 = CARTESIAN_POINT ( 'NONE',  ( 86.46048006423905008, 47.32182001325401188, 10.26516935212321968 ) ) ;
#11921 = CARTESIAN_POINT ( 'NONE',  ( 80.37872757669391888, 55.97141553226800426, 16.09280928407363831 ) ) ;
#11922 = CARTESIAN_POINT ( 'NONE',  ( 185.8931680259638028, 296.6947360474555921, 4.853906208423047985 ) ) ;
#11923 = CARTESIAN_POINT ( 'NONE',  ( 72.09555114463066161, 71.52603334931079360, -5.842164467371243397 ) ) ;
#11924 = CYLINDRICAL_SURFACE ( 'NONE', #71082, 17.82106496071139645 ) ;
#11925 = VERTEX_POINT ( 'NONE', #64366 ) ;
#11926 = CARTESIAN_POINT ( 'NONE',  ( 194.5078867822585664, 282.9899840733189080, 17.68867816471975019 ) ) ;
#11927 = CARTESIAN_POINT ( 'NONE',  ( 4.135592144620554578, 24.16126292948893450, -6.180339887498951690 ) ) ;
#11928 = CARTESIAN_POINT ( 'NONE',  ( 173.9683356937793519, 272.2847035684981734, -17.69864048336468088 ) ) ;
#11929 = VERTEX_POINT ( 'NONE', #18779 ) ;
#11930 = PLANE ( 'NONE',  #43280 ) ;
#11931 = CARTESIAN_POINT ( 'NONE',  ( 194.3541845315608612, 294.0156730581561533, -14.67567721756631016 ) ) ;
#11932 = DIRECTION ( 'NONE',  ( -0.000000000000000000, -0.000000000000000000, 1.000000000000000000 ) ) ;
#11933 = ORIENTED_EDGE ( 'NONE', *, *, #28143, .T. ) ;
#11934 = CARTESIAN_POINT ( 'NONE',  ( 79.40659458863603959, 59.69041580281565018, 16.52608132308844091 ) ) ;
#11935 = FACE_OUTER_BOUND ( 'NONE', #53012, .T. ) ;
#11936 = PLANE ( 'NONE',  #64222 ) ;
#11937 = CARTESIAN_POINT ( 'NONE',  ( 75.30072407401860346, 53.34595582841677697, 16.02892702632065891 ) ) ;
#11938 = ORIENTED_EDGE ( 'NONE', *, *, #53502, .F. ) ;
#11939 = CARTESIAN_POINT ( 'NONE',  ( 86.99453030705913648, 221.0333772461660544, 9.188101187500095079 ) ) ;
#11940 = CARTESIAN_POINT ( 'NONE',  ( 80.23640585404207570, 51.30364936960656763, -15.02180247759152643 ) ) ;
#11941 = CARTESIAN_POINT ( 'NONE',  ( 184.6889223697928912, 259.7167601846132925, -5.813120004385227801 ) ) ;
#11942 = ORIENTED_EDGE ( 'NONE', *, *, #235, .F. ) ;
#11943 = VERTEX_POINT ( 'NONE', #94802 ) ;
#11944 = CARTESIAN_POINT ( 'NONE',  ( 88.23407674691928548, 43.71813397101750098, 0.1961470715255514696 ) ) ;
#11945 = ORIENTED_EDGE ( 'NONE', *, *, #42377, .T. ) ;
#11946 = CARTESIAN_POINT ( 'NONE',  ( 77.55626133878482165, 49.73613333205595666, 14.95107568548285037 ) ) ;
#11947 = VERTEX_POINT ( 'NONE', #88726 ) ;
#11948 = CARTESIAN_POINT ( 'NONE',  ( 75.90866741198675527, 63.34674660074826846, 14.83779576734563044 ) ) ;
#11949 = CARTESIAN_POINT ( 'NONE',  ( 155.4810912439522212, 261.3458456796594760, -18.44218279064527266 ) ) ;
#11950 = ORIENTED_EDGE ( 'NONE', *, *, #26764, .F. ) ;
#11951 = CARTESIAN_POINT ( 'NONE',  ( 187.1789365411204926, 291.3781964708418286, -14.15416893886036220 ) ) ;
#11952 = CARTESIAN_POINT ( 'NONE',  ( 81.92915189185293912, 41.06609442470161042, 3.489617835449585037 ) ) ;
#11953 = CARTESIAN_POINT ( 'NONE',  ( 189.9197469165544874, 301.6963443103418854, 2.546707301993238026 ) ) ;
#11954 = CARTESIAN_POINT ( 'NONE',  ( 159.7566137705401843, 275.6830047768774534, -12.53866916850027025 ) ) ;
#11955 = CARTESIAN_POINT ( 'NONE',  ( 200.8147387322574957, 282.8256649374973790, -18.02438097732020239 ) ) ;
#11956 = CARTESIAN_POINT ( 'NONE',  ( 165.5093369583051128, 275.0219039653110258, -16.16693748275729803 ) ) ;
#11957 = CARTESIAN_POINT ( 'NONE',  ( 141.5001777056247931, 246.3768266524160140, 9.188101187500098632 ) ) ;
#11958 = CARTESIAN_POINT ( 'NONE',  ( 70.81316579118700361, 61.41551742078693366, -14.85192641767512889 ) ) ;
#11959 = CARTESIAN_POINT ( 'NONE',  ( 5.869580825389008716, 26.49540643055185996, 3.479690158560446702E-15 ) ) ;
#11960 = VERTEX_POINT ( 'NONE', #17780 ) ;
#11961 = AXIS2_PLACEMENT_3D ( 'NONE', #8154, #55226, #70446 ) ;
#11962 = EDGE_CURVE ( 'NONE', #94878, #97533, #57750, .T. ) ;
#11964 = ORIENTED_EDGE ( 'NONE', *, *, #75812, .F. ) ;
#11963 = DIRECTION ( 'NONE',  ( -0.000000000000000000, -0.000000000000000000, -1.000000000000000000 ) ) ;
#11965 = CARTESIAN_POINT ( 'NONE',  ( 156.6812872898450735, 261.2670451491295012, 0.000000000000000000 ) ) ;
#11966 = ADVANCED_FACE ( 'NONE', ( #10178 ), #41045, .T. ) ;
#11967 = CARTESIAN_POINT ( 'NONE',  ( 76.14996942406402525, 65.34647919798338478, -14.05451472204274310 ) ) ;
#11968 = CARTESIAN_POINT ( 'NONE',  ( 156.7598395624803231, 279.4774680247458605, 7.438909857426141414 ) ) ;
#11969 = CARTESIAN_POINT ( 'NONE',  ( 165.5287065161056717, 246.9177196700316870, -2.014791919525022568 ) ) ;
#11970 = CARTESIAN_POINT ( 'NONE',  ( 172.4473134597787976, 280.4758190227907448, 13.90356073592574049 ) ) ;
#11971 = CARTESIAN_POINT ( 'NONE',  ( 168.1310046488833905, 252.8833719797225967, 11.91735455981645764 ) ) ;
#11972 = CARTESIAN_POINT ( 'NONE',  ( 88.16692178265705593, 43.83444978110026824, -2.116868534317887462 ) ) ;
#11973 = EDGE_LOOP ( 'NONE', ( #9965, #79740, #16505, #32960, #95386 ) ) ;
#11974 = CARTESIAN_POINT ( 'NONE',  ( 185.0366554279405022, 273.1381174272470957, -16.61285403035061137 ) ) ;
#11975 = CARTESIAN_POINT ( 'NONE',  ( 66.44900687915006188, 68.94146508460354994, 0.02989588888337583669 ) ) ;
#11976 = ORIENTED_EDGE ( 'NONE', *, *, #53472, .T. ) ;
#11977 = B_SPLINE_CURVE_WITH_KNOTS ( 'NONE', 3,
 ( #84577, #15115, #78454, #62214 ),
 .UNSPECIFIED., .F., .F.,
 ( 4, 4 ),
 ( 0.02596114015397115241, 0.03520195514588816271 ),
 .UNSPECIFIED. ) ;
#11979 = EDGE_CURVE ( 'NONE', #75787, #50887, #3212, .T. ) ;
#11978 = DIRECTION ( 'NONE',  ( -0.000000000000000000, -0.000000000000000000, 1.000000000000000000 ) ) ;
#11980 = VECTOR ( 'NONE', #24118, 1000.000000000000227 ) ;
#11981 = CARTESIAN_POINT ( 'NONE',  ( 200.9434809886455469, 267.7932726406668849, -2.812590155380607637 ) ) ;
#11982 = CARTESIAN_POINT ( 'NONE',  ( 78.44203751522360335, 61.21016990572091032, 16.24725970467587999 ) ) ;
#11983 = CARTESIAN_POINT ( 'NONE',  ( 198.4097421844162170, 265.0824675037606539, -3.039349057205883664 ) ) ;
#11984 = CARTESIAN_POINT ( 'NONE',  ( 164.6405626616606526, 274.4174134527740989, 16.14945534314108144 ) ) ;
#11986 = CARTESIAN_POINT ( 'NONE',  ( 88.18856786306730555, 43.91052089632134425, 2.508363019901196367 ) ) ;
#11985 = CARTESIAN_POINT ( 'NONE',  ( 161.3190595899150139, 281.5918341196443748, -7.463758623216700805 ) ) ;
#11987 = CARTESIAN_POINT ( 'NONE',  ( 203.8395512996133334, 269.2639942102448458, 5.522558735337302238 ) ) ;
#11988 = EDGE_LOOP ( 'NONE', ( #69968, #41676, #63994, #75461 ) ) ;
#11989 = PRODUCT_DEFINITION_SHAPE ( 'NONE', 'NONE',  #32837 ) ;
#11990 = CARTESIAN_POINT ( 'NONE',  ( 75.82478874696548132, 61.23931674123156199, -15.47528407149140861 ) ) ;
#11991 = CARTESIAN_POINT ( 'NONE',  ( 189.8329410786966491, 274.2658440874778876, -15.65430098090321565 ) ) ;
#11992 = CARTESIAN_POINT ( 'NONE',  ( -67.91103796225580425, 44.10201266000169795, -10.00000000000000000 ) ) ;
#11993 = EDGE_CURVE ( 'NONE', #84833, #79042, #48166, .T. ) ;
#11994 = CARTESIAN_POINT ( 'NONE',  ( 172.4827362167600029, 289.4993777119672700, 2.605925812672743813 ) ) ;
#11995 = FACE_OUTER_BOUND ( 'NONE', #69506, .T. ) ;
#11996 = CARTESIAN_POINT ( 'NONE',  ( 80.64679548305885248, 43.26720623737277549, -9.272004999721030316 ) ) ;
#11997 = DIRECTION ( 'NONE',  ( 1.000000000000000000, -1.153838929164001651E-13, 0.000000000000000000 ) ) ;
#11998 = CARTESIAN_POINT ( 'NONE',  ( 4.640666744108908226, 182.6744531367911577, 4.594050593750047540 ) ) ;
#11999 = CARTESIAN_POINT ( 'NONE',  ( 110.3232631693849726, 228.3768266524160140, 9.188101187500098632 ) ) ;
#12000 = CARTESIAN_POINT ( 'NONE',  ( 87.77744914111154628, 44.40955816724378025, -3.958690154376787174 ) ) ;
#12001 = CARTESIAN_POINT ( 'NONE',  ( 181.5558742819051474, 255.2544784655372894, -2.503599602330015994 ) ) ;
#12002 = CARTESIAN_POINT ( 'NONE',  ( 197.9901163037401943, 272.1418500761980681, -13.83221381771805625 ) ) ;
#12003 = DIRECTION ( 'NONE',  ( 0.4999999999999992784, -0.8660254037844390407, 0.000000000000000000 ) ) ;
#12004 = B_SPLINE_CURVE_WITH_KNOTS ( 'NONE', 3,
 ( #28120, #81377, #4845, #81865, #44308, #58994, #51420, #82382, #5820, #36709, #67616, #98544, #11944, #50242, #65444, #56337, #42138, #58334, #64453, #89310, #73070, #72580 ),
 .UNSPECIFIED., .F., .F.,
 ( 4, 3, 3, 3, 3, 3, 3, 4 ),
 ( 0.4976065956401893864, 0.5844252810809384968, 0.6686540514502724575, 0.7354980260655605839, 0.8028463152565796790, 0.8633854507757419139, 0.9437142632667596676, 1.000000000000000000 ),
 .UNSPECIFIED. ) ;
#12005 = CARTESIAN_POINT ( 'NONE',  ( 164.0383833005010956, 283.8578478928177447, 5.735541721561834727 ) ) ;
#12006 = CARTESIAN_POINT ( 'NONE',  ( 194.5252985417586729, 293.7192948986070178, -14.54632727629426370 ) ) ;
#12007 = ADVANCED_FACE ( 'NONE', ( #63863 ), #80613, .F. ) ;
#12008 = CARTESIAN_POINT ( 'NONE',  ( 84.74507488503365948, 50.24295689512916141, 13.81875560728438224 ) ) ;
#12010 = CARTESIAN_POINT ( 'NONE',  ( 195.4436462626574667, 265.1414692012189676, -7.795071168451356058 ) ) ;
#12009 = B_SPLINE_CURVE_WITH_KNOTS ( 'NONE', 3,
 ( #27004, #41683, #20407, #89356, #19909, #51276, #50288, #57889, #96440, #73605, #34592, #35087, #97415, #3228, #27983, #65005, #72627, #50781, #65991, #34113, #81241, #82243, #59361, #96944, #74622, #81731, #11815, #26509, #12818, #19432, #58862, #88867, #42672, #89831, #5195, #90338, #43680, #95948, #27510, #80756, #80242, #57387, #36077, #42185, #12308, #73121, #43168, #74110, #66978, #88361 ),
 .UNSPECIFIED., .F., .F.,
 ( 4, 2, 2, 2, 2, 2, 2, 2, 2, 2, 2, 2, 2, 2, 2, 2, 2, 2, 2, 2, 2, 2, 2, 2, 4 ),
 ( 0.0007549782464651950487, 0.001244381850067043365, 0.001733785453668891356, 0.001978487255469815569, 0.002223189057270739781, 0.002345539958171201887, 0.002467890859071663993, 0.002590241759972126100, 0.002712592660872587772, 0.002957294462673536704, 0.003201996264474486070, 0.003691399868076324087, 0.004670207075280077315, 0.005649014282483829676, 0.006138417886085665090, 0.006627821489687500504, 0.006750172390587940927, 0.006811347841038178919, 0.006872523291488416043, 0.006994874192388890292, 0.007117225093289364542, 0.007361926895090339061, 0.007606628696891313580, 0.008096032300493266956, 0.008585435904095221199 ),
 .UNSPECIFIED. ) ;
#12011 = CARTESIAN_POINT ( 'NONE',  ( 76.44488007030824406, 54.92415880672584194, -16.57738246812632354 ) ) ;
#12012 = EDGE_CURVE ( 'NONE', #39035, #87819, #56760, .T. ) ;
#12013 = CARTESIAN_POINT ( 'NONE',  ( 172.9541071254618316, 262.8455706559834653, -15.93875919266165120 ) ) ;
#12014 = CARTESIAN_POINT ( 'NONE',  ( 78.92949518643405327, 222.5024278399160949, 9.188101187500095079 ) ) ;
#12015 = CARTESIAN_POINT ( 'NONE',  ( -42.23460334637721303, 26.80738527414552408, 10.00000000000000000 ) ) ;
#12016 = CARTESIAN_POINT ( 'NONE',  ( 45.34926676561319425, 66.39822172987334170, -10.00000000000000000 ) ) ;
#12017 = ADVANCED_FACE ( 'NONE', ( #64876 ), #95822, .T. ) ;
#12018 = CARTESIAN_POINT ( 'NONE',  ( -16.52110513491133759, 103.4226009623137514, 12.75654370805655091 ) ) ;
#12020 = CARTESIAN_POINT ( 'NONE',  ( 199.7779437056017571, 284.6214466006996417, 18.28733359541573478 ) ) ;
#12019 = CARTESIAN_POINT ( 'NONE',  ( 157.2333142128019858, 258.3109064714224132, 16.87956768598436597 ) ) ;
#12021 = CARTESIAN_POINT ( 'NONE',  ( 150.9363692955544991, 269.2175350005573478, -14.27857383982596140 ) ) ;
#12022 = CARTESIAN_POINT ( 'NONE',  ( 165.7433911102912987, 286.0540145108149090, -5.579755643435937884 ) ) ;
#12023 = CARTESIAN_POINT ( 'NONE',  ( 36.24660459446915439, 29.43085787977765833, -9.188101187500008038 ) ) ;
#12024 = CARTESIAN_POINT ( 'NONE',  ( 147.5381343315788172, 275.1034506142203782, -4.056595942992749393 ) ) ;
#12025 = CARTESIAN_POINT ( 'NONE',  ( 156.7442704525034571, 261.1579551113846378, 17.82061976529222846 ) ) ;
#12026 = ORIENTED_EDGE ( 'NONE', *, *, #77163, .F. ) ;
#12027 = CARTESIAN_POINT ( 'NONE',  ( 26.89353023359722883, 24.03085787977764198, 9.188101187500006262 ) ) ;
#12028 = DIRECTION ( 'NONE',  ( 1.000000000000000000, 7.275925893525578569E-14, 0.000000000000000000 ) ) ;
#12029 = PLANE ( 'NONE',  #28013 ) ;
#12030 = CARTESIAN_POINT ( 'NONE',  ( 189.2189693547002776, 286.5034521383401511, -15.94273063411117874 ) ) ;
#12031 = EDGE_CURVE ( 'NONE', #10803, #33624, #9510, .T. ) ;
#12032 = VERTEX_POINT ( 'NONE', #86064 ) ;
#12033 =( BOUNDED_CURVE ( )  B_SPLINE_CURVE ( 2, ( #4260, #3781, #48881, #66068, #3297, #2800, #27587, #19979, #50855 ),
 .UNSPECIFIED., .F., .T. ) 
 B_SPLINE_CURVE_WITH_KNOTS ( ( 3, 2, 2, 2, 3 ),
 ( 0.06854838709677418818, 0.06989247311827956333, 0.07258064516129032751, 0.07526881720430107781, 0.07661290322580645296 ),
 .UNSPECIFIED. ) 
 CURVE ( )  GEOMETRIC_REPRESENTATION_ITEM ( )  RATIONAL_B_SPLINE_CURVE ( ( 0.9330127018922194093, 0.9330127018922194093, 1.000000000000000000, 0.8660254037844387076, 1.000000000000000000, 0.8660254037844387076, 1.000000000000000000, 0.9330127018922194093, 0.9330127018922194093 ) ) 
 REPRESENTATION_ITEM ( '' )  );
#12034 = PLANE ( 'NONE',  #82596 ) ;
#12035 = CIRCLE ( 'NONE', #92963, 17.82106496071138224 ) ;
#12036 = CARTESIAN_POINT ( 'NONE',  ( 74.76373281376733360, 64.18679306110026062, 14.63261176689765364 ) ) ;
#12037 = CARTESIAN_POINT ( 'NONE',  ( 188.0361769804965206, 281.7550819701144746, -17.70093714309158983 ) ) ;
#12038 = CARTESIAN_POINT ( 'NONE',  ( 136.9263074957796675, 249.8615022471902591, -10.00000000000009592 ) ) ;
#12039 = CARTESIAN_POINT ( 'NONE',  ( 157.2777284163744582, 258.2339788142568864, -16.82360006463426316 ) ) ;
#12040 = CARTESIAN_POINT ( 'NONE',  ( 75.25301932441034580, 53.09737962384632937, 16.48714817978221348 ) ) ;
#12041 = ORIENTED_EDGE ( 'NONE', *, *, #74967, .T. ) ;
#12042 = CARTESIAN_POINT ( 'NONE',  ( 165.8692079773426826, 246.3314739835906835, -1.162168092255636775 ) ) ;
#12043 = ORIENTED_EDGE ( 'NONE', *, *, #34396, .T. ) ;
#12044 = CARTESIAN_POINT ( 'NONE',  ( 202.4943568615953779, 279.9164810001701085, 17.09064351659286984 ) ) ;
#12045 = CARTESIAN_POINT ( 'NONE',  ( 85.12278939449318216, 42.79832675737401360, 3.312954136966923535 ) ) ;
#12046 = ORIENTED_EDGE ( 'NONE', *, *, #89482, .F. ) ;
#12047 = PLANE ( 'NONE',  #46677 ) ;
#12049 = ORIENTED_EDGE ( 'NONE', *, *, #37813, .T. ) ;
#12048 = VECTOR ( 'NONE', #13447, 1000.000000000000000 ) ;
#12050 = CARTESIAN_POINT ( 'NONE',  ( 89.15240563351599690, 155.9128137034261954, 0.000000000000000000 ) ) ;
#12051 = CARTESIAN_POINT ( 'NONE',  ( 8.399671500380161859, 16.80066082961419482, 10.00000000000000533 ) ) ;
#12052 = LINE ( 'NONE', #26250, #16994 ) ;
#12053 = CARTESIAN_POINT ( 'NONE',  ( 87.98904372666932261, 44.25610683789894750, -4.385737539232398063 ) ) ;
#12054 = CARTESIAN_POINT ( 'NONE',  ( 95.64807497750081211, 214.4824982072973683, 3.021315404115420679E-15 ) ) ;
#12055 = CARTESIAN_POINT ( 'NONE',  ( 26.79248755578709762, 33.65586893147757763, -7.433330006724137462 ) ) ;
#12056 = CARTESIAN_POINT ( 'NONE',  ( 19.39999966495784989, 36.48715600906564305, -10.00000000000000000 ) ) ;
#12057 = CARTESIAN_POINT ( 'NONE',  ( 164.2758297317967902, 275.0605672077817871, 14.75495795951908740 ) ) ;
#12058 = LINE ( 'NONE', #87629, #65917 ) ;
#12059 = ORIENTED_EDGE ( 'NONE', *, *, #5644, .T. ) ;
#12060 = ORIENTED_EDGE ( 'NONE', *, *, #13474, .T. ) ;
#12061 = CARTESIAN_POINT ( 'NONE',  ( 87.23690874686347740, 46.15778144619924461, -8.941654336830676897 ) ) ;
#12063 = CARTESIAN_POINT ( 'NONE',  ( 165.8703699689788493, 274.3934474687724219, -15.11696372367774721 ) ) ;
#12062 = CARTESIAN_POINT ( 'NONE',  ( 164.2413944571582078, 246.1725554246774834, 7.304616466633322425 ) ) ;
#12064 = CARTESIAN_POINT ( 'NONE',  ( 85.65483554831503454, 48.88356815160276625, -12.11013705813561181 ) ) ;
#12065 = CARTESIAN_POINT ( 'NONE',  ( 66.18256082828796139, 68.61784451530441231, -2.171160931695417684 ) ) ;
#12066 = DIRECTION ( 'NONE',  ( -0.7080737730998298840, 0.7061384650677022812, 0.000000000000000000 ) ) ;
#12067 = CARTESIAN_POINT ( 'NONE',  ( 164.9009427471078766, 270.4319544559331234, -17.40525121274953335 ) ) ;
#12068 = CARTESIAN_POINT ( 'NONE',  ( 207.3954518193029912, 271.4275355207012694, -4.733997076022094852 ) ) ;
#12069 = CARTESIAN_POINT ( 'NONE',  ( 163.8835510476618254, 277.4261113242017132, -14.47671527678674330 ) ) ;
#12070 = CARTESIAN_POINT ( 'NONE',  ( 182.0294364313458857, 256.9024481669246143, 5.105451491673651532 ) ) ;
#12071 = CARTESIAN_POINT ( 'NONE',  ( 95.92524373570365981, 232.3149278399160949, -9.188101187500095079 ) ) ;
#12072 = ORIENTED_EDGE ( 'NONE', *, *, #11853, .F. ) ;
#12073 = CARTESIAN_POINT ( 'NONE',  ( 190.8860811105559208, 300.0226043892405414, 8.636347304323541252 ) ) ;
#12074 = CARTESIAN_POINT ( 'NONE',  ( 166.6051582734733358, 278.7391106529776721, -13.20946712174476545 ) ) ;
#12075 = ORIENTED_EDGE ( 'NONE', *, *, #5755, .F. ) ;
#12076 = ORIENTED_EDGE ( 'NONE', *, *, #57162, .F. ) ;
#12077 = EDGE_LOOP ( 'NONE', ( #86720, #97898, #21982, #83721, #76467 ) ) ;
#12078 = CARTESIAN_POINT ( 'NONE',  ( 86.99754070748903700, 45.91539075293407990, -8.140839447248088945 ) ) ;
#12079 = CARTESIAN_POINT ( 'NONE',  ( 180.3528982427918663, 293.8293478312841671, -2.635769195210191818 ) ) ;
#12080 = CARTESIAN_POINT ( 'NONE',  ( 164.2537261577595586, 249.8683019904829621, 10.06821014759007404 ) ) ;
#12081 = CARTESIAN_POINT ( 'NONE',  ( 10.74796456262465050, 21.90829794293879473, 10.00000000000000355 ) ) ;
#12082 = CARTESIAN_POINT ( 'NONE',  ( 163.0311878320900121, 248.2686947869521532, 10.33250033289960435 ) ) ;
#12083 = ORIENTED_EDGE ( 'NONE', *, *, #36288, .F. ) ;
#12084 = DIRECTION ( 'NONE',  ( -0.2575544297740022803, 0.9662637919863232838, 0.000000000000000000 ) ) ;
#12085 = CARTESIAN_POINT ( 'NONE',  ( 162.9383752892161397, 248.4294508267893491, -11.25953730674605957 ) ) ;
#12086 = ORIENTED_EDGE ( 'NONE', *, *, #77743, .T. ) ;
#12087 = ADVANCED_FACE ( 'NONE', ( #38884 ), #46477, .T. ) ;
#12088 = CARTESIAN_POINT ( 'NONE',  ( 194.9900005546388968, 265.9144807066997487, -8.896229505766779511 ) ) ;
#12089 = CARTESIAN_POINT ( 'NONE',  ( 153.2524140410926918, 266.3468094423246271, 16.28161397018561374 ) ) ;
#12090 = CARTESIAN_POINT ( 'NONE',  ( 66.17343954913512505, 68.52301864461630032, -2.711686016849372827 ) ) ;
#12092 = CARTESIAN_POINT ( 'NONE',  ( 199.9329555241513106, 283.7849761008080804, 16.97275319715699737 ) ) ;
#12091 = CARTESIAN_POINT ( 'NONE',  ( 129.5380282679697075, 245.5958772461660544, -9.188101187500095079 ) ) ;
#12093 = DIRECTION ( 'NONE',  ( 1.000000000000000000, 0.000000000000000000, 0.000000000000000000 ) ) ;
#12094 = CARTESIAN_POINT ( 'NONE',  ( -42.47074677134370546, 28.21475011077167849, -10.00000000000000000 ) ) ;
#12095 = EDGE_LOOP ( 'NONE', ( #90099, #61533, #6200, #90460 ) ) ;
#12096 = CARTESIAN_POINT ( 'NONE',  ( 86.25114834473923509, 43.91001722141434271, -4.889282600613897856 ) ) ;
#12097 = CARTESIAN_POINT ( 'NONE',  ( 177.2212890013350659, 257.5021112054951686, 11.61326389234794298 ) ) ;
#12098 = DIRECTION ( 'NONE',  ( 0.4999999999999992784, -0.8660254037844390407, 0.000000000000000000 ) ) ;
#12099 = CARTESIAN_POINT ( 'NONE',  ( 189.5156151668331290, 270.2242446231968529, 14.35960433212074250 ) ) ;
#12101 = EDGE_CURVE ( 'NONE', #59362, #55035, #94132, .T. ) ;
#12100 = CARTESIAN_POINT ( 'NONE',  ( -4.065086259125790136, 119.3853102282570120, 36.50000000000000000 ) ) ;
#12102 = DIRECTION ( 'NONE',  ( 0.9133924323370964382, -0.1624253398589829422, -0.3732723851572960494 ) ) ;
#12103 = EDGE_CURVE ( 'NONE', #99288, #13470, #99604, .T. ) ;
#12104 = VECTOR ( 'NONE', #49702, 1000.000000000000114 ) ;
#12105 = CARTESIAN_POINT ( 'NONE',  ( 82.49322465416763350, 40.88878199599866292, -3.716918875651960441 ) ) ;
#12106 = CARTESIAN_POINT ( 'NONE',  ( 142.6123662252853421, 259.5780487066560340, -7.305945665944390655 ) ) ;
#12107 = CARTESIAN_POINT ( 'NONE',  ( 80.13153417293931113, 50.66350872248114001, 14.80289417267747965 ) ) ;
#12108 = CARTESIAN_POINT ( 'NONE',  ( 206.7424236707713305, 272.1642866507044118, 6.817570650586102232 ) ) ;
#12109 = CARTESIAN_POINT ( 'NONE',  ( 159.9894443651313338, 253.5371490153152081, -16.36035038356864391 ) ) ;
#12110 = CARTESIAN_POINT ( 'NONE',  ( 77.80736617348490824, 61.72758938687779562, 16.06622420362090153 ) ) ;
#12111 = CARTESIAN_POINT ( 'NONE',  ( 207.6067494229581314, 271.0615573356529353, -1.924113146155245868 ) ) ;
#12112 = CARTESIAN_POINT ( 'NONE',  ( 110.0000000000000142, 15.00000000000000000, 1.387778780781445676E-14 ) ) ;
#12113 = AXIS2_PLACEMENT_3D ( 'NONE', #9725, #25917, #40579 ) ;
#12114 = CARTESIAN_POINT ( 'NONE',  ( 69.77890858254123430, 70.63368750135978757, -2.958018195249015658 ) ) ;
#12115 = CARTESIAN_POINT ( 'NONE',  ( 181.9913877802205775, 264.0113901683749305, 13.86632907263398096 ) ) ;
#12116 = CARTESIAN_POINT ( 'NONE',  ( 181.2370176562050688, 263.3306497680472944, -14.40870033085988666 ) ) ;
#12117 = CARTESIAN_POINT ( 'NONE',  ( 42.39820071321547346, 24.28848085856235173, 1.475505719884397138E-15 ) ) ;
#12118 = LINE ( 'NONE', #51091, #93521 ) ;
#12119 = CARTESIAN_POINT ( 'NONE',  ( 157.6058986277583642, 270.9393266711600177, -14.76023724535021664 ) ) ;
#12120 = CARTESIAN_POINT ( 'NONE',  ( 81.15576878495137692, 43.19889211345415703, -8.824872785026526500 ) ) ;
#12121 = CARTESIAN_POINT ( 'NONE',  ( 207.1285138014047504, 271.8898857301724661, -5.752177443817618752 ) ) ;
#12122 = EDGE_CURVE ( 'NONE', #23117, #54050, #15575, .T. ) ;
#12123 = CARTESIAN_POINT ( 'NONE',  ( 21.69106252476256458, 174.1423013555409796, -4.594050593750043987 ) ) ;
#12124 = CARTESIAN_POINT ( 'NONE',  ( 68.29064676983747972, 69.02907622317006542, 6.494102608087607642 ) ) ;
#12125 = ORIENTED_EDGE ( 'NONE', *, *, #48465, .T. ) ;
#12126 = EDGE_CURVE ( 'NONE', #77337, #87147, #62972, .T. ) ;
#12127 = CARTESIAN_POINT ( 'NONE',  ( 87.22595043061240005, 46.05622627631750987, 8.811080105847633348 ) ) ;
#12128 = EDGE_CURVE ( 'NONE', #34739, #4742, #40374, .T. ) ;
#12129 = FACE_OUTER_BOUND ( 'NONE', #97585, .T. ) ;
#12130 = CARTESIAN_POINT ( 'NONE',  ( 71.67936538144843439, 72.44724869688445779, -1.358217801655851931 ) ) ;
#12131 = CARTESIAN_POINT ( 'NONE',  ( 45.85867072306329817, 185.0327760586659451, 1.948934522072302763E-15 ) ) ;
#12132 = CIRCLE ( 'NONE', #33171, 49.99999999999999289 ) ;
#12133 = CARTESIAN_POINT ( 'NONE',  ( 200.7897860911934913, 282.8688841796032420, 18.17522996445731920 ) ) ;
#12134 = CARTESIAN_POINT ( 'NONE',  ( 174.0050912145983659, 289.3368536554620505, 7.990428673744625065 ) ) ;
#12135 = CARTESIAN_POINT ( 'NONE',  ( 190.2510882691990730, 301.1224442529128851, -5.480893437181090455 ) ) ;
#12136 = CARTESIAN_POINT ( 'NONE',  ( 3.825981621811214151, 23.18502408145589300, 5.678558825948277544 ) ) ;
#12137 = CARTESIAN_POINT ( 'NONE',  ( 203.0446730937520954, 269.9112416612543939, -7.271914997583759366 ) ) ;
#12138 = CARTESIAN_POINT ( 'NONE',  ( 191.0724301404414689, 299.6998384015373063, -9.342134220577969828 ) ) ;
#12139 = DIRECTION ( 'NONE',  ( -0.9909246428798921258, -0.1344185706417024839, 0.000000000000000000 ) ) ;
#12140 = DIRECTION ( 'NONE',  ( 1.000000000000000000, 0.000000000000000000, 0.000000000000000000 ) ) ;
#12141 = EDGE_CURVE ( 'NONE', #25763, #22997, #42004, .T. ) ;
#12142 = CARTESIAN_POINT ( 'NONE',  ( 113.3812418268422846, 236.2677522451418497, 10.00000000000009592 ) ) ;
#12143 = EDGE_CURVE ( 'NONE', #44579, #83882, #10966, .T. ) ;
#12144 = FACE_OUTER_BOUND ( 'NONE', #29588, .T. ) ;
#12145 = CARTESIAN_POINT ( 'NONE',  ( 74.01413570136905662, 57.15554519978635994, -15.99517262605232659 ) ) ;
#12146 = CARTESIAN_POINT ( 'NONE',  ( 83.66574516303668929, 209.1115022471902023, -5.000000000000041744 ) ) ;
#12147 = CARTESIAN_POINT ( 'NONE',  ( 7.868168403658736487, 186.8967562850346837, -4.648177544792955347E-16 ) ) ;
#12148 = LINE ( 'NONE', #57227, #88759 ) ;
#12149 = ORIENTED_EDGE ( 'NONE', *, *, #11582, .T. ) ;
#12150 = CARTESIAN_POINT ( 'NONE',  ( 50.56751030825869009, 193.8768266524160140, 9.188101187500098632 ) ) ;
#12151 = EDGE_LOOP ( 'NONE', ( #35328, #93972, #81868, #47918 ) ) ;
#12152 = CARTESIAN_POINT ( 'NONE',  ( 82.86586985908988368, 152.2544130683315871, 0.000000000000000000 ) ) ;
#12153 = CARTESIAN_POINT ( 'NONE',  ( 146.9376205018946848, 276.1435710778808925, 5.066564108429441937 ) ) ;
#12154 = PLANE ( 'NONE',  #79043 ) ;
#12155 = VERTEX_POINT ( 'NONE', #69292 ) ;
#12156 = CARTESIAN_POINT ( 'NONE',  ( 167.3572442387605577, 285.1339219078583938, 7.830934403729975735 ) ) ;
#12157 = CARTESIAN_POINT ( 'NONE',  ( 164.8670003495851404, 245.0889742334797177, -1.557028074864921674 ) ) ;
#12158 = CARTESIAN_POINT ( 'NONE',  ( -19.65312891409030271, 93.06504152958497400, -10.00000000000000888 ) ) ;
#12159 = CARTESIAN_POINT ( 'NONE',  ( 36.80649086932150027, 23.11110640527294535, -2.839279412974138328 ) ) ;
#12160 = CARTESIAN_POINT ( 'NONE',  ( 73.04656796621824810, 70.72172819928655940, -7.591179416118629675 ) ) ;
#12161 = CARTESIAN_POINT ( 'NONE',  ( 176.7491000883603078, 284.2402667147796933, -14.85471036738550055 ) ) ;
#12162 = FACE_OUTER_BOUND ( 'NONE', #51047, .T. ) ;
#12163 = ORIENTED_EDGE ( 'NONE', *, *, #43755, .T. ) ;
#12164 = CARTESIAN_POINT ( 'NONE',  ( 19.48598279363274344, 13.11110640527291693, -2.839279412974138328 ) ) ;
#12165 = CARTESIAN_POINT ( 'NONE',  ( 68.70248306966885821, 64.25130556195607312, 12.49291083475091746 ) ) ;
#12166 = CARTESIAN_POINT ( 'NONE',  ( 174.9106947789025241, 255.1781923355507899, 8.157823743021118901 ) ) ;
#12167 = CARTESIAN_POINT ( 'NONE',  ( 47.49582885874516336, 78.29235751436857527, -10.00000000000000000 ) ) ;
#12168 = ORIENTED_EDGE ( 'NONE', *, *, #49617, .T. ) ;
#12169 = CARTESIAN_POINT ( 'NONE',  ( 182.4004271739244700, 284.1903799708203451, 16.39187655311515002 ) ) ;
#12170 = CARTESIAN_POINT ( 'NONE',  ( 82.93017357788673394, 175.3855496052738374, -21.50000000000000000 ) ) ;
#12171 = CARTESIAN_POINT ( 'NONE',  ( 165.5845016731641124, 245.8462254865437160, 0.7221155814038995313 ) ) ;
#12172 = AXIS2_PLACEMENT_3D ( 'NONE', #74261, #35731, #28125 ) ;
#12173 = EDGE_LOOP ( 'NONE', ( #47654, #53343, #69862, #80647 ) ) ;
#12174 = ORIENTED_EDGE ( 'NONE', *, *, #90000, .T. ) ;
#12176 = CARTESIAN_POINT ( 'NONE',  ( 34.25126403021256749, 69.88882648778609052, 59.99999999999999289 ) ) ;
#12175 = CARTESIAN_POINT ( 'NONE',  ( 207.8844858873204657, 270.5805036682629066, -6.251308616122969397 ) ) ;
#12177 = CARTESIAN_POINT ( 'NONE',  ( 198.2505066714982149, 285.2670451491296149, 0.000000000000000000 ) ) ;
#12178 = EDGE_LOOP ( 'NONE', ( #74111, #71506, #64228, #32976 ) ) ;
#12179 = CARTESIAN_POINT ( 'NONE',  ( 66.07625507003409382, 68.50412252646739830, -2.501755903184967433 ) ) ;
#12180 = DIRECTION ( 'NONE',  ( -0.5102188382608503492, 0.8600446134263898257, 0.000000000000000000 ) ) ;
#12181 = FACE_OUTER_BOUND ( 'NONE', #13887, .T. ) ;
#12182 = CARTESIAN_POINT ( 'NONE',  ( 78.34332907769417886, 61.12495998885079018, -15.90539878443391864 ) ) ;
#12183 = EDGE_CURVE ( 'NONE', #71188, #86782, #56861, .T. ) ;
#12184 = CARTESIAN_POINT ( 'NONE',  ( 157.7593757092099906, 257.3997412317380054, -18.08445832352326121 ) ) ;
#12186 = CARTESIAN_POINT ( 'NONE',  ( 126.7237928014352804, 231.7202760586659736, -5.415160957724236172E-17 ) ) ;
#12185 = AXIS2_PLACEMENT_3D ( 'NONE', #14005, #6411, #21611 ) ;
#12187 = CARTESIAN_POINT ( 'NONE',  ( 164.2413944571582078, 246.1725554246774834, 7.304616466633322425 ) ) ;
#12188 = CYLINDRICAL_SURFACE ( 'NONE', #67366, 17.82106496071139645 ) ;
#12189 = ORIENTED_EDGE ( 'NONE', *, *, #80428, .F. ) ;
#12190 = B_SPLINE_CURVE_WITH_KNOTS ( 'NONE', 3,
 ( #97186, #29248, #43926, #20162 ),
 .UNSPECIFIED., .F., .F.,
 ( 4, 4 ),
 ( 0.01237858375601574683, 0.02090696561293280478 ),
 .UNSPECIFIED. ) ;
#12191 = CARTESIAN_POINT ( 'NONE',  ( 163.7183543885751078, 247.0784873978576854, -6.786164904910574336 ) ) ;
#12192 = ORIENTED_EDGE ( 'NONE', *, *, #30086, .F. ) ;
#12193 = CARTESIAN_POINT ( 'NONE',  ( 35.31080938399455249, 26.10170272979929607, -7.433330006724141015 ) ) ;
#12194 = FACE_BOUND ( 'NONE', #20291, .T. ) ;
#12195 = CARTESIAN_POINT ( 'NONE',  ( 75.31302016003080269, 66.58151914953994321, -13.09053389059541139 ) ) ;
#12196 = CARTESIAN_POINT ( 'NONE',  ( 76.60222546164588664, 215.0333772461660544, 9.188101187500095079 ) ) ;
#12197 = ORIENTED_EDGE ( 'NONE', *, *, #39476, .T. ) ;
#12198 = CARTESIAN_POINT ( 'NONE',  ( -30.22813246154364109, 95.60533857986700923, 12.75846431767311451 ) ) ;
#12199 = CARTESIAN_POINT ( 'NONE',  ( 120.3761533483303907, 228.7592609112379591, 2.679491924311254714 ) ) ;
#12200 = CARTESIAN_POINT ( 'NONE',  ( 150.9982109096994520, 269.1104221828363734, 14.90714565999273766 ) ) ;
#12201 = CARTESIAN_POINT ( 'NONE',  ( 175.6099198705963431, 278.4306179087495252, 15.49799073493723967 ) ) ;
#12202 = VERTEX_POINT ( 'NONE', #57581 ) ;
#12203 = CARTESIAN_POINT ( 'NONE',  ( 70.10178725980775027, 64.18715254517744029, -12.51786991059252685 ) ) ;
#12204 = CARTESIAN_POINT ( 'NONE',  ( -89.11465314115667979, 93.37593066204033221, -30.52142883766496695 ) ) ;
#12205 = CARTESIAN_POINT ( 'NONE',  ( 86.19918046091518704, 42.54196271365974980, 0.6765657524371224696 ) ) ;
#12206 = ORIENTED_EDGE ( 'NONE', *, *, #18483, .T. ) ;
#12207 = CARTESIAN_POINT ( 'NONE',  ( 143.0969038086192597, 260.4263049900483225, -7.951529393128359935 ) ) ;
#12208 = DIRECTION ( 'NONE',  ( -0.4999999999999987788, 0.8660254037844392627, 0.000000000000000000 ) ) ;
#12209 = DIRECTION ( 'NONE',  ( 0.000000000000000000, -0.000000000000000000, 1.000000000000000000 ) ) ;
#12210 = DIRECTION ( 'NONE',  ( 1.000000000000000000, 0.000000000000000000, 0.000000000000000000 ) ) ;
#12211 = EDGE_CURVE ( 'NONE', #6816, #59735, #88555, .T. ) ;
#12212 = DIRECTION ( 'NONE',  ( -0.000000000000000000, 0.000000000000000000, -1.000000000000000000 ) ) ;
#12213 = B_SPLINE_CURVE_WITH_KNOTS ( 'NONE', 3,
 ( #86725, #39043, #78080, #7668, #22863, #1075, #85734, #8173, #16263, #15753, #69954, #38045, #46659, #68959, #99881, #77060 ),
 .UNSPECIFIED., .F., .F.,
 ( 4, 1, 2, 2, 2, 1, 2, 2, 4 ),
 ( 0.000000000000000000, 0.1250000000000006661, 0.1875000000000009714, 0.2500000000000012768, 0.5000000000000007772, 0.6250000000000001110, 0.6875000000000006661, 0.7500000000000012212, 1.000000000000000000 ),
 .UNSPECIFIED. ) ;
#12214 = CARTESIAN_POINT ( 'NONE',  ( 151.6960368807307873, 276.4293682816003752, 8.579070964960488155 ) ) ;
#12215 = VECTOR ( 'NONE', #64162, 1000.000000000000000 ) ;
#12216 = CARTESIAN_POINT ( 'NONE',  ( 152.3784850679831493, 270.1081530411233302, -14.58078914583996344 ) ) ;
#12217 = DIRECTION ( 'NONE',  ( 0.000000000000000000, -1.000000000000000000, -1.201851678989722492E-15 ) ) ;
#12218 = ORIENTED_EDGE ( 'NONE', *, *, #77788, .T. ) ;
#12219 = CARTESIAN_POINT ( 'NONE',  ( 207.5408646414791178, 271.1756731246201753, 3.050859480894625886 ) ) ;
#12220 = CARTESIAN_POINT ( 'NONE',  ( 127.2647115830355347, 244.2833772461660544, -9.188101187500095079 ) ) ;
#12221 = EDGE_LOOP ( 'NONE', ( #85211, #60745, #73215, #46154 ) ) ;
#12222 = CARTESIAN_POINT ( 'NONE',  ( 191.0724301404414689, 299.6998384015373063, -9.342134220577969828 ) ) ;
#12223 = CARTESIAN_POINT ( 'NONE',  ( 49.07456115661582174, 91.13648234292965356, 10.00000000000000000 ) ) ;
#12224 = CARTESIAN_POINT ( 'NONE',  ( 155.3250150347760723, 261.6161776038049425, -18.57420904020362684 ) ) ;
#12225 = ADVANCED_FACE ( 'NONE', ( #42374 ), #3898, .T. ) ;
#12226 = CARTESIAN_POINT ( 'NONE',  ( 204.8762144138505903, 275.7909827032724479, 14.60855957933206817 ) ) ;
#12227 = EDGE_CURVE ( 'NONE', #71064, #42571, #1256, .T. ) ;
#12228 = CARTESIAN_POINT ( 'NONE',  ( 75.48702785388739755, 65.17841116432670390, 13.95333018839138006 ) ) ;
#12229 = DIRECTION ( 'NONE',  ( -0.000000000000000000, 0.000000000000000000, 1.000000000000000000 ) ) ;
#12230 = VERTEX_POINT ( 'NONE', #97138 ) ;
#12231 = CARTESIAN_POINT ( 'NONE',  ( -47.59865527897274973, 48.00312894580780210, 59.99999999999999289 ) ) ;
#12232 = CARTESIAN_POINT ( 'NONE',  ( 157.5458375898066663, 275.8685363031948441, 12.98959349559163634 ) ) ;
#12233 = CARTESIAN_POINT ( 'NONE',  ( -66.55019942848203129, 42.78701949053055387, -10.00000000000000000 ) ) ;
#12234 = CARTESIAN_POINT ( 'NONE',  ( 31.46967238556409896, 195.6427522451419350, -10.00000000000009592 ) ) ;
#12235 = CARTESIAN_POINT ( 'NONE',  ( 137.8731756836298814, 262.6589784336661637, -6.496448406907676862E-16 ) ) ;
#12236 = B_SPLINE_CURVE_WITH_KNOTS ( 'NONE', 3,
 ( #15748, #22858, #68455, #53742 ),
 .UNSPECIFIED., .F., .F.,
 ( 4, 4 ),
 ( 0.03872932741557565117, 0.04724607957928941143 ),
 .UNSPECIFIED. ) ;
#12237 = CARTESIAN_POINT ( 'NONE',  ( 146.8516045228164160, 276.2925551239072774, 3.995954059407343273 ) ) ;
#12238 = CARTESIAN_POINT ( 'NONE',  ( 68.34215885236082499, 69.21295319673539836, 4.808519653334967892 ) ) ;
#12239 = VECTOR ( 'NONE', #57268, 1000.000000000000114 ) ;
#12241 = CARTESIAN_POINT ( 'NONE',  ( 171.8245779312147477, 251.1353067130050363, 3.410672705103630076 ) ) ;
#12240 = B_SPLINE_CURVE_WITH_KNOTS ( 'NONE', 3,
 ( #35701, #66600, #58001, #58968, #89940, #5307, #82357, #42779, #67590, #20016, #75214, #89461, #36184, #21503, #4817, #74729, #19536, #67089, #50893, #21022, #28590, #81842, #83332, #12418, #43285, #97527, #12925, #59472, #98013, #58486, #51904, #50398, #74230, #35197, #90948, #11922, #81352, #73713, #28097, #82845, #13416, #20516, #27118, #42289, #51393, #4295, #88983, #43784 ),
 .UNSPECIFIED., .F., .F.,
 ( 4, 2, 2, 2, 2, 2, 2, 2, 2, 2, 2, 2, 2, 2, 2, 2, 2, 2, 2, 2, 2, 2, 2, 4 ),
 ( 0.002594831937057109125, 0.003014445506990537805, 0.003224252291957272962, 0.003329155684440719687, 0.003434059076924166412, 0.003538962469407613137, 0.003643865861891059862, 0.003853672646858035278, 0.004273286216791986544, 0.005112513356659858718, 0.005951740496527732627, 0.006790967636395604801, 0.007210581206329462825, 0.007630194776263320849, 0.007735098168746732880, 0.007787549864988394660, 0.007840001561230058175, 0.007944904953713385204, 0.008049808346196712233, 0.008469421916130011677, 0.008679228701096703899, 0.008889035486063394387, 0.009098842271030084874, 0.009308649055996777097 ),
 .UNSPECIFIED. ) ;
#12242 = CARTESIAN_POINT ( 'NONE',  ( 23.34564182995783455, 13.28848085856231442, 1.475505719884397138E-15 ) ) ;
#12243 = CARTESIAN_POINT ( 'NONE',  ( 190.7805732161387766, 300.2053494229706985, 4.237982805666590025 ) ) ;
#12244 = CARTESIAN_POINT ( 'NONE',  ( 81.84662774497913063, 41.65891706340769218, 5.409804292327541120 ) ) ;
#12245 = CARTESIAN_POINT ( 'NONE',  ( 169.3462360422239499, 285.1681312824781571, -8.761088339260869162 ) ) ;
#12246 = VECTOR ( 'NONE', #25241, 1000.000000000000227 ) ;
#12247 = DIRECTION ( 'NONE',  ( -1.000000000000000000, 0.000000000000000000, 0.000000000000000000 ) ) ;
#12248 = CARTESIAN_POINT ( 'NONE',  ( 157.4719395156559472, 271.1205387963237854, -14.65500712271581385 ) ) ;
#12249 = EDGE_CURVE ( 'NONE', #78709, #62627, #21069, .T. ) ;
#12250 = CARTESIAN_POINT ( 'NONE',  ( 136.7639277290221855, 239.7677522451417929, -5.000000000000041744 ) ) ;
#12251 = LINE ( 'NONE', #65929, #20817 ) ;
#12252 = ORIENTED_EDGE ( 'NONE', *, *, #34281, .F. ) ;
#12253 = CARTESIAN_POINT ( 'NONE',  ( 157.8763546842245376, 257.1971277035954699, 17.68444922773363004 ) ) ;
#12254 = CARTESIAN_POINT ( 'NONE',  ( 150.8247211172754589, 269.4109153179094278, -14.37608026040300402 ) ) ;
#12255 = CARTESIAN_POINT ( 'NONE',  ( -0.3657822996961275219, 170.5958772461660544, -9.188101187500095079 ) ) ;
#12256 = CARTESIAN_POINT ( 'NONE',  ( 63.88265089144443465, 201.5643266524160424, 9.188101187500095079 ) ) ;
#12257 = CARTESIAN_POINT ( 'NONE',  ( 83.55156767614275282, 41.73934938018408047, 4.529189728718444385 ) ) ;
#12258 = CARTESIAN_POINT ( 'NONE',  ( 24.48230016887698568, 13.94473085651392452, 1.475505719884397138E-15 ) ) ;
#12259 = CARTESIAN_POINT ( 'NONE',  ( 85.85757975920050455, 48.54684933318403495, 12.22929488966399880 ) ) ;
#12260 = CARTESIAN_POINT ( 'NONE',  ( 205.2660270307054304, 275.1158074454486382, -13.97598661256119179 ) ) ;
#12261 = CARTESIAN_POINT ( 'NONE',  ( 191.5311128828054734, 291.7127007975493598, -14.32894664656410910 ) ) ;
#12262 = CARTESIAN_POINT ( 'NONE',  ( 146.8881680668833951, 276.2292252078784145, 4.973452195244782104 ) ) ;
#12263 = CARTESIAN_POINT ( 'NONE',  ( 74.09797824419197809, 55.64112326900559680, -16.58847249929255341 ) ) ;
#12265 = CARTESIAN_POINT ( 'NONE',  ( 75.63696797857055287, 201.1427522451417644, 1.119607411625061291E-15 ) ) ;
#12264 = CARTESIAN_POINT ( 'NONE',  ( 170.8805640699686990, 257.7213711969266114, 14.63406020945912367 ) ) ;
#12266 = ADVANCED_FACE ( 'NONE', ( #13013 ), #52472, .T. ) ;
#12267 = CARTESIAN_POINT ( 'NONE',  ( 178.7496050114017123, 254.0362436929630121, -4.160075916196277035 ) ) ;
#12268 = CARTESIAN_POINT ( 'NONE',  ( 32.30839531297598910, 123.0650415295850593, -10.00000000000000888 ) ) ;
#12269 = CARTESIAN_POINT ( 'NONE',  ( 151.0254882145115971, 269.0631765050081299, 14.78274390654921078 ) ) ;
#12270 = CARTESIAN_POINT ( 'NONE',  ( 42.09652578138359047, 195.1115022471902591, 10.00000000000009592 ) ) ;
#12271 = CARTESIAN_POINT ( 'NONE',  ( 181.7891714221429709, 291.6511982500477984, 9.251581008942281414 ) ) ;
#12272 = LINE ( 'NONE', #74074, #38489 ) ;
#12273 = CARTESIAN_POINT ( 'NONE',  ( 1.284818304444202530, 180.7369531367911293, -4.594050593750048428 ) ) ;
#12274 = CARTESIAN_POINT ( 'NONE',  ( 167.7976356284401334, 287.1346734032483710, 5.039741953860431778 ) ) ;
#12275 = CARTESIAN_POINT ( 'NONE',  ( 153.1973045377566507, 265.3014802884401320, 17.70608187426261892 ) ) ;
#12276 = CARTESIAN_POINT ( 'NONE',  ( 35.16646543599519248, 35.70171378149922248, -9.188101187500004485 ) ) ;
#12277 = CARTESIAN_POINT ( 'NONE',  ( 20.54487693938818538, 27.56454794089042082, 10.00000000000000355 ) ) ;
#12278 = CARTESIAN_POINT ( 'NONE',  ( 207.1122325394003951, 271.9180857031755636, 7.794245785756032774 ) ) ;
#12279 = CARTESIAN_POINT ( 'NONE',  ( 193.7275870247597425, 295.1009717758319084, 14.48058678254265885 ) ) ;
#12280 = CARTESIAN_POINT ( 'NONE',  ( -19.65312891409030271, 93.06504152958497400, 10.00000000000000888 ) ) ;
#12281 = CARTESIAN_POINT ( 'NONE',  ( 176.6809650034762740, 260.2657671503346251, -13.65821825376172782 ) ) ;
#12282 = APPLICATION_PROTOCOL_DEFINITION ( 'draft international standard', 'automotive_design', 1998, #40519 ) ;
#12283 = EDGE_CURVE ( 'NONE', #2731, #63769, #21110, .T. ) ;
#12284 = CARTESIAN_POINT ( 'NONE',  ( 16.32921660555538423, 21.37878583063840310, 9.188101187500006262 ) ) ;
#12285 = CARTESIAN_POINT ( 'NONE',  ( 71.76139268086218692, 72.52520824035063640, 0.9833505332507315178 ) ) ;
#12286 = CARTESIAN_POINT ( 'NONE',  ( 82.42561518943209364, 53.83419803862933861, 15.85509184085860745 ) ) ;
#12287 = FACE_OUTER_BOUND ( 'NONE', #61546, .T. ) ;
#12288 = VECTOR ( 'NONE', #21447, 1000.000000000000000 ) ;
#12289 = DIRECTION ( 'NONE',  ( 0.9819794923402651587, -0.1889875038809575580, 0.000000000000000000 ) ) ;
#12290 = ORIENTED_EDGE ( 'NONE', *, *, #25559, .F. ) ;
#12291 = CARTESIAN_POINT ( 'NONE',  ( 18.51072855673551487, 34.18528772668518201, -1.583844403245363575 ) ) ;
#12292 = CARTESIAN_POINT ( 'NONE',  ( 74.94754896363279784, 53.48443655244039263, -16.53883777380878684 ) ) ;
#12293 = DIRECTION ( 'NONE',  ( 1.000000000000000000, 0.000000000000000000, 0.000000000000000000 ) ) ;
#12294 = CARTESIAN_POINT ( 'NONE',  ( 190.0534303668326288, 269.9073674132432643, 15.26070177760127322 ) ) ;
#12295 = ORIENTED_EDGE ( 'NONE', *, *, #49742, .T. ) ;
#12296 = CARTESIAN_POINT ( 'NONE',  ( 153.1973045377566507, 265.3014802884401320, 17.70608187426261892 ) ) ;
#12297 = CARTESIAN_POINT ( 'NONE',  ( 68.70570789778643928, 70.27148567445367178, -0.5708798829847213652 ) ) ;
#12298 = CIRCLE ( 'NONE', #13948, 70.00000000000001421 ) ;
#12299 = CARTESIAN_POINT ( 'NONE',  ( 66.43537002243755296, 68.65414004482329347, 4.832212937122434049 ) ) ;
#12300 = CARTESIAN_POINT ( 'NONE',  ( 87.10115137904760729, 45.28340438443852634, 6.995308688534726649 ) ) ;
#12301 = VERTEX_POINT ( 'NONE', #83419 ) ;
#12302 = ORIENTED_EDGE ( 'NONE', *, *, #74187, .F. ) ;
#12304 = DIRECTION ( 'NONE',  ( -0.7135562106085678868, 0.7005979833698787740, 0.000000000000000000 ) ) ;
#12303 = CARTESIAN_POINT ( 'NONE',  ( 164.8271680874279923, 246.4386526519062102, -4.335244565372774694 ) ) ;
#12305 = CARTESIAN_POINT ( 'NONE',  ( 153.1314981037513121, 265.4154603756023789, 17.73969815997475408 ) ) ;
#12306 = VERTEX_POINT ( 'NONE', #76300 ) ;
#12307 = CARTESIAN_POINT ( 'NONE',  ( 80.53198101875031512, 57.77087603849956565, 16.24514743536724026 ) ) ;
#12308 = CARTESIAN_POINT ( 'NONE',  ( 174.3163775853039965, 262.5928350672832607, 14.99201191324070948 ) ) ;
#12309 = ORIENTED_EDGE ( 'NONE', *, *, #85833, .F. ) ;
#12310 = CARTESIAN_POINT ( 'NONE',  ( 87.65912690667771301, 45.19743498868427167, -6.201137598350706881 ) ) ;
#12311 = CARTESIAN_POINT ( 'NONE',  ( 76.55480823776410659, 226.5530062829863027, -4.648177544792955347E-16 ) ) ;
#12312 = VERTEX_POINT ( 'NONE', #82450 ) ;
#12313 = CARTESIAN_POINT ( 'NONE',  ( 51.80235952159636525, 85.00000000000000000, 59.99999999999999289 ) ) ;
#12314 = CARTESIAN_POINT ( 'NONE',  ( 167.5922211047578401, 275.0307474144973980, -15.21854255687822999 ) ) ;
#12315 = CARTESIAN_POINT ( 'NONE',  ( 73.65586519493432149, 59.54601760613143568, 15.54039508984885565 ) ) ;
#12316 = ORIENTED_EDGE ( 'NONE', *, *, #97480, .T. ) ;
#12317 = CARTESIAN_POINT ( 'NONE',  ( 177.5270958125545064, 279.1683514342866488, -16.05247689478367690 ) ) ;
#12318 = CARTESIAN_POINT ( 'NONE',  ( 168.9651915494897878, 261.4198009647504932, -16.16106606682127023 ) ) ;
#12319 = ORIENTED_EDGE ( 'NONE', *, *, #67961, .F. ) ;
#12320 = CARTESIAN_POINT ( 'NONE',  ( 75.25170673533752108, 66.73598490943447814, 12.94887977284632896 ) ) ;
#12321 = VECTOR ( 'NONE', #60423, 1000.000000000000114 ) ;
#12322 = VERTEX_POINT ( 'NONE', #6872 ) ;
#12323 = DIRECTION ( 'NONE',  ( -0.000000000000000000, -0.000000000000000000, -1.000000000000000000 ) ) ;
#12324 = ORIENTED_EDGE ( 'NONE', *, *, #57378, .T. ) ;
#12325 =( BOUNDED_CURVE ( )  B_SPLINE_CURVE ( 2, ( #18460, #65536, #64548, #50828, #12352, #35635, #28031, #17963, #48860 ),
 .UNSPECIFIED., .F., .T. ) 
 B_SPLINE_CURVE_WITH_KNOTS ( ( 3, 2, 2, 2, 3 ),
 ( 0.4314516129032258118, 0.4327956989247311870, 0.4354838709677419373, 0.4381720430107526876, 0.4395161290322580627 ),
 .UNSPECIFIED. ) 
 CURVE ( )  GEOMETRIC_REPRESENTATION_ITEM ( )  RATIONAL_B_SPLINE_CURVE ( ( 0.9330127018922194093, 0.9330127018922194093, 1.000000000000000000, 0.8660254037844387076, 1.000000000000000000, 0.8660254037844387076, 1.000000000000000000, 0.9330127018922194093, 0.9330127018922194093 ) ) 
 REPRESENTATION_ITEM ( '' )  );
#12326 = LINE ( 'NONE', #71643, #64218 ) ;
#12327 = CARTESIAN_POINT ( 'NONE',  ( -71.45866285464214229, 45.60329508610311677, -10.00000000000000000 ) ) ;
#12328 = DIRECTION ( 'NONE',  ( 0.000000000000000000, -0.000000000000000000, -1.000000000000000000 ) ) ;
#12329 = DIRECTION ( 'NONE',  ( -0.9172102815912979157, -0.3984034379159046013, 0.000000000000000000 ) ) ;
#12330 = CARTESIAN_POINT ( 'NONE',  ( 157.5215017335775940, 258.4853116787141971, -16.92298772477023761 ) ) ;
#12331 = CARTESIAN_POINT ( 'NONE',  ( 178.1054448038686076, 292.3333982356375600, 7.160286041890884690 ) ) ;
#12332 = CARTESIAN_POINT ( 'NONE',  ( 158.5163285992952922, 256.0886603671742705, -16.16665996632518798 ) ) ;
#12333 = ORIENTED_EDGE ( 'NONE', *, *, #93576, .F. ) ;
#12334 = CARTESIAN_POINT ( 'NONE',  ( 80.48057461997055384, 55.60742216994913889, -16.06452287015007840 ) ) ;
#12335 = CARTESIAN_POINT ( 'NONE',  ( 164.9356397357043704, 244.9700873293209042, 2.799217332519396972 ) ) ;
#12337 = CARTESIAN_POINT ( 'NONE',  ( 164.8616299252405213, 245.0982760813026857, 1.544363874765093625 ) ) ;
#12336 = CARTESIAN_POINT ( 'NONE',  ( 196.5475899070771675, 290.2165835061676944, -17.89382743182097002 ) ) ;
#12339 = ORIENTED_EDGE ( 'NONE', *, *, #3999, .F. ) ;
#12338 = CARTESIAN_POINT ( 'NONE',  ( 198.4706398937704819, 286.8857632237200619, 17.04020736381253798 ) ) ;
#12340 = ORIENTED_EDGE ( 'NONE', *, *, #35836, .F. ) ;
#12341 = CARTESIAN_POINT ( 'NONE',  ( 146.6710848822482660, 276.6052243131355226, -3.256337828262574785 ) ) ;
#12342 = DIRECTION ( 'NONE',  ( -0.000000000000000000, -0.000000000000000000, -1.000000000000000000 ) ) ;
#12343 = DIRECTION ( 'NONE',  ( 0.8660254037844390407, 0.4999999999999992228, -0.000000000000000000 ) ) ;
#12344 = CARTESIAN_POINT ( 'NONE',  ( 118.1240276194171770, 250.5530062829863311, -4.648177544792955347E-16 ) ) ;
#12345 = EDGE_CURVE ( 'NONE', #47438, #82969, #95518, .T. ) ;
#12346 = CARTESIAN_POINT ( 'NONE',  ( 159.8797902884228392, 253.7270754474314458, -15.26054831571763160 ) ) ;
#12347 = EDGE_CURVE ( 'NONE', #90262, #5319, #83469, .T. ) ;
#12348 = CARTESIAN_POINT ( 'NONE',  ( 189.9902393611022546, 301.5742478148356440, 0.007239494267619051016 ) ) ;
#12349 = ORIENTED_EDGE ( 'NONE', *, *, #29235, .T. ) ;
#12350 = CARTESIAN_POINT ( 'NONE',  ( 170.5099130517262722, 255.7343107893726994, -11.93865830361121816 ) ) ;
#12351 = FACE_OUTER_BOUND ( 'NONE', #5807, .T. ) ;
#12352 = CARTESIAN_POINT ( 'NONE',  ( 56.38594494382682853, 203.3615022471902307, -10.00000000000009592 ) ) ;
#12353 = ADVANCED_FACE ( 'NONE', ( #74321 ), #37763, .T. ) ;
#12354 = DIRECTION ( 'NONE',  ( -0.8660254037844387076, -0.4999999999999998890, -0.000000000000000000 ) ) ;
#12355 = EDGE_CURVE ( 'NONE', #71997, #32616, #8099, .T. ) ;
#12356 = CARTESIAN_POINT ( 'NONE',  ( 20.28351092001508960, 192.5177522451419350, 5.000000000000046185 ) ) ;
#12357 = CARTESIAN_POINT ( 'NONE',  ( 108.2124997955428967, 221.0327760586659451, 1.948934522072302763E-15 ) ) ;
#12358 = CARTESIAN_POINT ( 'NONE',  ( 162.1227137712282342, 251.8422180177273901, -14.11218862277787345 ) ) ;
#12359 = CARTESIAN_POINT ( 'NONE',  ( 162.6150040737615257, 249.4375296638992268, -10.77107874254045505 ) ) ;
#12360 = CARTESIAN_POINT ( 'NONE',  ( 96.20275958967147290, 237.8967562850346837, -4.648177544792955347E-16 ) ) ;
#12361 = CARTESIAN_POINT ( 'NONE',  ( 171.3649617487770911, 251.0102673366500596, 7.372720983288576946 ) ) ;
#12362 = CARTESIAN_POINT ( 'NONE',  ( 28.21305602519035460, 187.0958772461660544, -9.188101187500095079 ) ) ;
#12363 = VECTOR ( 'NONE', #69757, 1000.000000000000000 ) ;
#12364 = DIRECTION ( 'NONE',  ( -0.8660254037844387076, -0.4999999999999998890, -0.000000000000000000 ) ) ;
#12365 = ORIENTED_EDGE ( 'NONE', *, *, #30617, .T. ) ;
#12366 = AXIS2_PLACEMENT_3D ( 'NONE', #3495, #66762, #58648 ) ;
#12367 = ORIENTED_EDGE ( 'NONE', *, *, #45328, .T. ) ;
#12368 = CARTESIAN_POINT ( 'NONE',  ( 142.9371257517045137, 259.7655487066560340, -7.305945665944389766 ) ) ;
#12369 = CARTESIAN_POINT ( 'NONE',  ( 74.45055738859878147, 68.30939989315471905, -11.41140116448488051 ) ) ;
#12370 = CARTESIAN_POINT ( 'NONE',  ( 74.23286061265172009, 64.97622957471450889, 14.08197172241813888 ) ) ;
#12371 = AXIS2_PLACEMENT_3D ( 'NONE', #30121, #45800, #15913 ) ;
#12372 = CARTESIAN_POINT ( 'NONE',  ( -19.65312891409030271, 93.06504152958497400, 10.00000000000000888 ) ) ;
#12373 = CARTESIAN_POINT ( 'NONE',  ( -22.42236680055709641, 157.8615022471902591, 0.000000000000000000 ) ) ;
#12374 = CARTESIAN_POINT ( 'NONE',  ( 176.1793590593251224, 285.1801416094290289, -12.37630502171867697 ) ) ;
#12375 = CARTESIAN_POINT ( 'NONE',  ( 67.00187114335926708, 67.08813303282481399, 8.529924657355552498 ) ) ;
#12376 = CARTESIAN_POINT ( 'NONE',  ( 55.46605327235566563, 193.6423013555410080, -4.594050593750043987 ) ) ;
#12377 = CARTESIAN_POINT ( 'NONE',  ( 89.49337443912149581, 229.1427522451419065, 10.00000000000009237 ) ) ;
#12378 = ORIENTED_EDGE ( 'NONE', *, *, #15660, .T. ) ;
#12379 = CARTESIAN_POINT ( 'NONE',  ( 196.5569465129259186, 267.2703004868020003, -7.811843761257617480 ) ) ;
#12380 = CYLINDRICAL_SURFACE ( 'NONE', #84138, 10.00000000000010658 ) ;
#12381 = CARTESIAN_POINT ( 'NONE',  ( 208.3829315663354862, 269.7171704273955015, -1.768817828503133072 ) ) ;
#12382 = VECTOR ( 'NONE', #27918, 1000.000000000000114 ) ;
#12383 = CARTESIAN_POINT ( 'NONE',  ( -9.405095999578703569, 171.5024278399160949, 9.188101187500095079 ) ) ;
#12384 = CARTESIAN_POINT ( 'NONE',  ( 198.8194531333411419, 286.2816009704309863, -17.01510935557533344 ) ) ;
#12385 = VECTOR ( 'NONE', #55762, 1000.000000000000000 ) ;
#12386 = DIRECTION ( 'NONE',  ( 0.4999999999999998890, -0.8660254037844385966, 0.000000000000000000 ) ) ;
#12387 = CARTESIAN_POINT ( 'NONE',  ( 192.9633865298379476, 296.4246058602058156, -11.85717392250713864 ) ) ;
#12388 = CARTESIAN_POINT ( 'NONE',  ( 71.72631157091053922, 72.05082354862287275, -1.633393872038913175 ) ) ;
#12389 = CARTESIAN_POINT ( 'NONE',  ( 49.48463145776311478, 205.5024278399160949, -9.188101187500093303 ) ) ;
#12390 = CARTESIAN_POINT ( 'NONE',  ( 164.0854748117396582, 246.4426161724408928, -5.757837433625331514 ) ) ;
#12391 = CARTESIAN_POINT ( 'NONE',  ( 72.52093223241688236, 57.39944909060013600, 16.31544603362117485 ) ) ;
#12392 = CARTESIAN_POINT ( 'NONE',  ( 69.57879208480075306, 68.94139417373898482, 7.052474478442530170 ) ) ;
#12393 = CARTESIAN_POINT ( 'NONE',  ( -19.65312891409030271, 93.06504152958497400, -10.00000000000000888 ) ) ;
#12394 = ORIENTED_EDGE ( 'NONE', *, *, #61621, .T. ) ;
#12395 = CARTESIAN_POINT ( 'NONE',  ( 5.723458822437168081, 174.1115022471902591, 10.00000000000009592 ) ) ;
#12396 = CARTESIAN_POINT ( 'NONE',  ( 82.28662647995521695, 41.83953847820645677, 6.586483578078058621 ) ) ;
#12397 = CARTESIAN_POINT ( 'NONE',  ( 115.9249311304092771, 246.9244531367911293, -4.594050593750046652 ) ) ;
#12398 = CARTESIAN_POINT ( 'NONE',  ( 18.31869600479030424, 33.68290643055186706, 3.479690158560446702E-15 ) ) ;
#12399 = CARTESIAN_POINT ( 'NONE',  ( 171.3751619920873281, 280.2398791927632828, 15.33202389549764888 ) ) ;
#12400 = CARTESIAN_POINT ( 'NONE',  ( 45.39824762976388683, 187.0177522451417929, 5.000000000000051514 ) ) ;
#12401 = EDGE_CURVE ( 'NONE', #47755, #60445, #37275, .T. ) ;
#12403 = CARTESIAN_POINT ( 'NONE',  ( 187.4983404922351156, 288.8742233168966891, 14.46822738816536358 ) ) ;
#12402 = CARTESIAN_POINT ( 'NONE',  ( 157.2744851780909414, 258.2395962677452985, 18.17792129701959070 ) ) ;
#12404 = CARTESIAN_POINT ( 'NONE',  ( 11.67130034620459256, 30.23654200823201776, 1.583844403245363353 ) ) ;
#12405 = EDGE_LOOP ( 'NONE', ( #95406, #7945, #89412, #68964 ) ) ;
#12406 = CARTESIAN_POINT ( 'NONE',  ( 191.5766842709549280, 298.8264446275616137, 8.039910086100929831 ) ) ;
#12407 = CARTESIAN_POINT ( 'NONE',  ( 163.4933893861717706, 247.4681382119453588, 7.531590497957860286 ) ) ;
#12408 = EDGE_CURVE ( 'NONE', #99455, #88304, #37472, .T. ) ;
#12409 = CARTESIAN_POINT ( 'NONE',  ( 82.12550757349835351, 41.17588303117550907, -3.464665208087097437 ) ) ;
#12410 = CARTESIAN_POINT ( 'NONE',  ( 172.9301907270271954, 268.1031614781803114, -16.30088698181723927 ) ) ;
#12411 = CARTESIAN_POINT ( 'NONE',  ( 47.32807415326522715, 108.5480133836684900, -10.00000000000000000 ) ) ;
#12412 = EDGE_LOOP ( 'NONE', ( #93334, #99067, #49693, #28617 ) ) ;
#12413 = CARTESIAN_POINT ( 'NONE',  ( 68.69386498186378276, 66.37052439002927429, 9.851853166250990057 ) ) ;
#12414 = CARTESIAN_POINT ( 'NONE',  ( 170.6697357073235253, 284.5009364175209043, -11.68571669126542822 ) ) ;
#12415 = CARTESIAN_POINT ( 'NONE',  ( 71.88106639363309114, 72.58558382077731608, 1.103795272596851174 ) ) ;
#12416 = CARTESIAN_POINT ( 'NONE',  ( 83.70208412440790369, 42.60878222363336931, 5.172964853322376655 ) ) ;
#12417 = CARTESIAN_POINT ( 'NONE',  ( 196.2233686317883326, 270.8944000944912887, 13.08481226931415442 ) ) ;
#12418 = CARTESIAN_POINT ( 'NONE',  ( 185.1111192456979211, 296.2605552703855096, 4.659568135049322990 ) ) ;
#12419 = CARTESIAN_POINT ( 'NONE',  ( -74.22192597045216189, 49.22161114575668250, -10.00000000000000000 ) ) ;
#12420 = CARTESIAN_POINT ( 'NONE',  ( 148.4964438259718520, 274.1392353305065512, -7.906637339856966484 ) ) ;
#12421 = CARTESIAN_POINT ( 'NONE',  ( 10.37514450368026786, 11.15404122711131407, 8.090169943749479842 ) ) ;
#12422 = LINE ( 'NONE', #75219, #44874 ) ;
#12423 = ORIENTED_EDGE ( 'NONE', *, *, #9942, .F. ) ;
#12424 = DIRECTION ( 'NONE',  ( 0.000000000000000000, 0.000000000000000000, 1.000000000000000000 ) ) ;
#12425 = ADVANCED_FACE ( 'NONE', ( #21589 ), #48592, .F. ) ;
#12426 = CARTESIAN_POINT ( 'NONE',  ( 147.6264044922760377, 274.9505622111005323, -8.841872555777701592 ) ) ;
#12427 = CARTESIAN_POINT ( 'NONE',  ( 156.1012082241142309, 261.7660268653759772, -17.00573470575184487 ) ) ;
#12428 = VERTEX_POINT ( 'NONE', #38761 ) ;
#12429 = LINE ( 'NONE', #53394, #94437 ) ;
#12430 = CARTESIAN_POINT ( 'NONE',  ( 185.4183139185963967, 291.0678344243584093, 12.11208453829537213 ) ) ;
#12431 = CARTESIAN_POINT ( 'NONE',  ( 204.7610021263893429, 275.9905362388115577, 13.36619428527026976 ) ) ;
#12432 = CARTESIAN_POINT ( 'NONE',  ( 20.30386484825465132, 170.9824982072973967, 3.021315404115420679E-15 ) ) ;
#12433 = VECTOR ( 'NONE', #79439, 1000.000000000000000 ) ;
#12434 = CARTESIAN_POINT ( 'NONE',  ( -55.59287931351117606, 32.99562883703961091, 10.00000000000000000 ) ) ;
#12435 = ORIENTED_EDGE ( 'NONE', *, *, #58313, .F. ) ;
#12436 = CARTESIAN_POINT ( 'NONE',  ( 85.53328598605538957, 214.0643266524159856, -9.188101187500093303 ) ) ;
#12437 = CARTESIAN_POINT ( 'NONE',  ( 155.1411698516235163, 261.9346068017520679, 17.17606690776768374 ) ) ;
#12438 = DIRECTION ( 'NONE',  ( -0.9778746070300391446, 0.2091919045418505763, 0.000000000000000000 ) ) ;
#12439 = CARTESIAN_POINT ( 'NONE',  ( 81.45273407654831033, 41.92911449342699370, -7.602784365630077978 ) ) ;
#12440 = ORIENTED_EDGE ( 'NONE', *, *, #94458, .T. ) ;
#12441 = ORIENTED_EDGE ( 'NONE', *, *, #90113, .F. ) ;
#12443 = CIRCLE ( 'NONE', #65781, 0.1418229129680854683 ) ;
#12442 = CARTESIAN_POINT ( 'NONE',  ( 207.1906716859447499, 270.1669981132436078, 1.693978511116863261 ) ) ;
#12444 = ORIENTED_EDGE ( 'NONE', *, *, #30036, .F. ) ;
#12445 = CARTESIAN_POINT ( 'NONE',  ( 76.90683638624993534, 49.81317808655190049, 15.10818565773490008 ) ) ;
#12446 = ORIENTED_EDGE ( 'NONE', *, *, #12012, .F. ) ;
#12447 = CARTESIAN_POINT ( 'NONE',  ( 75.95776633494669738, 63.62874501809822902, 14.74263889421621698 ) ) ;
#12448 = CARTESIAN_POINT ( 'NONE',  ( 202.8535267948003593, 279.2943804273081696, -15.36804658072946062 ) ) ;
#12449 = VERTEX_POINT ( 'NONE', #63568 ) ;
#12450 = CARTESIAN_POINT ( 'NONE',  ( 182.7578341729287104, 280.0865842805126249, -16.17247614028536873 ) ) ;
#12451 = CARTESIAN_POINT ( 'NONE',  ( 82.18687726816486361, 41.15680977039290411, 3.242629060634906857 ) ) ;
#12452 = CARTESIAN_POINT ( 'NONE',  ( 152.1671311979278016, 269.0857928536317445, 15.36489295260887822 ) ) ;
#12453 = CARTESIAN_POINT ( 'NONE',  ( 200.9061540366740246, 282.6673289856585143, -18.13083321883407351 ) ) ;
#12454 = CYLINDRICAL_SURFACE ( 'NONE', #56583, 10.00000000000001066 ) ;
#12455 = CARTESIAN_POINT ( 'NONE',  ( 22.27692774695706035, 28.56454794089042082, 10.00000000000000355 ) ) ;
#12456 = CARTESIAN_POINT ( 'NONE',  ( 138.9828575061699496, 260.2369531367911009, -4.594050593750048428 ) ) ;
#12457 = CARTESIAN_POINT ( 'NONE',  ( 156.8640796903996488, 258.9504394241315595, -18.30920512684366841 ) ) ;
#12458 = VERTEX_POINT ( 'NONE', #69665 ) ;
#12459 = FACE_OUTER_BOUND ( 'NONE', #11848, .T. ) ;
#12460 = CARTESIAN_POINT ( 'NONE',  ( 12.55777956335723644, 9.111106405272902720, -2.839279412974138328 ) ) ;
#12461 = ORIENTED_EDGE ( 'NONE', *, *, #98481, .F. ) ;
#12462 = CARTESIAN_POINT ( 'NONE',  ( 160.5893190321802138, 270.9897182155185078, 16.60663562724527864 ) ) ;
#12464 = ORIENTED_EDGE ( 'NONE', *, *, #55315, .T. ) ;
#12463 = CARTESIAN_POINT ( 'NONE',  ( 200.1100745001128303, 270.2489798220258308, 9.265985437337555197 ) ) ;
#12465 = AXIS2_PLACEMENT_3D ( 'NONE', #81145, #48194, #9723 ) ;
#12466 = CARTESIAN_POINT ( 'NONE',  ( -15.24570502058241139, 105.6897125274499842, 11.06526020485377160 ) ) ;
#12467 = CARTESIAN_POINT ( 'NONE',  ( -19.65312891409030271, 93.06504152958497400, 10.00000000000000888 ) ) ;
#12468 = CARTESIAN_POINT ( 'NONE',  ( 76.24546156567440391, 64.85285070271640961, -14.33378511211777706 ) ) ;
#12469 = CARTESIAN_POINT ( 'NONE',  ( 160.0293279782301568, 280.7546693694226860, -6.628616199906209872 ) ) ;
#12470 = DIRECTION ( 'NONE',  ( 0.000000000000000000, 0.000000000000000000, 1.000000000000000000 ) ) ;
#12471 = AXIS2_PLACEMENT_3D ( 'NONE', #73848, #58618, #28739 ) ;
#12473 = CYLINDRICAL_SURFACE ( 'NONE', #44723, 1.449999999999993072 ) ;
#12472 = B_SPLINE_CURVE_WITH_KNOTS ( 'NONE', 3,
 ( #84240, #69976, #14299, #99905, #29495, #68981, #54779, #21890, #29988, #38580, #91830, #6697, #77085, #92821, #91329, #78102, #45185, #22392, #46164, #37090, #30490, #22882, #54262, #37575, #100, #14789, #68483, #53768, #53288, #30984, #590, #67994, #60372, #52776, #7689, #76596, #84730, #38067, #15270, #61870, #85232, #15778, #46684 ),
 .UNSPECIFIED., .F., .F.,
 ( 4, 2, 2, 2, 2, 1, 2, 2, 2, 2, 2, 2, 2, 2, 2, 2, 2, 2, 2, 2, 2, 4 ),
 ( 0.02141244383927110029, 0.02208092004936386410, 0.02274939625945662791, 0.02408634867964215207, 0.02475482488973493669, 0.02542330109982772132, 0.02609177730992050595, 0.02676025352001328711, 0.02809720594019887718, 0.02876568215029168263, 0.02943415836038448807, 0.03077111078057008509, 0.03210806320075568210, 0.03277653941084848060, 0.03344501562094127911, 0.03478196804112686225, 0.03611892046131245232, 0.03745587288149804239, 0.03879282530168363247, 0.04012977772186922254, 0.04146673014205480567, 0.04280368256224039575 ),
 .UNSPECIFIED. ) ;
#12474 = CARTESIAN_POINT ( 'NONE',  ( 84.31620252596033538, 42.01387254285906891, 1.014253996708007088 ) ) ;
#12475 = CARTESIAN_POINT ( 'NONE',  ( 194.6016098382413873, 292.7469416705026788, 15.11077049397369976 ) ) ;
#12476 = EDGE_LOOP ( 'NONE', ( #12997, #60780, #7426 ) ) ;
#12477 = CARTESIAN_POINT ( 'NONE',  ( 184.6983412747724742, 272.9958233129013934, -16.41604421047053464 ) ) ;
#12478 = CARTESIAN_POINT ( 'NONE',  ( 65.98821791718346219, 68.67660198893013046, -0.1386984857929180193 ) ) ;
#12479 = ORIENTED_EDGE ( 'NONE', *, *, #17236, .F. ) ;
#12480 = CARTESIAN_POINT ( 'NONE',  ( 160.0377410834880720, 276.7385967903648520, 13.05697007622473294 ) ) ;
#12481 = EDGE_CURVE ( 'NONE', #33383, #58141, #77793, .T. ) ;
#12482 = B_SPLINE_CURVE_WITH_KNOTS ( 'NONE', 3,
 ( #50178, #11699, #50664, #26391 ),
 .UNSPECIFIED., .F., .F.,
 ( 4, 4 ),
 ( 0.01264251196720198728, 0.01893505409154686361 ),
 .UNSPECIFIED. ) ;
#12483 = CARTESIAN_POINT ( 'NONE',  ( 156.7047097395129924, 276.7985503127216020, 10.01792283833032648 ) ) ;
#12484 = CARTESIAN_POINT ( 'NONE',  ( 204.2264919259983174, 276.9163350630529976, -14.79221891897802799 ) ) ;
#12485 = CARTESIAN_POINT ( 'NONE',  ( 81.40384678758614712, 44.82616229828595777, -10.53103118534553850 ) ) ;
#12486 = DIRECTION ( 'NONE',  ( -0.000000000000000000, -0.000000000000000000, -1.000000000000000000 ) ) ;
#12488 = CARTESIAN_POINT ( 'NONE',  ( 88.42823867725131493, 44.01048851461693090, 2.280060627005664919 ) ) ;
#12487 = CARTESIAN_POINT ( 'NONE',  ( 1.396987757676521058, 24.30466486950695071, 1.224646799147354045E-15 ) ) ;
#12489 = CARTESIAN_POINT ( 'NONE',  ( 203.4034827258358007, 270.0124503379752241, 5.894888531434947510 ) ) ;
#12490 = ORIENTED_EDGE ( 'NONE', *, *, #73839, .F. ) ;
#12491 = ORIENTED_EDGE ( 'NONE', *, *, #38803, .F. ) ;
#12492 = DIRECTION ( 'NONE',  ( -0.9979398670145497308, -0.06415622980648832963, 0.000000000000000000 ) ) ;
#12493 = CARTESIAN_POINT ( 'NONE',  ( 80.17588645533830061, 58.12694466101720536, 16.26593623338475680 ) ) ;
#12494 = CARTESIAN_POINT ( 'NONE',  ( 85.73351810911900373, 48.76173041439603395, -12.45270611261531180 ) ) ;
#12495 = CARTESIAN_POINT ( 'NONE',  ( 175.3447835617839985, 290.8124204970986284, 2.566043682277154847 ) ) ;
#12496 = CARTESIAN_POINT ( 'NONE',  ( 192.4454213697443095, 297.3217478340386606, 12.58566886711101596 ) ) ;
#12497 = CARTESIAN_POINT ( 'NONE',  ( 81.03047946496111820, 43.68561371680597460, -9.505511175303684723 ) ) ;
#12498 = DIRECTION ( 'NONE',  ( -0.9086904199442051855, 0.4174706225611858335, 0.000000000000000000 ) ) ;
#12499 = CARTESIAN_POINT ( 'NONE',  ( 8.700681467995980967, 166.6423013555410080, -4.594050593750043987 ) ) ;
#12500 = CARTESIAN_POINT ( 'NONE',  ( 100.0117143358702236, 237.7369531367911009, -4.594050593750048428 ) ) ;
#12501 = CARTESIAN_POINT ( 'NONE',  ( 87.84569706029115821, 44.18597558567909545, -4.425511980624551533 ) ) ;
#12502 = CARTESIAN_POINT ( 'NONE',  ( 179.9032037953561201, 255.0686240464731895, -2.409017592585954937 ) ) ;
#12503 = CARTESIAN_POINT ( 'NONE',  ( 78.42722165381930211, 53.22649076314601047, 15.78604470347753264 ) ) ;
#12504 = CARTESIAN_POINT ( 'NONE',  ( 75.92491905781218975, 51.44142931567759547, 15.68752148852608741 ) ) ;
#12505 = VECTOR ( 'NONE', #57517, 1000.000000000000000 ) ;
#12506 = DIRECTION ( 'NONE',  ( -0.8660254037844387076, -0.4999999999999998890, -0.000000000000000000 ) ) ;
#12507 = CARTESIAN_POINT ( 'NONE',  ( 147.7112127936102866, 274.8036699242858276, -9.124700685424272706 ) ) ;
#12508 = CARTESIAN_POINT ( 'NONE',  ( 84.17379491356786048, 50.54589666422514682, 13.76883155557667138 ) ) ;
#12509 = CARTESIAN_POINT ( 'NONE',  ( 196.5044318023951178, 266.6999416850621287, 8.135797318270522993 ) ) ;
#12510 = PLANE ( 'NONE',  #52920 ) ;
#12511 = CARTESIAN_POINT ( 'NONE',  ( 162.3863246888976732, 251.8997027923403493, -12.94925132143062463 ) ) ;
#12512 = VECTOR ( 'NONE', #75516, 1000.000000000000000 ) ;
#12513 = CARTESIAN_POINT ( 'NONE',  ( 172.7048577836360721, 263.2835701223090155, -15.44053096649166079 ) ) ;
#12514 = CARTESIAN_POINT ( 'NONE',  ( 73.24602992621615272, 225.3464784336661353, 1.353441290958777327E-15 ) ) ;
#12515 = CARTESIAN_POINT ( 'NONE',  ( 10.26584248093601737, 14.43085787977761036, -9.188101187500008038 ) ) ;
#12516 = CARTESIAN_POINT ( 'NONE',  ( 151.4025156491502742, 268.4101458323662541, 14.71049357081981235 ) ) ;
#12517 = CARTESIAN_POINT ( 'NONE',  ( -14.03049543618944206, 103.5316844796765565, 11.08926661400182390 ) ) ;
#12519 = CARTESIAN_POINT ( 'NONE',  ( 86.30629612394095318, 43.10717986221388998, -0.8733839489286622237 ) ) ;
#12518 = CARTESIAN_POINT ( 'NONE',  ( 157.8849654228661166, 257.1822134667773980, 17.43614750057631468 ) ) ;
#12520 = CARTESIAN_POINT ( 'NONE',  ( 148.9874996956617395, 272.5930761648982070, 12.54755420039906078 ) ) ;
#12521 = CARTESIAN_POINT ( 'NONE',  ( 198.9590707264871412, 286.0397762054715827, -17.05306195936250191 ) ) ;
#12522 = LINE ( 'NONE', #36296, #96382 ) ;
#12523 = EDGE_CURVE ( 'NONE', #55246, #25048, #764, .T. ) ;
#12524 = CARTESIAN_POINT ( 'NONE',  ( 32.31339950491288704, 36.84336893147758474, -7.433330006724137462 ) ) ;
#12525 = CARTESIAN_POINT ( 'NONE',  ( 192.8301672656986341, 296.6553483942417415, -13.40355799340913556 ) ) ;
#12526 = EDGE_LOOP ( 'NONE', ( #95712, #7454, #98687, #6585 ) ) ;
#12527 = CARTESIAN_POINT ( 'NONE',  ( 25.24326406500046360, 20.28920272979927475, -7.433330006724141015 ) ) ;
#12528 = AXIS2_PLACEMENT_3D ( 'NONE', #726, #78749, #31612 ) ;
#12529 = CARTESIAN_POINT ( 'NONE',  ( 7.350711452622367581, 26.01751292744054567, 6.180339887498949913 ) ) ;
#12530 = CARTESIAN_POINT ( 'NONE',  ( 146.9129474150286683, 276.1863061179126930, -5.016087650759920358 ) ) ;
#12531 = CARTESIAN_POINT ( 'NONE',  ( 188.1389331190833047, 286.0020158130019468, -16.24451441855859102 ) ) ;
#12532 = CARTESIAN_POINT ( 'NONE',  ( 70.99214533039287289, 61.07251846123117645, 14.51118677859261119 ) ) ;
#12533 = DIRECTION ( 'NONE',  ( 0.5011331959107180323, 0.8653701635463924013, 0.000000000000000000 ) ) ;
#12534 = CARTESIAN_POINT ( 'NONE',  ( 155.2602186481262265, 267.5823991184574879, 15.87441468340182382 ) ) ;
#12535 = CARTESIAN_POINT ( 'NONE',  ( -19.65312891409030271, 93.06504152958497400, 59.99999999999999289 ) ) ;
#12536 = CARTESIAN_POINT ( 'NONE',  ( 144.7927049134883077, 247.7365022471901739, -10.00000000000009059 ) ) ;
#12537 = CARTESIAN_POINT ( 'NONE',  ( 17.41480177352709191, 180.8615022471902591, -10.00000000000009592 ) ) ;
#12539 = VECTOR ( 'NONE', #1673, 1000.000000000000114 ) ;
#12538 = CARTESIAN_POINT ( 'NONE',  ( 75.32443696912777398, 53.39185654545678972, 16.03229517472230370 ) ) ;
#12540 = ORIENTED_EDGE ( 'NONE', *, *, #32497, .T. ) ;
#12541 = CARTESIAN_POINT ( 'NONE',  ( 191.1126307253469747, 299.2020206802192206, -6.759625617318037349 ) ) ;
#12542 = CARTESIAN_POINT ( 'NONE',  ( 169.5007657120409874, 248.2156828994837099, -1.963647642838588503 ) ) ;
#12543 = VERTEX_POINT ( 'NONE', #16466 ) ;
#12544 = CARTESIAN_POINT ( 'NONE',  ( 196.9385840439278752, 265.2769846543552035, -4.547345364390803724 ) ) ;
#12545 = CARTESIAN_POINT ( 'NONE',  ( 83.77213608728635563, 41.72335732820068444, 1.354266426187002992 ) ) ;
#12546 = ADVANCED_FACE ( 'NONE', ( #47362 ), #1664, .T. ) ;
#12547 = ORIENTED_EDGE ( 'NONE', *, *, #33282, .F. ) ;
#12548 = DIRECTION ( 'NONE',  ( -0.6141984594095433181, -0.7891516029629183082, 0.000000000000000000 ) ) ;
#12549 = ORIENTED_EDGE ( 'NONE', *, *, #48077, .F. ) ;
#12550 = CARTESIAN_POINT ( 'NONE',  ( 72.01291228344958029, 71.60916324447191528, 5.531298035833710713 ) ) ;
#12551 = CARTESIAN_POINT ( 'NONE',  ( 158.3546312691470348, 256.3687283584388865, 16.55374228798595126 ) ) ;
#12552 = DIRECTION ( 'NONE',  ( -0.5000000000000002220, 0.8660254037844384856, 0.000000000000000000 ) ) ;
#12553 = CARTESIAN_POINT ( 'NONE',  ( 204.1541407990405332, 272.6956988606675623, 11.22829397770025395 ) ) ;
#12554 = CARTESIAN_POINT ( 'NONE',  ( 153.2906404175950854, 265.1398178023911782, -17.60231834963988007 ) ) ;
#12555 = FACE_OUTER_BOUND ( 'NONE', #50155, .T. ) ;
#12556 = CARTESIAN_POINT ( 'NONE',  ( 26.01788259378743362, 35.99752408145593563, 5.678558825948276656 ) ) ;
#12557 = CARTESIAN_POINT ( 'NONE',  ( 74.51118135615443805, 60.14921420329969948, -15.52886586986496376 ) ) ;
#12558 = CARTESIAN_POINT ( 'NONE',  ( 164.6179597924970039, 274.5158082661938579, 14.71820543651746327 ) ) ;
#12559 = ADVANCED_FACE ( 'NONE', ( #40751 ), #56957, .T. ) ;
#12560 = CARTESIAN_POINT ( 'NONE',  ( 189.6662795060866529, 300.6105458049610775, 0.3572493495538390240 ) ) ;
#12561 = ORIENTED_EDGE ( 'NONE', *, *, #34818, .T. ) ;
#12562 = ORIENTED_EDGE ( 'NONE', *, *, #15192, .T. ) ;
#12563 = CARTESIAN_POINT ( 'NONE',  ( 182.8792571200491750, 296.1546806419740960, 0.3348460080343949041 ) ) ;
#12565 = CARTESIAN_POINT ( 'NONE',  ( 165.9605670965306672, 274.2117924623952376, -15.14287719899917661 ) ) ;
#12564 = CARTESIAN_POINT ( 'NONE',  ( 68.10490905690869567, 65.76241361189985923, 10.87691428392215620 ) ) ;
#12566 = CARTESIAN_POINT ( 'NONE',  ( 85.71893696364587356, 48.44430998916941178, -11.74445541149036742 ) ) ;
#12567 = CARTESIAN_POINT ( 'NONE',  ( 19.16720650933548953, 170.3262482093457777, 3.021315404115420679E-15 ) ) ;
#12568 = CARTESIAN_POINT ( 'NONE',  ( 156.5981606942930853, 279.2183417136616868, -8.654364236849055203 ) ) ;
#12569 = CARTESIAN_POINT ( 'NONE',  ( 82.08088010363431408, 40.77644816011592610, 1.343812065088729302 ) ) ;
#12570 = CARTESIAN_POINT ( 'NONE',  ( 167.3807934234146160, 286.2060637682922675, -4.770210317880093420 ) ) ;
#12571 = CARTESIAN_POINT ( 'NONE',  ( 48.95103868752454446, 97.61288834769685252, -10.00000000000000000 ) ) ;
#12572 = CARTESIAN_POINT ( 'NONE',  ( 7.864685750751951865, 30.05722773587472929, -10.00000000000000000 ) ) ;
#12573 = CARTESIAN_POINT ( 'NONE',  ( 98.87557663705065636, 218.7048013555409796, 4.594050593750051981 ) ) ;
#12574 = ORIENTED_EDGE ( 'NONE', *, *, #41613, .T. ) ;
#12575 = CARTESIAN_POINT ( 'NONE',  ( -19.65312891409030271, 93.06504152958497400, -40.00000000000000000 ) ) ;
#12576 = CARTESIAN_POINT ( 'NONE',  ( 188.4688990864094080, 295.3997683978527675, -11.43812978727723717 ) ) ;
#12577 = CARTESIAN_POINT ( 'NONE',  ( 110.2137735815727808, 245.9860189848785126, -2.679491924311252493 ) ) ;
#12578 = AXIS2_PLACEMENT_3D ( 'NONE', #99825, #37496, #29910 ) ;
#12579 = ORIENTED_EDGE ( 'NONE', *, *, #87804, .F. ) ;
#12580 = VECTOR ( 'NONE', #48661, 999.9999999999998863 ) ;
#12581 = ORIENTED_EDGE ( 'NONE', *, *, #89508, .T. ) ;
#12582 = ADVANCED_FACE ( 'NONE', ( #48381 ), #79325, .F. ) ;
#12583 = CARTESIAN_POINT ( 'NONE',  ( 86.94972120171313179, 45.89256597715363739, -8.147647120779746288 ) ) ;
#12584 = ADVANCED_FACE ( 'NONE', ( #10385 ), #86642, .T. ) ;
#12586 = B_SPLINE_SURFACE_WITH_KNOTS ( 'NONE', 3, 1, ( 
 ( #91713, #60749 ),
 ( #22274, #7070 ),
 ( #15662, #46053 ),
 ( #29877, #76969 ),
 ( #53178, #23260 ),
 ( #22782, #68863 ),
 ( #99788, #30378 ),
 ( #7569, #38459 ),
 ( #38959, #100292 ),
 ( #30876, #92710 ),
 ( #46557, #52665 ),
 ( #85111, #8086 ),
 ( #69865, #31367 ),
 ( #62251, #93205 ),
 ( #52168, #13687 ),
 ( #91213, #75495 ),
 ( #6080, #67885 ),
 ( #29388, #83619 ),
 ( #21775, #79523 ),
 ( #9595, #2490 ),
 ( #62759, #39447 ),
 ( #17682, #16175 ),
 ( #93717, #64784 ),
 ( #56154, #10584 ),
 ( #78493, #1490 ),
 ( #70368, #79008 ),
 ( #23760, #47071 ),
 ( #87653, #32373 ),
 ( #18184, #41457 ),
 ( #72399, #48582 ),
 ( #17167, #8582 ),
 ( #3007, #86632 ),
 ( #33372, #87150 ),
 ( #24768, #978 ) ),
 .UNSPECIFIED., .T., .F., .F.,
 ( 4, 2, 2, 2, 2, 2, 2, 2, 2, 2, 2, 2, 2, 2, 2, 2, 4 ),
 ( 2, 2 ),
 ( 0.000000000000000000, 0.06250000000000000000, 0.1250000000000000000, 0.1875000000000000000, 0.2500000000000000000, 0.3125000000000000000, 0.3750000000000000000, 0.4375000000000000000, 0.5000000000000000000, 0.5625000000000000000, 0.6250000000000000000, 0.6875000000000000000, 0.7500000000000000000, 0.8125000000000000000, 0.8750000000000000000, 0.9375000000000000000, 1.000000000000000000 ),
 ( 0.000000000000000000, 1.000000000000000000 ),
 .UNSPECIFIED. ) ;
#12585 = CARTESIAN_POINT ( 'NONE',  ( 176.7716622781765921, 292.6737166345459968, -2.766366243292323279 ) ) ;
#12587 = CARTESIAN_POINT ( 'NONE',  ( 196.4677102463732012, 290.3549391369982686, 16.45225250689336249 ) ) ;
#12588 = LINE ( 'NONE', #34374, #85662 ) ;
#12589 = CARTESIAN_POINT ( 'NONE',  ( 208.2161171980831682, 270.0061013886409569, 2.944709006235987747 ) ) ;
#12590 = B_SPLINE_CURVE_WITH_KNOTS ( 'NONE', 3,
 ( #32149, #99575, #22563, #92017 ),
 .UNSPECIFIED., .F., .F.,
 ( 4, 4 ),
 ( 0.000000000000000000, 0.004985884173467201863 ),
 .UNSPECIFIED. ) ;
#12591 = EDGE_LOOP ( 'NONE', ( #89873, #86239, #13935, #47455 ) ) ;
#12592 = ADVANCED_FACE ( 'NONE', ( #77018 ), #44609, .F. ) ;
#12593 = AXIS2_PLACEMENT_3D ( 'NONE', #15827, #68535, #52833 ) ;
#12594 = ORIENTED_EDGE ( 'NONE', *, *, #64591, .F. ) ;
#12595 = CARTESIAN_POINT ( 'NONE',  ( 207.6050568035884680, 271.0644890383991310, -1.456818755242089702 ) ) ;
#12596 = ORIENTED_EDGE ( 'NONE', *, *, #66008, .F. ) ;
#12597 = ADVANCED_FACE ( 'NONE', ( #21829 ), #75544, .F. ) ;
#12598 = CARTESIAN_POINT ( 'NONE',  ( 191.3831180832644066, 263.8491544962765829, -8.012675887993349733 ) ) ;
#12599 = DIRECTION ( 'NONE',  ( -0.7911563084720502070, -0.6116140086401538056, 0.000000000000000000 ) ) ;
#12600 = CARTESIAN_POINT ( 'NONE',  ( 82.08766997739726889, 44.26091490527264938, 9.509083040982000412 ) ) ;
#12602 = FACE_OUTER_BOUND ( 'NONE', #13312, .T. ) ;
#12601 = CARTESIAN_POINT ( 'NONE',  ( 134.7341806906763395, 248.5958772461660544, -9.188101187500095079 ) ) ;
#12603 = CARTESIAN_POINT ( 'NONE',  ( 155.5777206977276990, 264.9826732634378459, -17.41861857130547975 ) ) ;
#12604 = VERTEX_POINT ( 'NONE', #16724 ) ;
#12605 = VECTOR ( 'NONE', #7316, 1000.000000000000000 ) ;
#12606 = FACE_OUTER_BOUND ( 'NONE', #98322, .T. ) ;
#12607 = EDGE_CURVE ( 'NONE', #9589, #45905, #84006, .T. ) ;
#12608 = CARTESIAN_POINT ( 'NONE',  ( 26.55243232390424879, 15.73415679381822585, 1.333680081654574804E-15 ) ) ;
#12609 = CARTESIAN_POINT ( 'NONE',  ( 159.5895502557670795, 254.2297859303815244, -16.92708575547316485 ) ) ;
#12610 = ADVANCED_FACE ( 'NONE', ( #78543, #9131 ), #18237, .F. ) ;
#12611 = CARTESIAN_POINT ( 'NONE',  ( 172.3471576652249269, 251.0617913708788649, -0.2555901567849299671 ) ) ;
#12612 = CARTESIAN_POINT ( 'NONE',  ( 34.73530984921583098, 200.8615022471903160, 5.000000000000046185 ) ) ;
#12613 = CARTESIAN_POINT ( 'NONE',  ( 76.45572749640669485, 51.64231386250387601, -16.15369532800221108 ) ) ;
#12614 = CARTESIAN_POINT ( 'NONE',  ( 199.0981677397162457, 281.8773224221018268, -16.59884707263596226 ) ) ;
#12615 = LINE ( 'NONE', #82548, #38124 ) ;
#12616 = CARTESIAN_POINT ( 'NONE',  ( 78.90549422596571105, 46.47045305960070039, 12.99985401326298984 ) ) ;
#12617 = VECTOR ( 'NONE', #49605, 1000.000000000000114 ) ;
#12618 = CARTESIAN_POINT ( 'NONE',  ( 206.7147678843052461, 272.1735785942267967, 6.914908267696407762 ) ) ;
#12619 = CARTESIAN_POINT ( 'NONE',  ( 167.5937759011995638, 249.9759899836699901, 7.306980044439311150 ) ) ;
#12620 = CARTESIAN_POINT ( 'NONE',  ( 27.58098951138966726, 43.10352854649765675, -10.00000000000000000 ) ) ;
#12621 = CARTESIAN_POINT ( 'NONE',  ( -54.25007008209492909, 32.21233689110872689, 177.5919119679930134 ) ) ;
#12622 = FACE_OUTER_BOUND ( 'NONE', #10470, .T. ) ;
#12623 = CARTESIAN_POINT ( 'NONE',  ( 68.23939761155092754, 69.98628890222548193, -0.9983377936462706215 ) ) ;
#12624 = CARTESIAN_POINT ( 'NONE',  ( -19.65312891409030271, 93.06504152958497400, 59.99999999999999289 ) ) ;
#12625 = CARTESIAN_POINT ( 'NONE',  ( 78.14015596324891533, 47.79605781560270117, 14.53813849190288465 ) ) ;
#12626 = CARTESIAN_POINT ( 'NONE',  ( 38.08795742478228163, 27.15404122711136381, 8.090169943749479842 ) ) ;
#12627 = CARTESIAN_POINT ( 'NONE',  ( 80.33315281163550026, 55.86497812776784855, -16.47487610438770034 ) ) ;
#12628 =( BOUNDED_CURVE ( )  B_SPLINE_CURVE ( 2, ( #35062, #4165, #52254, #89336, #44147, #19408, #11307, #73101, #27489 ),
 .UNSPECIFIED., .F., .T. ) 
 B_SPLINE_CURVE_WITH_KNOTS ( ( 3, 2, 2, 2, 3 ),
 ( 0.8266129032258064946, 0.8279569892473118697, 0.8306451612903226200, 0.8333333333333333703, 0.8346774193548387455 ),
 .UNSPECIFIED. ) 
 CURVE ( )  GEOMETRIC_REPRESENTATION_ITEM ( )  RATIONAL_B_SPLINE_CURVE ( ( 0.9330127018922194093, 0.9330127018922194093, 1.000000000000000000, 0.8660254037844387076, 1.000000000000000000, 0.8660254037844387076, 1.000000000000000000, 0.9330127018922194093, 0.9330127018922194093 ) ) 
 REPRESENTATION_ITEM ( '' )  );
#12629 = CARTESIAN_POINT ( 'NONE',  ( 82.28582548923134254, 54.25481651909717584, 15.63115421305295527 ) ) ;
#12630 = LINE ( 'NONE', #49613, #83569 ) ;
#12631 = CARTESIAN_POINT ( 'NONE',  ( 14.59995888762994554, 188.4244531367911293, -4.594050593750046652 ) ) ;
#12632 = B_SPLINE_CURVE_WITH_KNOTS ( 'NONE', 3,
 ( #87814, #64945, #42126, #73058, #26451, #57326, #34055, #81183, #18352, #95890, #56828, #64442, #88298, #50718, #18854, #96373, #34532, #49735, #66430, #80688, #26939, #49245, #11263, #41624, #50228, #3652, #65432, #41119, #57824, #88802, #27447, #19850, #4127, #89296, #58321, #19369, #11750, #80182, #72052, #35021, #42613, #73544, #12245, #65923, #72566, #96880, #89770, #43104, #10748, #81671 ),
 .UNSPECIFIED., .F., .F.,
 ( 4, 2, 2, 2, 2, 2, 2, 2, 2, 2, 2, 2, 2, 2, 2, 2, 2, 2, 2, 2, 2, 2, 2, 2, 4 ),
 ( 0.0001458946000596443712, 0.001144903916429049467, 0.001644408574613814844, 0.001894160903706147443, 0.002019037068252331306, 0.002143913232798515169, 0.002268789397344698599, 0.002393665561890882029, 0.002643417890983249322, 0.003142922549168039419, 0.004141931865537725431, 0.005140941181907411443, 0.005640445840092211081, 0.005890198169184619574, 0.006139950498277027199, 0.006202388580550207385, 0.006264826662823387571, 0.006327264745096566889, 0.006389702827369747942, 0.006639455156462413174, 0.006889207485555077538, 0.007138959814647742770, 0.007388712143740408869, 0.007638464472833074101, 0.008137969131018543342 ),
 .UNSPECIFIED. ) ;
#12633 = CARTESIAN_POINT ( 'NONE',  ( 42.09652578138355494, 205.1115022471903160, -5.000000000000047962 ) ) ;
#12634 = EDGE_LOOP ( 'NONE', ( #28333, #68118, #25117, #69331 ) ) ;
#12635 = AXIS2_PLACEMENT_3D ( 'NONE', #96526, #28072, #27096 ) ;
#12636 = CARTESIAN_POINT ( 'NONE',  ( 87.04534585051717954, 46.05262481000475105, 8.948764308993935046 ) ) ;
#12637 = LINE ( 'NONE', #66809, #90446 ) ;
#12638 = CARTESIAN_POINT ( 'NONE',  ( 71.49023828022640714, 72.34911387847559183, -1.236132173619994168 ) ) ;
#12639 = CARTESIAN_POINT ( 'NONE',  ( 60.33744616864313315, 196.4548013555410080, -4.594050593750042211 ) ) ;
#12640 = VECTOR ( 'NONE', #97804, 1000.000000000000000 ) ;
#12641 = EDGE_CURVE ( 'NONE', #82130, #76711, #40002, .T. ) ;
#12642 = CARTESIAN_POINT ( 'NONE',  ( 161.6707029936031574, 250.6251236501384483, 14.45053103226186231 ) ) ;
#12643 = CARTESIAN_POINT ( 'NONE',  ( 170.9744194226895786, 287.2191983458180857, 7.031205856223269102 ) ) ;
#12644 = CARTESIAN_POINT ( 'NONE',  ( 146.8881680668833951, 276.2292252078784145, 4.973452195244782104 ) ) ;
#12645 = CARTESIAN_POINT ( 'NONE',  ( 7.993722094130166766, 16.56628583063838533, 9.188101187500006262 ) ) ;
#12646 = LINE ( 'NONE', #35917, #72396 ) ;
#12647 = CARTESIAN_POINT ( 'NONE',  ( 178.8525359564782775, 293.5924254160544820, 2.661079731265041382 ) ) ;
#12648 = AXIS2_PLACEMENT_3D ( 'NONE', #8051, #942, #9038 ) ;
#12649 = CARTESIAN_POINT ( 'NONE',  ( 176.1198908959743221, 274.8737079364501597, 17.13331764512671285 ) ) ;
#12650 = CARTESIAN_POINT ( 'NONE',  ( 165.9091197491159164, 246.2627970730538323, -2.747640711776688338 ) ) ;
#12651 = CARTESIAN_POINT ( 'NONE',  ( 68.05640523449149271, 67.83844799063044206, -7.344562446520097154 ) ) ;
#12652 = CARTESIAN_POINT ( 'NONE',  ( 91.36976281398784749, 216.8927522451417929, -10.00000000000009237 ) ) ;
#12653 = ADVANCED_FACE ( 'NONE', ( #47118 ), #78039, .F. ) ;
#12654 = CARTESIAN_POINT ( 'NONE',  ( 81.90096821949344985, 41.09411741666988149, 3.667264625812675316 ) ) ;
#12655 = AXIS2_PLACEMENT_3D ( 'NONE', #8793, #93936, #84339 ) ;
#12656 = CARTESIAN_POINT ( 'NONE',  ( 98.82118972926437550, 217.8615022471902023, 5.000000000000051514 ) ) ;
#12657 = CARTESIAN_POINT ( 'NONE',  ( 75.45929019331548204, 53.24617608301296201, 16.49036319738879897 ) ) ;
#12658 = CARTESIAN_POINT ( 'NONE',  ( 161.7100178915388824, 267.7548849422799435, -16.97131824026628877 ) ) ;
#12659 = VERTEX_POINT ( 'NONE', #31416 ) ;
#12660 = CARTESIAN_POINT ( 'NONE',  ( 52.62397354648171444, 207.3149278399161233, 9.188101187500093303 ) ) ;
#12661 = ORIENTED_EDGE ( 'NONE', *, *, #19172, .F. ) ;
#12662 = CARTESIAN_POINT ( 'NONE',  ( 52.94219725692860834, 189.8262482093458061, 3.021315404115420679E-15 ) ) ;
#12663 = CARTESIAN_POINT ( 'NONE',  ( 147.5177358149801421, 275.1387818813681179, 4.867883209065928085 ) ) ;
#12664 = EDGE_CURVE ( 'NONE', #95472, #64892, #1545, .T. ) ;
#12665 = CARTESIAN_POINT ( 'NONE',  ( 67.43033157395939270, 67.25313052952390080, -8.647980512837968092 ) ) ;
#12666 = ORIENTED_EDGE ( 'NONE', *, *, #98157, .T. ) ;
#12667 = CARTESIAN_POINT ( 'NONE',  ( -2.631798339875063064, 146.7012482093458914, -10.71504827818132277 ) ) ;
#12668 = CARTESIAN_POINT ( 'NONE',  ( 164.3274319858398087, 246.0235340536434592, -1.770631424362269168 ) ) ;
#12669 = LINE ( 'NONE', #50636, #79981 ) ;
#12670 = CARTESIAN_POINT ( 'NONE',  ( 27.40352323984253502, 36.79752408145593279, -5.678558825948271327 ) ) ;
#12671 = CARTESIAN_POINT ( 'NONE',  ( 188.8667127848526661, 265.4704850057313479, 10.73802221655500233 ) ) ;
#12672 = CARTESIAN_POINT ( 'NONE',  ( 148.9322735291567597, 272.6887306911919495, -12.40988026045598858 ) ) ;
#12673 = CARTESIAN_POINT ( 'NONE',  ( 157.0808507922293131, 258.5749808621497436, 16.84357500595720580 ) ) ;
#12674 = EDGE_LOOP ( 'NONE', ( #56646, #1607, #10308, #6173 ) ) ;
#12675 = CARTESIAN_POINT ( 'NONE',  ( 12.93608109523609073, 25.65586893147755276, -7.433330006724137462 ) ) ;
#12676 = CARTESIAN_POINT ( 'NONE',  ( 30.57965140047823738, 19.78380873178787880, -6.180339887498949025 ) ) ;
#12677 = CARTESIAN_POINT ( 'NONE',  ( 175.3131846714599362, 254.5210658486609532, 7.854781054984586675 ) ) ;
#12678 = FACE_OUTER_BOUND ( 'NONE', #48082, .T. ) ;
#12679 = EDGE_CURVE ( 'NONE', #85413, #9557, #2545, .T. ) ;
#12680 = EDGE_LOOP ( 'NONE', ( #77334, #100033, #5823, #10437, #80569, #73665, #85880, #95077 ) ) ;
#12681 = CARTESIAN_POINT ( 'NONE',  ( 182.3022624411334220, 284.0886791389093560, 14.96227919629477832 ) ) ;
#12682 = DIRECTION ( 'NONE',  ( -0.5000000000000008882, 0.8660254037844381525, 0.000000000000000000 ) ) ;
#12683 = EDGE_CURVE ( 'NONE', #12306, #80748, #94264, .T. ) ;
#12684 = CARTESIAN_POINT ( 'NONE',  ( 159.3995226465659982, 254.5589234043588078, -16.81133486613867234 ) ) ;
#12685 = ORIENTED_EDGE ( 'NONE', *, *, #68758, .T. ) ;
#12686 = EDGE_LOOP ( 'NONE', ( #97066, #34494, #3005, #18329 ) ) ;
#12687 = AXIS2_PLACEMENT_3D ( 'NONE', #69833, #100261, #59733 ) ;
#12689 = CARTESIAN_POINT ( 'NONE',  ( 54.85235828774394662, 209.1427522451419350, -10.00000000000009592 ) ) ;
#12688 = CARTESIAN_POINT ( 'NONE',  ( 161.1492466472929266, 251.5283125358769212, -13.33353587056634915 ) ) ;
#12690 = DIRECTION ( 'NONE',  ( 0.5000000000000004441, -0.8660254037844383745, -0.000000000000000000 ) ) ;
#12691 = VERTEX_POINT ( 'NONE', #1033 ) ;
#12692 = CARTESIAN_POINT ( 'NONE',  ( 66.53067542137131340, 68.81138069514842925, -2.220520527782671838 ) ) ;
#12693 = DIRECTION ( 'NONE',  ( 0.4999999999999998890, -0.8660254037844385966, 0.000000000000000000 ) ) ;
#12694 = CARTESIAN_POINT ( 'NONE',  ( 81.86683804372771078, 55.45883585039843666, 16.28524382593451136 ) ) ;
#12695 = CARTESIAN_POINT ( 'NONE',  ( 78.18406947592188772, 61.66846224198985027, -16.12704840749690050 ) ) ;
#12696 = CARTESIAN_POINT ( 'NONE',  ( 118.9560200436548314, 248.6744531367911293, 4.594050593750047540 ) ) ;
#12697 = CARTESIAN_POINT ( 'NONE',  ( 150.6571681785161445, 269.7011255207979730, 15.24894850018880454 ) ) ;
#12698 = LINE ( 'NONE', #73992, #85196 ) ;
#12699 = ORIENTED_EDGE ( 'NONE', *, *, #90708, .T. ) ;
#12700 = CARTESIAN_POINT ( 'NONE',  ( 201.2142882557298265, 280.3114506667780574, 16.76591128755623572 ) ) ;
#12701 = ORIENTED_EDGE ( 'NONE', *, *, #41723, .F. ) ;
#12702 = EDGE_LOOP ( 'NONE', ( #62731, #572, #9434, #74564 ) ) ;
#12703 = EDGE_CURVE ( 'NONE', #77668, #20229, #23240, .T. ) ;
#12704 = FACE_BOUND ( 'NONE', #65637, .T. ) ;
#12705 = DIRECTION ( 'NONE',  ( -0.9879014915521923124, 0.1550826972584425645, 0.000000000000000000 ) ) ;
#12706 = CARTESIAN_POINT ( 'NONE',  ( 73.21957404993666785, 203.8923013555409796, 4.594050593750050204 ) ) ;
#12707 = CARTESIAN_POINT ( 'NONE',  ( 175.4967466201937611, 291.2628096033125189, 6.560984766252938805 ) ) ;
#12708 = CARTESIAN_POINT ( 'NONE',  ( 194.6050500505458842, 285.5465367126718093, -17.70104686455487553 ) ) ;
#12709 = CARTESIAN_POINT ( 'NONE',  ( 150.5355989389948093, 269.9116896202863245, 15.28294032643914768 ) ) ;
#12710 = CARTESIAN_POINT ( 'NONE',  ( 172.6757217805928235, 277.3386798770395103, 16.69748815113853979 ) ) ;
#12711 = CARTESIAN_POINT ( 'NONE',  ( 87.74082335983182190, 45.11567895962654973, 6.804767787324432327 ) ) ;
#12712 = EDGE_LOOP ( 'NONE', ( #28042, #21080, #9687, #66885 ) ) ;
#12713 = EDGE_CURVE ( 'NONE', #34033, #69834, #32919, .T. ) ;
#12714 = CARTESIAN_POINT ( 'NONE',  ( 66.43194084327845417, 68.18590565871475917, 4.517642387139569671 ) ) ;
#12715 = CARTESIAN_POINT ( 'NONE',  ( 87.29803824456323014, 43.36679595344801896, 2.358950023001834317 ) ) ;
#12716 = VECTOR ( 'NONE', #30004, 1000.000000000000114 ) ;
#12717 = ORIENTED_EDGE ( 'NONE', *, *, #29961, .T. ) ;
#12718 = CARTESIAN_POINT ( 'NONE',  ( -77.58047734835669473, 56.02942318228900120, -10.00000000000000000 ) ) ;
#12719 = CARTESIAN_POINT ( 'NONE',  ( 163.9665353451645160, 260.5250585567103485, -16.17572278673254615 ) ) ;
#12720 = CARTESIAN_POINT ( 'NONE',  ( -23.73952538801239598, 24.43184193311134678, 10.00000000000000000 ) ) ;
#12721 = VECTOR ( 'NONE', #70966, 1000.000000000000227 ) ;
#12722 = EDGE_CURVE ( 'NONE', #65850, #68464, #10638, .T. ) ;
#12723 = DIRECTION ( 'NONE',  ( -1.000000000000000000, 0.000000000000000000, 0.000000000000000000 ) ) ;
#12724 = VECTOR ( 'NONE', #10072, 1000.000000000000114 ) ;
#12725 = CARTESIAN_POINT ( 'NONE',  ( 206.1932826529868805, 273.5097535960530877, 11.72208607728249241 ) ) ;
#12726 = CYLINDRICAL_SURFACE ( 'NONE', #42803, 17.82106496071139645 ) ;
#12727 = ORIENTED_EDGE ( 'NONE', *, *, #90949, .T. ) ;
#12728 = CARTESIAN_POINT ( 'NONE',  ( 164.4817765375028102, 245.7562014482918755, -6.334578229142199035 ) ) ;
#12729 = AXIS2_PLACEMENT_3D ( 'NONE', #53275, #23360, #62865 ) ;
#12730 = EDGE_CURVE ( 'NONE', #36195, #99407, #47168, .T. ) ;
#12731 = CARTESIAN_POINT ( 'NONE',  ( 125.6948669907937415, 249.5024278399160949, 9.188101187500095079 ) ) ;
#12732 = ORIENTED_EDGE ( 'NONE', *, *, #24408, .T. ) ;
#12733 = CARTESIAN_POINT ( 'NONE',  ( 80.84437787308391421, 44.34192801377794524, -10.37496191005612900 ) ) ;
#12734 = CARTESIAN_POINT ( 'NONE',  ( 73.85816664754916872, 67.07998314229074310, -12.61123796580315570 ) ) ;
#12735 = CARTESIAN_POINT ( 'NONE',  ( -19.65312891409030271, 93.06504152958497400, 177.5919119679930134 ) ) ;
#12736 = CARTESIAN_POINT ( 'NONE',  ( 43.63646518856938172, 66.22046553916848666, 10.00000000000000000 ) ) ;
#12737 = CARTESIAN_POINT ( 'NONE',  ( 74.66991520905840218, 60.53581785384168512, 15.47673426609052960 ) ) ;
#12738 = CARTESIAN_POINT ( 'NONE',  ( 190.2204363742943656, 300.4646209966566062, -1.328626404316530739E-11 ) ) ;
#12739 = ORIENTED_EDGE ( 'NONE', *, *, #56431, .T. ) ;
#12740 = CARTESIAN_POINT ( 'NONE',  ( 77.49042508736837931, 60.78651308045809998, 15.85568622532634819 ) ) ;
#12741 = VECTOR ( 'NONE', #11218, 1000.000000000000000 ) ;
#12742 = CARTESIAN_POINT ( 'NONE',  ( 184.7266634662323952, 277.2745127826178759, -16.72297256227146534 ) ) ;
#12743 = CARTESIAN_POINT ( 'NONE',  ( 72.56743321539229896, 71.30517223960133322, -6.002003212711099600 ) ) ;
#12744 = CARTESIAN_POINT ( 'NONE',  ( 206.0013442967545245, 273.8422005809691768, -10.96701481760672792 ) ) ;
#12745 = CARTESIAN_POINT ( 'NONE',  ( 73.64963185817160252, 69.30855129028742567, -9.977530012273353677 ) ) ;
#12746 = B_SPLINE_CURVE_WITH_KNOTS ( 'NONE', 3,
 ( #97761, #28331, #82091, #83578, #21736, #97275, #14139, #27842, #98257, #83077, #6544, #90183 ),
 .UNSPECIFIED., .F., .F.,
 ( 4, 2, 2, 2, 2, 4 ),
 ( 0.001227138907740844311, 0.001452414644335943937, 0.001677690380931043564, 0.002128241854121296159, 0.002578793327311548322, 0.003029344800501800918 ),
 .UNSPECIFIED. ) ;
#12747 = CARTESIAN_POINT ( 'NONE',  ( 190.7569505155522904, 300.2462651405980978, -5.670926626284815697 ) ) ;
#12748 = CARTESIAN_POINT ( 'NONE',  ( 48.73804053012794668, 107.9864336245683631, 10.00000000000000000 ) ) ;
#12749 = VECTOR ( 'NONE', #67040, 1000.000000000000114 ) ;
#12750 = CARTESIAN_POINT ( 'NONE',  ( 157.1965120183049578, 258.3746497421212780, -18.06591467563559306 ) ) ;
#12751 = CARTESIAN_POINT ( 'NONE',  ( 195.9623275608007589, 270.6700471875816447, 12.00925747662462406 ) ) ;
#12752 = CARTESIAN_POINT ( 'NONE',  ( 14.02357142238433063, 26.83478043621387243, -8.090169943749479842 ) ) ;
#12753 = CARTESIAN_POINT ( 'NONE',  ( 177.4877928417686803, 293.5951873982637608, -2.837372163671336267 ) ) ;
#12754 = CARTESIAN_POINT ( 'NONE',  ( 71.81202244518919997, 222.2677522451419065, -5.000000000000047962 ) ) ;
#12755 = CARTESIAN_POINT ( 'NONE',  ( 15.68640692011977222, 32.55466486950700045, -1.111400068045478839E-16 ) ) ;
#12756 = CARTESIAN_POINT ( 'NONE',  ( 162.2482745412403631, 281.2414901047574745, 10.34674202811327248 ) ) ;
#12757 = CARTESIAN_POINT ( 'NONE',  ( 72.21898876619836471, 72.04774665458343463, -3.189688383038575381 ) ) ;
#12758 = CARTESIAN_POINT ( 'NONE',  ( 139.8671854259164036, 244.8927522451418497, 10.00000000000009592 ) ) ;
#12759 = CARTESIAN_POINT ( 'NONE',  ( 172.2535748400142097, 283.6734274018703559, -12.51371615245540880 ) ) ;
#12760 = ORIENTED_EDGE ( 'NONE', *, *, #84398, .F. ) ;
#12761 = CARTESIAN_POINT ( 'NONE',  ( 157.6673516573649181, 257.5591315650518141, 16.79781451397666103 ) ) ;
#12762 = CARTESIAN_POINT ( 'NONE',  ( 198.8157103782086210, 286.2880836124806478, -18.60729372713428020 ) ) ;
#12763 = CARTESIAN_POINT ( 'NONE',  ( 5.344833028331274605, 164.7048013555410080, 4.594050593750051981 ) ) ;
#12764 = CARTESIAN_POINT ( 'NONE',  ( 50.35065686154756293, 206.0024278399160949, 9.188101187500095079 ) ) ;
#12765 = CARTESIAN_POINT ( 'NONE',  ( 82.66777534753497036, 40.88273136530058594, 3.288167606880417981 ) ) ;
#12766 = CARTESIAN_POINT ( 'NONE',  ( 29.67845259158361415, 16.94473085651393163, 1.475505719884397138E-15 ) ) ;
#12767 = CARTESIAN_POINT ( 'NONE',  ( 85.48805828002734586, 48.64268271054365300, 12.46980397201070900 ) ) ;
#12768 = CARTESIAN_POINT ( 'NONE',  ( 157.1539462478114615, 258.4483758192793061, -17.96006278656275867 ) ) ;
#12769 = CARTESIAN_POINT ( 'NONE',  ( 192.6020092295239010, 292.3528725471387020, -14.35004337652128470 ) ) ;
#12770 = CARTESIAN_POINT ( 'NONE',  ( 147.7395812515338491, 275.4447818272566337, 3.760927250875937489 ) ) ;
#12772 = CARTESIAN_POINT ( 'NONE',  ( 64.01779381112923772, 217.7677522451419065, -5.000000000000047962 ) ) ;
#12771 = CARTESIAN_POINT ( 'NONE',  ( 167.5542314069692793, 256.6061373407214319, 13.74842419216645695 ) ) ;
#12773 = CARTESIAN_POINT ( 'NONE',  ( 181.4027557144102900, 255.2212836150004023, 2.052969345246689503 ) ) ;
#12774 = CARTESIAN_POINT ( 'NONE',  ( 150.4255120825602887, 270.1023656488765710, 15.17857413906334507 ) ) ;
#12775 = CARTESIAN_POINT ( 'NONE',  ( 179.2832723880610786, 294.0843149181845320, 1.044996869123359318 ) ) ;
#12776 = CARTESIAN_POINT ( 'NONE',  ( 58.19016453504443831, 197.7365022471902307, 10.00000000000009592 ) ) ;
#12777 = CARTESIAN_POINT ( 'NONE',  ( 184.1284384789660749, 293.1887098790314212, 9.479892220414697590 ) ) ;
#12778 = CARTESIAN_POINT ( 'NONE',  ( 163.4260108471723640, 247.5848412648317662, 10.45113099391573108 ) ) ;
#12779 = CIRCLE ( 'NONE', #82393, 10.00000000000011369 ) ;
#12780 = CARTESIAN_POINT ( 'NONE',  ( 18.36166996137734841, 193.6589784336661637, -6.496448406907675876E-16 ) ) ;
#12781 = CARTESIAN_POINT ( 'NONE',  ( 167.9915683551312782, 286.1490694072173824, 4.089171754536926606 ) ) ;
#12782 = CARTESIAN_POINT ( 'NONE',  ( 153.1314981037513121, 265.4154603756023789, 17.73969815997475408 ) ) ;
#12783 = CARTESIAN_POINT ( 'NONE',  ( 34.04545031248176912, 37.84336893147759184, -7.433330006724137462 ) ) ;
#12784 = CARTESIAN_POINT ( 'NONE',  ( 139.3620039403754731, 251.2677522451418497, 10.00000000000009592 ) ) ;
#12785 = ADVANCED_FACE ( 'NONE', ( #87205 ), #17738, .F. ) ;
#12787 = CARTESIAN_POINT ( 'NONE',  ( 183.0432481310025992, 278.8237664249871273, 16.78443556766483624 ) ) ;
#12786 = VECTOR ( 'NONE', #17473, 1000.000000000000114 ) ;
#12788 = CARTESIAN_POINT ( 'NONE',  ( 175.0686550866780635, 279.4321407445321483, 16.32612376929353815 ) ) ;
#12789 = DIRECTION ( 'NONE',  ( 0.4999999999999992784, -0.8660254037844390407, 0.000000000000000000 ) ) ;
#12790 = CARTESIAN_POINT ( 'NONE',  ( 177.7668908026954284, 261.5253217029109010, -12.97050892711601300 ) ) ;
#12791 = AXIS2_PLACEMENT_3D ( 'NONE', #53570, #68277, #60162 ) ;
#12792 = CARTESIAN_POINT ( 'NONE',  ( 16.86928618479236164, 18.24335787977762990, -9.188101187500008038 ) ) ;
#12793 = CARTESIAN_POINT ( 'NONE',  ( 71.71444459471547361, 72.49928141732986830, 0.9658765412761121105 ) ) ;
#12794 = CARTESIAN_POINT ( 'NONE',  ( 82.40504737207831454, 54.25064673307860375, 15.61126503404915233 ) ) ;
#12795 = CARTESIAN_POINT ( 'NONE',  ( 175.8027662909930484, 284.8719843250962072, 14.11304877541382119 ) ) ;
#12796 = CARTESIAN_POINT ( 'NONE',  ( 153.2146083375174328, 277.7743879745896720, -5.000743142145255504 ) ) ;
#12797 = ORIENTED_EDGE ( 'NONE', *, *, #61148, .T. ) ;
#12798 = CARTESIAN_POINT ( 'NONE',  ( 181.9257749470477563, 289.8349502344528901, 12.95467248944978422 ) ) ;
#12799 = CARTESIAN_POINT ( 'NONE',  ( 18.71323094475359738, 33.73705186507753950, -3.090169943749475845 ) ) ;
#12800 = CARTESIAN_POINT ( 'NONE',  ( 159.9647205790309101, 253.5799718689968927, -16.48298384325780219 ) ) ;
#12801 = EDGE_CURVE ( 'NONE', #50534, #98353, #57569, .T. ) ;
#12802 = ORIENTED_EDGE ( 'NONE', *, *, #72641, .F. ) ;
#12803 = CARTESIAN_POINT ( 'NONE',  ( 152.7043854946215049, 268.1552411151685078, 15.94764448997051964 ) ) ;
#12804 = DIRECTION ( 'NONE',  ( -0.000000000000000000, -1.000000000000000000, -0.000000000000000000 ) ) ;
#12805 = B_SPLINE_CURVE_WITH_KNOTS ( 'NONE', 3,
 ( #84436, #68186, #7905, #45387 ),
 .UNSPECIFIED., .F., .F.,
 ( 4, 4 ),
 ( 0.03473529416486713373, 0.04353459421610011981 ),
 .UNSPECIFIED. ) ;
#12806 = CARTESIAN_POINT ( 'NONE',  ( 200.0411626275569574, 270.6720010161316736, -11.59284015024147152 ) ) ;
#12807 = EDGE_CURVE ( 'NONE', #28368, #70394, #11641, .T. ) ;
#12808 = CARTESIAN_POINT ( 'NONE',  ( 155.4661767250933622, 261.3716783840932294, -17.10192542004562810 ) ) ;
#12809 = ORIENTED_EDGE ( 'NONE', *, *, #62765, .T. ) ;
#12810 = VECTOR ( 'NONE', #41667, 1000.000000000000000 ) ;
#12811 = ORIENTED_EDGE ( 'NONE', *, *, #35527, .F. ) ;
#12813 = CARTESIAN_POINT ( 'NONE',  ( 164.3961040135806968, 245.9045906125373904, 7.095190383188031191 ) ) ;
#12812 = CARTESIAN_POINT ( 'NONE',  ( 159.3076723029256812, 279.4120732660696262, -9.573196759042872372 ) ) ;
#12814 = CARTESIAN_POINT ( 'NONE',  ( 192.6773196027083372, 296.9200883123592689, 11.15745042875121484 ) ) ;
#12815 = ORIENTED_EDGE ( 'NONE', *, *, #12683, .T. ) ;
#12816 = CARTESIAN_POINT ( 'NONE',  ( 88.41107184461979784, 44.00353577411875960, -2.298891457252526749 ) ) ;
#12817 = CARTESIAN_POINT ( 'NONE',  ( 80.56456852273207403, 57.68474611512090178, 16.59351620786970827 ) ) ;
#12818 = CARTESIAN_POINT ( 'NONE',  ( 175.2632563419276721, 262.6760348153215432, 14.36099408182738912 ) ) ;
#12819 = ORIENTED_EDGE ( 'NONE', *, *, #22660, .F. ) ;
#12820 = CARTESIAN_POINT ( 'NONE',  ( 87.60616923137877166, 45.13511946215697890, -6.138091206483382578 ) ) ;
#12821 = CARTESIAN_POINT ( 'NONE',  ( 88.49445028879968334, 43.86712364161932243, -9.307608808691473302E-08 ) ) ;
#12822 = CARTESIAN_POINT ( 'NONE',  ( 80.67567036563099236, 43.43790138286748714, 9.454380761424062030 ) ) ;
#12823 = VERTEX_POINT ( 'NONE', #96261 ) ;
#12824 = CARTESIAN_POINT ( 'NONE',  ( 205.7867067512454184, 274.2139637150027056, 10.62737868262404106 ) ) ;
#12825 = CARTESIAN_POINT ( 'NONE',  ( 74.01533384933624404, 61.07494375654813723, 15.18702621176734446 ) ) ;
#12826 = PRODUCT_DEFINITION_SHAPE ( 'NONE', 'NONE',  #100297 ) ;
#12827 = EDGE_LOOP ( 'NONE', ( #11661, #76386, #17974, #34984 ) ) ;
#12828 = CARTESIAN_POINT ( 'NONE',  ( 177.7722849220445482, 279.4784791579494936, -16.51336255298548394 ) ) ;
#12829 = CARTESIAN_POINT ( 'NONE',  ( -32.94356256989595977, 94.88921800892812541, 43.89948692389422291 ) ) ;
#12830 = ORIENTED_EDGE ( 'NONE', *, *, #26890, .F. ) ;
#12831 = PLANE ( 'NONE',  #83906 ) ;
#12832 = ORIENTED_EDGE ( 'NONE', *, *, #85999, .T. ) ;
#12833 = CARTESIAN_POINT ( 'NONE',  ( 157.5260732920700661, 268.8916645685611115, 15.61200622228795254 ) ) ;
#12834 = ORIENTED_EDGE ( 'NONE', *, *, #70805, .T. ) ;
#12835 = ADVANCED_FACE ( 'NONE', ( #42500 ), #89671, .F. ) ;
#12836 = CARTESIAN_POINT ( 'NONE',  ( 156.5505791614179145, 266.8975169099628602, -16.19599294687877489 ) ) ;
#12837 = CARTESIAN_POINT ( 'NONE',  ( 198.2505066714982149, 285.2670451491296149, 0.000000000000000000 ) ) ;
#12838 = CARTESIAN_POINT ( 'NONE',  ( 190.1693911629507738, 301.2639477917662703, -5.112716700269980485 ) ) ;
#12839 = CARTESIAN_POINT ( 'NONE',  ( 83.01487341893997041, 53.35419878647658720, 15.61608225115200810 ) ) ;
#12840 = CARTESIAN_POINT ( 'NONE',  ( 190.0445576990143195, 301.4801656937889902, 4.140328216824785912 ) ) ;
#12841 = CARTESIAN_POINT ( 'NONE',  ( 192.7259387352017939, 296.8358775046606297, 11.24705370801146209 ) ) ;
#12842 = CARTESIAN_POINT ( 'NONE',  ( 39.06543686813810012, 183.3615022471902023, 5.000000000000051514 ) ) ;
#12843 = CARTESIAN_POINT ( 'NONE',  ( 159.0312449811773376, 255.1967990321049058, -16.31084382475164674 ) ) ;
#12844 = EDGE_LOOP ( 'NONE', ( #81144, #19702, #63111, #85220 ) ) ;
#12845 = EDGE_CURVE ( 'NONE', #62907, #83615, #53205, .T. ) ;
#12846 = CARTESIAN_POINT ( 'NONE',  ( -17.23454462704816947, 134.8759306620403038, 8.559299000364187034E-14 ) ) ;
#12847 = CARTESIAN_POINT ( 'NONE',  ( 206.4229368915142686, 273.1119807867502800, 10.31819530520674810 ) ) ;
#12849 = CARTESIAN_POINT ( 'NONE',  ( 164.3493441216711517, 245.9855811210807417, 1.722120810491653664 ) ) ;
#12848 = CARTESIAN_POINT ( 'NONE',  ( 149.6191398986701415, 271.4990432411842676, -11.66821883946526839 ) ) ;
#12850 = CARTESIAN_POINT ( 'NONE',  ( 168.7107245727987390, 286.5688979659043980, 4.076349780630120101 ) ) ;
#12851 = CARTESIAN_POINT ( 'NONE',  ( 48.81784752633561908, 86.82484054835779830, -10.00000000000000000 ) ) ;
#12852 = ORIENTED_EDGE ( 'NONE', *, *, #83952, .F. ) ;
#12853 = CARTESIAN_POINT ( 'NONE',  ( 70.92937966038938669, 67.01461546877725084, 10.61286113055345304 ) ) ;
#12854 = ADVANCED_FACE ( 'NONE', ( #12129 ), #95781, .T. ) ;
#12855 = CARTESIAN_POINT ( 'NONE',  ( 83.91622664933946396, 41.67106969241695680, 3.569253368665360249 ) ) ;
#12856 = FACE_OUTER_BOUND ( 'NONE', #93709, .T. ) ;
#12857 = CARTESIAN_POINT ( 'NONE',  ( 160.0264454347010883, 253.4730612828859364, -14.80461457038359541 ) ) ;
#12858 = CARTESIAN_POINT ( 'NONE',  ( 148.1504907822988457, 274.0428181292306249, -10.36053812211976144 ) ) ;
#12859 = ORIENTED_EDGE ( 'NONE', *, *, #21601, .T. ) ;
#12860 = CARTESIAN_POINT ( 'NONE',  ( 170.6724042201842622, 255.4561172912020481, -12.81820913873951717 ) ) ;
#12861 = CARTESIAN_POINT ( 'NONE',  ( 85.76883949360097859, 47.60599329228222842, 11.49143109850623823 ) ) ;
#12862 = CARTESIAN_POINT ( 'NONE',  ( 200.8147387322574957, 282.8256649374973790, -18.02438097732020239 ) ) ;
#12863 = CARTESIAN_POINT ( 'NONE',  ( 164.5867587387928950, 245.5743669417666126, -3.022048486790635202 ) ) ;
#12864 = CARTESIAN_POINT ( 'NONE',  ( 27.64472685218281711, 196.7677522451419350, -5.000000000000047962 ) ) ;
#12865 = CARTESIAN_POINT ( 'NONE',  ( 125.2893514524760548, 233.9548013555409796, -4.594050593750042211 ) ) ;
#12866 = CARTESIAN_POINT ( 'NONE',  ( 180.9267084132501964, 294.1738383600696238, -2.651135849888626606 ) ) ;
#12867 = AXIS2_PLACEMENT_3D ( 'NONE', #76068, #99355, #78429 ) ;
#12868 = CARTESIAN_POINT ( 'NONE',  ( 162.6810519034260665, 249.2653427326025906, -10.49599293899969688 ) ) ;
#12869 = CARTESIAN_POINT ( 'NONE',  ( 157.2333142128019858, 258.3109064714224132, 16.87956768598436597 ) ) ;
#12870 = CARTESIAN_POINT ( 'NONE',  ( 207.5987293781265919, 271.0754484607800237, 1.965225377555418484 ) ) ;
#12871 = CARTESIAN_POINT ( 'NONE',  ( 42.77328167419873495, 189.3768266524160140, 9.188101187500098632 ) ) ;
#12872 = CARTESIAN_POINT ( 'NONE',  ( 82.62131884904979984, 40.84117856601688601, 3.225010313909428383 ) ) ;
#12873 = ORIENTED_EDGE ( 'NONE', *, *, #36819, .F. ) ;
#12874 = VECTOR ( 'NONE', #84175, 1000.000000000000114 ) ;
#12875 = ORIENTED_EDGE ( 'NONE', *, *, #42459, .T. ) ;
#12876 = CARTESIAN_POINT ( 'NONE',  ( 73.01042618992920552, 69.46801108043791828, 9.349659332454741900 ) ) ;
#12877 = DIRECTION ( 'NONE',  ( -0.5000000000000019984, 0.8660254037844374864, 0.000000000000000000 ) ) ;
#12878 = CARTESIAN_POINT ( 'NONE',  ( 30.69616969366791537, 176.9824982072973967, 3.021315404115420679E-15 ) ) ;
#12879 = CARTESIAN_POINT ( 'NONE',  ( 146.9709166616330549, 276.0859004375172390, 3.755270622130282732 ) ) ;
#12880 = FACE_OUTER_BOUND ( 'NONE', #50551, .T. ) ;
#12881 = EDGE_CURVE ( 'NONE', #94756, #72513, #64164, .T. ) ;
#12882 = CARTESIAN_POINT ( 'NONE',  ( 207.7666684749232786, 270.7845694125510931, -6.630926507062123498 ) ) ;
#12883 = CARTESIAN_POINT ( 'NONE',  ( 168.0703335804080609, 251.8096463010647312, 10.49794630816577445 ) ) ;
#12884 = CARTESIAN_POINT ( 'NONE',  ( 88.69951781898578247, 222.0177522451418781, -10.00000000000009592 ) ) ;
#12885 = B_SPLINE_SURFACE_WITH_KNOTS ( 'NONE', 3, 1, ( 
 ( #43531, #3786 ),
 ( #11891, #58456 ),
 ( #42749, #26086 ),
 ( #56960, #4786 ),
 ( #81811, #87461 ),
 ( #80320, #80836 ),
 ( #87947, #72712 ),
 ( #17993, #34668 ),
 ( #88954, #41257 ),
 ( #49376, #41766 ),
 ( #48887, #89429 ),
 ( #27592, #10388 ),
 ( #88440, #11404 ),
 ( #19983, #72199 ),
 ( #34181, #2805 ),
 ( #65570, #33692 ),
 ( #64586, #96517 ),
 ( #73683, #50860 ),
 ( #4267, #18491 ),
 ( #10890, #95538 ),
 ( #12387, #3302 ),
 ( #19000, #65075 ),
 ( #96024, #26587 ),
 ( #43252, #74197 ),
 ( #57460, #27086 ),
 ( #35165, #66075 ),
 ( #49875, #42258 ),
 ( #73192, #57969 ),
 ( #19509, #50366 ),
 ( #81320, #97022 ),
 ( #59944, #28557 ),
 ( #37156, #13380 ),
 ( #30051, #14364 ),
 ( #84301, #14849 ) ),
 .UNSPECIFIED., .T., .F., .F.,
 ( 4, 2, 2, 2, 2, 2, 2, 2, 2, 2, 2, 2, 2, 2, 2, 2, 4 ),
 ( 2, 2 ),
 ( 0.000000000000000000, 0.06250000000000000000, 0.1250000000000000000, 0.1875000000000000000, 0.2500000000000000000, 0.3125000000000000000, 0.3750000000000000000, 0.4375000000000000000, 0.5000000000000000000, 0.5625000000000000000, 0.6250000000000000000, 0.6875000000000000000, 0.7500000000000000000, 0.8125000000000000000, 0.8750000000000000000, 0.9375000000000000000, 1.000000000000000000 ),
 ( 0.000000000000000000, 1.000000000000000000 ),
 .UNSPECIFIED. ) ;
#12886 = VERTEX_POINT ( 'NONE', #5028 ) ;
#12887 = EDGE_CURVE ( 'NONE', #63662, #58917, #67928, .T. ) ;
#12888 = CARTESIAN_POINT ( 'NONE',  ( 195.2652153521346463, 266.6463243828191025, -7.753748465262478184 ) ) ;
#12889 = CARTESIAN_POINT ( 'NONE',  ( 155.5460960050927213, 279.7549409233841402, -1.594755899433322854 ) ) ;
#12890 = CARTESIAN_POINT ( 'NONE',  ( 162.6425574510925003, 248.9418223522047526, -10.70838742014210077 ) ) ;
#12891 = CARTESIAN_POINT ( 'NONE',  ( 11.37951369124782453, 183.5024278399160949, 9.188101187500095079 ) ) ;
#12892 = B_SPLINE_CURVE_WITH_KNOTS ( 'NONE', 3,
 ( #51999, #98625, #83936, #44878, #29206, #4919, #60571, #52988, #82463, #52485 ),
 .UNSPECIFIED., .F., .F.,
 ( 4, 2, 2, 2, 4 ),
 ( 0.000000000000000000, 0.0002622400424273360143, 0.0005244800848546720285, 0.0007867201272820080428, 0.001048960169709344057 ),
 .UNSPECIFIED. ) ;
#12893 = CARTESIAN_POINT ( 'NONE',  ( 7.727700963378506316, 20.16454794089039382, -10.00000000000000355 ) ) ;
#12894 = FACE_OUTER_BOUND ( 'NONE', #80263, .T. ) ;
#12895 = CARTESIAN_POINT ( 'NONE',  ( 71.69771586823793541, 58.77412815006911728, -15.43371067787085416 ) ) ;
#12896 = CARTESIAN_POINT ( 'NONE',  ( 73.62250635243425734, 69.55784274833358438, 10.23584637956793131 ) ) ;
#12897 = CARTESIAN_POINT ( 'NONE',  ( 57.63111678181675757, 194.8923013555409796, 4.594050593750050204 ) ) ;
#12898 = FACE_OUTER_BOUND ( 'NONE', #32146, .T. ) ;
#12899 = CARTESIAN_POINT ( 'NONE',  ( 164.3010377730689981, 246.0692501711882869, 7.247566249275159578 ) ) ;
#12900 = CARTESIAN_POINT ( 'NONE',  ( 71.44251307236943660, 71.49647877896676107, 3.603793749803205770 ) ) ;
#12901 = CARTESIAN_POINT ( 'NONE',  ( 207.6508796976096107, 270.9851214578045528, 6.713685698622268383 ) ) ;
#12902 = VERTEX_POINT ( 'NONE', #26333 ) ;
#12903 = CARTESIAN_POINT ( 'NONE',  ( 2.692369909191673294, 162.3615022471902023, 5.000000000000051514 ) ) ;
#12904 = CARTESIAN_POINT ( 'NONE',  ( -19.65312891409030271, 93.06504152958497400, -10.00000000000000888 ) ) ;
#12905 = CARTESIAN_POINT ( 'NONE',  ( 145.9657079678295020, 245.8923013555409511, 4.594050593750050204 ) ) ;
#12906 = CARTESIAN_POINT ( 'NONE',  ( 29.91980124543643171, 22.98920272979927759, 7.433330006724137462 ) ) ;
#12907 = CARTESIAN_POINT ( 'NONE',  ( 206.7843909389352177, 272.4859240120160280, -7.614953610527129158 ) ) ;
#12908 = CARTESIAN_POINT ( 'NONE',  ( 83.52018940653934465, 51.62319858702418429, -14.86581989589152819 ) ) ;
#12909 = DIRECTION ( 'NONE',  ( 0.2194785493951409983, -0.9756173257765591300, 0.000000000000000000 ) ) ;
#12911 = CARTESIAN_POINT ( 'NONE',  ( 189.4521523383693875, 289.8044986729786388, 14.56744347494121961 ) ) ;
#12910 = DIRECTION ( 'NONE',  ( -0.04056776950002415755, 0.9991767892008865948, 0.000000000000000000 ) ) ;
#12912 = CARTESIAN_POINT ( 'NONE',  ( 190.5730759679604773, 300.5647451992460333, -7.149221719703987787 ) ) ;
#12913 = VERTEX_POINT ( 'NONE', #72953 ) ;
#12914 = CARTESIAN_POINT ( 'NONE',  ( 191.4941427383744781, 298.9694107557253346, 8.584406880462095657 ) ) ;
#12915 = CARTESIAN_POINT ( 'NONE',  ( 208.2813134324037492, 269.8931781983357041, -0.4511785827856357178 ) ) ;
#12916 = CARTESIAN_POINT ( 'NONE',  ( 151.3881894390805485, 268.8414657422088681, -14.32066872820409742 ) ) ;
#12917 = DIRECTION ( 'NONE',  ( -0.8660254037844379305, -0.5000000000000014433, -0.000000000000000000 ) ) ;
#12918 = CARTESIAN_POINT ( 'NONE',  ( 197.2082756938223440, 273.4841093250385597, -13.85768748786135340 ) ) ;
#12919 = ORIENTED_EDGE ( 'NONE', *, *, #34421, .T. ) ;
#12920 = CARTESIAN_POINT ( 'NONE',  ( 70.70503195363177440, 69.91188268790216398, 6.471540178100598339 ) ) ;
#12921 = CARTESIAN_POINT ( 'NONE',  ( 169.2808828497843763, 282.7368009450043473, -10.94465088845561773 ) ) ;
#12922 = EDGE_CURVE ( 'NONE', #14901, #59762, #44752, .T. ) ;
#12923 = CARTESIAN_POINT ( 'NONE',  ( 84.39397012298853440, 43.45927479173952435, 6.252015531843233553 ) ) ;
#12924 = CARTESIAN_POINT ( 'NONE',  ( 40.34888600819125060, 126.6204015641749834, 10.00000000000000000 ) ) ;
#12925 = CARTESIAN_POINT ( 'NONE',  ( 185.5894612333727309, 296.5431996284972911, 4.661688250043606985 ) ) ;
#12926 = EDGE_CURVE ( 'NONE', #17056, #8797, #31482, .T. ) ;
#12927 = CARTESIAN_POINT ( 'NONE',  ( 68.07503851180729271, 69.33559177987039845, 4.005160369666961984 ) ) ;
#12928 = CARTESIAN_POINT ( 'NONE',  ( 150.4933457285363261, 277.6093123845979562, -0.0001770771435699358459 ) ) ;
#12929 =( BOUNDED_CURVE ( )  B_SPLINE_CURVE ( 2, ( #92292, #46120, #84685, #29945, #70441, #92777, #30941, #14746, #62323, #77561, #84200, #61827, #23832 ),
 .UNSPECIFIED., .F., .T. ) 
 B_SPLINE_CURVE_WITH_KNOTS ( ( 3, 2, 2, 2, 2, 2, 3 ),
 ( 0.7375000000000000444, 0.7399999999999999911, 0.7449999999999999956, 0.7500000000000000000, 0.7550000000000000044, 0.7600000000000000089, 0.7625000000000000666 ),
 .UNSPECIFIED. ) 
 CURVE ( )  GEOMETRIC_REPRESENTATION_ITEM ( )  RATIONAL_B_SPLINE_CURVE ( ( 0.9755282581475767101, 0.9755282581475772652, 1.000000000000000000, 0.9510565162951535312, 1.000000000000000000, 0.9510565162951535312, 1.000000000000000000, 0.9510565162951535312, 1.000000000000000000, 0.9510565162951535312, 1.000000000000000000, 0.9755282581475761550, 0.9755282581475767101 ) ) 
 REPRESENTATION_ITEM ( '' )  );
#12930 = EDGE_CURVE ( 'NONE', #4371, #8415, #58696, .T. ) ;
#12931 = CARTESIAN_POINT ( 'NONE',  ( 15.05724179552094277, 20.64441083166259716, -10.00000000000000533 ) ) ;
#12932 = CARTESIAN_POINT ( 'NONE',  ( 192.0604745424677446, 287.4852189256589554, -16.59597026331354286 ) ) ;
#12933 = EDGE_LOOP ( 'NONE', ( #3732, #59001, #80770, #93215 ) ) ;
#12934 = LINE ( 'NONE', #67598, #31996 ) ;
#12935 = EDGE_CURVE ( 'NONE', #69469, #65627, #12637, .T. ) ;
#12936 = CARTESIAN_POINT ( 'NONE',  ( 86.50330892798304205, 47.09883604031134752, -10.56546389670382169 ) ) ;
#12937 = CARTESIAN_POINT ( 'NONE',  ( 159.7314908411816248, 264.1435442130865567, -17.48313506953057939 ) ) ;
#12938 = ORIENTED_EDGE ( 'NONE', *, *, #78890, .F. ) ;
#12939 = AXIS2_PLACEMENT_3D ( 'NONE', #33763, #87526, #95092 ) ;
#12940 = CARTESIAN_POINT ( 'NONE',  ( 147.1731211915891322, 275.7356719181125868, 0.5879280619134324981 ) ) ;
#12941 = CARTESIAN_POINT ( 'NONE',  ( 185.7591078734260464, 291.2087897148937827, 12.17200245411944692 ) ) ;
#12942 = CARTESIAN_POINT ( 'NONE',  ( 204.1953342137782954, 276.9703018036655067, 13.84727111424505885 ) ) ;
#12943 = CARTESIAN_POINT ( 'NONE',  ( 7.864685750751951865, 30.05722773587472929, 10.00000000000000000 ) ) ;
#12944 = VERTEX_POINT ( 'NONE', #90161 ) ;
#12945 = CARTESIAN_POINT ( 'NONE',  ( 81.04025856027610075, 229.8464784336661637, 1.353441290958777525E-15 ) ) ;
#12946 = CARTESIAN_POINT ( 'NONE',  ( 203.2362765626855889, 278.6314383827457846, 14.95873044600159929 ) ) ;
#12947 = CARTESIAN_POINT ( 'NONE',  ( 181.2982806733463974, 271.4113319947247760, -17.41859542398102434 ) ) ;
#12948 = CARTESIAN_POINT ( 'NONE',  ( 181.8697498269454513, 257.4598785196697008, -6.014196373383785321 ) ) ;
#12949 = ORIENTED_EDGE ( 'NONE', *, *, #86723, .F. ) ;
#12950 = ORIENTED_EDGE ( 'NONE', *, *, #46025, .T. ) ;
#12951 = CARTESIAN_POINT ( 'NONE',  ( 196.1252721995043942, 284.4712197134549001, -17.81715240067734030 ) ) ;
#12952 = VERTEX_POINT ( 'NONE', #20733 ) ;
#12953 = CARTESIAN_POINT ( 'NONE',  ( 80.88463073246907697, 48.08410267114198433, 13.33332236086108580 ) ) ;
#12954 = EDGE_LOOP ( 'NONE', ( #76120, #6071, #12197, #27432 ) ) ;
#12955 = CARTESIAN_POINT ( 'NONE',  ( 45.66470909604093720, 114.5311720768849995, -10.00000000000000000 ) ) ;
#12957 = CARTESIAN_POINT ( 'NONE',  ( 154.8786460229866577, 262.3893114111486398, -18.06164891362396929 ) ) ;
#12956 = AXIS2_PLACEMENT_3D ( 'NONE', #25062, #77269, #40749 ) ;
#12958 = ORIENTED_EDGE ( 'NONE', *, *, #17895, .F. ) ;
#12959 = DIRECTION ( 'NONE',  ( -0.000000000000000000, 1.000000000000000000, -0.000000000000000000 ) ) ;
#12960 = ADVANCED_FACE ( 'NONE', ( #51618 ), #82573, .T. ) ;
#12961 = CARTESIAN_POINT ( 'NONE',  ( 148.7588072053147243, 273.7711778218048835, -8.803803025135483296 ) ) ;
#12962 = DIRECTION ( 'NONE',  ( -0.8660254037844384856, -0.5000000000000002220, -3.252519625699449945E-16 ) ) ;
#12963 = CARTESIAN_POINT ( 'NONE',  ( -23.57869195597365319, 99.67400356242829673, 45.19938701403189896 ) ) ;
#12964 = CARTESIAN_POINT ( 'NONE',  ( 72.26211198664731228, 68.26187575085410231, -10.17965940589137830 ) ) ;
#12965 = CARTESIAN_POINT ( 'NONE',  ( 156.8158635136204850, 259.0339522920597233, -18.23857867748462880 ) ) ;
#12966 = ORIENTED_EDGE ( 'NONE', *, *, #67208, .F. ) ;
#12967 = CARTESIAN_POINT ( 'NONE',  ( 76.78200948252425917, 60.31104682374800774, 15.82330234246767731 ) ) ;
#12968 = CARTESIAN_POINT ( 'NONE',  ( 12.27453364332850505, 12.80170272979924739, 7.433330006724137462 ) ) ;
#12969 = ORIENTED_EDGE ( 'NONE', *, *, #93756, .F. ) ;
#12970 = VECTOR ( 'NONE', #49657, 1000.000000000000227 ) ;
#12971 = DIRECTION ( 'NONE',  ( 0.1860369090530955005, 0.9825427565607363078, 0.000000000000000000 ) ) ;
#12973 = ORIENTED_EDGE ( 'NONE', *, *, #98728, .F. ) ;
#12972 = CARTESIAN_POINT ( 'NONE',  ( 200.1387068151675237, 270.2636360650371330, 9.266071134921585184 ) ) ;
#12974 = CARTESIAN_POINT ( 'NONE',  ( -15.07180212829954158, 105.6728077113080673, 10.93289567214266711 ) ) ;
#12975 = CARTESIAN_POINT ( 'NONE',  ( 181.4433080673849474, 255.1351033649908402, 0.7872376121522187686 ) ) ;
#12976 = CARTESIAN_POINT ( 'NONE',  ( 188.9516232634142909, 259.5449388965931234, 2.625812016075142807 ) ) ;
#12977 = CARTESIAN_POINT ( 'NONE',  ( 160.8219329449452744, 281.1493571213889027, -6.602944771620161468 ) ) ;
#12978 = CARTESIAN_POINT ( 'NONE',  ( 164.6573736076317402, 246.3298132620209060, -1.876867566021173328 ) ) ;
#12979 = CARTESIAN_POINT ( 'NONE',  ( 157.6552178212553486, 258.0004517741330687, 16.70547076031876088 ) ) ;
#12980 = B_SPLINE_CURVE_WITH_KNOTS ( 'NONE', 3,
 ( #53368, #14865, #60960, #23453 ),
 .UNSPECIFIED., .F., .F.,
 ( 4, 4 ),
 ( 0.0002127203767480665916, 0.005436920270846633783 ),
 .UNSPECIFIED. ) ;
#12981 = CARTESIAN_POINT ( 'NONE',  ( 169.5829390051931966, 248.1378239353514914, -0.09087230163007473105 ) ) ;
#12982 = DIRECTION ( 'NONE',  ( 0.000000000000000000, 0.000000000000000000, 1.000000000000000000 ) ) ;
#12983 = EDGE_LOOP ( 'NONE', ( #25152, #72504, #13340, #57946 ) ) ;
#12984 = CARTESIAN_POINT ( 'NONE',  ( 181.7205532481384012, 270.6930945944329778, -16.08030108815028214 ) ) ;
#12985 = CARTESIAN_POINT ( 'NONE',  ( 66.04689650495228648, 69.25707841837410683, 0.2683665952402904398 ) ) ;
#12986 = ORIENTED_EDGE ( 'NONE', *, *, #32416, .F. ) ;
#12987 = CARTESIAN_POINT ( 'NONE',  ( 160.7513685639857783, 275.7766557047398805, 12.80917292314146572 ) ) ;
#12988 = CARTESIAN_POINT ( 'NONE',  ( -8.378993335088974703, 41.25363085138964436, 59.99999999999999289 ) ) ;
#12989 = CARTESIAN_POINT ( 'NONE',  ( 204.1357312349132087, 277.0735371913424387, -14.51687998123883716 ) ) ;
#12990 = CARTESIAN_POINT ( 'NONE',  ( -56.29836151245349640, 34.88994676555962826, -10.00000000000000000 ) ) ;
#12991 = EDGE_CURVE ( 'NONE', #28157, #34739, #36053, .T. ) ;
#12992 = CARTESIAN_POINT ( 'NONE',  ( 160.9438941661644549, 272.8970580874148482, 15.77033046387437842 ) ) ;
#12994 = CARTESIAN_POINT ( 'NONE',  ( 87.85678018468817640, 44.16677905111681923, 2.775409157791113746 ) ) ;
#12993 = CARTESIAN_POINT ( 'NONE',  ( -18.01139699756907930, 172.6589784336661637, -6.496448406907675876E-16 ) ) ;
#12995 = CARTESIAN_POINT ( 'NONE',  ( 165.0735250206753619, 246.7312630101393722, 5.989302113854410692 ) ) ;
#12996 = EDGE_LOOP ( 'NONE', ( #38849, #10868, #97075, #17240 ) ) ;
#12997 = ORIENTED_EDGE ( 'NONE', *, *, #7738, .F. ) ;
#12998 = CARTESIAN_POINT ( 'NONE',  ( -30.04356256989597185, 94.88921800892812541, 36.50000000000000000 ) ) ;
#12999 = CARTESIAN_POINT ( 'NONE',  ( 189.7410647174195901, 285.7743870009521743, -17.19896820403054605 ) ) ;
#13000 = CARTESIAN_POINT ( 'NONE',  ( 85.70478682239833290, 48.82600918481677610, -12.04570940814934410 ) ) ;
#13001 = CARTESIAN_POINT ( 'NONE',  ( 171.7934946240355600, 289.9441787457215582, 2.720480149874153764 ) ) ;
#13002 = CARTESIAN_POINT ( 'NONE',  ( 153.3616370783189211, 265.0168479788495688, 17.48287904751960653 ) ) ;
#13003 = CARTESIAN_POINT ( 'NONE',  ( 84.75487950562418860, 47.73074732454571745, 11.57677916824878750 ) ) ;
#13004 = CARTESIAN_POINT ( 'NONE',  ( 189.6666044902458168, 284.7049877867155487, 17.41007887138588117 ) ) ;
#13005 = CARTESIAN_POINT ( 'NONE',  ( 17.60459192459599365, 168.7202760586660020, -5.415160957724236172E-17 ) ) ;
#13006 = CARTESIAN_POINT ( 'NONE',  ( 99.93095832397169431, 222.3768266524160140, 9.188101187500098632 ) ) ;
#13007 = CARTESIAN_POINT ( 'NONE',  ( 48.42933654300943402, 188.7677522451417929, -5.000000000000041744 ) ) ;
#13008 = CARTESIAN_POINT ( 'NONE',  ( 186.7650389526093022, 295.9085115873210157, -7.616436736632654636 ) ) ;
#13010 = CARTESIAN_POINT ( 'NONE',  ( 78.93634411335234802, 55.84994475496723254, 16.12935936599136966 ) ) ;
#13009 = AXIS2_PLACEMENT_3D ( 'NONE', #23110, #25707, #57079 ) ;
#13011 = CARTESIAN_POINT ( 'NONE',  ( 177.9870452976290380, 283.3051803591353064, -14.47979671836508508 ) ) ;
#13012 = CARTESIAN_POINT ( 'NONE',  ( 190.7734523378904896, 299.7926839710546574, -4.885404362283661150 ) ) ;
#13013 = FACE_OUTER_BOUND ( 'NONE', #72216, .T. ) ;
#13014 = CARTESIAN_POINT ( 'NONE',  ( 181.1312229881957592, 273.4383946350568522, 16.62563511410547079 ) ) ;
#13015 = CARTESIAN_POINT ( 'NONE',  ( 148.1974503712686158, 273.9614817352322120, -7.884397846570731616 ) ) ;
#13016 = CARTESIAN_POINT ( 'NONE',  ( 84.15878383405946295, 50.51712059312899328, 13.75732096714377128 ) ) ;
#13017 = CARTESIAN_POINT ( 'NONE',  ( 196.2299774253775411, 266.0274705162634632, 8.373944587636422909 ) ) ;
#13018 = CARTESIAN_POINT ( 'NONE',  ( 53.86003751612224733, 195.2365022471902023, -10.00000000000009237 ) ) ;
#13019 = CARTESIAN_POINT ( 'NONE',  ( 162.4413493851164958, 251.9320596174019045, -12.94637656145141591 ) ) ;
#13020 = CARTESIAN_POINT ( 'NONE',  ( 47.32807415326522715, 108.5480133836684900, 10.00000000000000000 ) ) ;
#13021 = VECTOR ( 'NONE', #2776, 1000.000000000000000 ) ;
#13022 = CARTESIAN_POINT ( 'NONE',  ( 172.9387157878505263, 262.8721711101524079, -15.86194836379059225 ) ) ;
#13023 = CARTESIAN_POINT ( 'NONE',  ( 81.44681538588882574, 208.6423013555409796, -4.594050593750043987 ) ) ;
#13024 = CARTESIAN_POINT ( 'NONE',  ( 6.852252633650415703, 22.14336893147753571, 7.433330006724141015 ) ) ;
#13025 = CARTESIAN_POINT ( 'NONE',  ( 190.8604783348975502, 300.0669496974951471, 7.597731640149610222 ) ) ;
#13026 = CARTESIAN_POINT ( 'NONE',  ( 25.96864935082048831, 154.0458036431183189, 30.52142883766506998 ) ) ;
#13028 = CARTESIAN_POINT ( 'NONE',  ( 82.95114570043003255, 42.01829743365728831, -4.711341735647942564 ) ) ;
#13027 = CARTESIAN_POINT ( 'NONE',  ( 196.1241105319816143, 290.9500712997905794, 15.97146679939154268 ) ) ;
#13029 = CARTESIAN_POINT ( 'NONE',  ( 149.4009768994915248, 271.8769126400935079, 11.50055073237692049 ) ) ;
#13030 = CARTESIAN_POINT ( 'NONE',  ( 199.0756812798354645, 285.8378008023734083, -18.45377816087746936 ) ) ;
#13031 = PLANE ( 'NONE',  #55814 ) ;
#13032 = CARTESIAN_POINT ( 'NONE',  ( 34.04545031248176912, 37.84336893147759184, -7.433330006724137462 ) ) ;
#13033 = CARTESIAN_POINT ( 'NONE',  ( 146.9370072200009645, 276.1446333132804511, -3.799807221059707363 ) ) ;
#13034 = CARTESIAN_POINT ( 'NONE',  ( 86.46048006423905008, 47.32182001325401188, 10.26516935212321968 ) ) ;
#13035 = EDGE_LOOP ( 'NONE', ( #31391, #18954, #69585, #96311 ) ) ;
#13036 = CARTESIAN_POINT ( 'NONE',  ( 17.33597792084844258, 30.98502408145592213, -5.678558825948271327 ) ) ;
#13037 = CARTESIAN_POINT ( 'NONE',  ( 6.762080372528353145, 26.83705186507751961, 3.090169943749475401 ) ) ;
#13038 = CARTESIAN_POINT ( 'NONE',  ( 192.5076277540105423, 297.2140032159341558, -13.10094381206144298 ) ) ;
#13039 = LINE ( 'NONE', #65706, #34790 ) ;
#13040 = ORIENTED_EDGE ( 'NONE', *, *, #66674, .T. ) ;
#13041 = EDGE_CURVE ( 'NONE', #69843, #68477, #75082, .T. ) ;
#13042 = CARTESIAN_POINT ( 'NONE',  ( 70.99702552970684621, 61.08644655966345738, 14.50662264333758955 ) ) ;
#13043 = CARTESIAN_POINT ( 'NONE',  ( 198.4334039703542771, 286.9502577349437615, 18.47706603442866680 ) ) ;
#13044 = CARTESIAN_POINT ( 'NONE',  ( -25.04755574468711643, 23.27320705613571761, -10.00000000000000000 ) ) ;
#13045 = ADVANCED_FACE ( 'NONE', ( #85065 ), #21369, .T. ) ;
#13046 = DIRECTION ( 'NONE',  ( 0.000000000000000000, -0.000000000000000000, -1.000000000000000000 ) ) ;
#13047 = CARTESIAN_POINT ( 'NONE',  ( 138.2253456014562403, 260.6115022471903444, -5.000000000000047962 ) ) ;
#13048 = CARTESIAN_POINT ( 'NONE',  ( 88.30335668473479416, 44.31564768512615160, -2.101522154600196757 ) ) ;
#13049 = ORIENTED_EDGE ( 'NONE', *, *, #27670, .T. ) ;
#13050 = CARTESIAN_POINT ( 'NONE',  ( 91.29759403033908427, 223.5177522451418781, -10.00000000000009592 ) ) ;
#13051 = ORIENTED_EDGE ( 'NONE', *, *, #47220, .T. ) ;
#13052 = CARTESIAN_POINT ( 'NONE',  ( -22.42236680055709641, 157.8615022471902591, 0.000000000000000000 ) ) ;
#13053 = CARTESIAN_POINT ( 'NONE',  ( 84.60109600385015938, 42.34421550614859342, 2.521655685731596819 ) ) ;
#13054 = EDGE_CURVE ( 'NONE', #22165, #99984, #72511, .T. ) ;
#13055 = ORIENTED_EDGE ( 'NONE', *, *, #48308, .T. ) ;
#13056 = CYLINDRICAL_SURFACE ( 'NONE', #17627, 10.00000000000010658 ) ;
#13057 = ORIENTED_EDGE ( 'NONE', *, *, #52830, .F. ) ;
#13058 = CARTESIAN_POINT ( 'NONE',  ( 87.16490563351598553, 159.3552646834693292, 0.000000000000000000 ) ) ;
#13059 = CARTESIAN_POINT ( 'NONE',  ( 205.9504341145390924, 273.9303796031887259, 10.73680394385792525 ) ) ;
#13060 = CARTESIAN_POINT ( 'NONE',  ( 157.5065816067722722, 258.4198049196606917, -16.86844230480359741 ) ) ;
#13061 = CARTESIAN_POINT ( 'NONE',  ( 88.19817206715259772, 44.49282453600611831, -4.737833512016792703 ) ) ;
#13062 = CARTESIAN_POINT ( 'NONE',  ( 201.4066285247549786, 281.8004817444100354, -17.79749223817309201 ) ) ;
#13063 = CARTESIAN_POINT ( 'NONE',  ( -22.42236680055709641, 157.8615022471902591, 0.000000000000000000 ) ) ;
#13064 = CARTESIAN_POINT ( 'NONE',  ( 34.84170590957603508, 35.51421378149921537, -9.188101187500004485 ) ) ;
#13065 = CARTESIAN_POINT ( 'NONE',  ( 76.87832059550045471, 59.35088420047541291, -15.98204322003894973 ) ) ;
#13066 = CARTESIAN_POINT ( 'NONE',  ( 164.4948408606173302, 274.6928532213739800, 14.67008970210409657 ) ) ;
#13067 = EDGE_LOOP ( 'NONE', ( #40475, #39675, #71504, #96208, #62221, #13206, #66218 ) ) ;
#13068 = ORIENTED_EDGE ( 'NONE', *, *, #74460, .T. ) ;
#13069 = CARTESIAN_POINT ( 'NONE',  ( 182.3632850533476812, 274.9408504765579551, 17.79507043724071735 ) ) ;
#13071 = CARTESIAN_POINT ( 'NONE',  ( 194.1972774922283236, 294.2874440223457100, -15.09915398317898649 ) ) ;
#13070 = CARTESIAN_POINT ( 'NONE',  ( 67.00187114335926708, 67.08813303282481399, 8.529924657355548945 ) ) ;
#13072 = DIRECTION ( 'NONE',  ( -1.000000000000000000, 0.000000000000000000, 0.000000000000000000 ) ) ;
#13073 = CARTESIAN_POINT ( 'NONE',  ( 46.99867368304095550, 76.19044720721625197, -10.00000000000000000 ) ) ;
#13074 = CARTESIAN_POINT ( 'NONE',  ( 79.11723855630626190, 59.11194703662724237, -16.21433712332713029 ) ) ;
#13075 = CARTESIAN_POINT ( 'NONE',  ( 82.13265554904860721, 40.82714603808517495, 1.567016277279669412 ) ) ;
#13076 = CARTESIAN_POINT ( 'NONE',  ( 170.9887030610543661, 287.7172861656689520, -4.592964840281122285 ) ) ;
#13077 = CARTESIAN_POINT ( 'NONE',  ( 76.83812372118222811, 63.31165668814058023, -15.46182035231785079 ) ) ;
#13078 = CARTESIAN_POINT ( 'NONE',  ( 181.8344274857143432, 257.0251970467633669, 5.042215935203653743 ) ) ;
#13079 = CARTESIAN_POINT ( 'NONE',  ( 105.6144235841895664, 219.5327760586659451, 1.948934522072303157E-15 ) ) ;
#13080 = EDGE_LOOP ( 'NONE', ( #63896, #55019, #97428, #54159, #97201, #49040, #32426, #9591 ) ) ;
#13081 = LINE ( 'NONE', #82996, #2679 ) ;
#13082 = CARTESIAN_POINT ( 'NONE',  ( 165.0450258753809294, 270.9524041312169516, 16.77974215795885016 ) ) ;
#13083 = CARTESIAN_POINT ( 'NONE',  ( 179.5846872273510826, 291.4261084640538115, -10.07075702116988758 ) ) ;
#13084 = ORIENTED_EDGE ( 'NONE', *, *, #36055, .F. ) ;
#13085 = EDGE_LOOP ( 'NONE', ( #88154, #16129, #23924, #66897 ) ) ;
#13086 = CARTESIAN_POINT ( 'NONE',  ( 185.4241002709785846, 298.2501943955377328, -2.445652077582521233 ) ) ;
#13087 = CARTESIAN_POINT ( 'NONE',  ( -29.34079512516344934, 35.93620001148155296, 59.99999999999999289 ) ) ;
#13088 = CARTESIAN_POINT ( 'NONE',  ( 164.7199312521631214, 249.0629007997009126, 10.02713358784743747 ) ) ;
#13089 = CARTESIAN_POINT ( 'NONE',  ( 66.97748580466556234, 68.05911003901715617, 6.908000617270682042 ) ) ;
#13090 = CARTESIAN_POINT ( 'NONE',  ( 79.99999999999998579, 14.99999999999998934, 59.99999999999999289 ) ) ;
#13091 = ORIENTED_EDGE ( 'NONE', *, *, #79614, .F. ) ;
#13092 = VECTOR ( 'NONE', #72623, 1000.000000000000114 ) ;
#13093 = EDGE_LOOP ( 'NONE', ( #90102, #1495, #15262, #82142 ) ) ;
#13094 = B_SPLINE_CURVE_WITH_KNOTS ( 'NONE', 3,
 ( #43171, #73608, #35090, #57390, #41687, #65994, #65008, #95951, #96947, #27513, #51279, #88364, #12821 ),
 .UNSPECIFIED., .F., .F.,
 ( 4, 3, 3, 3, 4 ),
 ( 0.000000000000000000, 0.1333490885032349305, 0.3007194338854379256, 0.4699862290245218621, 0.4976065956401893864 ),
 .UNSPECIFIED. ) ;
#13095 = CARTESIAN_POINT ( 'NONE',  ( 207.6875671281972870, 270.9215769640275653, -2.211577121115235300 ) ) ;
#13096 = ORIENTED_EDGE ( 'NONE', *, *, #60680, .F. ) ;
#13097 = CARTESIAN_POINT ( 'NONE',  ( 191.9465615534260792, 264.5235098129936091, -7.852620813520595711 ) ) ;
#13098 = CARTESIAN_POINT ( 'NONE',  ( 24.36335893204212155, 173.3262482093457777, 3.021315404115420679E-15 ) ) ;
#13099 = ADVANCED_FACE ( 'NONE', ( #20889 ), #87493, .T. ) ;
#13100 = CARTESIAN_POINT ( 'NONE',  ( 48.98007068238331385, 88.97864505566217019, 10.00000000000000000 ) ) ;
#13102 = CARTESIAN_POINT ( 'NONE',  ( 69.58015593410982547, 62.56871313314800176, -13.92720401298870314 ) ) ;
#13101 = CARTESIAN_POINT ( 'NONE',  ( 144.5855667544892924, 242.0327760586659451, 1.948934522072303157E-15 ) ) ;
#13103 = CARTESIAN_POINT ( 'NONE',  ( 71.88281838930642209, 59.56282477439597045, -15.74156321294393024 ) ) ;
#13104 = EDGE_LOOP ( 'NONE', ( #26260, #81765, #40737, #42428 ) ) ;
#13105 = CARTESIAN_POINT ( 'NONE',  ( 147.5498377207569263, 275.0831797495432056, 4.097967709737811326 ) ) ;
#13106 = DIRECTION ( 'NONE',  ( -0.8660254037844387076, -0.4999999999999998890, -0.000000000000000000 ) ) ;
#13107 = CARTESIAN_POINT ( 'NONE',  ( 190.1998581979997311, 263.5875986082893405, -9.717754213320489498 ) ) ;
#13108 = CARTESIAN_POINT ( 'NONE',  ( 173.2404090740162133, 251.6421966675173678, -0.2950645122926903730 ) ) ;
#13109 = CARTESIAN_POINT ( 'NONE',  ( 178.3382078955913528, 285.3547819717112475, 13.04039342192868745 ) ) ;
#13110 = CARTESIAN_POINT ( 'NONE',  ( -19.65312891409030271, 93.06504152958497400, -59.99999999999999289 ) ) ;
#13111 = EDGE_CURVE ( 'NONE', #59762, #72864, #99157, .T. ) ;
#13112 = CARTESIAN_POINT ( 'NONE',  ( 199.0831254908205210, 281.9212699178648904, -16.61011480125563011 ) ) ;
#13113 = FACE_OUTER_BOUND ( 'NONE', #15810, .T. ) ;
#13114 = CARTESIAN_POINT ( 'NONE',  ( 79.58915790851577299, 48.58846474191479814, 14.00006715458789408 ) ) ;
#13115 = CARTESIAN_POINT ( 'NONE',  ( 68.72531525883097459, 70.03068556548458901, -2.698007717796147009 ) ) ;
#13116 = CARTESIAN_POINT ( 'NONE',  ( 52.13666070897046012, 213.1589784336661637, -6.496448406907675876E-16 ) ) ;
#13117 = CARTESIAN_POINT ( 'NONE',  ( 206.1062572280473546, 273.6604860535989587, -9.773577984388410300 ) ) ;
#13118 = CARTESIAN_POINT ( 'NONE',  ( 77.65745049418580948, 61.93790999624750526, 15.64425804037917977 ) ) ;
#13119 = CARTESIAN_POINT ( 'NONE',  ( 162.6396274730868186, 248.9468972229755082, -10.26162218571527518 ) ) ;
#13120 = EDGE_CURVE ( 'NONE', #7544, #63230, #13391, .T. ) ;
#13121 = CARTESIAN_POINT ( 'NONE',  ( 19.39689925177878749, 34.96947112835012916, -10.00000000000000000 ) ) ;
#13122 = LINE ( 'NONE', #59688, #54631 ) ;
#13124 = PLANE ( 'NONE',  #33409 ) ;
#13123 = B_SPLINE_CURVE_WITH_KNOTS ( 'NONE', 3,
 ( #25948, #19362, #95882, #18347, #50222, #88291, #56822, #87805, #11256, #41615, #49240, #42119, #51207, #73052, #12238, #4628, #57319, #4121, #81176, #49724, #80175, #11742, #73538, #35015, #65915, #66422, #19840, #27440, #50711, #81665, #43098, #97352, #97842, #5128, #36508, #44096, #28411, #14218, #52202, #45595, #29911, #67412, #44594, #51735, #76525, #98840 ),
 .UNSPECIFIED., .F., .F.,
 ( 4, 1, 1, 1, 2, 2, 1, 1, 1, 2, 2, 1, 1, 2, 2, 1, 1, 2, 2, 1, 1, 2, 2, 1, 2, 2, 1, 2, 2, 4 ),
 ( 0.000000000000000000, 0.06249999999998591405, 0.09374999999997879474, 0.1093749999999743955, 0.1171874999999721056, 0.1249999999999698158, 0.1874999999999572009, 0.2187499999999528988, 0.2343749999999486244, 0.2421874999999465150, 0.2499999999999444333, 0.3124999999999362177, 0.3437499999999322209, 0.3593749999999303335, 0.3749999999999283906, 0.4374999999999171774, 0.4687499999999125144, 0.4843749999999111822, 0.4999999999999098499, 0.5624999999999139577, 0.5937499999999159561, 0.6093749999999177325, 0.6249999999999195088, 0.6874999999999310552, 0.7187499999999377165, 0.7499999999999442668, 0.8124999999999570344, 0.8437499999999632516, 0.8749999999999695799, 1.000000000000000000 ),
 .UNSPECIFIED. ) ;
#13125 = CARTESIAN_POINT ( 'NONE',  ( 172.9897703034535539, 283.7959595487852766, 13.73707729917544285 ) ) ;
#13126 = DIRECTION ( 'NONE',  ( 0.000000000000000000, 0.000000000000000000, 1.000000000000000000 ) ) ;
#13127 = CARTESIAN_POINT ( 'NONE',  ( 78.70150085959764397, 59.83202584994826623, 16.12694553795978081 ) ) ;
#13128 = LINE ( 'NONE', #14612, #83498 ) ;
#13129 = CARTESIAN_POINT ( 'NONE',  ( 84.14312167556933275, 48.98415679381830756, 0.000000000000000000 ) ) ;
#13130 = CARTESIAN_POINT ( 'NONE',  ( 19.71535529843806245, 176.0643266524160424, 9.188101187500095079 ) ) ;
#13131 = CARTESIAN_POINT ( 'NONE',  ( 45.99364009841357159, 197.3615022471902591, -10.00000000000009592 ) ) ;
#13132 = ORIENTED_EDGE ( 'NONE', *, *, #7938, .T. ) ;
#13133 = CARTESIAN_POINT ( 'NONE',  ( 196.4994169513186364, 290.3000215130921902, 16.82935102260526961 ) ) ;
#13134 = CARTESIAN_POINT ( 'NONE',  ( 202.1030944152313111, 278.9078238741668656, 15.49021988960157792 ) ) ;
#13135 = CARTESIAN_POINT ( 'NONE',  ( 76.68698272566328455, 51.55172097108391682, -15.61692696388005253 ) ) ;
#13136 = CARTESIAN_POINT ( 'NONE',  ( 163.8455942243524248, 246.8581015375447691, -7.178103170949780676 ) ) ;
#13137 = CARTESIAN_POINT ( 'NONE',  ( 71.50396643458246615, 72.35543200887750004, -1.254608710098219060 ) ) ;
#13138 = CARTESIAN_POINT ( 'NONE',  ( 44.34243207491051209, 208.6589784336661921, -6.496448406907676862E-16 ) ) ;
#13139 = CARTESIAN_POINT ( 'NONE',  ( 161.7101619467568980, 250.5567787384628389, 13.05644392949610655 ) ) ;
#13140 = CARTESIAN_POINT ( 'NONE',  ( 171.0964841634227298, 287.0058847005474263, 7.064598226519137825 ) ) ;
#13141 = CARTESIAN_POINT ( 'NONE',  ( 147.5848197185516142, 275.0225891520124151, 4.420251097676741736 ) ) ;
#13142 = CARTESIAN_POINT ( 'NONE',  ( 38.90461549961826648, 38.16454794089044356, -10.00000000000000355 ) ) ;
#13143 = CARTESIAN_POINT ( 'NONE',  ( 203.2428933715266623, 269.5665350485680278, -7.504532614354034514 ) ) ;
#13144 = CARTESIAN_POINT ( 'NONE',  ( 74.83655476910678317, 53.51806293180211327, 16.54630480343736210 ) ) ;
#13145 = CARTESIAN_POINT ( 'NONE',  ( 177.5660330061924128, 275.6111645067952622, 16.43781890528649114 ) ) ;
#13146 = CARTESIAN_POINT ( 'NONE',  ( 73.27736499958758998, 63.96510177322678459, 13.82219565750662937 ) ) ;
#13147 = CARTESIAN_POINT ( 'NONE',  ( 67.15772368909350121, 67.74692886573922124, -6.548511843863573212 ) ) ;
#13148 = EDGE_CURVE ( 'NONE', #3917, #82089, #22938, .T. ) ;
#13149 = CARTESIAN_POINT ( 'NONE',  ( 163.6657122372590720, 255.3124181700179918, -14.98584762205334542 ) ) ;
#13150 = VECTOR ( 'NONE', #32611, 999.9999999999998863 ) ;
#13151 = CARTESIAN_POINT ( 'NONE',  ( 204.6823371430232896, 272.9704135290961062, -9.754921121218281144 ) ) ;
#13152 = FACE_OUTER_BOUND ( 'NONE', #53976, .T. ) ;
#13153 = CARTESIAN_POINT ( 'NONE',  ( 106.6154183633243377, 222.3615022471902023, 5.000000000000051514 ) ) ;
#13154 = CARTESIAN_POINT ( 'NONE',  ( 200.5438717407500917, 283.2948203288816558, 18.39667691545567152 ) ) ;
#13155 = CARTESIAN_POINT ( 'NONE',  ( 40.60966550219796289, 208.6868197944957330, -18.47570218321542868 ) ) ;
#13156 = ORIENTED_EDGE ( 'NONE', *, *, #12807, .T. ) ;
#13157 = CARTESIAN_POINT ( 'NONE',  ( 59.38997056143013964, 205.0958772461660828, -9.188101187500095079 ) ) ;
#13158 = ORIENTED_EDGE ( 'NONE', *, *, #27655, .F. ) ;
#13159 = EDGE_CURVE ( 'NONE', #68463, #76483, #13511, .T. ) ;
#13160 = DIRECTION ( 'NONE',  ( -0.8660254037844387076, -0.4999999999999998890, -0.000000000000000000 ) ) ;
#13161 = CARTESIAN_POINT ( 'NONE',  ( -19.65312891409030271, 93.06504152958497400, -10.00000000000000888 ) ) ;
#13162 = DIRECTION ( 'NONE',  ( 0.000000000000000000, 0.000000000000000000, 1.000000000000000000 ) ) ;
#13163 = EDGE_CURVE ( 'NONE', #51434, #24006, #2280, .T. ) ;
#13164 = EDGE_LOOP ( 'NONE', ( #58063, #86998, #92589, #84661 ) ) ;
#13165 = CARTESIAN_POINT ( 'NONE',  ( -71.61465314115659453, 63.06504152958490295, -45.00000000000001421 ) ) ;
#13166 = CARTESIAN_POINT ( 'NONE',  ( 79.18000070754021635, 45.80091866078065976, -13.04680284947386681 ) ) ;
#13167 = CARTESIAN_POINT ( 'NONE',  ( 71.84864803011454626, 61.11459157905925110, 15.23051327526690990 ) ) ;
#13168 = CARTESIAN_POINT ( 'NONE',  ( 35.44910642356613550, 21.26216523072496045, -2.296566073217252530E-15 ) ) ;
#13169 = CARTESIAN_POINT ( 'NONE',  ( 185.9748738598958369, 262.9711142029209441, 11.36824966179820251 ) ) ;
#13170 = CARTESIAN_POINT ( 'NONE',  ( 148.9831146496684084, 272.6006712873522133, -12.63706091291043343 ) ) ;
#13171 = CARTESIAN_POINT ( 'NONE',  ( 157.2470923712064348, 258.2870420010311250, 16.90933983342926439 ) ) ;
#13172 = EDGE_LOOP ( 'NONE', ( #23606, #33904, #89932, #28744 ) ) ;
#13173 = CARTESIAN_POINT ( 'NONE',  ( 19.08967936351193373, 31.99752408145592497, 5.678558825948276656 ) ) ;
#13174 = CARTESIAN_POINT ( 'NONE',  ( 76.49863583581506532, 63.42625474237735261, 14.98000607567798070 ) ) ;
#13175 = CARTESIAN_POINT ( 'NONE',  ( 70.23435920221514550, 70.16979271778447469, -5.338967590826342757 ) ) ;
#13176 = CARTESIAN_POINT ( 'NONE',  ( 11.78502771447809394, 29.73705186507753240, -3.090169943749475845 ) ) ;
#13177 = EDGE_LOOP ( 'NONE', ( #40247, #63883, #63594, #53875, #2482 ) ) ;
#13178 = CARTESIAN_POINT ( 'NONE',  ( 182.3585487608926883, 284.1109264421751277, 14.96762621272966243 ) ) ;
#13179 = CARTESIAN_POINT ( 'NONE',  ( 151.4384131719918685, 268.3479694989391078, 14.98299707687648841 ) ) ;
#13180 = CARTESIAN_POINT ( 'NONE',  ( 38.90713653809340400, 79.99999999999998579, 54.99999999999999289 ) ) ;
#13181 = ORIENTED_EDGE ( 'NONE', *, *, #82689, .F. ) ;
#13182 = EDGE_LOOP ( 'NONE', ( #62104, #14432, #9856, #38700 ) ) ;
#13184 = DIRECTION ( 'NONE',  ( 0.000000000000000000, 0.000000000000000000, 1.000000000000000000 ) ) ;
#13183 = CARTESIAN_POINT ( 'NONE',  ( 159.5335386611425861, 282.9547953765525108, -3.344663661812444566 ) ) ;
#13185 = CARTESIAN_POINT ( 'NONE',  ( 149.1939152435731728, 272.2355539484436235, -11.44223522189843933 ) ) ;
#13186 = CARTESIAN_POINT ( 'NONE',  ( 66.08197961146748867, 68.50086866870223901, -2.540402597524118455 ) ) ;
#13187 = CARTESIAN_POINT ( 'NONE',  ( 159.2111180226792726, 254.8852497853115722, 16.01057445397460910 ) ) ;
#13188 = DIRECTION ( 'NONE',  ( -0.8660254037844378194, -0.5000000000000014433, -0.000000000000000000 ) ) ;
#13189 = CARTESIAN_POINT ( 'NONE',  ( 161.0784938446909393, 262.9894285514246235, -17.68042406554819834 ) ) ;
#13190 = CARTESIAN_POINT ( 'NONE',  ( 126.3172359758225554, 252.9244531367911293, -4.594050593750046652 ) ) ;
#13191 = CARTESIAN_POINT ( 'NONE',  ( 123.0902549634681407, 230.3262482093458061, 3.021315404115420679E-15 ) ) ;
#13192 = VERTEX_POINT ( 'NONE', #3287 ) ;
#13193 = CARTESIAN_POINT ( 'NONE',  ( 171.2823453295078195, 264.2191545540018183, 15.82956524986185798 ) ) ;
#13194 = CARTESIAN_POINT ( 'NONE',  ( 66.61587002248256795, 219.2677522451419065, -5.000000000000047962 ) ) ;
#13195 = VERTEX_POINT ( 'NONE', #33158 ) ;
#13196 = CARTESIAN_POINT ( 'NONE',  ( 149.1653648461108617, 275.5304674000249179, 7.618651205328232479 ) ) ;
#13197 = ORIENTED_EDGE ( 'NONE', *, *, #34417, .T. ) ;
#13198 = VERTEX_POINT ( 'NONE', #86420 ) ;
#13199 = FACE_BOUND ( 'NONE', #1885, .T. ) ;
#13200 = CARTESIAN_POINT ( 'NONE',  ( 75.14783087284527596, 67.02178724657008502, -12.71884470538153877 ) ) ;
#13201 = CARTESIAN_POINT ( 'NONE',  ( 64.39641960523518094, 217.1744531367911293, 4.594050593750047540 ) ) ;
#13202 = CARTESIAN_POINT ( 'NONE',  ( -30.10073558955866702, 95.30624366923747459, 12.73418565006493175 ) ) ;
#13203 = CARTESIAN_POINT ( 'NONE',  ( -19.65312891409030271, 93.06504152958497400, 59.99999999999999289 ) ) ;
#13204 = CARTESIAN_POINT ( 'NONE',  ( 193.9401685343300699, 294.7327698005063326, 14.01047396938887069 ) ) ;
#13205 = CARTESIAN_POINT ( 'NONE',  ( 175.7203579514784053, 278.2834176361697587, 16.78628766804663996 ) ) ;
#13206 = ORIENTED_EDGE ( 'NONE', *, *, #73082, .F. ) ;
#13207 =( BOUNDED_CURVE ( )  B_SPLINE_CURVE ( 2, ( #8069, #63257, #94198, #71377, #40932, #1966, #25254, #85615, #87135, #93698, #31839, #79506, #963 ),
 .UNSPECIFIED., .F., .T. ) 
 B_SPLINE_CURVE_WITH_KNOTS ( ( 3, 2, 2, 2, 2, 2, 3 ),
 ( 0.8375000000000000222, 0.8399999999999999689, 0.8449999999999999734, 0.8499999999999999778, 0.8549999999999999822, 0.8599999999999999867, 0.8625000000000000444 ),
 .UNSPECIFIED. ) 
 CURVE ( )  GEOMETRIC_REPRESENTATION_ITEM ( )  RATIONAL_B_SPLINE_CURVE ( ( 0.9755282581475767101, 0.9755282581475772652, 1.000000000000000000, 0.9510565162951535312, 1.000000000000000000, 0.9510565162951535312, 1.000000000000000000, 0.9510565162951535312, 1.000000000000000000, 0.9510565162951535312, 1.000000000000000000, 0.9755282581475761550, 0.9755282581475767101 ) ) 
 REPRESENTATION_ITEM ( '' )  );
#13208 = CARTESIAN_POINT ( 'NONE',  ( 71.38275130371390276, 63.94649258510062850, -13.17855260962158326 ) ) ;
#13209 = B_SPLINE_CURVE_WITH_KNOTS ( 'NONE', 3,
 ( #81832, #88462, #41277, #42278 ),
 .UNSPECIFIED., .F., .F.,
 ( 4, 4 ),
 ( 0.008185576491779684646, 0.01406236705198208627 ),
 .UNSPECIFIED. ) ;
#13210 = CARTESIAN_POINT ( 'NONE',  ( 201.3715986869907510, 281.8611552031986776, -17.89433714524984964 ) ) ;
#13211 = CARTESIAN_POINT ( 'NONE',  ( 155.6328838216860220, 261.0829332228125850, -17.51014940606912518 ) ) ;
#13212 = ORIENTED_EDGE ( 'NONE', *, *, #26317, .T. ) ;
#13213 = CARTESIAN_POINT ( 'NONE',  ( -15.29569941879559281, 168.6427522451419350, -10.00000000000009592 ) ) ;
#13214 = CARTESIAN_POINT ( 'NONE',  ( 76.05516770966454487, 51.24013347110783201, -16.11765975597679912 ) ) ;
#13215 = CARTESIAN_POINT ( 'NONE',  ( 174.0844628251548727, 253.6050010518140994, -7.541462950351128569 ) ) ;
#13216 = CARTESIAN_POINT ( 'NONE',  ( 80.67108465943677231, 56.43556366967433746, 16.52050149510320765 ) ) ;
#13217 = CARTESIAN_POINT ( 'NONE',  ( 164.4494343874829099, 245.8122196953522121, 2.922779519406129456 ) ) ;
#13218 = ADVANCED_FACE ( 'NONE', ( #40239 ), #71685, .T. ) ;
#13219 = CARTESIAN_POINT ( 'NONE',  ( 149.2923684163597784, 272.0650280510108701, -12.99082738998495756 ) ) ;
#13220 = CARTESIAN_POINT ( 'NONE',  ( 154.8782533782051871, 264.3899914918594050, -17.45241046926759765 ) ) ;
#13221 = ORIENTED_EDGE ( 'NONE', *, *, #3285, .F. ) ;
#13222 = CARTESIAN_POINT ( 'NONE',  ( 207.8060684685902686, 270.7163266217015689, 2.015725026008670540 ) ) ;
#13223 = CARTESIAN_POINT ( 'NONE',  ( 128.9153121871758572, 254.4244531367911293, -4.594050593750046652 ) ) ;
#13224 = VERTEX_POINT ( 'NONE', #17979 ) ;
#13225 = CARTESIAN_POINT ( 'NONE',  ( -7.836314268245596182, 177.8297689869269220, -2.679491924311252493 ) ) ;
#13226 = CARTESIAN_POINT ( 'NONE',  ( 182.2900984803647475, 257.5098244155703355, 6.713694854764257869 ) ) ;
#13227 = EDGE_CURVE ( 'NONE', #1997, #97187, #33673, .T. ) ;
#13228 = CARTESIAN_POINT ( 'NONE',  ( 88.02868988710136477, 43.76708177457258842, -2.199075477856099692 ) ) ;
#13229 =( BOUNDED_CURVE ( )  B_SPLINE_CURVE ( 2, ( #39134, #24950, #30566, #15850, #84799, #23950, #40139, #47253, #660, #69052, #85831, #99983, #61452 ),
 .UNSPECIFIED., .F., .T. ) 
 B_SPLINE_CURVE_WITH_KNOTS ( ( 3, 2, 2, 2, 2, 2, 3 ),
 ( 0.1875000000000000000, 0.1900000000000000022, 0.1950000000000000067, 0.2000000000000000111, 0.2049999999999999878, 0.2099999999999999922, 0.2124999999999999944 ),
 .UNSPECIFIED. ) 
 CURVE ( )  GEOMETRIC_REPRESENTATION_ITEM ( )  RATIONAL_B_SPLINE_CURVE ( ( 0.9755282581475768211, 0.9755282581475768211, 1.000000000000000000, 0.9510565162951535312, 1.000000000000000000, 0.9510565162951535312, 1.000000000000000000, 0.9510565162951535312, 1.000000000000000000, 0.9510565162951535312, 1.000000000000000000, 0.9755282581475768211, 0.9755282581475768211 ) ) 
 REPRESENTATION_ITEM ( '' )  );
#13230 = CARTESIAN_POINT ( 'NONE',  ( 72.97386446981147401, 70.68132344495337804, 8.316175787459503255 ) ) ;
#13231 = CARTESIAN_POINT ( 'NONE',  ( -22.42236680055709641, 157.8615022471902591, 0.000000000000000000 ) ) ;
#13232 = AXIS2_PLACEMENT_3D ( 'NONE', #22354, #77042, #37540 ) ;
#13233 = CARTESIAN_POINT ( 'NONE',  ( 183.4480379275034920, 257.0748008084844400, -5.332061893044733658 ) ) ;
#13234 = ORIENTED_EDGE ( 'NONE', *, *, #54762, .T. ) ;
#13235 = CARTESIAN_POINT ( 'NONE',  ( 49.66226845319756222, 83.29899382260624918, 177.5919119679930134 ) ) ;
#13236 = CARTESIAN_POINT ( 'NONE',  ( 182.1086373701226933, 275.6374269030367827, -16.43891936414332733 ) ) ;
#13237 = CARTESIAN_POINT ( 'NONE',  ( 158.6496056213609904, 257.8578177934796258, 17.38082990300775776 ) ) ;
#13238 = CARTESIAN_POINT ( 'NONE',  ( 81.12147712725017357, 52.00152150211298618, 15.09009577504130029 ) ) ;
#13239 = CARTESIAN_POINT ( 'NONE',  ( 202.1505501530674849, 267.6816150296156138, 0.8512892188848613095 ) ) ;
#13240 = EDGE_CURVE ( 'NONE', #47570, #34846, #48373, .T. ) ;
#13241 = CARTESIAN_POINT ( 'NONE',  ( 146.8000281410530192, 276.3818880375922049, 4.652863924796177386 ) ) ;
#13242 = CARTESIAN_POINT ( 'NONE',  ( 185.7490732957863031, 282.1293503020006028, 16.17923647030573875 ) ) ;
#13243 = CARTESIAN_POINT ( 'NONE',  ( 204.9463377925012253, 275.6695254486514841, -14.15865086131798378 ) ) ;
#13244 = CARTESIAN_POINT ( 'NONE',  ( 196.1276372599845388, 270.7547217853674510, 12.00612363897915991 ) ) ;
#13245 = EDGE_CURVE ( 'NONE', #15824, #22001, #19968, .T. ) ;
#13246 = CARTESIAN_POINT ( 'NONE',  ( 26.31557204471864253, 27.14441083166262203, 10.00000000000000533 ) ) ;
#13247 = EDGE_CURVE ( 'NONE', #20907, #75140, #35653, .T. ) ;
#13248 = CARTESIAN_POINT ( 'NONE',  ( 190.0445576990143195, 301.4801656937889902, 4.140328216824785912 ) ) ;
#13249 = CARTESIAN_POINT ( 'NONE',  ( 80.17564311316536418, 205.5494855054051584, -2.679491924311248496 ) ) ;
#13250 = CARTESIAN_POINT ( 'NONE',  ( 69.62482084542597249, 69.32845382139950630, -7.406819698113993766 ) ) ;
#13251 = CARTESIAN_POINT ( 'NONE',  ( 198.4334039703542771, 286.9502577349437615, 18.47706603442866680 ) ) ;
#13252 = CARTESIAN_POINT ( 'NONE',  ( 207.4071614940804125, 271.4072537690463491, 6.386333739406530263 ) ) ;
#13253 = CARTESIAN_POINT ( 'NONE',  ( 144.5581563630821051, 244.2677522451417929, -5.000000000000041744 ) ) ;
#13254 = CARTESIAN_POINT ( 'NONE',  ( 176.0042927459173541, 285.4150976940742339, -11.97940611282195711 ) ) ;
#13255 = ORIENTED_EDGE ( 'NONE', *, *, #98161, .T. ) ;
#13256 = CARTESIAN_POINT ( 'NONE',  ( 66.83852597929605110, 67.59941986568811956, -6.474490792332534994 ) ) ;
#13257 = CARTESIAN_POINT ( 'NONE',  ( 198.5201458116119397, 286.8000164587433005, -18.30276554821096013 ) ) ;
#13258 = CARTESIAN_POINT ( 'NONE',  ( 9.079046938504149011, 185.2369531367911293, -4.594050593750048428 ) ) ;
#13259 = CARTESIAN_POINT ( 'NONE',  ( 178.8948291856917194, 273.8999092347531246, -17.56902132216663404 ) ) ;
#13260 = CARTESIAN_POINT ( 'NONE',  ( 25.74102936209481385, 30.56454794089042437, 10.00000000000000355 ) ) ;
#13261 = CARTESIAN_POINT ( 'NONE',  ( 85.56872147382391347, 49.01729895498410627, 12.25953038224546887 ) ) ;
#13262 = CARTESIAN_POINT ( 'NONE',  ( 157.8159121039657293, 257.3018173235443555, -17.05074702406642118 ) ) ;
#13263 = PLANE ( 'NONE',  #54913 ) ;
#13264 = DIRECTION ( 'NONE',  ( -0.5242119900219301964, 0.000000000000000000, -0.8515878049369001168 ) ) ;
#13265 = ADVANCED_FACE ( 'NONE', ( #96500 ), #63939, .F. ) ;
#13266 = CARTESIAN_POINT ( 'NONE',  ( 169.4877538909896657, 257.6357214041063344, 13.73911095073034971 ) ) ;
#13267 = CARTESIAN_POINT ( 'NONE',  ( 7.313483791488072150, 163.4824982072973683, 3.021315404115420679E-15 ) ) ;
#13268 = CARTESIAN_POINT ( 'NONE',  ( 150.9982109096994520, 269.1104221828363734, 14.90714565999273766 ) ) ;
#13269 = EDGE_CURVE ( 'NONE', #93745, #709, #30037, .T. ) ;
#13270 = CARTESIAN_POINT ( 'NONE',  ( 179.1768322581812072, 294.1168262153754540, 1.049777515246110626 ) ) ;
#13271 = CARTESIAN_POINT ( 'NONE',  ( 57.25197034761130510, 193.8615022471901739, 5.000000000000051514 ) ) ;
#13272 = DIRECTION ( 'NONE',  ( -1.000000000000000000, 0.000000000000000000, 0.000000000000000000 ) ) ;
#13273 = CARTESIAN_POINT ( 'NONE',  ( 190.5969391768923913, 300.5234129089444650, -0.7564693504096553500 ) ) ;
#13274 = CARTESIAN_POINT ( 'NONE',  ( 24.31594170816038059, 184.8458772461660544, 9.188101187500095079 ) ) ;
#13275 = CARTESIAN_POINT ( 'NONE',  ( 165.1207195983944018, 284.8810180499550597, 4.168337116055295333 ) ) ;
#13276 = CARTESIAN_POINT ( 'NONE',  ( 79.25902298712658478, 59.95016084666949752, 16.14518600951581817 ) ) ;
#13277 = CARTESIAN_POINT ( 'NONE',  ( 39.01788588657935719, 31.03085787977765975, 9.188101187500006262 ) ) ;
#13278 = DIRECTION ( 'NONE',  ( -0.000000000000000000, -0.000000000000000000, -1.000000000000000000 ) ) ;
#13279 = CARTESIAN_POINT ( 'NONE',  ( 164.3524132573224392, 245.9802652221976587, -2.749586949851067441 ) ) ;
#13280 = EDGE_CURVE ( 'NONE', #66266, #99455, #31377, .T. ) ;
#13281 = CARTESIAN_POINT ( 'NONE',  ( 189.0748872544347421, 267.9482830477340940, 14.04708774900528923 ) ) ;
#13282 = CARTESIAN_POINT ( 'NONE',  ( 178.6026051973306323, 254.4708812555809345, 5.813106864979912913 ) ) ;
#13283 = CARTESIAN_POINT ( 'NONE',  ( 164.1573396782106329, 281.5441427519270974, 8.957208755700603930 ) ) ;
#13284 = DIRECTION ( 'NONE',  ( 0.000000000000000000, 0.000000000000000000, 1.000000000000000000 ) ) ;
#13285 = CARTESIAN_POINT ( 'NONE',  ( 19.48598279363274344, 13.11110640527291693, -2.839279412974138328 ) ) ;
#13286 = CARTESIAN_POINT ( 'NONE',  ( 165.1857505493459826, 286.1010072127883177, -0.2758970588906190513 ) ) ;
#13287 = CARTESIAN_POINT ( 'NONE',  ( 82.74741872462533365, 53.81327073439516084, 15.79824936317409900 ) ) ;
#13288 = CARTESIAN_POINT ( 'NONE',  ( 159.5035715461357597, 258.8388755763825202, 16.93030532244410935 ) ) ;
#13289 = ADVANCED_FACE ( 'NONE', ( #85283 ), #52835, .F. ) ;
#13290 = CARTESIAN_POINT ( 'NONE',  ( 155.6559071247401960, 261.0430556921643870, 17.79853447468815375 ) ) ;
#13291 = VERTEX_POINT ( 'NONE', #46213 ) ;
#13292 = CARTESIAN_POINT ( 'NONE',  ( 181.6354493118350035, 289.5265713693888756, 12.82447052786679542 ) ) ;
#13293 = CARTESIAN_POINT ( 'NONE',  ( 176.0788078253698075, 257.6164099357736177, 12.34344903931495629 ) ) ;
#13294 = EDGE_CURVE ( 'NONE', #70849, #57017, #83785, .T. ) ;
#13295 = CARTESIAN_POINT ( 'NONE',  ( 81.35504097469424778, 42.12982285155051443, 8.020547866998608555 ) ) ;
#13296 = ADVANCED_FACE ( 'NONE', ( #77135 ), #18350, .T. ) ;
#13298 = VERTEX_POINT ( 'NONE', #72050 ) ;
#13297 = B_SPLINE_CURVE_WITH_KNOTS ( 'NONE', 3,
 ( #36944, #22244, #67857, #44533 ),
 .UNSPECIFIED., .F., .F.,
 ( 4, 4 ),
 ( 0.004102704876220263433, 0.008715148612197043745 ),
 .UNSPECIFIED. ) ;
#13299 = CARTESIAN_POINT ( 'NONE',  ( 196.6089555368279775, 289.7213370384957329, -16.36024457473861204 ) ) ;
#13300 = CARTESIAN_POINT ( 'NONE',  ( 148.5203124366314285, 276.0708632542248893, -5.652538179724669654 ) ) ;
#13301 = CARTESIAN_POINT ( 'NONE',  ( 179.0755312288822267, 253.6311214754194907, -0.8622901554475785879 ) ) ;
#13302 = CARTESIAN_POINT ( 'NONE',  ( 155.0304386007204016, 262.1263989543018056, -17.12961552904782181 ) ) ;
#13303 = ORIENTED_EDGE ( 'NONE', *, *, #55887, .F. ) ;
#13304 = VERTEX_POINT ( 'NONE', #10246 ) ;
#13306 = CARTESIAN_POINT ( 'NONE',  ( 164.4761815919938215, 245.7658921781788592, 6.833796894895563412 ) ) ;
#13305 = CYLINDRICAL_SURFACE ( 'NONE', #56734, 70.00000000000002842 ) ;
#13307 = CARTESIAN_POINT ( 'NONE',  ( 192.1859061758433143, 297.7712413352111298, 11.15082371775444336 ) ) ;
#13308 = ORIENTED_EDGE ( 'NONE', *, *, #43064, .T. ) ;
#13309 = CARTESIAN_POINT ( 'NONE',  ( 150.8167050463783312, 269.4247995599803289, 14.38040671671637938 ) ) ;
#13310 = CARTESIAN_POINT ( 'NONE',  ( 80.56202954020665175, 57.53823600680944139, 16.23110421993948549 ) ) ;
#13311 = DIRECTION ( 'NONE',  ( 0.8660254037844378194, 0.5000000000000015543, -0.000000000000000000 ) ) ;
#13312 = EDGE_LOOP ( 'NONE', ( #61220, #65838, #19420, #27984 ) ) ;
#13313 = DIRECTION ( 'NONE',  ( -0.8660254037844387076, -0.4999999999999998890, -0.000000000000000000 ) ) ;
#13314 = ORIENTED_EDGE ( 'NONE', *, *, #16607, .F. ) ;
#13315 = CARTESIAN_POINT ( 'NONE',  ( 164.7762319088960794, 245.2461897844768828, 2.994040459560653122 ) ) ;
#13316 = CARTESIAN_POINT ( 'NONE',  ( 158.1790816997512081, 265.1500479989031192, 17.24717362645544583 ) ) ;
#13317 = ORIENTED_EDGE ( 'NONE', *, *, #11861, .T. ) ;
#13318 = CARTESIAN_POINT ( 'NONE',  ( 174.4214100286941687, 277.0989115522935435, -15.68430753576282477 ) ) ;
#13319 = CARTESIAN_POINT ( 'NONE',  ( 172.3722536416338755, 263.7283137945269686, -15.47002134700890608 ) ) ;
#13320 = ORIENTED_EDGE ( 'NONE', *, *, #43309, .T. ) ;
#13321 = DIRECTION ( 'NONE',  ( -0.4897629171537489778, 0.8718556560469457040, 0.000000000000000000 ) ) ;
#13322 = CARTESIAN_POINT ( 'NONE',  ( 193.0761489135300906, 296.2292956824684893, -11.99675185248219655 ) ) ;
#13323 = VERTEX_POINT ( 'NONE', #39113 ) ;
#13324 = ORIENTED_EDGE ( 'NONE', *, *, #73317, .F. ) ;
#13325 = CARTESIAN_POINT ( 'NONE',  ( 82.71332607344807286, 50.53308841156612630, -14.58498437345447662 ) ) ;
#13326 = CARTESIAN_POINT ( 'NONE',  ( 147.0670278774466908, 275.9194309285509235, 3.666898409139099257 ) ) ;
#13327 = CARTESIAN_POINT ( 'NONE',  ( 188.8233448568038000, 298.7241042047116935, -4.267409509285561953 ) ) ;
#13328 = CARTESIAN_POINT ( 'NONE',  ( 148.9266665119372703, 272.6984423298952152, 12.06339424062075061 ) ) ;
#13329 = DIRECTION ( 'NONE',  ( 0.4999999999999998890, -0.8660254037844385966, 0.000000000000000000 ) ) ;
#13330 = CARTESIAN_POINT ( 'NONE',  ( 146.5103748552642458, 276.8835822451575268, -0.1083234189483069515 ) ) ;
#13331 = CARTESIAN_POINT ( 'NONE',  ( 147.2784190576484491, 275.5532906641692534, 0.2793038414862047958 ) ) ;
#13332 = ORIENTED_EDGE ( 'NONE', *, *, #12930, .F. ) ;
#13333 = CARTESIAN_POINT ( 'NONE',  ( 81.20168625321292666, 55.28033247127913796, -15.96862711004452784 ) ) ;
#13334 = CARTESIAN_POINT ( 'NONE',  ( 165.0020474182383339, 244.8550658491588479, 1.825383354618924425 ) ) ;
#13335 = AXIS2_PLACEMENT_3D ( 'NONE', #20269, #51143, #73473 ) ;
#13336 = CARTESIAN_POINT ( 'NONE',  ( 9.561825351099750847, 42.17961057553871029, 59.99999999999999289 ) ) ;
#13337 = CARTESIAN_POINT ( 'NONE',  ( 67.27771118422515428, 66.58732564224565920, 8.551707608175874498 ) ) ;
#13338 = CARTESIAN_POINT ( 'NONE',  ( 171.3900039105615747, 288.6384802392489064, 4.197201579658607962 ) ) ;
#13339 = CARTESIAN_POINT ( 'NONE',  ( 85.51384538016034753, 42.26407845341874747, 2.123067372083550897 ) ) ;
#13340 = ORIENTED_EDGE ( 'NONE', *, *, #36398, .T. ) ;
#13341 = FACE_OUTER_BOUND ( 'NONE', #20079, .T. ) ;
#13342 = CARTESIAN_POINT ( 'NONE',  ( 71.05835085023741726, 67.33870905001845131, 10.36604878428025955 ) ) ;
#13343 = CARTESIAN_POINT ( 'NONE',  ( 144.9899443387551798, 254.5170451491295296, 0.000000000000000000 ) ) ;
#13344 = CARTESIAN_POINT ( 'NONE',  ( 79.36339018020615299, 45.77489031751736093, 12.95595637456517046 ) ) ;
#13345 = CARTESIAN_POINT ( 'NONE',  ( 47.86207023800641025, 186.8932355074536247, -2.679491924311248496 ) ) ;
#13346 = LINE ( 'NONE', #45701, #43373 ) ;
#13347 = ORIENTED_EDGE ( 'NONE', *, *, #50076, .T. ) ;
#13348 = CARTESIAN_POINT ( 'NONE',  ( 170.5469799148650623, 255.6610463425538740, -11.75595153296455386 ) ) ;
#13349 = CARTESIAN_POINT ( 'NONE',  ( 205.4925884257800988, 274.0740247280971857, 10.80283695292349222 ) ) ;
#13350 = CARTESIAN_POINT ( 'NONE',  ( 164.9779129355220562, 244.8968679994381148, -1.771286574179712803 ) ) ;
#13351 = CARTESIAN_POINT ( 'NONE',  ( 33.27389197678166965, 200.0177522451419350, 5.000000000000046185 ) ) ;
#13352 = CARTESIAN_POINT ( 'NONE',  ( 118.1982478153434357, 248.2369531367911293, -4.594050593750048428 ) ) ;
#13353 = EDGE_CURVE ( 'NONE', #7177, #41184, #82335, .T. ) ;
#13354 = CARTESIAN_POINT ( 'NONE',  ( 151.1230807375396807, 268.8941412966845519, -14.26613110909109849 ) ) ;
#13355 = VECTOR ( 'NONE', #1239, 1000.000000000000114 ) ;
#13356 = CARTESIAN_POINT ( 'NONE',  ( 164.8364259028313938, 281.3006012430400915, -11.81268714249731744 ) ) ;
#13357 = CARTESIAN_POINT ( 'NONE',  ( 84.54558420127669649, 50.65463084595457843, 13.70779263677913562 ) ) ;
#13358 = CARTESIAN_POINT ( 'NONE',  ( 175.4442551608554197, 253.5494353995385097, -3.969463160058352980 ) ) ;
#13359 = CARTESIAN_POINT ( 'NONE',  ( 40.17520546284541894, 187.8768266524160140, 9.188101187500098632 ) ) ;
#13360 = CARTESIAN_POINT ( 'NONE',  ( 160.4237162281696953, 273.2376347127639633, -15.66572034412998882 ) ) ;
#13361 = EDGE_LOOP ( 'NONE', ( #88641, #12699, #30043, #83456 ) ) ;
#13362 = CARTESIAN_POINT ( 'NONE',  ( -1.271452699050922508, 181.6199935810941497, 2.679491924311264039 ) ) ;
#13363 = CARTESIAN_POINT ( 'NONE',  ( 181.8730065081939529, 266.9336132126444454, 16.02317259067967115 ) ) ;
#13364 = ADVANCED_FACE ( 'NONE', ( #24441 ), #16832, .F. ) ;
#13365 = CARTESIAN_POINT ( 'NONE',  ( 70.60363933684126891, 71.39732000281048840, -0.9291670929876240104 ) ) ;
#13366 = EDGE_CURVE ( 'NONE', #4112, #36600, #41175, .T. ) ;
#13367 = CARTESIAN_POINT ( 'NONE',  ( 76.12823843484866870, 51.15411698274154162, 16.08981265264790750 ) ) ;
#13368 = CARTESIAN_POINT ( 'NONE',  ( 81.73250340314956475, 41.47603874751758468, -5.132177573234927515 ) ) ;
#13369 = FACE_OUTER_BOUND ( 'NONE', #58363, .T. ) ;
#13370 = DIRECTION ( 'NONE',  ( 1.000000000000000000, 0.000000000000000000, 0.000000000000000000 ) ) ;
#13371 = CARTESIAN_POINT ( 'NONE',  ( -73.83803415018344651, 50.74234351129840093, -10.00000000000000000 ) ) ;
#13372 = CARTESIAN_POINT ( 'NONE',  ( 96.42157766939708097, 213.1427522451417644, 1.119607411625061291E-15 ) ) ;
#13373 = ORIENTED_EDGE ( 'NONE', *, *, #55327, .T. ) ;
#13374 = CARTESIAN_POINT ( 'NONE',  ( 194.8081329026015283, 266.2519905409982357, -7.562986739740034992 ) ) ;
#13375 = CARTESIAN_POINT ( 'NONE',  ( 162.7561251957091031, 248.7451172484279027, 11.07313294959361194 ) ) ;
#13376 = CARTESIAN_POINT ( 'NONE',  ( 153.9103552012488478, 264.4948476654334968, 16.51460358841814013 ) ) ;
#13377 = CARTESIAN_POINT ( 'NONE',  ( 10.86574497745707646, 167.8923013555410080, 4.594050593750050204 ) ) ;
#13378 = CARTESIAN_POINT ( 'NONE',  ( 4.856824484202590497, 25.73705186507751819, -3.090169943749475845 ) ) ;
#13379 = CARTESIAN_POINT ( 'NONE',  ( 195.8285188278500470, 273.2427770020486832, 15.26130794574777383 ) ) ;
#13380 = CARTESIAN_POINT ( 'NONE',  ( 146.9129474150286683, 276.1863061179126930, -5.016087650759920358 ) ) ;
#13381 = CARTESIAN_POINT ( 'NONE',  ( 73.63650596374165502, 69.59800771093053129, 10.20034856658873323 ) ) ;
#13382 = CARTESIAN_POINT ( 'NONE',  ( 51.92050145378936321, 200.7833772461660828, -9.188101187500095079 ) ) ;
#13383 = CARTESIAN_POINT ( 'NONE',  ( 208.3135187673106543, 269.8373969220020285, 2.829653198597726682 ) ) ;
#13384 = CARTESIAN_POINT ( 'NONE',  ( 203.9008254367631423, 275.8039027522635251, 13.14957672819812906 ) ) ;
#13385 = CARTESIAN_POINT ( 'NONE',  ( 69.32567463353416315, 68.52802923855151107, 7.491982181575302491 ) ) ;
#13386 = CARTESIAN_POINT ( 'NONE',  ( 66.31646558143364700, 68.08799829551760752, -4.617347279476426536 ) ) ;
#13387 = ORIENTED_EDGE ( 'NONE', *, *, #88072, .F. ) ;
#13388 = ADVANCED_FACE ( 'NONE', ( #19367 ), #17000, .F. ) ;
#13389 = CARTESIAN_POINT ( 'NONE',  ( 79.76359975193354046, 44.98417069036879923, 11.54310746654911846 ) ) ;
#13390 = CARTESIAN_POINT ( 'NONE',  ( 23.47697960001819695, 174.3615022471901739, 5.000000000000051514 ) ) ;
#13391 = B_SPLINE_CURVE_WITH_KNOTS ( 'NONE', 3,
 ( #12542, #34332, #96671, #35824, #65715, #11050, #89104, #27736, #3453, #3931, #81966, #50032, #19654, #50516, #18646, #89581, #27239, #57616, #80985, #43415, #74361, #58605, #58123, #72863, #26732, #4425, #57114, #19158, #11551, #65228, #66719, #4945, #33859, #95693, #42410, #64743, #81468, #12042, #96171, #41927 ),
 .UNSPECIFIED., .F., .F.,
 ( 4, 2, 2, 2, 2, 2, 2, 2, 2, 2, 2, 2, 2, 2, 2, 2, 2, 2, 2, 4 ),
 ( 0.003288512847727886965, 0.003481580978879881844, 0.003578115044455918315, 0.003674649110031955219, 0.003771183175607992124, 0.003867717241184029028, 0.004060785372336020438, 0.004446921634640086524, 0.004833057896944153477, 0.005605330421552257025, 0.006377602946160361441, 0.007922147995376568538, 0.008018682060952613683, 0.008115216126528658827, 0.008163483159316682267, 0.008211750192104705706, 0.008308284257680728299, 0.008694420519984849896, 0.009080556782288969758, 0.009466693044593091355 ),
 .UNSPECIFIED. ) ;
#13392 = CARTESIAN_POINT ( 'NONE',  ( 83.84382548910321020, 44.36689950846875519, 9.171174898895673167 ) ) ;
#13393 = CARTESIAN_POINT ( 'NONE',  ( 141.2833242589136375, 258.5024278399160380, 9.188101187500095079 ) ) ;
#13394 = CARTESIAN_POINT ( 'NONE',  ( 28.84566271970979301, 17.44966523072494979, -2.296566073217252530E-15 ) ) ;
#13395 = CARTESIAN_POINT ( 'NONE',  ( 207.5810977459049127, 271.1059873436086036, -7.529053122148023469 ) ) ;
#13396 = CARTESIAN_POINT ( 'NONE',  ( 83.78311978599397492, 51.75050911116664309, -14.85521894841905599 ) ) ;
#13397 = DIRECTION ( 'NONE',  ( -0.000000000000000000, -0.000000000000000000, 1.000000000000000000 ) ) ;
#13399 = CARTESIAN_POINT ( 'NONE',  ( 189.2359190933219679, 289.8534420722585310, 14.44421633591829845 ) ) ;
#13398 = CARTESIAN_POINT ( 'NONE',  ( 157.7861133721078772, 257.3534302411229646, 18.03837896619386783 ) ) ;
#13400 = EDGE_CURVE ( 'NONE', #24879, #34490, #5620, .T. ) ;
#13401 = FACE_OUTER_BOUND ( 'NONE', #35716, .T. ) ;
#13402 = ORIENTED_EDGE ( 'NONE', *, *, #64126, .F. ) ;
#13403 = CARTESIAN_POINT ( 'NONE',  ( 190.7851866479434761, 300.1973587246873194, 7.931162401707728016 ) ) ;
#13404 = CARTESIAN_POINT ( 'NONE',  ( 163.5920121195164256, 247.2973186270110091, 8.917636558496976562 ) ) ;
#13405 = CARTESIAN_POINT ( 'NONE',  ( 175.5746833524315775, 278.5347786252573314, 16.94864957847115505 ) ) ;
#13406 = CARTESIAN_POINT ( 'NONE',  ( 172.8373704755632332, 268.6438884681230661, -16.58280638298598575 ) ) ;
#13407 = CARTESIAN_POINT ( 'NONE',  ( 193.8727374453239349, 270.7503200800575769, -13.89828984444790017 ) ) ;
#13408 = ORIENTED_EDGE ( 'NONE', *, *, #1703, .F. ) ;
#13409 = CARTESIAN_POINT ( 'NONE',  ( 70.25375250786443360, 69.20215222833037672, 7.266984090244938521 ) ) ;
#13410 = VECTOR ( 'NONE', #42774, 1000.000000000000000 ) ;
#13411 = CARTESIAN_POINT ( 'NONE',  ( -69.61464189717713680, 45.83092310410447112, 10.00000000000000000 ) ) ;
#13412 = EDGE_CURVE ( 'NONE', #79361, #42173, #44599, .T. ) ;
#13413 = B_SPLINE_SURFACE_WITH_KNOTS ( 'NONE', 3, 1, ( 
 ( #1565, #86703 ),
 ( #23332, #54220 ),
 ( #47633, #30446 ),
 ( #40024, #85186 ),
 ( #69442, #9150 ),
 ( #32450, #92294 ),
 ( #62835, #78565 ),
 ( #53728, #62325 ),
 ( #84687, #15733 ),
 ( #46638, #23834 ),
 ( #77563, #93791 ),
 ( #94284, #39519 ),
 ( #1053, #77038 ),
 ( #15228, #8152 ),
 ( #46122, #93279 ),
 ( #39026, #7644 ),
 ( #24352, #69932 ),
 ( #551, #54728 ),
 ( #85709, #16245 ),
 ( #47136, #38535 ),
 ( #60, #96792 ),
 ( #26356, #18758 ),
 ( #71962, #58233 ),
 ( #80091, #56234 ),
 ( #57232, #11663 ),
 ( #49637, #42039 ),
 ( #95803, #40531 ),
 ( #50630, #26852 ),
 ( #42525, #11172 ),
 ( #87227, #49156 ),
 ( #88707, #64346 ),
 ( #65827, #41534 ),
 ( #79594, #32939 ),
 ( #19277, #27352 ) ),
 .UNSPECIFIED., .T., .F., .F.,
 ( 4, 2, 2, 2, 2, 2, 2, 2, 2, 2, 2, 2, 2, 2, 2, 2, 4 ),
 ( 2, 2 ),
 ( 0.000000000000000000, 0.06250000000000000000, 0.1250000000000000000, 0.1875000000000000000, 0.2500000000000000000, 0.3125000000000000000, 0.3750000000000000000, 0.4375000000000000000, 0.5000000000000000000, 0.5625000000000000000, 0.6250000000000000000, 0.6875000000000000000, 0.7500000000000000000, 0.8125000000000000000, 0.8750000000000000000, 0.9375000000000000000, 1.000000000000000000 ),
 ( 0.000000000000000000, 1.000000000000000000 ),
 .UNSPECIFIED. ) ;
#13414 = CARTESIAN_POINT ( 'NONE',  ( 200.8510819094290696, 281.8070453751917057, -16.75700185107683282 ) ) ;
#13415 = CARTESIAN_POINT ( 'NONE',  ( 196.1722677117792557, 270.9862039110303158, 12.91586066753414919 ) ) ;
#13416 = CARTESIAN_POINT ( 'NONE',  ( 185.7938733065929853, 296.8758775647544894, 5.418709528595011982 ) ) ;
#13417 = CARTESIAN_POINT ( 'NONE',  ( 137.8880043751089772, 261.9637435831424455, 2.679491924311251605 ) ) ;
#13418 = CARTESIAN_POINT ( 'NONE',  ( 175.1271263694729328, 272.4273639404348728, 17.81557788710851042 ) ) ;
#13419 = DIRECTION ( 'NONE',  ( -0.6123724356957817028, -0.3535533905932665699, -0.7071067811865623387 ) ) ;
#13420 = ORIENTED_EDGE ( 'NONE', *, *, #98027, .T. ) ;
#13421 = CARTESIAN_POINT ( 'NONE',  ( 11.06379537489605625, 28.16126292948893806, -6.180339887498951690 ) ) ;
#13422 = DIRECTION ( 'NONE',  ( 1.000000000000000000, 0.000000000000000000, 0.000000000000000000 ) ) ;
#13423 = VERTEX_POINT ( 'NONE', #90777 ) ;
#13424 = DIRECTION ( 'NONE',  ( 0.000000000000000000, 1.000000000000000000, 1.097929109219269329E-14 ) ) ;
#13425 = CARTESIAN_POINT ( 'NONE',  ( 86.44808582675112518, 47.03435218195901513, -10.53111747673477794 ) ) ;
#13426 = CARTESIAN_POINT ( 'NONE',  ( 159.6494826941923861, 264.1119501240779073, -17.72553829314773566 ) ) ;
#13427 = B_SPLINE_CURVE_WITH_KNOTS ( 'NONE', 3,
 ( #4751, #66040, #60404, #74663 ),
 .UNSPECIFIED., .F., .F.,
 ( 4, 4 ),
 ( 0.01047501919852616287, 0.01579130575507147610 ),
 .UNSPECIFIED. ) ;
#13428 = ORIENTED_EDGE ( 'NONE', *, *, #87455, .F. ) ;
#13429 = CARTESIAN_POINT ( 'NONE',  ( 147.1447476476323004, 275.7848163378367872, 0.6373001129109078233 ) ) ;
#13430 = CARTESIAN_POINT ( 'NONE',  ( 185.6176320207485446, 291.1239150995572231, 12.16464820431206206 ) ) ;
#13431 = B_SPLINE_CURVE_WITH_KNOTS ( 'NONE', 3,
 ( #24669, #47467, #93098, #55552, #22686, #53565, #30783, #45952, #872, #16072, #86536, #17066, #46974, #78900, #8479, #61664 ),
 .UNSPECIFIED., .F., .F.,
 ( 4, 2, 2, 2, 2, 2, 2, 4 ),
 ( -9.576356418732827919E-06, 3.142278651979172423E-05, 7.242192945831627806E-05, 0.0001544202153353389177, 0.0003184167870893806732, 0.0006464099305974667321, 0.0009744030741055529537, 0.001302396217613638850 ),
 .UNSPECIFIED. ) ;
#13432 = CARTESIAN_POINT ( 'NONE',  ( 204.2556901454867955, 276.8657622634082713, 13.61111001399713949 ) ) ;
#13433 = CARTESIAN_POINT ( 'NONE',  ( 159.3655983545995127, 283.2591999228209829, -2.078818975303923899 ) ) ;
#13434 = CARTESIAN_POINT ( 'NONE',  ( 49.32136238152735785, 210.8297689869269220, -2.679491924311252493 ) ) ;
#13435 = EDGE_LOOP ( 'NONE', ( #10822, #45067, #32364, #36708 ) ) ;
#13436 = CARTESIAN_POINT ( 'NONE',  ( 92.46148921633090367, 218.0643266524160140, 9.188101187500095079 ) ) ;
#13437 = CARTESIAN_POINT ( 'NONE',  ( 155.2317605920271717, 261.7776990366773475, 17.06683146360218828 ) ) ;
#13438 = DIRECTION ( 'NONE',  ( 0.2347357813929421555, -0.4065742997269585213, 0.8829475928589297640 ) ) ;
#13439 = CARTESIAN_POINT ( 'NONE',  ( 81.35748880148535989, 42.22347387491733883, -7.155507324468844743 ) ) ;
#13440 = B_SPLINE_SURFACE_WITH_KNOTS ( 'NONE', 3, 1, ( 
 ( #41513, #88687 ),
 ( #50124, #10134 ),
 ( #64835, #3061 ),
 ( #57211, #17216 ),
 ( #9652, #48122 ),
 ( #2546, #33429 ),
 ( #64326, #27821 ),
 ( #74449, #13626 ),
 ( #37398, #44498 ),
 ( #5519, #58697 ),
 ( #67308, #52106 ),
 ( #5029, #89672 ),
 ( #28307, #14119 ),
 ( #83554, #6522 ),
 ( #73930, #90670 ),
 ( #36402, #20232 ),
 ( #44999, #21227 ),
 ( #35416, #98742 ),
 ( #75945, #83053 ),
 ( #4516, #66323 ),
 ( #12130, #21714 ),
 ( #43510, #98235 ),
 ( #74936, #75429 ),
 ( #97740, #82574 ),
 ( #67819, #68303 ),
 ( #27333, #28820 ),
 ( #59704, #58215 ),
 ( #89193, #60188 ),
 ( #13137, #36906 ),
 ( #12638, #91149 ),
 ( #6013, #51620 ) ),
 .UNSPECIFIED., .F., .F., .F.,
 ( 4, 3, 3, 3, 3, 3, 3, 3, 3, 3, 4 ),
 ( 2, 2 ),
 ( 0.000000000000000000, 0.1333490885032380391, 0.3007194338854225490, 0.4699862290244999907, 0.5844252810809225096, 0.6686540514502540278, 0.7354980260655328284, 0.8028463152565535887, 0.8633854507757017238, 0.9437142632667037123, 1.000000000000000000 ),
 ( 0.000000000000000000, 1.000000000000000000 ),
 .UNSPECIFIED. ) ;
#13441 = ORIENTED_EDGE ( 'NONE', *, *, #57812, .T. ) ;
#13442 = ORIENTED_EDGE ( 'NONE', *, *, #24101, .T. ) ;
#13443 = CARTESIAN_POINT ( 'NONE',  ( 207.3790894204113613, 271.0808592135389858, 2.321707834868911302 ) ) ;
#13444 = ORIENTED_EDGE ( 'NONE', *, *, #54776, .T. ) ;
#13445 = LINE ( 'NONE', #83358, #48212 ) ;
#13446 = VERTEX_POINT ( 'NONE', #75534 ) ;
#13447 = DIRECTION ( 'NONE',  ( 0.000000000000000000, 0.000000000000000000, 1.000000000000000000 ) ) ;
#13448 = DIRECTION ( 'NONE',  ( 1.000000000000000000, 0.000000000000000000, 0.000000000000000000 ) ) ;
#13449 = VERTEX_POINT ( 'NONE', #29919 ) ;
#13450 = CARTESIAN_POINT ( 'NONE',  ( 165.5428789467008244, 248.7867348279617659, -9.239987926238155680 ) ) ;
#13452 = EDGE_CURVE ( 'NONE', #85116, #3917, #83664, .T. ) ;
#13451 = CARTESIAN_POINT ( 'NONE',  ( 174.4380169027350291, 291.1401200322444538, -5.384106100014290242 ) ) ;
#13453 = CARTESIAN_POINT ( 'NONE',  ( 10.46624461501205872, 188.3967562850346837, -4.648177544792955347E-16 ) ) ;
#13454 = CARTESIAN_POINT ( 'NONE',  ( 73.67429767784587114, 67.97956927692818851, -11.30367013265376563 ) ) ;
#13455 = CARTESIAN_POINT ( 'NONE',  ( 164.7447033178649747, 265.0565378767570905, -16.62346194256757315 ) ) ;
#13456 = ORIENTED_EDGE ( 'NONE', *, *, #48506, .F. ) ;
#13457 = CARTESIAN_POINT ( 'NONE',  ( 81.30818518503046732, 58.89441083166271085, 0.000000000000000000 ) ) ;
#13458 = CARTESIAN_POINT ( 'NONE',  ( 6.244247187202517146, 25.64646525600388216, -2.839279412974133887 ) ) ;
#13459 = VERTEX_POINT ( 'NONE', #45114 ) ;
#13460 = LINE ( 'NONE', #5840, #5768 ) ;
#13462 = VERTEX_POINT ( 'NONE', #92749 ) ;
#13461 = CARTESIAN_POINT ( 'NONE',  ( 200.0161915203198362, 270.0763376282534409, 10.26060645788218295 ) ) ;
#13463 = DIRECTION ( 'NONE',  ( -0.8660254037844387076, -0.4999999999999998890, -0.000000000000000000 ) ) ;
#13464 = CARTESIAN_POINT ( 'NONE',  ( 187.3586742363142150, 260.2951279848165882, 2.860953161626957009 ) ) ;
#13465 = CARTESIAN_POINT ( 'NONE',  ( 150.9020882617336383, 276.5917379820504038, -5.284388463461365149 ) ) ;
#13466 = CARTESIAN_POINT ( 'NONE',  ( -12.34951437337453228, 41.85136669140065635, 59.99999999999999289 ) ) ;
#13467 = DIRECTION ( 'NONE',  ( -0.8660254037844387076, -0.4999999999999998890, -0.000000000000000000 ) ) ;
#13468 = CARTESIAN_POINT ( 'NONE',  ( 147.1270795744234476, 264.4111747905818675, -1.822351119449947324E-15 ) ) ;
#13469 = CARTESIAN_POINT ( 'NONE',  ( 195.1831177385782894, 292.1517303617533230, 15.29763345156017174 ) ) ;
#13470 = VERTEX_POINT ( 'NONE', #36514 ) ;
#13471 = LINE ( 'NONE', #91994, #33247 ) ;
#13472 = EDGE_LOOP ( 'NONE', ( #31596, #41401, #1945, #40723 ) ) ;
#13473 = CARTESIAN_POINT ( 'NONE',  ( 160.3055490814878681, 276.2749098051363603, 12.65412181104003508 ) ) ;
#13474 = EDGE_CURVE ( 'NONE', #18285, #94538, #77008, .T. ) ;
#13475 = CARTESIAN_POINT ( 'NONE',  ( 171.3124858205567023, 279.6758709237702760, -14.80999945890478742 ) ) ;
#13476 = CARTESIAN_POINT ( 'NONE',  ( 203.9713276076765283, 277.3582926266647632, -14.32166128205299138 ) ) ;
#13477 = CARTESIAN_POINT ( 'NONE',  ( 86.05489758235616193, 44.63495567976185185, -6.775695627399047183 ) ) ;
#13478 = CARTESIAN_POINT ( 'NONE',  ( 164.5892160260162882, 274.3781231134265681, 14.76927392745111334 ) ) ;
#13480 = CARTESIAN_POINT ( 'NONE',  ( 75.96128792555467157, 65.56719406519354720, 13.89537262461679212 ) ) ;
#13479 = CARTESIAN_POINT ( 'NONE',  ( -5.561934722402757991, 167.5958772461660544, -9.188101187500095079 ) ) ;
#13481 = CARTESIAN_POINT ( 'NONE',  ( 28.09809348231459936, 175.4824982072973967, 3.021315404115420679E-15 ) ) ;
#13482 = ORIENTED_EDGE ( 'NONE', *, *, #65196, .F. ) ;
#13483 = EDGE_LOOP ( 'NONE', ( #22501, #42882, #25014, #81312 ) ) ;
#13484 = CARTESIAN_POINT ( 'NONE',  ( 156.6812872898450735, 261.2670451491295012, 0.000000000000000000 ) ) ;
#13485 = CARTESIAN_POINT ( 'NONE',  ( -61.58631828649576079, 53.07550491216805710, 59.99999999999999289 ) ) ;
#13486 = AXIS2_PLACEMENT_3D ( 'NONE', #59322, #5647, #13272 ) ;
#13487 = EDGE_CURVE ( 'NONE', #861, #17015, #53214, .T. ) ;
#13488 = CARTESIAN_POINT ( 'NONE',  ( 69.10717603675902865, 66.30743475805610387, -10.20864196604519769 ) ) ;
#13489 = CARTESIAN_POINT ( 'NONE',  ( 174.0250796533206312, 290.1103312770194407, 2.568368125944323843 ) ) ;
#13490 = CARTESIAN_POINT ( 'NONE',  ( 85.78101276405163844, 42.88643024831080908, 1.820988380798113537 ) ) ;
#13491 = EDGE_CURVE ( 'NONE', #11268, #60486, #53219, .T. ) ;
#13492 = CARTESIAN_POINT ( 'NONE',  ( 83.66738886159650690, 44.95173633656256129, 9.291185867263966003 ) ) ;
#13493 = CARTESIAN_POINT ( 'NONE',  ( 171.1295603993285965, 249.6517061031812545, 4.344809613321301889 ) ) ;
#13494 = CARTESIAN_POINT ( 'NONE',  ( 10.51348828746337816, 183.0024278399160949, -9.188101187500093303 ) ) ;
#13495 = VECTOR ( 'NONE', #36911, 1000.000000000000114 ) ;
#13496 = CARTESIAN_POINT ( 'NONE',  ( 114.9778026189612632, 243.3149278399160664, 9.188101187500093303 ) ) ;
#13497 = DIRECTION ( 'NONE',  ( -0.000000000000000000, -0.000000000000000000, -1.000000000000000000 ) ) ;
#13498 = DIRECTION ( 'NONE',  ( -0.8756465943326132706, -0.4829524219151362097, 0.000000000000000000 ) ) ;
#13499 = CARTESIAN_POINT ( 'NONE',  ( 78.01941338035848617, 51.47862715311421056, 15.42328866796606235 ) ) ;
#13500 = AXIS2_PLACEMENT_3D ( 'NONE', #40536, #22486, #53378 ) ;
#13501 = CARTESIAN_POINT ( 'NONE',  ( 181.1156277128715431, 292.7914473640799997, 9.490545386343454126 ) ) ;
#13502 = CARTESIAN_POINT ( 'NONE',  ( 190.0977106519948450, 299.8480667433163944, -5.515936301684110532 ) ) ;
#13503 = CARTESIAN_POINT ( 'NONE',  ( 154.8596847415876994, 262.4221533139083817, 17.65401077761399762 ) ) ;
#13504 = LINE ( 'NONE', #98613, #93405 ) ;
#13505 = CARTESIAN_POINT ( 'NONE',  ( 147.6095889327917803, 274.9796876144846465, -8.460961150142429332 ) ) ;
#13506 = CARTESIAN_POINT ( 'NONE',  ( 84.68103419341217375, 50.25510846593720515, 13.84703097836258934 ) ) ;
#13507 = CARTESIAN_POINT ( 'NONE',  ( 187.7344944884639801, 299.0281582812487500, -0.5885417617450732219 ) ) ;
#13508 = CARTESIAN_POINT ( 'NONE',  ( 78.46959274032997200, 226.1115022471903160, -5.000000000000047962 ) ) ;
#13509 = CARTESIAN_POINT ( 'NONE',  ( 183.8229730883442130, 268.4974150671761777, -15.08127568743503311 ) ) ;
#13510 = CARTESIAN_POINT ( 'NONE',  ( -25.89332989531674301, 24.59406508915897760, 10.00000000000000000 ) ) ;
#13511 =( BOUNDED_CURVE ( )  B_SPLINE_CURVE ( 2, ( #54950, #8856, #17457, #39724, #70654, #1777, #32150, #25566, #55431, #32656, #63556, #72180, #1266 ),
 .UNSPECIFIED., .F., .T. ) 
 B_SPLINE_CURVE_WITH_KNOTS ( ( 3, 2, 2, 2, 2, 2, 3 ),
 ( 0.6125000000000000444, 0.6149999999999999911, 0.6199999999999999956, 0.6250000000000000000, 0.6300000000000000044, 0.6350000000000000089, 0.6375000000000000666 ),
 .UNSPECIFIED. ) 
 CURVE ( )  GEOMETRIC_REPRESENTATION_ITEM ( )  RATIONAL_B_SPLINE_CURVE ( ( 0.9755282581475767101, 0.9755282581475772652, 1.000000000000000000, 0.9510565162951535312, 1.000000000000000000, 0.9510565162951535312, 1.000000000000000000, 0.9510565162951535312, 1.000000000000000000, 0.9510565162951535312, 1.000000000000000000, 0.9755282581475761550, 0.9755282581475767101 ) ) 
 REPRESENTATION_ITEM ( '' )  );
#13512 = ADVANCED_FACE ( 'NONE', ( #98846 ), #93682, .T. ) ;
#13513 = CARTESIAN_POINT ( 'NONE',  ( -61.60412911085354182, 37.02832515102500111, 177.5919119679930134 ) ) ;
#13514 = CARTESIAN_POINT ( 'NONE',  ( 93.48972083544241229, 224.7833772461660260, -9.188101187500095079 ) ) ;
#13515 = CARTESIAN_POINT ( 'NONE',  ( 5.120201826081539842, 21.14336893147752861, 7.433330006724141015 ) ) ;
#13516 = CARTESIAN_POINT ( 'NONE',  ( 172.9380501958987111, 251.0613099074927561, -5.462789090222858412 ) ) ;
#13518 = CARTESIAN_POINT ( 'NONE',  ( 200.4229826824105203, 283.5042063200048119, 17.40835197696380376 ) ) ;
#13517 = CARTESIAN_POINT ( 'NONE',  ( 196.4390255720217908, 290.4046224503736653, 16.34739044515864848 ) ) ;
#13519 = CARTESIAN_POINT ( 'NONE',  ( 149.1848515893298952, 272.2512526580950407, 13.00839212001256229 ) ) ;
#13520 = CARTESIAN_POINT ( 'NONE',  ( 151.1699610800269511, 268.8129421616204695, -14.28929860221299286 ) ) ;
#13521 = CARTESIAN_POINT ( 'NONE',  ( -80.08603253397792798, 57.73992072201551906, 10.00000000000000000 ) ) ;
#13522 = CARTESIAN_POINT ( 'NONE',  ( 37.43858582280105907, 33.56628583063844218, 9.188101187500006262 ) ) ;
#13523 = CARTESIAN_POINT ( 'NONE',  ( 192.9633865298379476, 296.4246058602058156, -11.85717392250713864 ) ) ;
#13524 = FACE_BOUND ( 'NONE', #85588, .T. ) ;
#13525 = EDGE_LOOP ( 'NONE', ( #61489, #59531, #55894, #17653 ) ) ;
#13526 = CARTESIAN_POINT ( 'NONE',  ( 24.12224894148702248, 22.43085787977763701, -9.188101187500008038 ) ) ;
#13527 = CARTESIAN_POINT ( 'NONE',  ( 36.34934470066777834, 21.39040679176985194, 1.333680081654574804E-15 ) ) ;
#13528 = CARTESIAN_POINT ( 'NONE',  ( 197.1972787308770023, 267.5603457548782558, 9.837912184082732381 ) ) ;
#13529 = CARTESIAN_POINT ( 'NONE',  ( 191.6361107213085120, 287.8645130632154974, -15.84396015365595289 ) ) ;
#13530 = VERTEX_POINT ( 'NONE', #21819 ) ;
#13531 = CARTESIAN_POINT ( 'NONE',  ( 70.90699100671335486, 61.04309739204857266, 15.03109142694147948 ) ) ;
#13532 = CARTESIAN_POINT ( 'NONE',  ( 198.6012358295098750, 286.6595644277572887, 18.21911298807435386 ) ) ;
#13533 = CARTESIAN_POINT ( 'NONE',  ( 73.16956295238907160, 57.33411781477383329, 16.38320611710937058 ) ) ;
#13534 = CARTESIAN_POINT ( 'NONE',  ( 170.7170432258869255, 252.9330647848325668, -8.768963007360460082 ) ) ;
#13535 = CARTESIAN_POINT ( 'NONE',  ( 1.023347710557721113, 26.18841396516314646, 10.00000000000000000 ) ) ;
#13536 = CARTESIAN_POINT ( 'NONE',  ( 135.1220879045620507, 255.4865022471903444, 10.00000000000009237 ) ) ;
#13537 = CARTESIAN_POINT ( 'NONE',  ( 157.0887340267001946, 258.5613266995183039, -17.61824281915036394 ) ) ;
#13538 = ORIENTED_EDGE ( 'NONE', *, *, #68927, .F. ) ;
#13539 = CARTESIAN_POINT ( 'NONE',  ( 83.70225478178599587, 46.26040777977714669, -11.35289932219425602 ) ) ;
#13540 = ORIENTED_EDGE ( 'NONE', *, *, #93450, .F. ) ;
#13541 = CARTESIAN_POINT ( 'NONE',  ( 196.8307300463833087, 264.7821886061209966, -4.649540328500814113 ) ) ;
#13542 = DIRECTION ( 'NONE',  ( 0.4999999999999998890, -0.8660254037844385966, 0.000000000000000000 ) ) ;
#13543 = ORIENTED_EDGE ( 'NONE', *, *, #32562, .T. ) ;
#13544 = CARTESIAN_POINT ( 'NONE',  ( 185.2870392614587445, 292.5660204067580139, -10.68714641920701602 ) ) ;
#13545 = EDGE_LOOP ( 'NONE', ( #63281, #18529, #82853, #24110 ) ) ;
#13546 = CYLINDRICAL_SURFACE ( 'NONE', #81433, 17.82106496071139645 ) ;
#13547 = B_SPLINE_CURVE_WITH_KNOTS ( 'NONE', 3,
 ( #55767, #88260, #56283, #3136, #48714, #16794, #79645, #10211, #49692, #24400, #34020, #63895, #86255, #87282, #9203, #48196 ),
 .UNSPECIFIED., .F., .F.,
 ( 4, 1, 2, 2, 2, 1, 2, 2, 4 ),
 ( 0.000000000000000000, 0.1250000000000055234, 0.1875000000000074385, 0.2500000000000093814, 0.5000000000000118794, 0.6250000000000117684, 0.6875000000000107692, 0.7500000000000096589, 1.000000000000000000 ),
 .UNSPECIFIED. ) ;
#13548 = CARTESIAN_POINT ( 'NONE',  ( 158.4014687745750223, 256.2876034193376427, 17.30374031384843292 ) ) ;
#13549 = CARTESIAN_POINT ( 'NONE',  ( 88.17106782721933200, 44.41923492627702075, -4.565543248975949098 ) ) ;
#13550 = CARTESIAN_POINT ( 'NONE',  ( 152.8328714238065515, 265.9326969577624027, -16.29536156676786263 ) ) ;
#13551 = EDGE_CURVE ( 'NONE', #23610, #26627, #7111, .T. ) ;
#13552 = CARTESIAN_POINT ( 'NONE',  ( 37.65389587561886486, 30.24335787977765833, -9.188101187500008038 ) ) ;
#13553 = CARTESIAN_POINT ( 'NONE',  ( 80.12724894187661562, 44.72419067623221167, 11.12292608744810529 ) ) ;
#13554 = CARTESIAN_POINT ( 'NONE',  ( 72.09806618716604021, 60.83808587311448690, -14.86418196441615258 ) ) ;
#13555 = CARTESIAN_POINT ( 'NONE',  ( -19.65312891409030271, 93.06504152958497400, 177.5919119679930134 ) ) ;
#13556 = DIRECTION ( 'NONE',  ( 1.235257323912246174E-15, 1.000000000000000000, -0.000000000000000000 ) ) ;
#13557 = ORIENTED_EDGE ( 'NONE', *, *, #95300, .T. ) ;
#13558 = VECTOR ( 'NONE', #32477, 1000.000000000000114 ) ;
#13559 = ORIENTED_EDGE ( 'NONE', *, *, #96924, .F. ) ;
#13560 = CARTESIAN_POINT ( 'NONE',  ( 87.04122873496829982, 46.31593380912286761, -9.298662157179395038 ) ) ;
#13562 = CARTESIAN_POINT ( 'NONE',  ( 163.8998849419727435, 272.9681336415193869, -15.35406178914973907 ) ) ;
#13561 = CARTESIAN_POINT ( 'NONE',  ( 174.5182925596964196, 257.2711356623013899, -12.07587375265958229 ) ) ;
#13563 = CARTESIAN_POINT ( 'NONE',  ( -22.42236680055709641, 157.8615022471902591, 0.000000000000000000 ) ) ;
#13564 = CARTESIAN_POINT ( 'NONE',  ( 197.8534124529632834, 273.4752411235029967, -13.40023471225654106 ) ) ;
#13565 = VECTOR ( 'NONE', #37179, 1000.000000000000000 ) ;
#13566 = CARTESIAN_POINT ( 'NONE',  ( 74.65094944003260480, 60.90640990763624529, -15.37438762173259121 ) ) ;
#13567 = CARTESIAN_POINT ( 'NONE',  ( 190.5154909595809727, 300.6644853595138329, -0.04129855346138300298 ) ) ;
#13568 = CARTESIAN_POINT ( 'NONE',  ( 167.3389692517741878, 286.2055908521544438, -4.776237697990188380 ) ) ;
#13569 = CARTESIAN_POINT ( 'NONE',  ( 77.08262651433446422, 63.62497865693946153, -15.40261155718560815 ) ) ;
#13570 = AXIS2_PLACEMENT_3D ( 'NONE', #14550, #53030, #65862 ) ;
#13571 = CARTESIAN_POINT ( 'NONE',  ( 78.86410592861936664, 59.57720046317054852, 16.50785913320112996 ) ) ;
#13572 = CARTESIAN_POINT ( 'NONE',  ( 107.8059429699301575, 242.2369531367911009, -4.594050593750048428 ) ) ;
#13573 = DIRECTION ( 'NONE',  ( 0.000000000000000000, 0.000000000000000000, 1.000000000000000000 ) ) ;
#13574 = CARTESIAN_POINT ( 'NONE',  ( 191.6404332549959690, 275.2293478342741651, 16.16297667511041425 ) ) ;
#13575 = EDGE_LOOP ( 'NONE', ( #67097, #45065, #10208, #73381 ) ) ;
#13576 = CARTESIAN_POINT ( 'NONE',  ( 74.22019797964286170, 68.67351823779483766, -11.46693203622143820 ) ) ;
#13577 = FACE_OUTER_BOUND ( 'NONE', #6215, .T. ) ;
#13578 = CARTESIAN_POINT ( 'NONE',  ( 157.8360072705708603, 257.2670114739976839, 17.12122855844125269 ) ) ;
#13579 = CARTESIAN_POINT ( 'NONE',  ( 68.45576418072165836, 69.87261364207513736, 4.691110543634933627 ) ) ;
#13580 = CARTESIAN_POINT ( 'NONE',  ( 74.15525029152222203, 55.50479885125673718, -16.11756190328145166 ) ) ;
#13581 = ORIENTED_EDGE ( 'NONE', *, *, #62001, .F. ) ;
#13582 = VERTEX_POINT ( 'NONE', #60790 ) ;
#13583 = CARTESIAN_POINT ( 'NONE',  ( 201.3911183001464451, 266.9640362439821502, -3.754059931952923534 ) ) ;
#13584 = ORIENTED_EDGE ( 'NONE', *, *, #26286, .F. ) ;
#13585 = CARTESIAN_POINT ( 'NONE',  ( 192.4760896514942203, 263.8193595997221337, -8.316349228157742246 ) ) ;
#13586 = DIRECTION ( 'NONE',  ( 1.000000000000000000, 0.000000000000000000, 0.000000000000000000 ) ) ;
#13587 = FACE_OUTER_BOUND ( 'NONE', #15754, .T. ) ;
#13589 = CARTESIAN_POINT ( 'NONE',  ( 69.89140086045073019, 62.80215112504183850, -13.32307909001956858 ) ) ;
#13588 = CARTESIAN_POINT ( 'NONE',  ( 198.2391837281077756, 286.3575794386269422, 17.25947343406376078 ) ) ;
#13590 = CARTESIAN_POINT ( 'NONE',  ( 202.7282074973916792, 277.5114398175890642, -15.40750263959311184 ) ) ;
#13591 = ORIENTED_EDGE ( 'NONE', *, *, #49408, .F. ) ;
#13592 = DIRECTION ( 'NONE',  ( 0.8660254037844395958, 0.4999999999999985567, 0.000000000000000000 ) ) ;
#13593 = CARTESIAN_POINT ( 'NONE',  ( 179.8432160940321296, 258.5759063625694694, 11.15262217193699001 ) ) ;
#13594 = CARTESIAN_POINT ( 'NONE',  ( 82.34676179634530513, 41.29334736454898547, -3.425696165949260852 ) ) ;
#13595 = CARTESIAN_POINT ( 'NONE',  ( 173.7083855031236510, 250.9142590195035325, -1.051028738215985303 ) ) ;
#13596 = CARTESIAN_POINT ( 'NONE',  ( 122.6368883333364295, 231.6115022471901739, -5.000000000000041744 ) ) ;
#13597 = ADVANCED_FACE ( 'NONE', ( #37505 ), #98514, .F. ) ;
#13598 = CARTESIAN_POINT ( 'NONE',  ( 49.93482446054089507, 85.48106202472366988, -10.00000000000000000 ) ) ;
#13599 = CYLINDRICAL_SURFACE ( 'NONE', #3267, 70.00000000000002842 ) ;
#13600 = EDGE_CURVE ( 'NONE', #87229, #49470, #20020, .T. ) ;
#13601 = CARTESIAN_POINT ( 'NONE',  ( -17.42236680055705023, 149.2012482093457777, 0.000000000000000000 ) ) ;
#13602 = CARTESIAN_POINT ( 'NONE',  ( -44.43135095815892299, 47.65333612089700921, 59.99999999999999289 ) ) ;
#13603 = CARTESIAN_POINT ( 'NONE',  ( 69.81478986972626899, 70.37643060760527192, -3.960572301807858242 ) ) ;
#13604 = EDGE_CURVE ( 'NONE', #63278, #8092, #49977, .T. ) ;
#13605 = CARTESIAN_POINT ( 'NONE',  ( 80.01237403692960015, 210.8768266524159856, -9.188101187500091527 ) ) ;
#13606 = CARTESIAN_POINT ( 'NONE',  ( 159.8946522441011382, 253.7013337850969492, -16.68230890105693121 ) ) ;
#13607 = DIRECTION ( 'NONE',  ( -0.000000000000000000, -0.000000000000000000, -1.000000000000000000 ) ) ;
#13608 = CARTESIAN_POINT ( 'NONE',  ( 162.6425574510925003, 248.9418223522047526, -10.70838742014210077 ) ) ;
#13609 = EDGE_CURVE ( 'NONE', #2782, #29718, #21806, .T. ) ;
#13610 = LINE ( 'NONE', #92150, #40083 ) ;
#13611 = CARTESIAN_POINT ( 'NONE',  ( 207.6129110656513035, 271.0508850574501025, -5.265106572941297358 ) ) ;
#13612 = CARTESIAN_POINT ( 'NONE',  ( 18.86034532297697908, 34.61239144260639478, 10.00000000000000000 ) ) ;
#13614 = CARTESIAN_POINT ( 'NONE',  ( -20.77255224845912451, 95.18466417500319210, 45.19939659820781230 ) ) ;
#13613 = CARTESIAN_POINT ( 'NONE',  ( 73.47309087361824709, 69.99741330878467238, -9.625970422713120200 ) ) ;
#13615 =( LENGTH_UNIT ( ) NAMED_UNIT ( * ) SI_UNIT ( .MILLI., .METRE. ) );
#13616 = DIRECTION ( 'NONE',  ( 0.5000000000000002220, -0.8660254037844387076, -0.000000000000000000 ) ) ;
#13617 = CARTESIAN_POINT ( 'NONE',  ( -66.52313368742112232, 58.99514187658198949, 59.99999999999999289 ) ) ;
#13618 = CARTESIAN_POINT ( 'NONE',  ( 85.49318370521093868, 48.99722645306706426, -12.73116331006621316 ) ) ;
#13619 = CARTESIAN_POINT ( 'NONE',  ( 72.24711563986207352, 72.09099709781209242, 3.122935046306669626 ) ) ;
#13620 = AXIS2_PLACEMENT_3D ( 'NONE', #12016, #49017, #11027 ) ;
#13621 = CARTESIAN_POINT ( 'NONE',  ( 30.10766014385131939, 182.0643266524160424, 9.188101187500095079 ) ) ;
#13622 = DIRECTION ( 'NONE',  ( -0.000000000000000000, 0.000000000000000000, 1.000000000000000000 ) ) ;
#13624 = CARTESIAN_POINT ( 'NONE',  ( 199.7368853651836105, 277.6985558088923653, 15.20939665263245111 ) ) ;
#13623 = VECTOR ( 'NONE', #34224, 1000.000000000000114 ) ;
#13625 = CARTESIAN_POINT ( 'NONE',  ( 194.3442947553755005, 294.0328026529847421, -15.97648891113594871 ) ) ;
#13626 = CARTESIAN_POINT ( 'NONE',  ( 72.13656828596906223, 72.31233833605649863, -1.326438232958793595 ) ) ;
#13627 = CARTESIAN_POINT ( 'NONE',  ( 58.84905177982987823, 192.5327760586659451, 1.948934522072302763E-15 ) ) ;
#13628 = CARTESIAN_POINT ( 'NONE',  ( 14.85459438965255607, 31.68290643055186706, 3.479690158560446702E-15 ) ) ;
#13629 = CARTESIAN_POINT ( 'NONE',  ( 198.9590707264871412, 286.0397762054715827, -17.05306195936250191 ) ) ;
#13630 = CARTESIAN_POINT ( 'NONE',  ( 46.80869107419874098, 110.6443039040113092, 10.00000000000000000 ) ) ;
#13631 = CARTESIAN_POINT ( 'NONE',  ( 35.06352437372437691, 42.01751292744058475, 6.180339887498949913 ) ) ;
#13632 = CARTESIAN_POINT ( 'NONE',  ( 201.1507709783248004, 268.9741687161805999, -6.437191260250949121 ) ) ;
#13633 = CARTESIAN_POINT ( 'NONE',  ( 76.50778254745674190, 62.49071378302044621, 15.67075087195867944 ) ) ;
#13634 = CARTESIAN_POINT ( 'NONE',  ( 179.9883836461400506, 276.4655832705219041, 17.64582730720814752 ) ) ;
#13635 = CARTESIAN_POINT ( 'NONE',  ( 72.66072155841338542, 61.62800837470290816, 14.69956871679224442 ) ) ;
#13636 = CARTESIAN_POINT ( 'NONE',  ( -42.72532191160158987, 28.29708160126036987, -10.00000000000000000 ) ) ;
#13637 = PRODUCT ( 'Screw Retaining Piece Part', 'Screw Retaining Piece Part', '', ( #36050 ) ) ;
#13638 = CARTESIAN_POINT ( 'NONE',  ( 163.4836020540464006, 255.6328358810647785, -14.84222631813321236 ) ) ;
#13639 = CARTESIAN_POINT ( 'NONE',  ( 36.73352089011212485, 76.83585917327397397, 59.99999999999999289 ) ) ;
#13640 = CARTESIAN_POINT ( 'NONE',  ( 86.69683407628214411, 230.8615022471903160, 5.000000000000046185 ) ) ;
#13641 = CARTESIAN_POINT ( 'NONE',  ( 200.1385401540174769, 283.9968752310148830, 17.30012534137638625 ) ) ;
#13642 = CARTESIAN_POINT ( 'NONE',  ( 165.0023938551389051, 269.5197546249395941, -16.29883053466163645 ) ) ;
#13643 = ORIENTED_EDGE ( 'NONE', *, *, #66124, .T. ) ;
#13644 = CARTESIAN_POINT ( 'NONE',  ( 50.64826632015721231, 209.2369531367911293, -4.594050593750048428 ) ) ;
#13645 = ORIENTED_EDGE ( 'NONE', *, *, #82293, .F. ) ;
#13646 = LINE ( 'NONE', #99748, #38390 ) ;
#13647 = CARTESIAN_POINT ( 'NONE',  ( 147.4368675721658519, 275.2788497866417288, 5.050119523016719292 ) ) ;
#13648 = DIRECTION ( 'NONE',  ( -0.000000000000000000, -0.000000000000000000, 1.000000000000000000 ) ) ;
#13649 = ORIENTED_EDGE ( 'NONE', *, *, #59652, .F. ) ;
#13650 = EDGE_CURVE ( 'NONE', #4734, #52681, #44539, .T. ) ;
#13651 = CARTESIAN_POINT ( 'NONE',  ( -22.42236680055709641, 157.8615022471902591, 0.000000000000000000 ) ) ;
#13652 = CARTESIAN_POINT ( 'NONE',  ( 79.17880889709233827, 46.03054149826856190, -13.20140403770785831 ) ) ;
#13653 = CARTESIAN_POINT ( 'NONE',  ( -11.40312891409031693, 78.77562236714182120, 59.99999999999999289 ) ) ;
#13654 = CARTESIAN_POINT ( 'NONE',  ( 176.1831251786226176, 274.1662096868063259, -16.54240975180354312 ) ) ;
#13655 = DIRECTION ( 'NONE',  ( -0.1580495287025880657, -0.9874311856918890351, 0.000000000000000000 ) ) ;
#13656 = EDGE_CURVE ( 'NONE', #20045, #29993, #18233, .T. ) ;
#13657 = CARTESIAN_POINT ( 'NONE',  ( 204.7705395286511703, 275.9740169735222821, 14.67688412961845579 ) ) ;
#13658 = ORIENTED_EDGE ( 'NONE', *, *, #24862, .T. ) ;
#13659 = CARTESIAN_POINT ( 'NONE',  ( 26.13094010387951371, 20.80170272979927049, 7.433330006724137462 ) ) ;
#13660 = CARTESIAN_POINT ( 'NONE',  ( 22.17733255989135088, 35.73705186507754661, -3.090169943749475845 ) ) ;
#13661 = CARTESIAN_POINT ( 'NONE',  ( 72.13796995798945488, 70.29191212227198093, -7.425297919149587145 ) ) ;
#13662 = CARTESIAN_POINT ( 'NONE',  ( 75.07870222088888568, 67.13256391452974015, -13.06718628923150582 ) ) ;
#13663 = ORIENTED_EDGE ( 'NONE', *, *, #61017, .F. ) ;
#13664 = CARTESIAN_POINT ( 'NONE',  ( 182.6072171861806623, 283.8313970932354664, 15.32190259022742929 ) ) ;
#13665 = CARTESIAN_POINT ( 'NONE',  ( 206.6298919378964740, 272.7535241315335384, -9.267551915974392429 ) ) ;
#13666 = EDGE_LOOP ( 'NONE', ( #10427, #25237, #37357, #83611 ) ) ;
#13668 = FACE_OUTER_BOUND ( 'NONE', #60144, .T. ) ;
#13667 = CARTESIAN_POINT ( 'NONE',  ( 165.5951377484445288, 285.5575308855258641, -6.564525145918313598 ) ) ;
#13669 = FACE_OUTER_BOUND ( 'NONE', #57048, .T. ) ;
#13670 = CARTESIAN_POINT ( 'NONE',  ( 66.32409466995383696, 68.70548013689253253, -2.129162495935091659 ) ) ;
#13671 = CARTESIAN_POINT ( 'NONE',  ( 160.0105735053945182, 253.5005522708592594, 16.10371386499367929 ) ) ;
#13672 = CARTESIAN_POINT ( 'NONE',  ( 85.93470712620026575, 48.23248545518190866, 11.93606436224419909 ) ) ;
#13673 = CARTESIAN_POINT ( 'NONE',  ( 10.06845959268932411, 31.07446838803123157, 10.00000000000000000 ) ) ;
#13674 = EDGE_CURVE ( 'NONE', #89979, #97433, #72632, .T. ) ;
#13675 = CARTESIAN_POINT ( 'NONE',  ( 121.1210835531159091, 249.9244531367911293, -4.594050593750046652 ) ) ;
#13676 = CARTESIAN_POINT ( 'NONE',  ( 204.8523313866422484, 275.8323493198358847, 14.65426965484541100 ) ) ;
#13677 = VERTEX_POINT ( 'NONE', #53468 ) ;
#13678 = CARTESIAN_POINT ( 'NONE',  ( 170.1416266488643316, 264.1956996214873357, 16.71664234929178505 ) ) ;
#13679 = LINE ( 'NONE', #36964, #54466 ) ;
#13680 = ORIENTED_EDGE ( 'NONE', *, *, #21060, .F. ) ;
#13681 = CARTESIAN_POINT ( 'NONE',  ( 160.2165948300100808, 253.5243271026905632, 14.75162392979510528 ) ) ;
#13682 = VERTEX_POINT ( 'NONE', #21114 ) ;
#13683 = ORIENTED_EDGE ( 'NONE', *, *, #23169, .T. ) ;
#13684 = CARTESIAN_POINT ( 'NONE',  ( 76.27744555259825177, 65.02376616331082460, 14.64893924750894350 ) ) ;
#13685 = LINE ( 'NONE', #82641, #38569 ) ;
#13686 = CARTESIAN_POINT ( 'NONE',  ( 2.117331368781439682, 160.4824982072973683, 3.021315404115420679E-15 ) ) ;
#13687 = CARTESIAN_POINT ( 'NONE',  ( 147.2784190576484491, 275.5532906641692534, 0.2793038414862047958 ) ) ;
#13688 = DIRECTION ( 'NONE',  ( 1.000000000000000000, 0.000000000000000000, 0.000000000000000000 ) ) ;
#13689 = CARTESIAN_POINT ( 'NONE',  ( 194.2669918475045279, 294.1666952169902629, 14.00965265288584050 ) ) ;
#13690 = CARTESIAN_POINT ( 'NONE',  ( 70.68522907938090327, 64.69131028183736021, 12.41109312486960015 ) ) ;
#13691 = CARTESIAN_POINT ( 'NONE',  ( 87.39560864876780499, 44.96555158233555716, 6.898727475461879699 ) ) ;
#13692 = ORIENTED_EDGE ( 'NONE', *, *, #12249, .T. ) ;
#13693 = AXIS2_PLACEMENT_3D ( 'NONE', #30130, #22535, #53422 ) ;
#13694 = LINE ( 'NONE', #64791, #64158 ) ;
#13695 = CARTESIAN_POINT ( 'NONE',  ( 66.24778991220809132, 68.20621754481172161, 4.138286745133333611 ) ) ;
#13696 = DIRECTION ( 'NONE',  ( 0.9778746070300412541, -0.2091919045418403900, 0.000000000000000000 ) ) ;
#13697 = EDGE_LOOP ( 'NONE', ( #37024, #42691, #35607, #46963 ) ) ;
#13698 = CARTESIAN_POINT ( 'NONE',  ( 71.93062239541285408, 69.86009586726821396, -7.857747555887292457 ) ) ;
#13699 = CARTESIAN_POINT ( 'NONE',  ( 76.16520121882301453, 51.58665863457357403, -16.17654979223751610 ) ) ;
#13700 = CARTESIAN_POINT ( 'NONE',  ( 174.2182000476488781, 253.7820565303687772, -7.498782541138584889 ) ) ;
#13701 = VECTOR ( 'NONE', #25855, 1000.000000000000000 ) ;
#13702 = CARTESIAN_POINT ( 'NONE',  ( 206.4768661561222984, 273.0185725604343361, 11.39716120335626925 ) ) ;
#13703 = CARTESIAN_POINT ( 'NONE',  ( -19.65312891409030271, 93.06504152958497400, 177.5919119679930134 ) ) ;
#13704 = CARTESIAN_POINT ( 'NONE',  ( 144.9103262809084924, 242.2202760586659167, -5.415160957724236172E-17 ) ) ;
#13705 = ORIENTED_EDGE ( 'NONE', *, *, #21120, .T. ) ;
#13706 = CARTESIAN_POINT ( 'NONE',  ( 88.24418735786636603, 44.41312371456485408, 4.416884733071428926 ) ) ;
#13707 = CARTESIAN_POINT ( 'NONE',  ( 85.20344164368778195, 43.30853108818458708, 4.813148867806795295 ) ) ;
#13708 = CARTESIAN_POINT ( 'NONE',  ( 88.01315147845571119, 43.76068472133272280, -2.215761827693341957 ) ) ;
#13709 = CARTESIAN_POINT ( 'NONE',  ( 150.1593742671934137, 278.0125080970104250, -1.457479655811878994 ) ) ;
#13710 = FACE_OUTER_BOUND ( 'NONE', #10090, .T. ) ;
#13711 = ORIENTED_EDGE ( 'NONE', *, *, #46180, .F. ) ;
#13712 = CARTESIAN_POINT ( 'NONE',  ( 75.95696686559092825, 52.20348117277876554, 15.83814512776487327 ) ) ;
#13713 = CARTESIAN_POINT ( 'NONE',  ( 185.2639226435235287, 277.5828175794305253, -16.89321975366465622 ) ) ;
#13714 = CARTESIAN_POINT ( 'NONE',  ( 167.5773306199838260, 249.1887448877641020, -5.496113628205799628 ) ) ;
#13715 = CARTESIAN_POINT ( 'NONE',  ( 81.18177496026471829, 52.29543988957072997, 15.18084038034863248 ) ) ;
#13716 = CARTESIAN_POINT ( 'NONE',  ( 73.70115868159994932, 69.61480312196140119, -9.646229744283855823 ) ) ;
#13717 = CARTESIAN_POINT ( 'NONE',  ( 195.6138585057339014, 264.3086811827035376, 0.8332931476443066199 ) ) ;
#13718 = EDGE_CURVE ( 'NONE', #59645, #38166, #67629, .T. ) ;
#13719 = CYLINDRICAL_SURFACE ( 'NONE', #54618, 70.00000000000002842 ) ;
#13720 = CARTESIAN_POINT ( 'NONE',  ( 182.9739835170253741, 280.6533030732829275, 16.67168179050610277 ) ) ;
#13721 = CARTESIAN_POINT ( 'NONE',  ( 195.8334532154173075, 270.5958172793855852, 12.00696150519691585 ) ) ;
#13722 = CARTESIAN_POINT ( 'NONE',  ( 20.95177465265983585, 30.83478043621388665, -8.090169943749479842 ) ) ;
#13723 = DIRECTION ( 'NONE',  ( 0.000000000000000000, 0.000000000000000000, 1.000000000000000000 ) ) ;
#13724 = LINE ( 'NONE', #36515, #96883 ) ;
#13725 = CYLINDRICAL_SURFACE ( 'NONE', #3019, 17.82106496071139645 ) ;
#13726 = CARTESIAN_POINT ( 'NONE',  ( 198.1230806404959139, 287.4877535090322453, 17.00698319228197164 ) ) ;
#13727 = CARTESIAN_POINT ( 'NONE',  ( 161.8938357633344651, 250.2386463561303458, 14.09469623995626719 ) ) ;
#13728 = CARTESIAN_POINT ( 'NONE',  ( -4.722712290662820500, 158.8923013555410080, 4.594050593750050204 ) ) ;
#13729 = CARTESIAN_POINT ( 'NONE',  ( 172.1838089403669585, 283.7306525937339075, -12.60449918999284513 ) ) ;
#13730 = ORIENTED_EDGE ( 'NONE', *, *, #94145, .F. ) ;
#13731 = CARTESIAN_POINT ( 'NONE',  ( 72.93368834549268342, 70.33274728410245302, -8.126413671899975100 ) ) ;
#13732 = CARTESIAN_POINT ( 'NONE',  ( 198.7136873185829984, 286.4647927352960437, -18.57144721070432070 ) ) ;
#13733 = CARTESIAN_POINT ( 'NONE',  ( -1.313257906909115480, 179.2369531367911293, -4.594050593750048428 ) ) ;
#13734 = CARTESIAN_POINT ( 'NONE',  ( 27.53097578467762219, 16.86426979415090699, -3.090169943749474069 ) ) ;
#13735 = CARTESIAN_POINT ( 'NONE',  ( 85.66185486794186943, 48.65504738537000406, 12.40237352552430750 ) ) ;
#13736 = CARTESIAN_POINT ( 'NONE',  ( 205.2121761402296443, 275.2090799237855094, -14.05269615702442465 ) ) ;
#13737 = CARTESIAN_POINT ( 'NONE',  ( 71.98986200492696241, 72.23686350399877654, -3.591898176886850980 ) ) ;
#13738 = DIRECTION ( 'NONE',  ( -0.3766285016932175989, 0.9263643838751153270, 0.000000000000000000 ) ) ;
#13740 = CARTESIAN_POINT ( 'NONE',  ( 70.44081555586384980, 218.1427522451419065, -10.00000000000009415 ) ) ;
#13739 = PLANE ( 'NONE',  #15324 ) ;
#13741 = CARTESIAN_POINT ( 'NONE',  ( 176.1981167356123308, 253.9691465762882672, -3.865530600323666466 ) ) ;
#13742 = CARTESIAN_POINT ( 'NONE',  ( 198.2555168952299027, 287.2583671870688704, 16.98288975666356748 ) ) ;
#13743 = AXIS2_PLACEMENT_3D ( 'NONE', #76487, #46046, #59761 ) ;
#13744 = CARTESIAN_POINT ( 'NONE',  ( 64.25234236153551137, 201.2365022471902023, -10.00000000000009059 ) ) ;
#13745 = CARTESIAN_POINT ( 'NONE',  ( 81.84820468759039613, 41.18211169042432829, 5.670485032956731786 ) ) ;
#13746 = CARTESIAN_POINT ( 'NONE',  ( 148.2980785574368952, 273.7871886041155562, 9.134436720559454770 ) ) ;
#13747 = CARTESIAN_POINT ( 'NONE',  ( 15.73713787374454043, 170.7048013555409796, 4.594050593750051981 ) ) ;
#13748 = CARTESIAN_POINT ( 'NONE',  ( 168.2754412017935977, 286.2846751750494150, 4.214248324995869766 ) ) ;
#13749 = CARTESIAN_POINT ( 'NONE',  ( -62.38288563085208693, 61.66892052422337400, 59.99999999999999289 ) ) ;
#13750 = CARTESIAN_POINT ( 'NONE',  ( 33.27084535048209091, 40.18502408145594273, 5.678558825948277544 ) ) ;
#13751 = CARTESIAN_POINT ( 'NONE',  ( 165.5845016731641124, 245.8462254865437160, 0.7221155814038995313 ) ) ;
#13752 = VECTOR ( 'NONE', #66510, 1000.000000000000000 ) ;
#13753 = FACE_OUTER_BOUND ( 'NONE', #94286, .T. ) ;
#13754 = CARTESIAN_POINT ( 'NONE',  ( 185.7319119612792520, 266.7507276504825313, 13.19901251433546641 ) ) ;
#13755 = CARTESIAN_POINT ( 'NONE',  ( -22.42236680055709641, 157.8615022471902591, 0.000000000000000000 ) ) ;
#13756 = CARTESIAN_POINT ( 'NONE',  ( 160.8891438268352374, 281.0495864612497599, 9.578199528566821996 ) ) ;
#13757 = APPLICATION_PROTOCOL_DEFINITION ( 'draft international standard', 'automotive_design', 1998, #46600 ) ;
#13758 = CARTESIAN_POINT ( 'NONE',  ( 20.49695707787433463, 14.76004757982089188, 5.678558825948272215 ) ) ;
#13759 = CARTESIAN_POINT ( 'NONE',  ( 189.8123550829396891, 301.8823524224806647, -0.5679054518196169354 ) ) ;
#13760 = DIRECTION ( 'NONE',  ( -0.8660254037844387076, -0.4999999999999998890, -0.000000000000000000 ) ) ;
#13761 = CARTESIAN_POINT ( 'NONE',  ( 71.40405452044859658, 59.30247739756921987, 15.73691996190138731 ) ) ;
#13762 = EDGE_CURVE ( 'NONE', #63494, #36466, #771, .T. ) ;
#13763 = CARTESIAN_POINT ( 'NONE',  ( 154.9344967692067598, 262.2925750810547356, 17.30210568643136781 ) ) ;
#13764 = ORIENTED_EDGE ( 'NONE', *, *, #77078, .F. ) ;
#13765 = CARTESIAN_POINT ( 'NONE',  ( 185.3399667980721972, 290.9400795177430155, 12.16828865084649536 ) ) ;
#13766 = CARTESIAN_POINT ( 'NONE',  ( 187.4166251561426293, 263.4339899954952102, 11.64397722261905166 ) ) ;
#13767 = CARTESIAN_POINT ( 'NONE',  ( 88.15969727192141647, 44.33042168331400745, 2.709744954521523308 ) ) ;
#13768 = ADVANCED_FACE ( 'NONE', ( #49256 ), #23557, .T. ) ;
#13769 = ORIENTED_EDGE ( 'NONE', *, *, #84524, .T. ) ;
#13770 = CARTESIAN_POINT ( 'NONE',  ( 195.4590938341275717, 290.3887709481238062, -16.68818639969873985 ) ) ;
#13771 = CARTESIAN_POINT ( 'NONE',  ( 82.69197927684081151, 40.54452889128955206, 0.8884936269468197700 ) ) ;
#13772 = LINE ( 'NONE', #23351, #44501 ) ;
#13773 = CARTESIAN_POINT ( 'NONE',  ( 202.9490938173916561, 279.1288534886517709, -16.56031645010252973 ) ) ;
#13774 = EDGE_LOOP ( 'NONE', ( #73707, #8671, #89866, #94192, #87422, #20562, #50702 ) ) ;
#13775 =( BOUNDED_CURVE ( )  B_SPLINE_CURVE ( 2, ( #73222, #34696, #65598, #83835, #99011, #45769, #68584, #15365, #92915 ),
 .UNSPECIFIED., .F., .T. ) 
 B_SPLINE_CURVE_WITH_KNOTS ( ( 3, 2, 2, 2, 3 ),
 ( 0.2943548387096774355, 0.2956989247311828106, 0.2983870967741935609, 0.3010752688172043112, 0.3024193548387096864 ),
 .UNSPECIFIED. ) 
 CURVE ( )  GEOMETRIC_REPRESENTATION_ITEM ( )  RATIONAL_B_SPLINE_CURVE ( ( 0.9330127018922194093, 0.9330127018922194093, 1.000000000000000000, 0.8660254037844387076, 1.000000000000000000, 0.8660254037844387076, 1.000000000000000000, 0.9330127018922194093, 0.9330127018922194093 ) ) 
 REPRESENTATION_ITEM ( '' )  );
#13776 = ORIENTED_EDGE ( 'NONE', *, *, #20226, .T. ) ;
#13778 = CARTESIAN_POINT ( 'NONE',  ( 204.6427704787179493, 276.1953194596412118, 13.28850621060895953 ) ) ;
#13777 = CARTESIAN_POINT ( 'NONE',  ( 186.5702472824191318, 272.0476927240400755, -16.61350243714774066 ) ) ;
#13779 = VERTEX_POINT ( 'NONE', #24074 ) ;
#13780 = CARTESIAN_POINT ( 'NONE',  ( 151.2455280670316711, 268.6820563007532314, 14.35914944935941229 ) ) ;
#13781 = CARTESIAN_POINT ( 'NONE',  ( 80.15404930735284950, 58.24487849859600885, -16.60713908503101521 ) ) ;
#13782 = CARTESIAN_POINT ( 'NONE',  ( 80.24454609401104221, 57.41156006636176556, -16.59009416930489422 ) ) ;
#13783 = CARTESIAN_POINT ( 'NONE',  ( -19.65312891409030271, 93.06504152958497400, 10.00000000000000888 ) ) ;
#13785 = EDGE_CURVE ( 'NONE', #34934, #41570, #85426, .T. ) ;
#13784 = VERTEX_POINT ( 'NONE', #84914 ) ;
#13786 = CARTESIAN_POINT ( 'NONE',  ( -16.99542894172669349, 24.36904009834038476, 10.00000000000000000 ) ) ;
#13787 = B_SPLINE_CURVE_WITH_KNOTS ( 'NONE', 3,
 ( #8693, #39562, #101, #31476, #23376, #76597, #85233, #38068, #47675, #16288, #15779, #69977, #7182, #24884, #93841, #38581, #47182, #40069 ),
 .UNSPECIFIED., .F., .F.,
 ( 4, 2, 2, 2, 2, 2, 2, 2, 4 ),
 ( 0.0001829895512004093639, 0.0005381298376754407690, 0.0008932701241504720658, 0.001248410410625503363, 0.001603550697100531407, 0.001958690983575559017, 0.002313831270050587061, 0.002668971556525614672, 0.003024111843000642282 ),
 .UNSPECIFIED. ) ;
#13788 = ORIENTED_EDGE ( 'NONE', *, *, #65951, .F. ) ;
#13789 = CARTESIAN_POINT ( 'NONE',  ( 164.2813349609167517, 246.1033764428878214, 1.949810150281061638 ) ) ;
#13790 = CARTESIAN_POINT ( 'NONE',  ( 150.8555837531579868, 276.0290483310748755, -8.437460036063264113 ) ) ;
#13791 = ORIENTED_EDGE ( 'NONE', *, *, #83109, .F. ) ;
#13792 = CARTESIAN_POINT ( 'NONE',  ( 149.3833831332874240, 271.9073859370555510, 11.40518020539810173 ) ) ;
#13793 = CARTESIAN_POINT ( 'NONE',  ( 172.2573413188522977, 264.0388785342783535, -16.66050399420761607 ) ) ;
#13794 = ORIENTED_EDGE ( 'NONE', *, *, #88245, .F. ) ;
#13795 = CARTESIAN_POINT ( 'NONE',  ( 161.1881684952116416, 277.3746372515906273, -13.39559945919683948 ) ) ;
#13796 = EDGE_CURVE ( 'NONE', #13906, #74614, #45898, .T. ) ;
#13797 = CARTESIAN_POINT ( 'NONE',  ( 31.60618414714233637, 41.18080186712595747, 3.090169943749475401 ) ) ;
#13798 = CARTESIAN_POINT ( 'NONE',  ( -13.11024591527723615, 27.99999999999999645, -32.50000000000017053 ) ) ;
#13799 = CARTESIAN_POINT ( 'NONE',  ( 47.84007798744509898, 106.1754093786579318, 10.00000000000000000 ) ) ;
#13800 = ORIENTED_EDGE ( 'NONE', *, *, #46624, .F. ) ;
#13801 = VERTEX_POINT ( 'NONE', #61566 ) ;
#13802 = CARTESIAN_POINT ( 'NONE',  ( 82.53565421717173933, 50.59536920694240791, -14.66185160561549594 ) ) ;
#13803 = CARTESIAN_POINT ( 'NONE',  ( 190.1858949294064871, 301.2353624297489887, -5.249932979468886707 ) ) ;
#13804 = CARTESIAN_POINT ( 'NONE',  ( 188.3515280933679890, 299.0335169455429423, -5.233410187156488647 ) ) ;
#13805 = DIRECTION ( 'NONE',  ( 1.000000000000000000, 0.000000000000000000, 0.000000000000000000 ) ) ;
#13806 = CARTESIAN_POINT ( 'NONE',  ( 153.1973045377566507, 265.3014802884401320, 17.70608187426261892 ) ) ;
#13807 = CARTESIAN_POINT ( 'NONE',  ( 191.2490492842387368, 299.3939250708912141, 9.771632328273542001 ) ) ;
#13808 = CARTESIAN_POINT ( 'NONE',  ( 146.9456733906991417, 276.1296230653242105, -0.7988785540157754550 ) ) ;
#13809 = ORIENTED_EDGE ( 'NONE', *, *, #39078, .F. ) ;
#13810 = CARTESIAN_POINT ( 'NONE',  ( 72.28945313610159928, 58.55580128780883342, -15.58200032445072125 ) ) ;
#13812 = CARTESIAN_POINT ( 'NONE',  ( -76.38857681351474582, 54.22815603855766398, -10.00000000000000000 ) ) ;
#13811 = CARTESIAN_POINT ( 'NONE',  ( 149.3141802193904368, 272.0272488999566463, -11.40332369054239336 ) ) ;
#13813 = CARTESIAN_POINT ( 'NONE',  ( 189.5821670815687412, 300.5718190871559159, 1.753508275674212413 ) ) ;
#13814 = DIRECTION ( 'NONE',  ( -0.9762143704923794685, 0.2168075248790210796, 0.000000000000000000 ) ) ;
#13815 = CARTESIAN_POINT ( 'NONE',  ( 102.8537940617441819, 224.0643266524160140, 9.188101187500095079 ) ) ;
#13816 = ORIENTED_EDGE ( 'NONE', *, *, #1880, .T. ) ;
#13817 = CARTESIAN_POINT ( 'NONE',  ( 149.5844699681647683, 271.5590933223148227, -11.62982666799845788 ) ) ;
#13818 = EDGE_CURVE ( 'NONE', #88596, #30831, #51670, .T. ) ;
#13819 = CARTESIAN_POINT ( 'NONE',  ( 79.41195711930690493, 53.07626158231409619, -15.66850831761463070 ) ) ;
#13820 = EDGE_CURVE ( 'NONE', #22997, #25763, #24814, .T. ) ;
#13821 = CARTESIAN_POINT ( 'NONE',  ( 149.0332838374355617, 273.1880737991430124, 9.708030931401681940 ) ) ;
#13822 = CARTESIAN_POINT ( 'NONE',  ( 79.49951204047911801, 46.37032438487754149, 12.70281872619212393 ) ) ;
#13823 = AXIS2_PLACEMENT_3D ( 'NONE', #79538, #80534, #12093 ) ;
#13824 = CARTESIAN_POINT ( 'NONE',  ( 31.52185460810256856, 85.49507869652470049, 59.99999999999999289 ) ) ;
#13825 = CARTESIAN_POINT ( 'NONE',  ( 83.66603977373949874, 52.22634557578435732, -14.68915192515179235 ) ) ;
#13826 = ORIENTED_EDGE ( 'NONE', *, *, #8795, .T. ) ;
#13828 = EDGE_CURVE ( 'NONE', #42192, #32489, #30686, .T. ) ;
#13827 = CARTESIAN_POINT ( 'NONE',  ( 168.1460105092157846, 253.8898197004758117, -11.82587461664797779 ) ) ;
#13829 = DIRECTION ( 'NONE',  ( -0.000000000000000000, -0.000000000000000000, 1.000000000000000000 ) ) ;
#13830 = CARTESIAN_POINT ( 'NONE',  ( 155.3692710881836661, 261.9322098443626601, 16.97327933481185624 ) ) ;
#13831 = CARTESIAN_POINT ( 'NONE',  ( 43.66619682219493370, 206.0177522451419350, 5.000000000000046185 ) ) ;
#13832 = CARTESIAN_POINT ( 'NONE',  ( 120.0931990297694085, 230.9548013555409796, -4.594050593750042211 ) ) ;
#13833 = AXIS2_PLACEMENT_3D ( 'NONE', #82716, #11305, #97882 ) ;
#13834 = CARTESIAN_POINT ( 'NONE',  ( -19.65312891409030271, 93.06504152958497400, 177.5919119679930134 ) ) ;
#13835 = ADVANCED_FACE ( 'NONE', ( #95903 ), #78292, .T. ) ;
#13836 = CARTESIAN_POINT ( 'NONE',  ( 165.5298684834693574, 269.3554679133272884, -17.63324793928101997 ) ) ;
#13837 = CARTESIAN_POINT ( 'NONE',  ( 157.0957870390718369, 258.5491105237443321, 17.69218919045495397 ) ) ;
#13838 = CARTESIAN_POINT ( 'NONE',  ( 172.2297690901025646, 250.8531890094506878, -4.040578270607043443 ) ) ;
#13839 = CARTESIAN_POINT ( 'NONE',  ( 39.55283647781661216, 184.4548013555409796, -4.594050593750042211 ) ) ;
#13840 = DIRECTION ( 'NONE',  ( 0.6116140086401538056, -0.7911563084720502070, 0.000000000000000000 ) ) ;
#13841 = ORIENTED_EDGE ( 'NONE', *, *, #77873, .F. ) ;
#13843 = EDGE_CURVE ( 'NONE', #8304, #130, #90655, .T. ) ;
#13842 = DIRECTION ( 'NONE',  ( 0.000000000000000000, 0.000000000000000000, -1.000000000000000000 ) ) ;
#13844 = CARTESIAN_POINT ( 'NONE',  ( 81.89485588203808675, 55.22971306509118250, 16.24120679747552032 ) ) ;
#13845 = EDGE_CURVE ( 'NONE', #70075, #27651, #28995, .T. ) ;
#13846 = CARTESIAN_POINT ( 'NONE',  ( 19.39713158799116499, 193.5530062829863311, -4.648177544792955347E-16 ) ) ;
#13847 = CARTESIAN_POINT ( 'NONE',  ( 190.9380839614473473, 299.9325328093580652, -5.232187664503159752 ) ) ;
#13848 = DIRECTION ( 'NONE',  ( 0.5000000000000014433, -0.8660254037844378194, 0.000000000000000000 ) ) ;
#13849 = CARTESIAN_POINT ( 'NONE',  ( 164.4288763552480646, 253.6070193120362148, -14.40234560624782389 ) ) ;
#13850 = CARTESIAN_POINT ( 'NONE',  ( 178.0315741628076012, 287.5935043698759728, -13.06113257055532451 ) ) ;
#13851 = CARTESIAN_POINT ( 'NONE',  ( 68.74436278108203169, 64.70250930642976073, -12.15889933130203637 ) ) ;
#13852 = CARTESIAN_POINT ( 'NONE',  ( 111.2883471010299274, 228.3927522451418213, 10.00000000000009592 ) ) ;
#13853 = ORIENTED_EDGE ( 'NONE', *, *, #51571, .T. ) ;
#13854 = CARTESIAN_POINT ( 'NONE',  ( 195.0751939884018782, 266.5450544056012063, -7.747489274975008833 ) ) ;
#13855 = CARTESIAN_POINT ( 'NONE',  ( 155.1510707464528025, 280.2034007906984812, -2.423017525748603962 ) ) ;
#13856 = CARTESIAN_POINT ( 'NONE',  ( 154.0926933875380485, 264.1656124941568464, 16.59860039027621426 ) ) ;
#13857 = CIRCLE ( 'NONE', #49445, 0.1418229129680897982 ) ;
#13858 = CARTESIAN_POINT ( 'NONE',  ( 12.40843950188935629, 165.7202760586659736, -5.415160957724236172E-17 ) ) ;
#13859 = CARTESIAN_POINT ( 'NONE',  ( 5.272250483539712818, 24.81751292744053927, -6.180339887498951690 ) ) ;
#13860 = CARTESIAN_POINT ( 'NONE',  ( 192.3455884257783453, 272.0184315964207258, 14.19712417015736605 ) ) ;
#13861 = CARTESIAN_POINT ( 'NONE',  ( 71.79142014069363142, 59.57573540338584195, -15.72233485351718230 ) ) ;
#13862 = LINE ( 'NONE', #52851, #36169 ) ;
#13864 = CARTESIAN_POINT ( 'NONE',  ( 45.15450443884093090, 203.0024278399160949, 9.188101187500095079 ) ) ;
#13863 = CARTESIAN_POINT ( 'NONE',  ( 197.6572998268543699, 277.0061036579921279, -15.32695017695141892 ) ) ;
#13865 = CARTESIAN_POINT ( 'NONE',  ( 208.0287371622045782, 270.3306531311065442, 3.558879245883286746 ) ) ;
#13866 = CARTESIAN_POINT ( 'NONE',  ( 38.65784837781280459, 56.65029301956750629, -10.00000000000000000 ) ) ;
#13867 = CARTESIAN_POINT ( 'NONE',  ( 67.79725476218452229, 65.71048819351143777, 10.00598338191753101 ) ) ;
#13868 = CARTESIAN_POINT ( 'NONE',  ( 66.07327459268398684, 68.54940412191220389, -4.524685454579428168 ) ) ;
#13869 = ORIENTED_EDGE ( 'NONE', *, *, #98665, .T. ) ;
#13870 = VECTOR ( 'NONE', #55054, 1000.000000000000000 ) ;
#13871 = CARTESIAN_POINT ( 'NONE',  ( 13.08467475460494001, 168.3615022471902023, 5.000000000000051514 ) ) ;
#13872 = CARTESIAN_POINT ( 'NONE',  ( 163.8947349411736525, 246.7729873192901664, -5.868803394723933309 ) ) ;
#13873 = CARTESIAN_POINT ( 'NONE',  ( 141.5541307454787727, 252.5333772461660260, 9.188101187500095079 ) ) ;
#13874 = CARTESIAN_POINT ( 'NONE',  ( 23.65314546706850862, 31.84336893147757408, -7.433330006724137462 ) ) ;
#13875 = CARTESIAN_POINT ( 'NONE',  ( 164.3112480427713251, 246.0515654653044351, 1.977753308040909319 ) ) ;
#13876 = CARTESIAN_POINT ( 'NONE',  ( 83.70956241415673560, 51.66838590121233210, -14.83800726304596118 ) ) ;
#13877 = CARTESIAN_POINT ( 'NONE',  ( 66.11068853694165171, 215.6427522451419065, 10.00000000000009415 ) ) ;
#13879 = CARTESIAN_POINT ( 'NONE',  ( 75.10353227920388974, 67.08955699197328215, 13.10598502456514503 ) ) ;
#13878 = CARTESIAN_POINT ( 'NONE',  ( 88.11819866784119881, 43.86870363832048270, 2.501606352371071651 ) ) ;
#13880 = CARTESIAN_POINT ( 'NONE',  ( 68.58822102335196291, 64.27314873672484907, 12.42572437470450986 ) ) ;
#13881 = ORIENTED_EDGE ( 'NONE', *, *, #31531, .T. ) ;
#13882 = CARTESIAN_POINT ( 'NONE',  ( 190.8623743139412454, 300.0636657654615647, 8.577953960666059530 ) ) ;
#13883 = CARTESIAN_POINT ( 'NONE',  ( 164.0776496603550925, 246.4561697322156419, 8.566708626497000267 ) ) ;
#13884 = CARTESIAN_POINT ( 'NONE',  ( 151.3542526322075901, 269.2885850756041464, -14.28695254860580199 ) ) ;
#13885 = CARTESIAN_POINT ( 'NONE',  ( -72.48190909937208914, 49.06123820388767598, 10.00000000000000000 ) ) ;
#13886 = CARTESIAN_POINT ( 'NONE',  ( 194.0943399085664396, 271.0983644945322339, -13.64356464264049507 ) ) ;
#13887 = EDGE_LOOP ( 'NONE', ( #33896, #26230, #89016, #75010 ) ) ;
#13888 = CARTESIAN_POINT ( 'NONE',  ( 80.20857538925844210, 44.21345027839175401, -11.30608575764590107 ) ) ;
#13889 = EDGE_CURVE ( 'NONE', #705, #37697, #36144, .T. ) ;
#13890 = DIRECTION ( 'NONE',  ( -0.000000000000000000, 0.000000000000000000, 1.000000000000000000 ) ) ;
#13891 = AXIS2_PLACEMENT_3D ( 'NONE', #89163, #19709, #18701 ) ;
#13892 = CARTESIAN_POINT ( 'NONE',  ( 71.65793835465373718, 72.08874482037508358, 0.6792430321896046896 ) ) ;
#13893 = EDGE_CURVE ( 'NONE', #15824, #7154, #48643, .T. ) ;
#13894 = CYLINDRICAL_SURFACE ( 'NONE', #66760, 10.00000000000010658 ) ;
#13895 = CARTESIAN_POINT ( 'NONE',  ( 20.97457486420976380, 194.4637435831424739, 2.679491924311251605 ) ) ;
#13896 = CARTESIAN_POINT ( 'NONE',  ( 89.42916389074625272, 233.9860189848785694, -2.679491924311252493 ) ) ;
#13897 = CARTESIAN_POINT ( 'NONE',  ( 149.0710170770012724, 245.3262482093457777, 3.021315404115420679E-15 ) ) ;
#13898 = CARTESIAN_POINT ( 'NONE',  ( 201.1060504099706350, 282.3210983108598384, -18.18000168485860257 ) ) ;
#13899 = PLANE ( 'NONE',  #50306 ) ;
#13900 = CARTESIAN_POINT ( 'NONE',  ( 13.13113612116928763, 15.78052372038639106, -10.00000000000000355 ) ) ;
#13901 = CARTESIAN_POINT ( 'NONE',  ( 192.0527661830250565, 287.4924844977863359, -16.47094169987085266 ) ) ;
#13902 = VERTEX_POINT ( 'NONE', #63826 ) ;
#13903 = CARTESIAN_POINT ( 'NONE',  ( 190.8072577185990610, 300.1591305089344814, 3.698484652594827171 ) ) ;
#13904 = DIRECTION ( 'NONE',  ( 0.000000000000000000, -0.000000000000000000, 1.000000000000000000 ) ) ;
#13905 = CARTESIAN_POINT ( 'NONE',  ( 189.2141853381722001, 297.1461156523275235, 8.137912133790496938 ) ) ;
#13906 = VERTEX_POINT ( 'NONE', #6285 ) ;
#13908 = EDGE_CURVE ( 'NONE', #41583, #78218, #30355, .T. ) ;
#13907 = EDGE_LOOP ( 'NONE', ( #25591, #83308, #23226, #22511 ) ) ;
#13909 = CARTESIAN_POINT ( 'NONE',  ( 30.67947171958994090, 41.21091486745863364, -1.111400068045478839E-16 ) ) ;
#13910 = CARTESIAN_POINT ( 'NONE',  ( 176.6943099527350682, 256.7931168052207340, -11.17617521364210731 ) ) ;
#13911 = B_SPLINE_CURVE_WITH_KNOTS ( 'NONE', 3,
 ( #39851, #62664, #47475, #70784, #55558, #25696, #9495, #11873, #86051, #55066, #32275, #43233, #48489, #74174, #1395, #50347, #24677, #4246, #25176, #56576, #79430, #71804, #94122, #93616, #88932, #40858, #24184, #78399, #63178, #19491, #2401 ),
 .UNSPECIFIED., .F., .F.,
 ( 4, 3, 3, 3, 3, 3, 3, 3, 3, 3, 4 ),
 ( 0.000000000000000000, 0.1333490885032357076, 0.3007194338854359827, 0.4699862290245028773, 0.5844252810809169585, 0.6686540514502661292, 0.7354980260655498148, 0.8028463152565713523, 0.8633854507757302565, 0.9437142632667330222, 1.000000000000000000 ),
 .UNSPECIFIED. ) ;
#13912 = CARTESIAN_POINT ( 'NONE',  ( 204.7986527064648214, 275.9253235211867263, 14.74587861556245905 ) ) ;
#13913 = DIRECTION ( 'NONE',  ( -0.000000000000000000, 0.000000000000000000, -1.000000000000000000 ) ) ;
#13914 = CARTESIAN_POINT ( 'NONE',  ( 56.45811372747556334, 196.7365022471902023, -10.00000000000009237 ) ) ;
#13915 = ORIENTED_EDGE ( 'NONE', *, *, #81117, .T. ) ;
#13916 = CARTESIAN_POINT ( 'NONE',  ( 98.14495447654879001, 215.2202760586659167, -5.415160957724236172E-17 ) ) ;
#13917 = CARTESIAN_POINT ( 'NONE',  ( 155.0965287368403835, 262.0119274806629051, 17.25554003307136597 ) ) ;
#13918 = CARTESIAN_POINT ( 'NONE',  ( 73.07600783879472317, 69.60248043393922046, -9.824339152688605026 ) ) ;
#13919 = CARTESIAN_POINT ( 'NONE',  ( 177.8829175822941693, 268.9868278392930847, -16.69667492248571250 ) ) ;
#13920 = CARTESIAN_POINT ( 'NONE',  ( 81.23681747614864435, 42.40944431637972656, -7.576782141913678714 ) ) ;
#13921 = ORIENTED_EDGE ( 'NONE', *, *, #67570, .T. ) ;
#13922 = APPLICATION_CONTEXT ( 'automotive_design' ) ;
#13923 = EDGE_CURVE ( 'NONE', #83671, #53015, #70427, .T. ) ;
#13924 = ORIENTED_EDGE ( 'NONE', *, *, #76177, .F. ) ;
#13925 = EDGE_CURVE ( 'NONE', #17814, #41047, #87208, .T. ) ;
#13926 = ORIENTED_EDGE ( 'NONE', *, *, #41427, .T. ) ;
#13927 = CARTESIAN_POINT ( 'NONE',  ( 73.76584831522593788, 68.38082682530667000, 11.49424229391076402 ) ) ;
#13928 = ORIENTED_EDGE ( 'NONE', *, *, #96808, .T. ) ;
#13929 = CARTESIAN_POINT ( 'NONE',  ( 70.43095659816272303, 71.06107982962434733, 2.817390920827290923 ) ) ;
#13930 = EDGE_LOOP ( 'NONE', ( #85636, #48558, #61291, #64500 ) ) ;
#13931 = CARTESIAN_POINT ( 'NONE',  ( -19.65312891409030271, 93.06504152958497400, 177.5919119679930134 ) ) ;
#13932 = CARTESIAN_POINT ( 'NONE',  ( -23.49900916367506198, 99.79204404934422712, 45.19947629006753687 ) ) ;
#13933 = CARTESIAN_POINT ( 'NONE',  ( 70.10515995482631979, 68.44220587271549050, -8.343978931046503789 ) ) ;
#13934 = CARTESIAN_POINT ( 'NONE',  ( 165.0963524469224808, 264.4083487871739067, -17.41401503043321952 ) ) ;
#13935 = ORIENTED_EDGE ( 'NONE', *, *, #31039, .T. ) ;
#13936 = CARTESIAN_POINT ( 'NONE',  ( 66.06214068257196459, 68.71579393632853794, -0.4716098740908659659 ) ) ;
#13937 = CARTESIAN_POINT ( 'NONE',  ( 16.86928618479236164, 18.24335787977762990, -9.188101187500008038 ) ) ;
#13938 = ORIENTED_EDGE ( 'NONE', *, *, #90752, .T. ) ;
#13939 = VECTOR ( 'NONE', #60164, 1000.000000000000000 ) ;
#13940 = CARTESIAN_POINT ( 'NONE',  ( 164.0935187385000802, 281.7221265701088555, 8.691696607283486031 ) ) ;
#13941 = CARTESIAN_POINT ( 'NONE',  ( 183.5953950971229744, 289.9057545191589043, -13.74357891376704544 ) ) ;
#13943 = ORIENTED_EDGE ( 'NONE', *, *, #14414, .F. ) ;
#13942 = CARTESIAN_POINT ( 'NONE',  ( 46.99867368304095550, 76.19044720721625197, -10.00000000000000000 ) ) ;
#13944 = CARTESIAN_POINT ( 'NONE',  ( 163.3706531435203146, 247.6807236201477735, 10.06957846017757241 ) ) ;
#13945 = CARTESIAN_POINT ( 'NONE',  ( 188.2597630871935905, 260.7361237437183377, 2.610217646800272906 ) ) ;
#13946 = CARTESIAN_POINT ( 'NONE',  ( 160.2954372498352598, 280.8823328917059712, -6.618626993187716856 ) ) ;
#13947 = DIRECTION ( 'NONE',  ( -1.000000000000000000, 0.000000000000000000, 0.000000000000000000 ) ) ;
#13948 = AXIS2_PLACEMENT_3D ( 'NONE', #74137, #81263, #13805 ) ;
#13949 = PLANE ( 'NONE',  #20467 ) ;
#13950 = CARTESIAN_POINT ( 'NONE',  ( 161.1990332043106946, 251.4420796895884394, 14.26998817770995487 ) ) ;
#13951 = CARTESIAN_POINT ( 'NONE',  ( 159.2007417150840922, 281.7182816310744329, 2.076871834512827864 ) ) ;
#13952 = ORIENTED_EDGE ( 'NONE', *, *, #20471, .F. ) ;
#13954 = EDGE_CURVE ( 'NONE', #31220, #57520, #51057, .T. ) ;
#13953 = CARTESIAN_POINT ( 'NONE',  ( 194.5735419582797192, 293.6357348500615103, -15.26985155323035137 ) ) ;
#13955 = CARTESIAN_POINT ( 'NONE',  ( 71.25860280237223776, 63.33879986367642090, -13.50434263417577263 ) ) ;
#13956 = CARTESIAN_POINT ( 'NONE',  ( 160.5931239613893524, 275.7977860495605000, 12.74539326669525252 ) ) ;
#13957 = CARTESIAN_POINT ( 'NONE',  ( -3.099174982164758951, 179.0177522451419350, 5.000000000000046185 ) ) ;
#13958 = ADVANCED_FACE ( 'NONE', ( #1549 ), #55210, .T. ) ;
#13959 = CARTESIAN_POINT ( 'NONE',  ( 192.7698958495311388, 267.0084935405105853, -11.19755117076729256 ) ) ;
#13960 = EDGE_CURVE ( 'NONE', #79412, #51044, #74931, .T. ) ;
#13961 = CARTESIAN_POINT ( 'NONE',  ( 171.5105039590924321, 279.6811076753780867, -14.64826990109219551 ) ) ;
#13962 = CARTESIAN_POINT ( 'NONE',  ( 163.4609802778453513, 247.5242724341946712, -7.586713275286927072 ) ) ;
#13963 = CARTESIAN_POINT ( 'NONE',  ( 169.6860864027741798, 284.9274174890383620, -11.04576083116783103 ) ) ;
#13964 = DIRECTION ( 'NONE',  ( -0.1887253692075926415, 0.9820299053580078263, 0.000000000000000000 ) ) ;
#13966 = CARTESIAN_POINT ( 'NONE',  ( 76.27744555259825177, 65.02376616331082460, 14.64893924750894705 ) ) ;
#13965 = CARTESIAN_POINT ( 'NONE',  ( -10.21716836350912949, 177.1589784336661637, -6.496448406907675876E-16 ) ) ;
#13967 = CARTESIAN_POINT ( 'NONE',  ( 27.98206807853016542, 175.4155109091896065, 2.679491924311254714 ) ) ;
#13968 = ORIENTED_EDGE ( 'NONE', *, *, #90314, .F. ) ;
#13969 = ADVANCED_FACE ( 'NONE', ( #80071 ), #32922, .F. ) ;
#13970 = VECTOR ( 'NONE', #70278, 1000.000000000000114 ) ;
#13971 = ORIENTED_EDGE ( 'NONE', *, *, #92441, .F. ) ;
#13972 = PLANE ( 'NONE',  #30636 ) ;
#13973 = DIRECTION ( 'NONE',  ( -0.8660254037844377084, -0.5000000000000014433, -0.000000000000000000 ) ) ;
#13974 = CARTESIAN_POINT ( 'NONE',  ( 171.6461529521897944, 289.6503080272315174, 2.692092882840170454 ) ) ;
#13975 = VECTOR ( 'NONE', #48368, 1000.000000000000000 ) ;
#13976 = CARTESIAN_POINT ( 'NONE',  ( -22.42236680055709641, 157.8615022471902591, 0.000000000000000000 ) ) ;
#13977 = CARTESIAN_POINT ( 'NONE',  ( 202.0120093381390802, 280.7519314177017691, -17.07120787497099101 ) ) ;
#13978 = CARTESIAN_POINT ( 'NONE',  ( 81.04961468568201610, 43.68546784643918812, -9.492462169003026418 ) ) ;
#13979 = CARTESIAN_POINT ( 'NONE',  ( 150.1232578106812241, 276.5731483457047943, 3.538916378592138923 ) ) ;
#13980 = CARTESIAN_POINT ( 'NONE',  ( 9.836819166815537585, 185.6744531367911293, 4.594050593750047540 ) ) ;
#13981 = CARTESIAN_POINT ( 'NONE',  ( 119.3079296378835181, 245.8149278399160949, -9.188101187500095079 ) ) ;
#13982 = CARTESIAN_POINT ( 'NONE',  ( 87.82209769797702847, 44.43170261543946964, -3.947207905613685952 ) ) ;
#13983 = CARTESIAN_POINT ( 'NONE',  ( 183.2725204446199143, 257.5467570156531565, -3.032576513086016057 ) ) ;
#13984 = CARTESIAN_POINT ( 'NONE',  ( 79.42866338260434134, 59.50128377535573776, 16.18467811310512872 ) ) ;
#13985 = CARTESIAN_POINT ( 'NONE',  ( 178.4067385319158632, 283.6684656904566282, -14.65910435069753781 ) ) ;
#13986 = CARTESIAN_POINT ( 'NONE',  ( 80.24139587601152357, 53.52586694347819929, -15.66200724048011672 ) ) ;
#13987 = CARTESIAN_POINT ( 'NONE',  ( 66.10228174255657052, 68.64626758096548542, 4.271897712742705799 ) ) ;
#13988 = CARTESIAN_POINT ( 'NONE',  ( 161.8150574665248200, 250.3750943687383881, -13.25074899737357903 ) ) ;
#13989 = CARTESIAN_POINT ( 'NONE',  ( 189.7272758596897972, 284.7347432595483383, 17.38904331496314271 ) ) ;
#13990 = CARTESIAN_POINT ( 'NONE',  ( 84.54066908761240029, 50.65850875116926488, 13.71172019562601285 ) ) ;
#13991 = CARTESIAN_POINT ( 'NONE',  ( 186.8003541658358984, 299.2222177555264011, -0.6103433986344138917 ) ) ;
#13992 = FACE_OUTER_BOUND ( 'NONE', #57411, .T. ) ;
#13993 = CARTESIAN_POINT ( 'NONE',  ( 164.2659629401757968, 252.9733372042652491, -12.96157098613237046 ) ) ;
#13994 = DIRECTION ( 'NONE',  ( 1.000000000000000000, 0.000000000000000000, 0.000000000000000000 ) ) ;
#13995 = CARTESIAN_POINT ( 'NONE',  ( 181.7546150825112932, 268.0742755205600361, 15.00729537999377072 ) ) ;
#13996 = EDGE_CURVE ( 'NONE', #35708, #5362, #25849, .T. ) ;
#13997 = CARTESIAN_POINT ( 'NONE',  ( 97.11602866590727956, 233.0024278399160664, 9.188101187500095079 ) ) ;
#13998 = CARTESIAN_POINT ( 'NONE',  ( 13.25720545158990937, 8.449665230724928477, -2.296566073217252530E-15 ) ) ;
#13999 = CARTESIAN_POINT ( 'NONE',  ( 190.7851751463332164, 300.1973786460605425, 8.237717828100052486 ) ) ;
#14000 = CARTESIAN_POINT ( 'NONE',  ( 158.9391986220684885, 259.2430622464574981, -17.23821710380677530 ) ) ;
#14002 = CARTESIAN_POINT ( 'NONE',  ( 82.60090280491364467, 41.94575979494328521, -5.057853582627321209 ) ) ;
#14001 = CARTESIAN_POINT ( 'NONE',  ( -27.77457187288641904, 24.79904599702367562, 10.00000000000000000 ) ) ;
#14003 = CARTESIAN_POINT ( 'NONE',  ( 203.2640693213759846, 272.1719133495528240, -9.742646638232304923 ) ) ;
#14004 = CARTESIAN_POINT ( 'NONE',  ( 198.5954523381739989, 286.6695817285962562, -18.45134152028667174 ) ) ;
#14005 = CARTESIAN_POINT ( 'NONE',  ( 48.16808589598787904, 104.3116767361652535, -10.00000000000000000 ) ) ;
#14006 = AXIS2_PLACEMENT_3D ( 'NONE', #23254, #91703, #100285 ) ;
#14007 = CARTESIAN_POINT ( 'NONE',  ( 32.92443518896833154, 39.98502408145595410, -5.678558825948271327 ) ) ;
#14008 = CARTESIAN_POINT ( 'NONE',  ( 192.6170194583582429, 297.0245312260774995, -11.90166228306590490 ) ) ;
#14009 = CARTESIAN_POINT ( 'NONE',  ( 203.3286960320409094, 267.8359400968079171, 2.569349860321338941 ) ) ;
#14010 = VERTEX_POINT ( 'NONE', #87708 ) ;
#14011 = CARTESIAN_POINT ( 'NONE',  ( 18.31869600479030424, 33.68290643055186706, 3.479690158560446702E-15 ) ) ;
#14012 = CARTESIAN_POINT ( 'NONE',  ( 13.57497413706089517, 16.03677371833800436, 10.00000000000000533 ) ) ;
#14013 = VECTOR ( 'NONE', #81523, 1000.000000000000000 ) ;
#14014 = CARTESIAN_POINT ( 'NONE',  ( 192.4212750754384160, 297.3635704425909125, -12.73704185013552248 ) ) ;
#14015 = CARTESIAN_POINT ( 'NONE',  ( 196.7130436017243653, 289.9300093007386749, -16.33278734947153765 ) ) ;
#14016 = AXIS2_PLACEMENT_3D ( 'NONE', #44816, #75752, #6336 ) ;
#14017 = CARTESIAN_POINT ( 'NONE',  ( 70.39311885314104700, 61.02709512477209586, 14.38506243159549314 ) ) ;
#14018 = CARTESIAN_POINT ( 'NONE',  ( 75.96213316711562413, 65.70078031631311433, -14.22672748915905316 ) ) ;
#14019 = CARTESIAN_POINT ( 'NONE',  ( 73.57796644695659438, 59.01413344347207612, 16.12674309221841895 ) ) ;
#14020 = CARTESIAN_POINT ( 'NONE',  ( 172.9891656436891196, 253.8445998218816726, -8.983167006877987859 ) ) ;
#14021 = CARTESIAN_POINT ( 'NONE',  ( 142.0502911348376358, 239.4865022471901455, 1.119607411625061291E-15 ) ) ;
#14022 = ORIENTED_EDGE ( 'NONE', *, *, #57800, .F. ) ;
#14023 = EDGE_LOOP ( 'NONE', ( #78630, #22964, #77161, #16147 ) ) ;
#14024 = CARTESIAN_POINT ( 'NONE',  ( -25.89332989531674301, 24.59406508915897760, 10.00000000000000000 ) ) ;
#14025 = CARTESIAN_POINT ( 'NONE',  ( -19.65312891409030271, 93.06504152958497400, 177.5919119679930134 ) ) ;
#14026 = ORIENTED_EDGE ( 'NONE', *, *, #87652, .T. ) ;
#14027 = CARTESIAN_POINT ( 'NONE',  ( 181.4130213927826389, 290.9717498374031379, -11.17998538662018326 ) ) ;
#14029 = EDGE_CURVE ( 'NONE', #61860, #89848, #10642, .T. ) ;
#14028 = ORIENTED_EDGE ( 'NONE', *, *, #66044, .F. ) ;
#14030 = CARTESIAN_POINT ( 'NONE',  ( 86.46015012553586132, 47.50298594968677435, -10.46242490754989518 ) ) ;
#14031 = CARTESIAN_POINT ( 'NONE',  ( 158.7260964210017562, 256.4256569865397637, 16.36035822569746756 ) ) ;
#14032 = CARTESIAN_POINT ( 'NONE',  ( 190.7223573502357681, 278.9099053379666771, -16.52215294300326320 ) ) ;
#14033 = CARTESIAN_POINT ( 'NONE',  ( 153.7548618668677705, 264.3357626662872235, -16.52670224644400676 ) ) ;
#14034 = CARTESIAN_POINT ( 'NONE',  ( 200.6680263064462792, 283.0797783131037022, -17.21821073473145347 ) ) ;
#14035 = CARTESIAN_POINT ( 'NONE',  ( -52.32156893544651410, 31.15564784356141814, -10.00000000000000000 ) ) ;
#14036 = CARTESIAN_POINT ( 'NONE',  ( 37.26657704017246431, 36.91421378149922816, 9.188101187500008038 ) ) ;
#14037 = VECTOR ( 'NONE', #96964, 1000.000000000000227 ) ;
#14038 = CARTESIAN_POINT ( 'NONE',  ( 148.6829486123639015, 276.4333369876038091, 4.903683765799150329 ) ) ;
#14040 = ADVANCED_FACE ( 'NONE', ( #2036 ), #72057, .F. ) ;
#14039 = CARTESIAN_POINT ( 'NONE',  ( 36.25628400652970384, 53.06077264917335867, -10.00000000000000000 ) ) ;
#14041 = CARTESIAN_POINT ( 'NONE',  ( 87.66480641278828045, 45.41976245752641006, 6.618816385381215639 ) ) ;
#14042 = AXIS2_PLACEMENT_3D ( 'NONE', #42443, #64778, #4461 ) ;
#14043 = EDGE_CURVE ( 'NONE', #47254, #81234, #83057, .T. ) ;
#14044 = VERTEX_POINT ( 'NONE', #67312 ) ;
#14045 = ORIENTED_EDGE ( 'NONE', *, *, #6907, .T. ) ;
#14046 = CARTESIAN_POINT ( 'NONE',  ( 198.0693404800861970, 286.9154998458281511, 16.94403134481562390 ) ) ;
#14047 = LINE ( 'NONE', #4445, #15259 ) ;
#14049 = CARTESIAN_POINT ( 'NONE',  ( 194.1852025340051284, 294.3083584634874796, -15.46421316575964688 ) ) ;
#14048 = CARTESIAN_POINT ( 'NONE',  ( 204.8762144138505903, 275.7909827032724479, 14.60855957933206817 ) ) ;
#14050 = CARTESIAN_POINT ( 'NONE',  ( 164.5696622524448287, 245.6039789247527096, -0.9250471598561700315 ) ) ;
#14051 = CARTESIAN_POINT ( 'NONE',  ( 68.96685452785939674, 69.33442928595859200, 6.693821423866975984 ) ) ;
#14052 = CARTESIAN_POINT ( 'NONE',  ( 75.29281472599660674, 60.68631827055407513, -15.54484235153014282 ) ) ;
#14053 = CARTESIAN_POINT ( 'NONE',  ( 147.6140518775699491, 274.9719575673779559, 8.457032797753797126 ) ) ;
#14054 = CARTESIAN_POINT ( 'NONE',  ( 170.1618648994021896, 287.2524135899183193, -4.625886296424732258 ) ) ;
#14055 = CARTESIAN_POINT ( 'NONE',  ( 77.21485428481166480, 62.97229237163904969, -15.28182260264458492 ) ) ;
#14056 = CARTESIAN_POINT ( 'NONE',  ( 184.3726654517722068, 285.2721521148185957, -15.05498701587415411 ) ) ;
#14057 = CARTESIAN_POINT ( 'NONE',  ( 107.1835739849013578, 238.8149278399160664, 9.188101187500093303 ) ) ;
#14058 = VERTEX_POINT ( 'NONE', #69314 ) ;
#14059 = CARTESIAN_POINT ( 'NONE',  ( 148.0905168928549074, 274.5273101863830334, -6.357871172357103973 ) ) ;
#14060 = CARTESIAN_POINT ( 'NONE',  ( 37.18115723113500337, 22.26216523072496400, -2.296566073217252530E-15 ) ) ;
#14061 = CARTESIAN_POINT ( 'NONE',  ( 191.9783149651901510, 275.2774038663249598, 16.54544651655929144 ) ) ;
#14062 = ORIENTED_EDGE ( 'NONE', *, *, #38471, .T. ) ;
#14063 = CARTESIAN_POINT ( 'NONE',  ( 163.8579349293242444, 248.3789907627131583, -9.588306200948446545 ) ) ;
#14064 = DIRECTION ( 'NONE',  ( -0.8944271909999158554, 0.000000000000000000, -0.4472135954999578722 ) ) ;
#14065 = CARTESIAN_POINT ( 'NONE',  ( 196.0034224882197975, 291.1591091234520263, 17.53794140922627776 ) ) ;
#14066 = CARTESIAN_POINT ( 'NONE',  ( 206.7893622945242385, 272.4773133715531230, -10.52881283832460291 ) ) ;
#14067 = CARTESIAN_POINT ( 'NONE',  ( 19.46394688279507079, 19.43677371833800649, -10.00000000000000355 ) ) ;
#14068 = VERTEX_POINT ( 'NONE', #76906 ) ;
#14069 = CARTESIAN_POINT ( 'NONE',  ( 148.5256826847395359, 273.3929666916147312, 8.949121270729929023 ) ) ;
#14070 = VERTEX_POINT ( 'NONE', #85049 ) ;
#14071 = EDGE_CURVE ( 'NONE', #57476, #50548, #92652, .T. ) ;
#14072 = CARTESIAN_POINT ( 'NONE',  ( 79.14312167556931854, 57.64441083166269664, 0.000000000000000000 ) ) ;
#14073 = ORIENTED_EDGE ( 'NONE', *, *, #87329, .T. ) ;
#14074 = FACE_OUTER_BOUND ( 'NONE', #37086, .T. ) ;
#14075 = DIRECTION ( 'NONE',  ( 0.5000000000000006661, -0.8660254037844383745, -3.433594394091488070E-15 ) ) ;
#14076 = CARTESIAN_POINT ( 'NONE',  ( 157.4345159935474783, 262.7946473092207498, 17.12007574691928369 ) ) ;
#14077 = CIRCLE ( 'NONE', #69021, 0.1418229129680863287 ) ;
#14078 = DIRECTION ( 'NONE',  ( 0.4999999999999992784, -0.8660254037844390407, 0.000000000000000000 ) ) ;
#14080 = CARTESIAN_POINT ( 'NONE',  ( 69.99892673467476811, 62.80419320708934094, -13.35911945385968735 ) ) ;
#14079 = CARTESIAN_POINT ( 'NONE',  ( -22.42236680055709641, 157.8615022471902591, 0.000000000000000000 ) ) ;
#14081 = CARTESIAN_POINT ( 'NONE',  ( 162.6991225460172927, 284.8212170328912975, -3.897741803361528756 ) ) ;
#14082 = ORIENTED_EDGE ( 'NONE', *, *, #49998, .F. ) ;
#14084 = CARTESIAN_POINT ( 'NONE',  ( 190.1752790837055045, 301.2537496138681945, -5.177773110520776711 ) ) ;
#14083 = AXIS2_PLACEMENT_3D ( 'NONE', #37443, #76950, #98285 ) ;
#14085 = CARTESIAN_POINT ( 'NONE',  ( 63.33450210234187239, 195.8262482093458061, 3.021315404115420679E-15 ) ) ;
#14086 = CARTESIAN_POINT ( 'NONE',  ( 3.722289961109204626, 27.08330320443191752, 177.5919119679930134 ) ) ;
#14087 = EDGE_CURVE ( 'NONE', #39984, #18565, #33629, .T. ) ;
#14088 = CARTESIAN_POINT ( 'NONE',  ( 170.1900998099124251, 249.2102026740786300, -0.2624473253846250076 ) ) ;
#14089 = CARTESIAN_POINT ( 'NONE',  ( 189.0595448167310906, 269.8736603083619912, -13.99715981437423906 ) ) ;
#14090 = CARTESIAN_POINT ( 'NONE',  ( 71.83801353683954005, 72.23051172126305630, 3.257724734605890848 ) ) ;
#14091 = CARTESIAN_POINT ( 'NONE',  ( 84.24093560737047426, 44.97564044950197371, 8.884023765932731465 ) ) ;
#14092 = CARTESIAN_POINT ( 'NONE',  ( 50.45802072044652675, 211.4860189848785410, -2.679491924311252493 ) ) ;
#14093 = AXIS2_PLACEMENT_3D ( 'NONE', #32272, #31756, #23659 ) ;
#14094 =( BOUNDED_CURVE ( )  B_SPLINE_CURVE ( 2, ( #67681, #98611, #92996, #94010, #79324, #31648, #31154, #24066, #55940, #762, #46347, #94510, #54959 ),
 .UNSPECIFIED., .F., .T. ) 
 B_SPLINE_CURVE_WITH_KNOTS ( ( 3, 2, 2, 2, 2, 2, 3 ),
 ( 0.7875000000000000888, 0.7900000000000000355, 0.7950000000000000400, 0.8000000000000000444, 0.8050000000000000488, 0.8100000000000000533, 0.8125000000000000000 ),
 .UNSPECIFIED. ) 
 CURVE ( )  GEOMETRIC_REPRESENTATION_ITEM ( )  RATIONAL_B_SPLINE_CURVE ( ( 0.9755282581475767101, 0.9755282581475772652, 1.000000000000000000, 0.9510565162951535312, 1.000000000000000000, 0.9510565162951535312, 1.000000000000000000, 0.9510565162951535312, 1.000000000000000000, 0.9510565162951535312, 1.000000000000000000, 0.9755282581475768211, 0.9755282581475768211 ) ) 
 REPRESENTATION_ITEM ( '' )  );
#14095 = CARTESIAN_POINT ( 'NONE',  ( 70.54765706325409269, 60.82528431242337064, -15.03543891230351370 ) ) ;
#14096 = CARTESIAN_POINT ( 'NONE',  ( 72.40063605961431392, 70.75631031022656714, -6.847773698889723981 ) ) ;
#14097 = CARTESIAN_POINT ( 'NONE',  ( 72.92127039979699532, 225.1589784336661637, -6.496448406907675876E-16 ) ) ;
#14098 = CARTESIAN_POINT ( 'NONE',  ( 206.2809287719926488, 273.3579460648492159, -10.70911012174624588 ) ) ;
#14099 = CARTESIAN_POINT ( 'NONE',  ( -19.65312891409030271, 93.06504152958497400, 177.5919119679930134 ) ) ;
#14100 = CARTESIAN_POINT ( 'NONE',  ( 163.4218292706009095, 247.5920839679097014, -10.44611490715852042 ) ) ;
#14101 = B_SPLINE_CURVE_WITH_KNOTS ( 'NONE', 3,
 ( #33922, #40486, #32400, #72430, #18711, #71416, #71917, #70912, #86659, #39977, #48611, #63799, #32892, #56181, #94733, #80042 ),
 .UNSPECIFIED., .F., .F.,
 ( 4, 2, 2, 2, 2, 2, 2, 4 ),
 ( 7.775354953989597285E-17, 0.0003787177898469638068, 0.0007574355796938498763, 0.001136153369540736108, 0.001514871159387622124, 0.001893588949234508139, 0.002272306739081394154, 0.003029742318775003988 ),
 .UNSPECIFIED. ) ;
#14102 = B_SPLINE_CURVE_WITH_KNOTS ( 'NONE', 3,
 ( #84920, #69178, #83430, #68179, #68676, #54454, #8390, #52984, #100108, #53477 ),
 .UNSPECIFIED., .F., .F.,
 ( 4, 2, 2, 2, 4 ),
 ( 0.000000000000000000, 0.0002622400424273382911, 0.0005244800848546765822, 0.0007867201272820148732, 0.001048960169709353164 ),
 .UNSPECIFIED. ) ;
#14103 = CARTESIAN_POINT ( 'NONE',  ( 207.1285138014047504, 271.8898857301724661, -5.752177443817618752 ) ) ;
#14104 = CARTESIAN_POINT ( 'NONE',  ( 154.6982851380984130, 273.6571292083216349, -13.42362762759460892 ) ) ;
#14105 = CIRCLE ( 'NONE', #70722, 70.00000000000001421 ) ;
#14107 = CARTESIAN_POINT ( 'NONE',  ( -20.77265562100329532, 95.16204261274404530, 45.19941863730353049 ) ) ;
#14106 = CARTESIAN_POINT ( 'NONE',  ( 73.27146650943220152, 69.63413511619549467, -9.919440617956860606 ) ) ;
#14108 = CARTESIAN_POINT ( 'NONE',  ( 50.33970617970974359, 92.06352491358971690, 177.5919119679930134 ) ) ;
#14109 = CARTESIAN_POINT ( 'NONE',  ( 68.55513178119723250, 64.39780669069259034, 11.67030924314737206 ) ) ;
#14110 = CARTESIAN_POINT ( 'NONE',  ( 82.55167669771859096, 54.18190009503562266, 15.56852171010267938 ) ) ;
#14111 = CARTESIAN_POINT ( 'NONE',  ( 72.04296851029907600, 72.03750459758265379, 2.856970073737167048 ) ) ;
#14112 = ADVANCED_FACE ( 'NONE', ( #44504 ), #14623, .F. ) ;
#14113 = CARTESIAN_POINT ( 'NONE',  ( 25.42527643493543366, 194.6744531367911293, 4.594050593750047540 ) ) ;
#14114 = AXIS2_PLACEMENT_3D ( 'NONE', #43121, #27467, #58337 ) ;
#14115 = EDGE_CURVE ( 'NONE', #8334, #96434, #98746, .T. ) ;
#14116 = CARTESIAN_POINT ( 'NONE',  ( 196.3720681610792553, 290.5205960880691691, 16.18360420724715354 ) ) ;
#14117 = CARTESIAN_POINT ( 'NONE',  ( 81.27790830334583916, 42.47193573065089822, -7.638390500584347542 ) ) ;
#14118 = CARTESIAN_POINT ( 'NONE',  ( 80.61857449287080613, 50.42422421458247328, -14.58301214530503387 ) ) ;
#14119 = CARTESIAN_POINT ( 'NONE',  ( 72.04541054607656747, 72.23942076927355060, -1.584012611844705765 ) ) ;
#14120 = CARTESIAN_POINT ( 'NONE',  ( 49.15987193134397160, 205.3149278399160949, -9.188101187500095079 ) ) ;
#14121 = CARTESIAN_POINT ( 'NONE',  ( 28.84566271970979301, 17.44966523072495335, -2.296566073217252530E-15 ) ) ;
#14122 = CARTESIAN_POINT ( 'NONE',  ( 171.4108310039837875, 286.6584375100259763, 7.439453781534334453 ) ) ;
#14123 = CARTESIAN_POINT ( 'NONE',  ( 197.0313051377892748, 289.3787641501790517, -17.15509075150697882 ) ) ;
#14124 = CARTESIAN_POINT ( 'NONE',  ( 45.26690985970349601, 25.94473085651396005, 1.475505719884397138E-15 ) ) ;
#14125 = DIRECTION ( 'NONE',  ( -0.6444573283588950208, 0.7646402761590023189, 0.000000000000000000 ) ) ;
#14126 = CARTESIAN_POINT ( 'NONE',  ( 182.0814719340378645, 255.7199348603173519, -3.369638453849108206 ) ) ;
#14127 = CARTESIAN_POINT ( 'NONE',  ( 175.8186258879950685, 291.0967586842824630, 2.548988351986237522 ) ) ;
#14128 = CARTESIAN_POINT ( 'NONE',  ( 176.1090663942078436, 274.8498405251406780, 17.00816766817632342 ) ) ;
#14129 = CARTESIAN_POINT ( 'NONE',  ( -66.69146994933839778, 41.22495595238228105, 177.5919119679930134 ) ) ;
#14130 = CARTESIAN_POINT ( 'NONE',  ( 11.80767242186427879, 30.53330575246453904, -10.00000000000000000 ) ) ;
#14131 = CARTESIAN_POINT ( 'NONE',  ( 44.95821123098110661, 116.5722627105190270, -10.00000000000000000 ) ) ;
#14132 = CARTESIAN_POINT ( 'NONE',  ( 96.15094473426229627, 232.9865022471902876, 10.00000000000009237 ) ) ;
#14133 = CARTESIAN_POINT ( 'NONE',  ( 200.2631011806900005, 283.7811292041749311, 18.23377125296567058 ) ) ;
#14134 = CARTESIAN_POINT ( 'NONE',  ( 165.2613035890315132, 269.7019032284875379, -16.28361342814668689 ) ) ;
#14135 = ORIENTED_EDGE ( 'NONE', *, *, #6838, .F. ) ;
#14136 = CARTESIAN_POINT ( 'NONE',  ( 68.13167480270307408, 200.9548013555409796, -4.594050593750042211 ) ) ;
#14137 = ORIENTED_EDGE ( 'NONE', *, *, #66124, .F. ) ;
#14138 = CARTESIAN_POINT ( 'NONE',  ( 166.0424944338363105, 265.3088416721781755, 16.55799481498140224 ) ) ;
#14139 = CARTESIAN_POINT ( 'NONE',  ( 161.9111943820872170, 250.8713438377554326, 12.61905948367559027 ) ) ;
#14140 = DIRECTION ( 'NONE',  ( -0.9646071681523451513, 0.2636911283094546254, 0.000000000000000000 ) ) ;
#14141 = ORIENTED_EDGE ( 'NONE', *, *, #55410, .F. ) ;
#14142 = CARTESIAN_POINT ( 'NONE',  ( 174.0424481033923314, 287.4814580433055653, 10.99910921803667208 ) ) ;
#14143 = CARTESIAN_POINT ( 'NONE',  ( 79.15998105033318666, 45.86243901705208259, -13.09633689766342890 ) ) ;
#14144 = CARTESIAN_POINT ( 'NONE',  ( 178.6782777294722848, 260.6412425082613709, 13.57969907341511551 ) ) ;
#14145 = CARTESIAN_POINT ( 'NONE',  ( 84.00344187778067351, 41.31840900968617802, 1.163504541493592948 ) ) ;
#14146 = CARTESIAN_POINT ( 'NONE',  ( -0.2492734796364602656, 27.10516647459198225, -10.00000000000000000 ) ) ;
#14147 = VECTOR ( 'NONE', #8389, 1000.000000000000000 ) ;
#14148 = CARTESIAN_POINT ( 'NONE',  ( 157.4729130248890954, 257.8959091554543761, 17.83439074639795052 ) ) ;
#14149 = ORIENTED_EDGE ( 'NONE', *, *, #90732, .T. ) ;
#14150 = AXIS2_PLACEMENT_3D ( 'NONE', #66125, #43310, #89484 ) ;
#14151 = CARTESIAN_POINT ( 'NONE',  ( 23.96105869301208813, 16.76004757982089899, 5.678558825948272215 ) ) ;
#14152 = CARTESIAN_POINT ( 'NONE',  ( 175.3483744890668277, 254.4581768569554185, 7.871548991938851714 ) ) ;
#14153 = CARTESIAN_POINT ( 'NONE',  ( 170.3198432486256024, 250.1987702182942996, -6.980229573997380754 ) ) ;
#14154 = ORIENTED_EDGE ( 'NONE', *, *, #3400, .F. ) ;
#14156 = ADVANCED_FACE ( 'NONE', ( #84559 ), #33210, .F. ) ;
#14155 = CARTESIAN_POINT ( 'NONE',  ( 183.8570876466514790, 294.7988146780254510, 8.885945338395226045 ) ) ;
#14157 = CARTESIAN_POINT ( 'NONE',  ( 206.3454060440500086, 273.2462681537123785, -9.268083217908118954 ) ) ;
#14158 = EDGE_CURVE ( 'NONE', #79592, #9076, #32569, .T. ) ;
#14159 = ORIENTED_EDGE ( 'NONE', *, *, #88749, .T. ) ;
#14160 = EDGE_LOOP ( 'NONE', ( #30952, #7186, #92331, #79641 ) ) ;
#14161 = AXIS2_PLACEMENT_3D ( 'NONE', #36632, #97481, #74177 ) ;
#14163 = CARTESIAN_POINT ( 'NONE',  ( -22.42236680055709641, 157.8615022471902591, 0.000000000000000000 ) ) ;
#14162 = CARTESIAN_POINT ( 'NONE',  ( 73.02433024948126672, 69.66517378990661769, 9.714162469163332148 ) ) ;
#14164 = CARTESIAN_POINT ( 'NONE',  ( 67.41069134358542669, 70.04696837240071261, -4.305487806446024446E-08 ) ) ;
#14165 = CARTESIAN_POINT ( 'NONE',  ( 204.8189571845487080, 275.8901551335242175, 13.43702398685204358 ) ) ;
#14166 = EDGE_CURVE ( 'NONE', #39829, #41328, #79957, .T. ) ;
#14167 = CARTESIAN_POINT ( 'NONE',  ( 198.6755293322981117, 286.5308843062557571, 17.86676876308990103 ) ) ;
#14168 = CARTESIAN_POINT ( 'NONE',  ( -4.027391858960333693, 36.50819422017340088, 59.99999999999999289 ) ) ;
#14169 = DIRECTION ( 'NONE',  ( 0.4999999999999992784, -0.8660254037844390407, 0.000000000000000000 ) ) ;
#14170 = EDGE_CURVE ( 'NONE', #93753, #14510, #91813, .T. ) ;
#14171 = CARTESIAN_POINT ( 'NONE',  ( 134.5180214354952284, 236.2202760586659736, -5.415160957724236172E-17 ) ) ;
#14172 = CARTESIAN_POINT ( 'NONE',  ( 159.8882960419693120, 255.1631675222682532, -16.13735980308360496 ) ) ;
#14173 = CARTESIAN_POINT ( 'NONE',  ( 180.0191955535601949, 258.0046308849226762, 10.27888219584907858 ) ) ;
#14174 = CARTESIAN_POINT ( 'NONE',  ( 64.07166007881600933, 216.9869531367911293, 4.594050593750046652 ) ) ;
#14175 = VERTEX_POINT ( 'NONE', #12025 ) ;
#14176 = CARTESIAN_POINT ( 'NONE',  ( 170.2148871637432705, 264.0733095026099022, 16.11244079653449646 ) ) ;
#14177 = CARTESIAN_POINT ( 'NONE',  ( 165.5046005952566475, 282.3973782299070763, -11.17475345190591973 ) ) ;
#14178 = ORIENTED_EDGE ( 'NONE', *, *, #41565, .F. ) ;
#14179 = AXIS2_PLACEMENT_3D ( 'NONE', #80388, #25652, #10447 ) ;
#14180 = CARTESIAN_POINT ( 'NONE',  ( -19.79069005721430230, 93.09954762390393057, 59.99999999999999289 ) ) ;
#14181 = ORIENTED_EDGE ( 'NONE', *, *, #34705, .T. ) ;
#14182 = B_SPLINE_CURVE_WITH_KNOTS ( 'NONE', 3,
 ( #64774, #17156, #11084, #10573, #64262, #48054, #40447, #41448, #26766, #86129, #1970, #16659, #2999, #33888, #47553, #9067, #70873, #63261, #94202, #24757, #58637, #4973, #90097, #51554, #20666, #36848, #65748, #52055, #98681, #13571, #5462 ),
 .UNSPECIFIED., .F., .F.,
 ( 4, 3, 3, 3, 3, 3, 3, 3, 3, 3, 4 ),
 ( 0.000000000000000000, 0.1333490885032346807, 0.3007194338854402571, 0.4699862290245250818, 0.5844252810809306142, 0.6686540514502837818, 0.7354980260655518132, 0.8028463152565542549, 0.8633854507757066088, 0.9437142632667097075, 1.000000000000000000 ),
 .UNSPECIFIED. ) ;
#14183 = ORIENTED_EDGE ( 'NONE', *, *, #18080, .T. ) ;
#14184 = FACE_BOUND ( 'NONE', #24149, .T. ) ;
#14185 = CARTESIAN_POINT ( 'NONE',  ( 66.45490466085416870, 67.84821477620812402, 6.733515886304859421 ) ) ;
#14186 = CARTESIAN_POINT ( 'NONE',  ( 194.2232752567778675, 284.7421936660649067, 17.38045846422785345 ) ) ;
#14187 = CARTESIAN_POINT ( 'NONE',  ( -32.32883188359665638, 96.08671883726218255, 11.63744038197175534 ) ) ;
#14188 = CARTESIAN_POINT ( 'NONE',  ( 81.40581815559377787, 55.82057330830384956, 16.38440887150438385 ) ) ;
#14189 = CARTESIAN_POINT ( 'NONE',  ( 155.0929244053699847, 262.0181703658971628, 18.51426604808664678 ) ) ;
#14190 = CARTESIAN_POINT ( 'NONE',  ( 71.50375327671149250, 66.90100933989515397, 11.02690240348687212 ) ) ;
#14191 = ORIENTED_EDGE ( 'NONE', *, *, #61393, .F. ) ;
#14192 = AXIS2_PLACEMENT_3D ( 'NONE', #53938, #77780, #79317 ) ;
#14193 = CARTESIAN_POINT ( 'NONE',  ( -32.94356256989595977, 94.88921800892812541, 36.50000000000000000 ) ) ;
#14194 = CARTESIAN_POINT ( 'NONE',  ( 201.1075649649426111, 282.3184750246975909, -17.62722514768381998 ) ) ;
#14195 = ORIENTED_EDGE ( 'NONE', *, *, #83693, .T. ) ;
#14196 = CARTESIAN_POINT ( 'NONE',  ( 163.8938939028770392, 260.7256311026002891, -16.27231015239807732 ) ) ;
#14197 = CARTESIAN_POINT ( 'NONE',  ( 174.5211454378950009, 254.1122819737915393, -7.432909296658919196 ) ) ;
#14198 = CARTESIAN_POINT ( 'NONE',  ( 191.0504085702373800, 299.7379808799933016, 6.468263574011999140 ) ) ;
#14199 = CARTESIAN_POINT ( 'NONE',  ( 164.7462163020046262, 245.2981783406326599, 1.451255823150352064 ) ) ;
#14200 = CARTESIAN_POINT ( 'NONE',  ( 36.44700672854521883, 203.3967562850347122, 1.101618078115930403E-13 ) ) ;
#14201 = DIRECTION ( 'NONE',  ( -0.000000000000000000, -0.000000000000000000, -1.000000000000000000 ) ) ;
#14202 = CARTESIAN_POINT ( 'NONE',  ( 137.6570164284488271, 250.2833772461660544, -9.188101187500095079 ) ) ;
#14203 = VERTEX_POINT ( 'NONE', #80970 ) ;
#14204 = CARTESIAN_POINT ( 'NONE',  ( 185.1790142135946837, 260.5378326486920741, -9.806357480331048038 ) ) ;
#14205 = CARTESIAN_POINT ( 'NONE',  ( 182.2071301927472575, 257.5162533253280230, 6.694102600255701141 ) ) ;
#14206 = CARTESIAN_POINT ( 'NONE',  ( 84.99999999999998579, 14.99999999999999467, 59.99999999999999289 ) ) ;
#14207 = CARTESIAN_POINT ( 'NONE',  ( 73.06720963123042623, 70.70023934857047720, 7.647115370324644168 ) ) ;
#14208 = CARTESIAN_POINT ( 'NONE',  ( 69.98405410183003994, 67.38768254928731949, -9.599236973523137095 ) ) ;
#14209 = ORIENTED_EDGE ( 'NONE', *, *, #76401, .T. ) ;
#14210 = CARTESIAN_POINT ( 'NONE',  ( 199.6670208576438768, 266.3510233136422016, 4.737243403722396273 ) ) ;
#14211 = CARTESIAN_POINT ( 'NONE',  ( 72.46615884746773872, 71.21309588215865460, -6.079728238972058385 ) ) ;
#14212 = AXIS2_PLACEMENT_3D ( 'NONE', #87221, #63839, #39512 ) ;
#14213 = CARTESIAN_POINT ( 'NONE',  ( 80.92950541471338965, 51.12517857173720159, 14.80259026963665470 ) ) ;
#14214 = CARTESIAN_POINT ( 'NONE',  ( 73.59632604377750908, 69.25558887711068223, -10.00338666068682691 ) ) ;
#14215 = CARTESIAN_POINT ( 'NONE',  ( 198.2014190056785310, 266.0765624434006327, 0.8202294858332698224 ) ) ;
#14216 = CARTESIAN_POINT ( 'NONE',  ( -80.27490717900100492, 58.06504152958491005, 177.5919119679930134 ) ) ;
#14217 = B_SPLINE_CURVE_WITH_KNOTS ( 'NONE', 3,
 ( #25718, #33300, #66569, #97495, #44250, #89906, #87584, #18109, #90421, #20994 ),
 .UNSPECIFIED., .F., .F.,
 ( 4, 2, 2, 2, 4 ),
 ( 0.000000000000000000, 0.2500000000000000000, 0.5000000000000000000, 0.7500000000000000000, 1.000000000000000000 ),
 .UNSPECIFIED. ) ;
#14218 = CARTESIAN_POINT ( 'NONE',  ( 70.77025480411006697, 71.48656028203394897, 1.095472859252403897 ) ) ;
#14219 =( REPRESENTATION_RELATIONSHIP ('NONE','NONE', #67038, #78010 ) REPRESENTATION_RELATIONSHIP_WITH_TRANSFORMATION ( #8157 )SHAPE_REPRESENTATION_RELATIONSHIP( ) );
#14221 = EDGE_CURVE ( 'NONE', #42087, #98884, #54908, .T. ) ;
#14220 = AXIS2_PLACEMENT_3D ( 'NONE', #10114, #63809, #48620 ) ;
#14222 = AXIS2_PLACEMENT_3D ( 'NONE', #49042, #79976, #41419 ) ;
#14223 = CARTESIAN_POINT ( 'NONE',  ( 207.6628070930962906, 270.9644626028195376, 7.378217122120054761 ) ) ;
#14224 = CARTESIAN_POINT ( 'NONE',  ( 167.2515702596184042, 262.0622343731731689, -17.21809106051008342 ) ) ;
#14225 = B_SPLINE_SURFACE_WITH_KNOTS ( 'NONE', 3, 1, ( 
 ( #14554, #59629 ),
 ( #45429, #92100 ),
 ( #5948, #98171 ),
 ( #21651, #67750 ),
 ( #30747, #30242 ),
 ( #22645, #15023 ),
 ( #98674, #38324 ),
 ( #45914, #52534 ),
 ( #7431, #100161 ),
 ( #83484, #43933 ),
 ( #74872, #14050 ),
 ( #44928, #31712 ),
 ( #24139, #25128 ),
 ( #17027, #94078 ),
 ( #84971, #56010 ),
 ( #46418, #55024 ),
 ( #63133, #16531 ),
 ( #15516, #1346 ),
 ( #87006, #38823 ),
 ( #8937, #46936 ),
 ( #62113, #79387 ),
 ( #24631, #95087 ),
 ( #62617, #86005 ),
 ( #70735, #2354 ),
 ( #16035, #94572 ),
 ( #39803, #32232 ),
 ( #47428, #33233 ),
 ( #70227, #8441 ),
 ( #93570, #64137 ),
 ( #55511, #78355 ),
 ( #86499, #47920 ),
 ( #31227, #63635 ),
 ( #17533, #78859 ),
 ( #7950, #25650 ) ),
 .UNSPECIFIED., .T., .F., .F.,
 ( 4, 2, 2, 2, 2, 2, 2, 2, 2, 2, 2, 2, 2, 2, 2, 2, 4 ),
 ( 2, 2 ),
 ( 0.000000000000000000, 0.06250000000000000000, 0.1250000000000000000, 0.1875000000000000000, 0.2500000000000000000, 0.3125000000000000000, 0.3750000000000000000, 0.4375000000000000000, 0.5000000000000000000, 0.5625000000000000000, 0.6250000000000000000, 0.6875000000000000000, 0.7500000000000000000, 0.8125000000000000000, 0.8750000000000000000, 0.9375000000000000000, 1.000000000000000000 ),
 ( 0.000000000000000000, 1.000000000000000000 ),
 .UNSPECIFIED. ) ;
#14226 = CARTESIAN_POINT ( 'NONE',  ( 20.44744908501035852, 27.50829794293881037, -10.00000000000000355 ) ) ;
#14227 = DIRECTION ( 'NONE',  ( 0.8660254037844399289, 0.4999999999999977240, -0.000000000000000000 ) ) ;
#14228 = CARTESIAN_POINT ( 'NONE',  ( 204.9751544352041890, 274.4268820053481477, 11.86595640911393268 ) ) ;
#14229 = DIRECTION ( 'NONE',  ( -0.000000000000000000, -0.000000000000000000, -1.000000000000000000 ) ) ;
#14230 = CARTESIAN_POINT ( 'NONE',  ( 159.7608930362198407, 253.9330115291272421, 15.38895778945778581 ) ) ;
#14231 = CARTESIAN_POINT ( 'NONE',  ( 72.30698315258602804, 72.02217937971185791, -3.539662339715687889 ) ) ;
#14232 = CARTESIAN_POINT ( 'NONE',  ( 139.7950166422676261, 261.5177522451418781, 5.000000000000046185 ) ) ;
#14233 = CARTESIAN_POINT ( 'NONE',  ( 182.5998193346738390, 278.6774981096693864, 17.57078003122366283 ) ) ;
#14234 = VERTEX_POINT ( 'NONE', #3916 ) ;
#14235 = CIRCLE ( 'NONE', #20687, 70.00000000000001421 ) ;
#14236 = CARTESIAN_POINT ( 'NONE',  ( 178.0923676029798344, 255.8199948319143573, 8.866499536866403020 ) ) ;
#14237 = CARTESIAN_POINT ( 'NONE',  ( 72.78592982716214976, 70.27025758361958196, -8.090204238294326444 ) ) ;
#14238 = CARTESIAN_POINT ( 'NONE',  ( 150.7850480413316632, 269.4796311011364764, -14.43114374163211089 ) ) ;
#14239 = CARTESIAN_POINT ( 'NONE',  ( 3.882894515797516988, 182.2369531367911009, -4.594050593750048428 ) ) ;
#14240 = CARTESIAN_POINT ( 'NONE',  ( 31.96529204653334588, 20.58380873178789017, 6.180339887498953466 ) ) ;
#14241 = CARTESIAN_POINT ( 'NONE',  ( 85.12553491092469926, 49.00280835124235779, 12.44658997562346769 ) ) ;
#14242 = CARTESIAN_POINT ( 'NONE',  ( 157.7593757092099906, 257.3997412317380054, -18.08445832352326121 ) ) ;
#14243 = CARTESIAN_POINT ( 'NONE',  ( 72.06167755366938366, 71.78506459024572450, -3.928121392008132151 ) ) ;
#14244 = CARTESIAN_POINT ( 'NONE',  ( 122.1835217032046330, 252.8967562850346553, -4.648177544792955347E-16 ) ) ;
#14245 = B_SPLINE_SURFACE_WITH_KNOTS ( 'NONE', 3, 1, ( 
 ( #21295, #59254 ),
 ( #58765, #29389 ),
 ( #59769, #52169 ),
 ( #98302, #67886 ),
 ( #5580, #28892 ),
 ( #6081, #66387 ),
 ( #5092, #97316 ),
 ( #35973, #20802 ),
 ( #89735, #51695 ),
 ( #43060, #76012 ),
 ( #74003, #4589 ),
 ( #66875, #36974 ),
 ( #20297, #83118 ),
 ( #6590, #44561 ),
 ( #60258, #21777 ),
 ( #52666, #83621 ),
 ( #14188, #37463 ),
 ( #78494, #92232 ),
 ( #15157, #85631 ),
 ( #39448, #479 ),
 ( #93206, #99790 ),
 ( #23762, #93718 ),
 ( #39950, #16176 ),
 ( #38960, #32374 ),
 ( #84616, #91715 ),
 ( #1491, #85112 ),
 ( #30379, #86142 ),
 ( #61262, #7572 ),
 ( #22783, #24279 ),
 ( #53660, #100293 ),
 ( #70369, #76493 ) ),
 .UNSPECIFIED., .F., .F., .F.,
 ( 4, 3, 3, 3, 3, 3, 3, 3, 3, 3, 4 ),
 ( 2, 2 ),
 ( 0.000000000000000000, 0.1333490885032341255, 0.3007194338854348725, 0.4699862290245032659, 0.5844252810809253962, 0.6686540514502775645, 0.7354980260655532565, 0.8028463152565672445, 0.8633854507757174890, 0.9437142632667334663, 1.000000000000000000 ),
 ( 0.000000000000000000, 1.000000000000000000 ),
 .UNSPECIFIED. ) ;
#14246 = DIRECTION ( 'NONE',  ( -0.5000000000000002220, 0.8660254037844384856, 0.000000000000000000 ) ) ;
#14247 = CARTESIAN_POINT ( 'NONE',  ( 151.0438343122359584, 269.0314001316289705, 14.41873139571475626 ) ) ;
#14248 = CARTESIAN_POINT ( 'NONE',  ( 43.46773267070889091, 209.2365022471903444, 2.944929066748280225E-16 ) ) ;
#14249 = DIRECTION ( 'NONE',  ( 0.7845058662179964504, 0.6201213960746324583, 0.000000000000000000 ) ) ;
#14250 = AXIS2_PLACEMENT_3D ( 'NONE', #39295, #77329, #7936 ) ;
#14251 = CARTESIAN_POINT ( 'NONE',  ( 190.5154909595809727, 300.6644853595138329, -0.04129855346138300298 ) ) ;
#14252 = CARTESIAN_POINT ( 'NONE',  ( 5.371288904610766579, 186.1589784336661637, -6.496448406907675876E-16 ) ) ;
#14253 = CARTESIAN_POINT ( 'NONE',  ( 71.24258803893445702, 70.28559471200580333, -7.340107459681124880 ) ) ;
#14254 = CARTESIAN_POINT ( 'NONE',  ( 192.7693357657653053, 296.7607116428271183, 12.22606306887835714 ) ) ;
#14255 = CARTESIAN_POINT ( 'NONE',  ( 36.29711636232130445, 39.14336893147758900, 7.433330006724141015 ) ) ;
#14256 = CARTESIAN_POINT ( 'NONE',  ( 142.4652616372697480, 246.3927522451418497, 10.00000000000009948 ) ) ;
#14257 = CARTESIAN_POINT ( 'NONE',  ( 207.3502731283117555, 271.5057873089173768, 6.280625384230454245 ) ) ;
#14258 = CARTESIAN_POINT ( 'NONE',  ( 189.1359039112073503, 268.2262726479567618, 13.76342687570769030 ) ) ;
#14259 = CARTESIAN_POINT ( 'NONE',  ( 164.1724755390579276, 281.5534210847879422, 9.615559972177582182 ) ) ;
#14260 = CARTESIAN_POINT ( 'NONE',  ( 21.59269996301512862, 13.26216523072493914, -2.296566073217252530E-15 ) ) ;
#14261 = CARTESIAN_POINT ( 'NONE',  ( 14.99119413235835729, 10.78380873178785571, -6.180339887498949025 ) ) ;
#14262 = CARTESIAN_POINT ( 'NONE',  ( 71.49559693922878978, 59.13754170620860862, 15.79921231626542699 ) ) ;
#14263 = CARTESIAN_POINT ( 'NONE',  ( 193.9204722154232741, 294.7668848255750049, 15.43855698596013859 ) ) ;
#14264 = ORIENTED_EDGE ( 'NONE', *, *, #13845, .T. ) ;
#14265 = CARTESIAN_POINT ( 'NONE',  ( 181.5930883117324868, 289.4714290587421033, 12.79629105351733109 ) ) ;
#14266 = PLANE ( 'NONE',  #74472 ) ;
#14267 = CARTESIAN_POINT ( 'NONE',  ( 88.00349997577261263, 44.64923112938744509, 4.253506518527974123 ) ) ;
#14268 = CARTESIAN_POINT ( 'NONE',  ( 81.60392558426443088, 42.57997742557506626, 7.507547604040053280 ) ) ;
#14269 = ORIENTED_EDGE ( 'NONE', *, *, #26875, .T. ) ;
#14270 = CARTESIAN_POINT ( 'NONE',  ( 57.60966550219794158, 179.2419560658248940, 18.47570218321542868 ) ) ;
#14271 = CARTESIAN_POINT ( 'NONE',  ( 82.32225094544060084, 40.36431351492650776, 1.323353720485960672 ) ) ;
#14272 = CARTESIAN_POINT ( 'NONE',  ( 76.95450487289042485, 63.82793267849404373, 14.93104742799489593 ) ) ;
#14273 = CARTESIAN_POINT ( 'NONE',  ( 155.0453531195792038, 262.1005662498678817, -18.46987289964740953 ) ) ;
#14274 = ORIENTED_EDGE ( 'NONE', *, *, #92811, .F. ) ;
#14275 = VERTEX_POINT ( 'NONE', #2949 ) ;
#14277 = CARTESIAN_POINT ( 'NONE',  ( 151.8574524980327567, 274.5526676221680873, 11.13270052181353975 ) ) ;
#14276 = CARTESIAN_POINT ( 'NONE',  ( 202.4683350698883544, 279.2420349807568414, 15.54043181306517774 ) ) ;
#14278 = ORIENTED_EDGE ( 'NONE', *, *, #73528, .T. ) ;
#14279 = CARTESIAN_POINT ( 'NONE',  ( 201.2139346379346705, 282.1342373466909521, -16.65315141107179286 ) ) ;
#14280 = VECTOR ( 'NONE', #62560, 1000.000000000000000 ) ;
#14281 = CARTESIAN_POINT ( 'NONE',  ( 71.74963559588888984, 69.27730147043639874, 9.283338642638904403 ) ) ;
#14282 = CARTESIAN_POINT ( 'NONE',  ( -86.81108781737714253, 15.00000000000000000, 0.000000000000000000 ) ) ;
#14283 = CARTESIAN_POINT ( 'NONE',  ( 45.37789370152431445, 208.5530062829863027, -4.648177544792955347E-16 ) ) ;
#14284 = B_SPLINE_CURVE_WITH_KNOTS ( 'NONE', 3,
 ( #48246, #79191, #18356, #55812, #3175, #9767, #57828, #24936, #17861, #25962, #42130, #49249, #34060, #19373, #71563, #3658, #26455, #2659, #1665, #56331, #87327, #33551, #40627, #96379, #81187, #63940, #48759, #32548, #72058, #64951, #79691, #10253, #95405, #95895, #49740, #10753, #41629, #26943, #80693, #63447, #72571, #73062, #57330, #88303, #94382, #18858 ),
 .UNSPECIFIED., .F., .F.,
 ( 4, 1, 1, 1, 2, 2, 1, 1, 1, 2, 2, 1, 1, 2, 2, 1, 1, 2, 2, 1, 1, 2, 2, 1, 2, 2, 1, 2, 2, 4 ),
 ( 0.000000000000000000, 0.06250000000002038647, 0.09375000000003029521, 0.1093750000000349165, 0.1171875000000369843, 0.1250000000000390521, 0.1875000000000338896, 0.2187500000000316136, 0.2343750000000324463, 0.2421875000000331679, 0.2500000000000338618, 0.3125000000000286438, 0.3437500000000238698, 0.3593750000000215383, 0.3750000000000191513, 0.4375000000000183187, 0.4687500000000181521, 0.4843750000000158762, 0.5000000000000135447, 0.5625000000000096589, 0.5937500000000056621, 0.6093750000000056621, 0.6250000000000056621, 0.6875000000000015543, 0.7187499999999994449, 0.7499999999999972244, 0.8124999999999938938, 0.8437499999999943379, 0.8749999999999947820, 1.000000000000000000 ),
 .UNSPECIFIED. ) ;
#14285 = ORIENTED_EDGE ( 'NONE', *, *, #83999, .F. ) ;
#14287 = ADVANCED_FACE ( 'NONE', ( #10525 ), #4409, .T. ) ;
#14286 = CARTESIAN_POINT ( 'NONE',  ( 87.60166352820709790, 45.45111633860030054, -6.741156191458166802 ) ) ;
#14288 = CIRCLE ( 'NONE', #4837, 70.00000000000001421 ) ;
#14289 = CARTESIAN_POINT ( 'NONE',  ( 149.4171629335945681, 271.8488776066536730, -11.42564036194071520 ) ) ;
#14290 = AXIS2_PLACEMENT_3D ( 'NONE', #24390, #29986, #83734 ) ;
#14291 = EDGE_LOOP ( 'NONE', ( #1446, #34230, #47266, #22383 ) ) ;
#14292 = CARTESIAN_POINT ( 'NONE',  ( 164.9356397357043704, 244.9700873293209042, 2.799217332519396972 ) ) ;
#14293 = VECTOR ( 'NONE', #90853, 1000.000000000000000 ) ;
#14294 = CARTESIAN_POINT ( 'NONE',  ( 53.17212233558426959, 213.0530062829863311, -4.648177544792955347E-16 ) ) ;
#14295 = VERTEX_POINT ( 'NONE', #97156 ) ;
#14296 = CARTESIAN_POINT ( 'NONE',  ( 149.6877696051026305, 271.3801731027346591, 11.89134584187677390 ) ) ;
#14297 = DIRECTION ( 'NONE',  ( 0.000000000000000000, -0.000000000000000000, 1.000000000000000000 ) ) ;
#14298 = VERTEX_POINT ( 'NONE', #11034 ) ;
#14299 = CARTESIAN_POINT ( 'NONE',  ( -18.14236540235112116, 78.33508314200840061, 13.72324207012383468 ) ) ;
#14300 = DIRECTION ( 'NONE',  ( -0.000000000000000000, -0.000000000000000000, 1.000000000000000000 ) ) ;
#14301 = CARTESIAN_POINT ( 'NONE',  ( 83.61215227093727265, 52.34510252200112035, 14.76249278255550657 ) ) ;
#14302 = VERTEX_POINT ( 'NONE', #3438 ) ;
#14303 = ORIENTED_EDGE ( 'NONE', *, *, #33636, .T. ) ;
#14304 = AXIS2_PLACEMENT_3D ( 'NONE', #83231, #7691, #67996 ) ;
#14305 = CARTESIAN_POINT ( 'NONE',  ( 156.0580231375089681, 266.2288738017929290, -16.26249046113716545 ) ) ;
#14306 = DIRECTION ( 'NONE',  ( -1.000000000000000000, 0.000000000000000000, 0.000000000000000000 ) ) ;
#14307 = CARTESIAN_POINT ( 'NONE',  ( 148.3519871123208986, 273.6938162480936398, 8.180046468253793890 ) ) ;
#14308 = CARTESIAN_POINT ( 'NONE',  ( 190.6893905452545823, 300.3632824417117604, 3.294993852933539191 ) ) ;
#14309 = CARTESIAN_POINT ( 'NONE',  ( 152.8522706834672533, 265.8990964544007056, 17.63080661522264947 ) ) ;
#14310 = CARTESIAN_POINT ( 'NONE',  ( 191.1855251068263328, 299.5039521736787265, 8.464810282331489688 ) ) ;
#14311 = CARTESIAN_POINT ( 'NONE',  ( 191.3610003135137276, 299.2000202002271294, -9.855749861282104618 ) ) ;
#14312 = CIRCLE ( 'NONE', #73979, 70.00000000000001421 ) ;
#14313 = CARTESIAN_POINT ( 'NONE',  ( 163.5175435169129798, 257.7444940288048087, 15.51854699187649089 ) ) ;
#14314 = CARTESIAN_POINT ( 'NONE',  ( -19.24216595772339744, 41.33483386289255890, 59.99999999999999289 ) ) ;
#14315 = CARTESIAN_POINT ( 'NONE',  ( 96.22311351791105949, 216.3615022471902023, 5.000000000000051514 ) ) ;
#14316 = CARTESIAN_POINT ( 'NONE',  ( 66.97123670830937670, 67.01180370489193194, 8.614194428613410892 ) ) ;
#14317 = CARTESIAN_POINT ( 'NONE',  ( 170.3267854104257992, 288.9614774289731827, 4.405198534815358613 ) ) ;
#14318 = CARTESIAN_POINT ( 'NONE',  ( 178.2382707639212356, 285.7843550335422833, 14.43266090959460435 ) ) ;
#14319 = CARTESIAN_POINT ( 'NONE',  ( 98.84807947347611901, 234.0024278399160664, -9.188101187500093303 ) ) ;
#14320 = ORIENTED_EDGE ( 'NONE', *, *, #66712, .F. ) ;
#14321 = CARTESIAN_POINT ( 'NONE',  ( 190.0509677963674164, 301.4690630794920594, -3.786306570772668412 ) ) ;
#14322 = CARTESIAN_POINT ( 'NONE',  ( 72.15493168869993212, 69.90749124128198844, 8.044790318638545656 ) ) ;
#14323 = LINE ( 'NONE', #22418, #52825 ) ;
#14324 = CARTESIAN_POINT ( 'NONE',  ( 35.10516808903320651, 74.11552124184515833, 59.99999999999999289 ) ) ;
#14325 = CARTESIAN_POINT ( 'NONE',  ( 191.6458595453738099, 297.4183736063205288, -10.67255559255732855 ) ) ;
#14326 = CARTESIAN_POINT ( 'NONE',  ( 190.3911359119452413, 288.4005044049387720, 16.54395277729882707 ) ) ;
#14327 = CARTESIAN_POINT ( 'NONE',  ( 69.54903494467576763, 65.01932103406771546, -11.65098723592027063 ) ) ;
#14328 = VERTEX_POINT ( 'NONE', #27722 ) ;
#14329 = CARTESIAN_POINT ( 'NONE',  ( 167.8408648507877956, 253.6332239154487240, -11.89335889730976348 ) ) ;
#14330 = CARTESIAN_POINT ( 'NONE',  ( 159.2122473525774069, 254.8832937285494609, -16.22689353966294590 ) ) ;
#14331 = VECTOR ( 'NONE', #95400, 1000.000000000000000 ) ;
#14332 = FACE_OUTER_BOUND ( 'NONE', #92038, .T. ) ;
#14333 = CARTESIAN_POINT ( 'NONE',  ( 49.65620586503739986, 186.1427522451417644, 1.119607411625061291E-15 ) ) ;
#14334 = CARTESIAN_POINT ( 'NONE',  ( 116.0067284296028589, 225.5327760586659451, 1.948934522072302763E-15 ) ) ;
#14335 = CARTESIAN_POINT ( 'NONE',  ( -28.50628834134440126, 40.78531227041054308, 59.99999999999999289 ) ) ;
#14336 = CARTESIAN_POINT ( 'NONE',  ( 11.61660434717087043, 51.85354971528389001, 59.99999999999999289 ) ) ;
#14337 = CARTESIAN_POINT ( 'NONE',  ( 157.0848929289108469, 258.5679796760466047, 17.57466231005294688 ) ) ;
#14338 = CARTESIAN_POINT ( 'NONE',  ( 172.2319936421038449, 250.7099816150368383, -4.070406209060837277 ) ) ;
#14339 = CARTESIAN_POINT ( 'NONE',  ( 34.43744006700849525, 196.8149278399160664, 9.188101187500093303 ) ) ;
#14341 = EDGE_CURVE ( 'NONE', #43956, #4734, #43953, .T. ) ;
#14340 = AXIS2_PLACEMENT_3D ( 'NONE', #98095, #81925, #21582 ) ;
#14342 = DIRECTION ( 'NONE',  ( 0.3074612162317589825, -0.9515606131578205895, 0.000000000000000000 ) ) ;
#14343 = ORIENTED_EDGE ( 'NONE', *, *, #80742, .T. ) ;
#14344 = CARTESIAN_POINT ( 'NONE',  ( 201.5036534377215958, 270.3153034880852488, -10.25451236307256409 ) ) ;
#14345 = CARTESIAN_POINT ( 'NONE',  ( 181.8197068046096661, 267.0272984663218949, 15.22864918630029329 ) ) ;
#14346 = CARTESIAN_POINT ( 'NONE',  ( 32.07315653955450330, 47.77038272570916888, 10.00000000000000000 ) ) ;
#14347 = CARTESIAN_POINT ( 'NONE',  ( 147.0538900202505488, 275.9421863647172017, 5.192507380313251986 ) ) ;
#14348 = CARTESIAN_POINT ( 'NONE',  ( 81.76046516772940720, 41.68411953923578039, -5.589761987555794676 ) ) ;
#14349 = EDGE_CURVE ( 'NONE', #38681, #75209, #91047, .T. ) ;
#14350 = DIRECTION ( 'NONE',  ( -0.8660254037844378194, -0.5000000000000014433, -0.000000000000000000 ) ) ;
#14351 = CARTESIAN_POINT ( 'NONE',  ( 164.1573714183803361, 250.0513545240398230, 10.30907450286302840 ) ) ;
#14352 = CARTESIAN_POINT ( 'NONE',  ( 109.4841275098123248, 234.0177522451418781, -10.00000000000009592 ) ) ;
#14353 = CIRCLE ( 'NONE', #45080, 70.00000000000001421 ) ;
#14354 = EDGE_LOOP ( 'NONE', ( #88705, #96598, #55475, #19963 ) ) ;
#14355 = EDGE_CURVE ( 'NONE', #62875, #97599, #53489, .T. ) ;
#14356 = CARTESIAN_POINT ( 'NONE',  ( 79.25252407528779486, 59.49743072449277292, -16.53464936128684926 ) ) ;
#14357 = AXIS2_PLACEMENT_3D ( 'NONE', #80187, #17339, #2160 ) ;
#14358 = CARTESIAN_POINT ( 'NONE',  ( 155.0438369506338177, 280.3867491788369080, -2.458805040944644915 ) ) ;
#14359 = CARTESIAN_POINT ( 'NONE',  ( 153.9680911965096470, 265.0746596462684579, 16.74034374412752513 ) ) ;
#14360 = CARTESIAN_POINT ( 'NONE',  ( 13.11156449881669595, 184.5024278399160949, -9.188101187500093303 ) ) ;
#14361 = AXIS2_PLACEMENT_3D ( 'NONE', #38804, #53993, #78332 ) ;
#14362 = CARTESIAN_POINT ( 'NONE',  ( 15.40662013169548672, 9.864269794150882120, -3.090169943749474069 ) ) ;
#14363 = CARTESIAN_POINT ( 'NONE',  ( 196.1978789692381895, 273.6107559518669632, 15.03886906253136146 ) ) ;
#14364 = CARTESIAN_POINT ( 'NONE',  ( 146.9422184197532317, 276.1356072505412840, -5.063317562214876943 ) ) ;
#14365 = B_SPLINE_CURVE_WITH_KNOTS ( 'NONE', 3,
 ( #97590, #74790, #50954, #81905 ),
 .UNSPECIFIED., .F., .F.,
 ( 4, 4 ),
 ( 0.002278044366665053690, 0.01021365927721262952 ),
 .UNSPECIFIED. ) ;
#14366 = CARTESIAN_POINT ( 'NONE',  ( 73.10017469210082197, 69.78597432261236122, 9.621008654245756020 ) ) ;
#14368 = CARTESIAN_POINT ( 'NONE',  ( 70.62149783858335184, 202.3923013555409796, 4.594050593750050204 ) ) ;
#14367 = CARTESIAN_POINT ( 'NONE',  ( 174.1634402936988977, 287.2696604785184036, 10.41966287398365232 ) ) ;
#14369 = CARTESIAN_POINT ( 'NONE',  ( 207.8302079587528794, 270.6745157982714431, 3.572475529330238153 ) ) ;
#14370 = CARTESIAN_POINT ( 'NONE',  ( 73.13476967714909449, 57.39438153525127007, 15.88807208273859395 ) ) ;
#14371 = CARTESIAN_POINT ( 'NONE',  ( -21.75249381947928740, 146.7012482093458914, -37.49999999999995737 ) ) ;
#14372 = CARTESIAN_POINT ( 'NONE',  ( 66.43183815540312764, 68.23408033485772251, -4.371383677469295570 ) ) ;
#14373 = ORIENTED_EDGE ( 'NONE', *, *, #74681, .F. ) ;
#14374 = CIRCLE ( 'NONE', #71017, 70.00000000000001421 ) ;
#14375 =( BOUNDED_CURVE ( )  B_SPLINE_CURVE ( 2, ( #59272, #19344, #43594, #27420, #90250, #36492, #3628, #34506, #65407 ),
 .UNSPECIFIED., .F., .T. ) 
 B_SPLINE_CURVE_WITH_KNOTS ( ( 3, 2, 2, 2, 3 ),
 ( 0.1088709677419354843, 0.1102150537634408595, 0.1129032258064516098, 0.1155913978494623601, 0.1169354838709677491 ),
 .UNSPECIFIED. ) 
 CURVE ( )  GEOMETRIC_REPRESENTATION_ITEM ( )  RATIONAL_B_SPLINE_CURVE ( ( 0.9330127018922194093, 0.9330127018922194093, 1.000000000000000000, 0.8660254037844387076, 1.000000000000000000, 0.8660254037844387076, 1.000000000000000000, 0.9330127018922189652, 0.9330127018922192983 ) ) 
 REPRESENTATION_ITEM ( '' )  );
#14376 = CARTESIAN_POINT ( 'NONE',  ( 165.3951733978771017, 269.2638120270026434, 16.94313702576530289 ) ) ;
#14377 = CARTESIAN_POINT ( 'NONE',  ( 7.094665711762471183, 188.2365022471903444, 2.944929066748280225E-16 ) ) ;
#14378 = CARTESIAN_POINT ( 'NONE',  ( 164.4578252119609090, 245.7976863610386999, -6.211333091911165560 ) ) ;
#14379 = CARTESIAN_POINT ( 'NONE',  ( 136.3579783227721691, 249.5333772461660544, 9.188101187500095079 ) ) ;
#14380 = CARTESIAN_POINT ( 'NONE',  ( 21.92109465949963720, 30.84336893147756697, -7.433330006724137462 ) ) ;
#14381 = CARTESIAN_POINT ( 'NONE',  ( 164.6787707939755023, 245.4149973872815167, 0.8898042037103690571 ) ) ;
#14382 = DIRECTION ( 'NONE',  ( -0.4493970231495795775, 0.7783784768652820540, -0.4383711467890876734 ) ) ;
#14383 = CARTESIAN_POINT ( 'NONE',  ( 198.6417698102810903, 282.3377161438529015, -17.61035883595712548 ) ) ;
#14385 = CARTESIAN_POINT ( 'NONE',  ( 185.0625584367380156, 277.4576075603951608, -17.68842772276633823 ) ) ;
#14384 = CARTESIAN_POINT ( 'NONE',  ( 70.98241741224116197, 71.33924828472395063, 4.661226392503834859 ) ) ;
#14386 = CARTESIAN_POINT ( 'NONE',  ( 68.75657388079734744, 64.08238207491497462, 12.00962459721684894 ) ) ;
#14387 = ORIENTED_EDGE ( 'NONE', *, *, #90170, .F. ) ;
#14388 = CARTESIAN_POINT ( 'NONE',  ( 156.9440562780969231, 274.4750137900673508, 13.77464823823377316 ) ) ;
#14389 = CARTESIAN_POINT ( 'NONE',  ( -22.42236680055709641, 157.8615022471902591, 0.000000000000000000 ) ) ;
#14390 = CARTESIAN_POINT ( 'NONE',  ( 189.2060028741113626, 262.3212090535250809, -9.063150766256741875 ) ) ;
#14391 = CARTESIAN_POINT ( 'NONE',  ( 172.8981760910776586, 268.5351074533131168, -17.67640058404859360 ) ) ;
#14392 = CARTESIAN_POINT ( 'NONE',  ( 7.993722094130166766, 16.56628583063838533, 9.188101187500006262 ) ) ;
#14394 = ORIENTED_EDGE ( 'NONE', *, *, #93100, .F. ) ;
#14393 = VECTOR ( 'NONE', #66956, 1000.000000000000227 ) ;
#14395 = CARTESIAN_POINT ( 'NONE',  ( 33.28585168620431745, 96.06718347469407604, 59.99999999999999289 ) ) ;
#14396 = CARTESIAN_POINT ( 'NONE',  ( 171.0863495110653218, 284.1046068702937646, -11.19458109666653023 ) ) ;
#14397 = ADVANCED_FACE ( 'NONE', ( #45392, #44392, #21131, #28708, #99620, #29217, #7390, #84441, #76322, #60084, #6897, #21614, #69191, #59586, #67202, #52494, #13524, #90562, #44887 ), #6414, .T. ) ;
#14398 = EDGE_CURVE ( 'NONE', #38805, #35, #50678, .T. ) ;
#14399 = CARTESIAN_POINT ( 'NONE',  ( 200.8877589446975094, 282.0066036887982364, -16.66018347811495204 ) ) ;
#14400 = CARTESIAN_POINT ( 'NONE',  ( 192.0603001030472683, 293.3461588932823929, -14.68827779892621344 ) ) ;
#14401 = CARTESIAN_POINT ( 'NONE',  ( 183.8037341582430884, 275.4624792557407318, 17.77592483611231700 ) ) ;
#14402 = CARTESIAN_POINT ( 'NONE',  ( 163.2256942281324541, 247.9317998266098471, -9.780520296312531059 ) ) ;
#14403 = CARTESIAN_POINT ( 'NONE',  ( 58.43017357788678368, 217.8207943907113133, 2.194453944013934668E-14 ) ) ;
#14404 = ORIENTED_EDGE ( 'NONE', *, *, #49575, .F. ) ;
#14405 = LINE ( 'NONE', #39164, #89205 ) ;
#14406 = CARTESIAN_POINT ( 'NONE',  ( 9.331744567327184825, 27.16126292948893806, -6.180339887498951690 ) ) ;
#14407 = CARTESIAN_POINT ( 'NONE',  ( 72.52317797754714945, 70.67061044535299175, 7.191400705033394125 ) ) ;
#14408 = ORIENTED_EDGE ( 'NONE', *, *, #88883, .T. ) ;
#14409 = CARTESIAN_POINT ( 'NONE',  ( 190.7222376050763444, 300.3063896652212179, 3.365789908110941475 ) ) ;
#14410 = CARTESIAN_POINT ( 'NONE',  ( 86.13879346367242817, 46.95025718893441535, -10.63009676298478823 ) ) ;
#14411 = CARTESIAN_POINT ( 'NONE',  ( 86.74128215123107566, 44.99823344504448386, -6.819724595823730695 ) ) ;
#14412 = ORIENTED_EDGE ( 'NONE', *, *, #51965, .T. ) ;
#14414 = EDGE_CURVE ( 'NONE', #24764, #73348, #82472, .T. ) ;
#14413 = CARTESIAN_POINT ( 'NONE',  ( 146.6647111637776106, 276.6162639173599587, -0.6373001129109082674 ) ) ;
#14415 = CARTESIAN_POINT ( 'NONE',  ( 79.24569797405095528, 59.88260215966532485, -16.14197575274306828 ) ) ;
#14416 = CARTESIAN_POINT ( 'NONE',  ( 204.4781092559247782, 276.4805210635553863, 13.30606382016679490 ) ) ;
#14417 = CARTESIAN_POINT ( 'NONE',  ( 20.37106723994074997, 58.28585045587018953, 59.99999999999999289 ) ) ;
#14418 = CARTESIAN_POINT ( 'NONE',  ( 69.85710753323976974, 62.58612235388682876, 13.43716744926057061 ) ) ;
#14419 = EDGE_LOOP ( 'NONE', ( #83204, #29267, #74619, #23546 ) ) ;
#14420 = CARTESIAN_POINT ( 'NONE',  ( 96.62871582839601103, 238.8464784336661637, 1.353441290958777525E-15 ) ) ;
#14421 = CARTESIAN_POINT ( 'NONE',  ( 203.0654848288144478, 278.9272583433232171, 16.42392292156888445 ) ) ;
#14422 = CARTESIAN_POINT ( 'NONE',  ( 169.2345181364990765, 254.6337805363678228, -13.16056876093153427 ) ) ;
#14423 = CARTESIAN_POINT ( 'NONE',  ( 178.2910397215446494, 269.1225465846854945, -17.06547196193329796 ) ) ;
#14424 = CARTESIAN_POINT ( 'NONE',  ( 81.38143055733745257, 42.03490022094371170, -7.845107503210293487 ) ) ;
#14425 = VERTEX_POINT ( 'NONE', #99121 ) ;
#14426 = ADVANCED_FACE ( 'NONE', ( #90049 ), #37786, .T. ) ;
#14427 = VERTEX_POINT ( 'NONE', #75327 ) ;
#14428 = VERTEX_POINT ( 'NONE', #91536 ) ;
#14429 = CARTESIAN_POINT ( 'NONE',  ( 80.69421300080995252, 47.47854041208089626, 13.01832096680326600 ) ) ;
#14430 = ORIENTED_EDGE ( 'NONE', *, *, #45700, .F. ) ;
#14431 = CARTESIAN_POINT ( 'NONE',  ( 159.1311797733062861, 257.0237068946943282, -17.13424826516079946 ) ) ;
#14432 = ORIENTED_EDGE ( 'NONE', *, *, #1944, .T. ) ;
#14433 = CARTESIAN_POINT ( 'NONE',  ( 164.2090401137261892, 246.2285947913476889, -5.787448100099915393 ) ) ;
#14434 = DIRECTION ( 'NONE',  ( -0.5000000000000003331, 0.8660254037844383745, -9.251858538542982674E-17 ) ) ;
#14435 = CARTESIAN_POINT ( 'NONE',  ( 170.1297270883495969, 282.5512338199900455, 11.77438199859611956 ) ) ;
#14436 = CARTESIAN_POINT ( 'NONE',  ( -23.53063603519568048, 99.78015757744582004, 45.19948828869558355 ) ) ;
#14437 = CARTESIAN_POINT ( 'NONE',  ( 69.58285789709184144, 68.44046384883969836, -7.877954211123528339 ) ) ;
#14438 = ORIENTED_EDGE ( 'NONE', *, *, #73646, .F. ) ;
#14439 = CARTESIAN_POINT ( 'NONE',  ( 77.04509665064642832, 61.98795237192920382, 15.49868876593534495 ) ) ;
#14440 = CARTESIAN_POINT ( 'NONE',  ( 13.45569633750675465, 25.95586893147754282, 7.433330006724141015 ) ) ;
#14441 = CARTESIAN_POINT ( 'NONE',  ( 201.5505397922970587, 279.0059902033771664, -15.80381168536360370 ) ) ;
#14442 = CARTESIAN_POINT ( 'NONE',  ( 80.47095457055254997, 57.75622231085856129, 16.59751886879109151 ) ) ;
#14443 = VECTOR ( 'NONE', #21793, 1000.000000000000114 ) ;
#14445 = ORIENTED_EDGE ( 'NONE', *, *, #81125, .F. ) ;
#14444 = CARTESIAN_POINT ( 'NONE',  ( 179.1458458498692039, 281.5336445223243800, 16.66751556302194359 ) ) ;
#14446 = CARTESIAN_POINT ( 'NONE',  ( 202.7599932440484451, 279.4563852894229967, 15.58249343055423353 ) ) ;
#14447 = CARTESIAN_POINT ( 'NONE',  ( 188.6122357780320442, 260.1364690911672142, 2.208924378594173010 ) ) ;
#14448 = CARTESIAN_POINT ( 'NONE',  ( 161.3400561738205852, 281.5235411820722220, -6.446175152765177607 ) ) ;
#14449 = CARTESIAN_POINT ( 'NONE',  ( 77.38344707992527560, 49.10671604805792612, -15.27628165681131200 ) ) ;
#14450 = CARTESIAN_POINT ( 'NONE',  ( -19.65312891409030271, 93.06504152958497400, 59.99999999999999289 ) ) ;
#14451 = CARTESIAN_POINT ( 'NONE',  ( 171.2679739083015988, 255.5491317200628885, 11.22258467113546310 ) ) ;
#14452 = CARTESIAN_POINT ( 'NONE',  ( 157.3860572040868533, 282.0393593213248664, 1.488781532780958372 ) ) ;
#14453 = AXIS2_PLACEMENT_3D ( 'NONE', #65168, #4884, #95632 ) ;
#14454 = ORIENTED_EDGE ( 'NONE', *, *, #21336, .F. ) ;
#14455 = CARTESIAN_POINT ( 'NONE',  ( 181.8559704853444430, 270.4563004562098740, -16.38363252787888413 ) ) ;
#14456 = B_SPLINE_CURVE_WITH_KNOTS ( 'NONE', 3,
 ( #78815, #16492, #54469, #23578, #53975, #30705, #55474 ),
 .UNSPECIFIED., .F., .F.,
 ( 4, 2, 1, 4 ),
 ( 0.7443881330833320709, 0.8082910998124995805, 0.8721940665416672012, 1.000000000000000000 ),
 .UNSPECIFIED. ) ;
#14457 = PLANE ( 'NONE',  #4664 ) ;
#14458 = CARTESIAN_POINT ( 'NONE',  ( 1.158783253108745637, 178.1427522451419065, 10.00000000000009237 ) ) ;
#14459 = CARTESIAN_POINT ( 'NONE',  ( 82.87527646796823433, 53.57285545580594999, -15.34456322816472706 ) ) ;
#14460 = CARTESIAN_POINT ( 'NONE',  ( 201.5189872289815867, 266.7509884862435570, -2.318412474989284267 ) ) ;
#14461 = CARTESIAN_POINT ( 'NONE',  ( 204.0543048838297864, 277.2145717684933857, -15.78942579435808824 ) ) ;
#14462 = CARTESIAN_POINT ( 'NONE',  ( 72.11017239049232330, 72.33233329575897130, 0.8941507534055238571 ) ) ;
#14463 = LINE ( 'NONE', #69142, #37060 ) ;
#14465 = CARTESIAN_POINT ( 'NONE',  ( 3.829028248110833754, 163.0177522451418213, 5.000000000000051514 ) ) ;
#14464 = CARTESIAN_POINT ( 'NONE',  ( -6.590166341514275494, 160.8768266524160140, 9.188101187500098632 ) ) ;
#14466 = EDGE_CURVE ( 'NONE', #21, #89234, #10879, .T. ) ;
#14467 = CARTESIAN_POINT ( 'NONE',  ( 25.55183212637049195, 178.8927522451418497, 10.00000000000009948 ) ) ;
#14468 = ORIENTED_EDGE ( 'NONE', *, *, #70209, .F. ) ;
#14469 = ORIENTED_EDGE ( 'NONE', *, *, #26762, .T. ) ;
#14470 = DIRECTION ( 'NONE',  ( 0.000000000000000000, 0.000000000000000000, 1.000000000000000000 ) ) ;
#14471 = DIRECTION ( 'NONE',  ( 0.000000000000000000, -0.000000000000000000, 1.000000000000000000 ) ) ;
#14472 = ADVANCED_FACE ( 'NONE', ( #52008 ), #83947, .T. ) ;
#14473 = CARTESIAN_POINT ( 'NONE',  ( 81.39417835958199987, 46.77585984559194543, -12.26216018662527318 ) ) ;
#14474 = CARTESIAN_POINT ( 'NONE',  ( 85.68543549478557964, 42.81554016910153848, 1.675580183874652018 ) ) ;
#14475 = CARTESIAN_POINT ( 'NONE',  ( 162.8063655212930314, 248.6580984519274296, -10.21361106748447334 ) ) ;
#14476 = CARTESIAN_POINT ( 'NONE',  ( 83.29938471922254450, 44.25013702680151795, 8.630921364687216268 ) ) ;
#14477 = CARTESIAN_POINT ( 'NONE',  ( 169.1417317201558319, 248.6322817555173401, 4.786625344359500822 ) ) ;
#14478 = CARTESIAN_POINT ( 'NONE',  ( 27.99689677000926125, 174.7202760586659736, -5.415160957724236172E-17 ) ) ;
#14479 = CARTESIAN_POINT ( 'NONE',  ( 115.6001716039901055, 246.7369531367911009, -4.594050593750048428 ) ) ;
#14480 = CARTESIAN_POINT ( 'NONE',  ( 181.9266546068691639, 294.6628528558310336, -6.525654968116115562 ) ) ;
#14481 = CARTESIAN_POINT ( 'NONE',  ( 65.81099121317393497, 68.96265426817872424, 2.147452934379848521 ) ) ;
#14482 = ADVANCED_FACE ( 'NONE', ( #76797 ), #82951, .T. ) ;
#14483 = DIRECTION ( 'NONE',  ( -0.1378186779084930869, 0.2387089523694814197, -0.9612616959383223358 ) ) ;
#14484 = B_SPLINE_CURVE_WITH_KNOTS ( 'NONE', 3,
 ( #68892, #30402, #99819, #31887, #61295, #7601, #85145, #45590, #69893, #91242 ),
 .UNSPECIFIED., .F., .F.,
 ( 4, 2, 2, 2, 4 ),
 ( 0.000000000000000000, 0.2500000000000000000, 0.5000000000000000000, 0.7500000000000000000, 1.000000000000000000 ),
 .UNSPECIFIED. ) ;
#14485 = DIRECTION ( 'NONE',  ( -0.000000000000000000, -0.000000000000000000, -1.000000000000000000 ) ) ;
#14486 = CARTESIAN_POINT ( 'NONE',  ( 67.98707691180798918, 203.3927522451417929, -10.00000000000009237 ) ) ;
#14487 = CARTESIAN_POINT ( 'NONE',  ( 193.9204722154232741, 294.7668848255750049, 15.43855698596013859 ) ) ;
#14488 = CARTESIAN_POINT ( 'NONE',  ( 184.0057710604646388, 275.0402031074996216, 16.36095971177830322 ) ) ;
#14489 = CARTESIAN_POINT ( 'NONE',  ( 147.8505793332463725, 274.5622799967613332, -9.317516487097901035 ) ) ;
#14490 = EDGE_CURVE ( 'NONE', #87546, #3917, #85739, .T. ) ;
#14491 = CARTESIAN_POINT ( 'NONE',  ( 167.7509841405270095, 278.2029002482612441, 14.51312790891695137 ) ) ;
#14492 = CARTESIAN_POINT ( 'NONE',  ( -1.503503506619806140, 181.4860189848785694, -2.679491924311240503 ) ) ;
#14493 = CARTESIAN_POINT ( 'NONE',  ( 191.1747001918821525, 299.5227014763493116, -9.654804683100723040 ) ) ;
#14494 = CARTESIAN_POINT ( 'NONE',  ( 162.3216239674494261, 251.7437731844563871, -12.88187769518047610 ) ) ;
#14495 = EDGE_CURVE ( 'NONE', #25441, #49704, #24092, .T. ) ;
#14496 = CARTESIAN_POINT ( 'NONE',  ( 50.53943819540625526, 89.99351993437284136, -10.00000000000000000 ) ) ;
#14497 = CARTESIAN_POINT ( 'NONE',  ( 185.0442626281781031, 269.6655662514531855, 15.59706165446737813 ) ) ;
#14498 = CARTESIAN_POINT ( 'NONE',  ( 87.77910550741502504, 230.6744531367911293, 4.594050593750047540 ) ) ;
#14499 = CARTESIAN_POINT ( 'NONE',  ( 207.8575108622103755, 270.6272257822888037, -6.381720258959569847 ) ) ;
#14500 = CONICAL_SURFACE ( 'NONE', #25803, 2.749999999999999112, 0.7853981633974469467 ) ;
#14501 = CARTESIAN_POINT ( 'NONE',  ( 174.4781466557367651, 251.8266234104975467, -5.118404912015881436 ) ) ;
#14503 = CARTESIAN_POINT ( 'NONE',  ( 82.89325122283835867, 42.00608085941690462, -4.768917158401198009 ) ) ;
#14502 = CARTESIAN_POINT ( 'NONE',  ( 66.07943095046397275, 68.55699243926717656, 2.188521597562036902 ) ) ;
#14504 = CARTESIAN_POINT ( 'NONE',  ( 193.4618118942367175, 290.7196881563408510, -16.34060166011831328 ) ) ;
#14505 = CARTESIAN_POINT ( 'NONE',  ( 188.9122134955663910, 290.7695941481946988, -15.11888497690123678 ) ) ;
#14506 = CARTESIAN_POINT ( 'NONE',  ( 146.4729408656479563, 243.8262482093457493, 3.021315404115420679E-15 ) ) ;
#14507 = CARTESIAN_POINT ( 'NONE',  ( 42.04415689841856363, 29.98920272979930246, 7.433330006724137462 ) ) ;
#14508 = CARTESIAN_POINT ( 'NONE',  ( -13.11024591527734628, 27.99999999999999645, 32.50000000000000000 ) ) ;
#14509 = CARTESIAN_POINT ( 'NONE',  ( 6.427104459464150210, 164.5177522451418213, 5.000000000000051514 ) ) ;
#14510 = VERTEX_POINT ( 'NONE', #32190 ) ;
#14511 = CARTESIAN_POINT ( 'NONE',  ( 25.90481151690805106, 33.14336893147756768, 7.433330006724141015 ) ) ;
#14512 = VECTOR ( 'NONE', #82434, 1000.000000000000000 ) ;
#14513 = CARTESIAN_POINT ( 'NONE',  ( 178.9682364468813773, 280.6870550632783647, 15.99938731543359971 ) ) ;
#14514 = CARTESIAN_POINT ( 'NONE',  ( 146.7943851877206214, 276.3916619194686746, -4.608908220452185844 ) ) ;
#14515 = CARTESIAN_POINT ( 'NONE',  ( 86.18027666378027618, 49.75620593066998509, 1.003037947553365612E-13 ) ) ;
#14516 = ADVANCED_FACE ( 'NONE', ( #17497 ), #93022, .F. ) ;
#14517 = ORIENTED_EDGE ( 'NONE', *, *, #43673, .T. ) ;
#14518 = B_SPLINE_CURVE_WITH_KNOTS ( 'NONE', 3,
 ( #23842, #93288, #47145, #39527, #70452, #1062, #93800, #24361, #55232, #2577, #80605, #19287, #49166, #95813, #4051, #80102, #35449, #50154, #57738, #81106, #10668, #11182, #89223, #26367, #58729, #56752, #27361, #57242, #96802, #50640, #88217, #18272, #11673, #42535, #27851, #34455, #42049, #43024, #73468, #34941, #65837, #72983, #79605, #49647, #58244, #10168, #71972, #88717, #19771, #81593 ),
 .UNSPECIFIED., .F., .F.,
 ( 4, 2, 2, 2, 2, 2, 2, 2, 2, 2, 2, 2, 2, 2, 2, 2, 2, 2, 2, 2, 2, 2, 2, 2, 4 ),
 ( 0.001702369874200513212, 0.002155302416493423082, 0.002608234958786333386, 0.002834701229932852073, 0.002947934365506177552, 0.003061167501079503465, 0.003287633772226124067, 0.003514100043372744668, 0.003967032585666028371, 0.004419965127959312942, 0.005325830212545880349, 0.006231695297132447756, 0.006684627839425727122, 0.007137560381719008223, 0.007250793517292348014, 0.007307410085079029186, 0.007364026652865710357, 0.007477259788438970350, 0.007590492924012230344, 0.007816959195158743393, 0.008043425466305256441, 0.008269891737451771224, 0.008496358008598284273, 0.008722824279744799056, 0.008949290550891312104 ),
 .UNSPECIFIED. ) ;
#14519 = CARTESIAN_POINT ( 'NONE',  ( 70.86521028213462614, 60.91151414948516418, 14.54696446430460810 ) ) ;
#14520 = CARTESIAN_POINT ( 'NONE',  ( 76.03824915322937272, 65.38513206480712370, -14.40956150002899783 ) ) ;
#14521 = CARTESIAN_POINT ( 'NONE',  ( 180.1973166148897576, 262.1945337904856501, -12.69576189704895519 ) ) ;
#14522 = CARTESIAN_POINT ( 'NONE',  ( 173.2643044339734786, 253.6696019359482364, -9.161360666162188693 ) ) ;
#14523 = CIRCLE ( 'NONE', #45238, 70.00000000000001421 ) ;
#14524 = CARTESIAN_POINT ( 'NONE',  ( 173.4036004108148177, 284.0055530444776650, -13.75802448165205405 ) ) ;
#14525 = EDGE_CURVE ( 'NONE', #65117, #18962, #26434, .T. ) ;
#14526 = VERTEX_POINT ( 'NONE', #77303 ) ;
#14527 = CARTESIAN_POINT ( 'NONE',  ( 73.46598367719339251, 69.88918780369783690, 9.751349427452053575 ) ) ;
#14528 = B_SPLINE_SURFACE_WITH_KNOTS ( 'NONE', 3, 1, ( 
 ( #47921, #63134 ),
 ( #94079, #2355 ),
 ( #39311, #64138 ),
 ( #23616, #54509 ),
 ( #70736, #1850 ),
 ( #24632, #86006 ),
 ( #31713, #47429 ),
 ( #16036, #1347 ),
 ( #17534, #8442 ),
 ( #62114, #55512 ),
 ( #46937, #8938 ),
 ( #71256, #87521 ),
 ( #70228, #62618 ),
 ( #48442, #32233 ),
 ( #40317, #93571 ),
 ( #2869, #32732 ),
 ( #93061, #79883 ),
 ( #39804, #48948 ),
 ( #40813, #95088 ),
 ( #63636, #86500 ),
 ( #24140, #94573 ),
 ( #41319, #33234 ),
 ( #17028, #77854 ),
 ( #25129, #55025 ),
 ( #56011, #87007 ),
 ( #79388, #71760 ),
 ( #25651, #56532 ),
 ( #10446, #18053 ),
 ( #16532, #78356 ),
 ( #11953, #80898 ),
 ( #58521, #89494 ),
 ( #3367, #49434 ),
 ( #19064, #81875 ),
 ( #34730, #50925 ) ),
 .UNSPECIFIED., .T., .F., .F.,
 ( 4, 2, 2, 2, 2, 2, 2, 2, 2, 2, 2, 2, 2, 2, 2, 2, 4 ),
 ( 2, 2 ),
 ( 0.000000000000000000, 0.06250000000000000000, 0.1250000000000000000, 0.1875000000000000000, 0.2500000000000000000, 0.3125000000000000000, 0.3750000000000000000, 0.4375000000000000000, 0.5000000000000000000, 0.5625000000000000000, 0.6250000000000000000, 0.6875000000000000000, 0.7500000000000000000, 0.8125000000000000000, 0.8750000000000000000, 0.9375000000000000000, 1.000000000000000000 ),
 ( 0.000000000000000000, 1.000000000000000000 ),
 .UNSPECIFIED. ) ;
#14529 = ORIENTED_EDGE ( 'NONE', *, *, #17227, .T. ) ;
#14530 = DIRECTION ( 'NONE',  ( -0.000000000000000000, -0.000000000000000000, -1.000000000000000000 ) ) ;
#14531 = CARTESIAN_POINT ( 'NONE',  ( 184.7674300623272359, 293.5985477127894683, -10.64018628136773970 ) ) ;
#14532 = VERTEX_POINT ( 'NONE', #32692 ) ;
#14534 = EDGE_CURVE ( 'NONE', #71177, #36219, #14456, .T. ) ;
#14533 = FACE_OUTER_BOUND ( 'NONE', #48826, .T. ) ;
#14535 = CARTESIAN_POINT ( 'NONE',  ( 159.3056354669941470, 256.7215407695565546, 17.03060606420897471 ) ) ;
#14536 = CARTESIAN_POINT ( 'NONE',  ( 190.4965153239555775, 278.7350028254225549, -16.50919675735249115 ) ) ;
#14537 = CARTESIAN_POINT ( 'NONE',  ( 192.5136100383170401, 297.2036415955699340, -12.98767194394231872 ) ) ;
#14538 = CARTESIAN_POINT ( 'NONE',  ( 188.8544700204132880, 297.4231428397746413, 9.261439979758030461 ) ) ;
#14539 = EDGE_CURVE ( 'NONE', #34466, #4961, #46895, .T. ) ;
#14540 = CARTESIAN_POINT ( 'NONE',  ( 35.45274159363147959, 38.65586893147759184, -7.433330006724137462 ) ) ;
#14541 = CARTESIAN_POINT ( 'NONE',  ( 81.59924320624311633, 55.92250459863397083, -16.38315390958105411 ) ) ;
#14542 = EDGE_CURVE ( 'NONE', #29044, #14044, #25086, .T. ) ;
#14543 = EDGE_CURVE ( 'NONE', #76666, #16524, #39763, .T. ) ;
#14544 = AXIS2_PLACEMENT_3D ( 'NONE', #31, #8622, #9121 ) ;
#14545 = CARTESIAN_POINT ( 'NONE',  ( 71.21219703145997926, 63.67509445150784586, -13.83477564754000788 ) ) ;
#14546 = ORIENTED_EDGE ( 'NONE', *, *, #72666, .F. ) ;
#14547 = DIRECTION ( 'NONE',  ( -0.000000000000000000, -0.000000000000000000, 1.000000000000000000 ) ) ;
#14548 = ORIENTED_EDGE ( 'NONE', *, *, #29889, .T. ) ;
#14549 = EDGE_LOOP ( 'NONE', ( #67521, #20126, #38689, #42561 ) ) ;
#14550 = CARTESIAN_POINT ( 'NONE',  ( -15.31269525828471068, 104.2312461070085021, 36.50000000000000000 ) ) ;
#14551 = CARTESIAN_POINT ( 'NONE',  ( 87.15508732983295204, 45.91009000376428872, -8.663677684674611967 ) ) ;
#14553 = CARTESIAN_POINT ( 'NONE',  ( 164.4219970653926453, 246.2565599513234815, 2.253343996881020050 ) ) ;
#14552 = FACE_OUTER_BOUND ( 'NONE', #46879, .T. ) ;
#14554 = CARTESIAN_POINT ( 'NONE',  ( 206.7044739906782809, 272.6243442267827959, -10.28926534613781030 ) ) ;
#14555 = CARTESIAN_POINT ( 'NONE',  ( 70.16456968396876448, 70.84923341515788309, 4.730100017123507250 ) ) ;
#14556 = CARTESIAN_POINT ( 'NONE',  ( 200.0313018224816801, 276.5939864008022369, 15.71640468486303099 ) ) ;
#14557 = CARTESIAN_POINT ( 'NONE',  ( 189.9457600613112902, 301.6512882219586800, 0.04117870562599101891 ) ) ;
#14558 = CARTESIAN_POINT ( 'NONE',  ( 170.9803632111054128, 287.8799287371469973, -4.334810812907764266 ) ) ;
#14559 = CARTESIAN_POINT ( 'NONE',  ( 77.08113471857714671, 63.57880127914461355, -15.41835532793242791 ) ) ;
#14560 = CARTESIAN_POINT ( 'NONE',  ( 183.6912085166904944, 284.8534958222698492, -15.01658379341915683 ) ) ;
#14561 = CARTESIAN_POINT ( 'NONE',  ( 114.8970466070627907, 227.9548013555409796, -4.594050593750042211 ) ) ;
#14562 = EDGE_LOOP ( 'NONE', ( #63093, #55643, #95199, #41335 ) ) ;
#14563 = CARTESIAN_POINT ( 'NONE',  ( 148.2066559145867757, 274.5764911490276177, -6.721604152511306829 ) ) ;
#14564 = CARTESIAN_POINT ( 'NONE',  ( 39.38594668318775405, 31.24335787977766188, -9.188101187500008038 ) ) ;
#14565 = CARTESIAN_POINT ( 'NONE',  ( 188.4921780175364177, 291.9130024176957932, -14.30062038179651474 ) ) ;
#14566 = EDGE_LOOP ( 'NONE', ( #92678, #83072, #30486, #36692 ) ) ;
#14567 = ORIENTED_EDGE ( 'NONE', *, *, #80039, .T. ) ;
#14568 = B_SPLINE_CURVE_WITH_KNOTS ( 'NONE', 3,
 ( #46430, #38339, #75380, #52547, #99172, #53052, #60139, #5963, #13576, #44946, #83499, #36856, #22662, #84008, #54029, #30760, #53544, #45444, #69743, #37840, #91099, #21667, #30255, #61140, #67766, #76378, #77359, #84984, #6951, #44447, #75889 ),
 .UNSPECIFIED., .F., .F.,
 ( 4, 3, 3, 3, 3, 3, 3, 3, 3, 3, 4 ),
 ( 0.000000000000000000, 0.1333490885032349860, 0.3007194338854367599, 0.4699862290245074292, 0.5844252810809225096, 0.6686540514502804511, 0.7354980260655492597, 0.8028463152565746830, 0.8633854507757233732, 0.9437142632667367970, 1.000000000000000000 ),
 .UNSPECIFIED. ) ;
#14569 = CARTESIAN_POINT ( 'NONE',  ( 86.92574391271591594, 45.77938117786232652, -8.666101563913320760 ) ) ;
#14570 = LINE ( 'NONE', #84011, #78747 ) ;
#14571 = CARTESIAN_POINT ( 'NONE',  ( 146.6682761148193777, 276.6100892410288452, 3.415557024771299410 ) ) ;
#14572 = CARTESIAN_POINT ( 'NONE',  ( 159.2102594322688844, 254.8867369075254885, -16.13039487917589199 ) ) ;
#14573 = CARTESIAN_POINT ( 'NONE',  ( -69.42640704509901184, 61.99316646242160544, 59.99999999999999289 ) ) ;
#14574 = EDGE_LOOP ( 'NONE', ( #42344, #84005, #99466 ) ) ;
#14575 = CARTESIAN_POINT ( 'NONE',  ( 147.9582107679231626, 274.3758568834094262, 9.970076002444663743 ) ) ;
#14576 = ORIENTED_EDGE ( 'NONE', *, *, #29555, .F. ) ;
#14577 = CARTESIAN_POINT ( 'NONE',  ( 46.28462696178780789, 185.9824982072973967, 3.021315404115420679E-15 ) ) ;
#14578 = ORIENTED_EDGE ( 'NONE', *, *, #20011, .T. ) ;
#14579 = CYLINDRICAL_SURFACE ( 'NONE', #74268, 10.00000000000001066 ) ;
#14580 = CARTESIAN_POINT ( 'NONE',  ( 191.7730772792068308, 298.4862819590180720, -10.97593358402262886 ) ) ;
#14581 = LINE ( 'NONE', #77379, #2538 ) ;
#14582 = CARTESIAN_POINT ( 'NONE',  ( 69.55679667848153258, 71.27692851584133393, -0.5916159062426952220 ) ) ;
#14584 = CARTESIAN_POINT ( 'NONE',  ( 69.72818323148324282, 63.14936655818974032, -13.63905201428613090 ) ) ;
#14583 = CARTESIAN_POINT ( 'NONE',  ( 184.3598761222536382, 288.8827646574232517, -13.18844735319207118 ) ) ;
#14585 = CARTESIAN_POINT ( 'NONE',  ( 200.9450245801223787, 276.0628505547339273, -15.19655820136303070 ) ) ;
#14586 = ORIENTED_EDGE ( 'NONE', *, *, #16992, .T. ) ;
#14587 = CARTESIAN_POINT ( 'NONE',  ( 204.6861706212249885, 276.1201482077632363, 14.69005155300678922 ) ) ;
#14588 = CARTESIAN_POINT ( 'NONE',  ( 73.17451026478642007, 68.08244569788803346, 10.88860031406959727 ) ) ;
#14589 = CARTESIAN_POINT ( 'NONE',  ( 82.62224726316846102, 40.93996069151095440, -3.627884205396067596 ) ) ;
#14590 = CARTESIAN_POINT ( 'NONE',  ( 173.3159035555527225, 251.5876627122220555, -0.6300199127931779275 ) ) ;
#14591 = CARTESIAN_POINT ( 'NONE',  ( 190.8844566442973303, 271.0387251322553084, -14.20173667283605567 ) ) ;
#14592 = CARTESIAN_POINT ( 'NONE',  ( 71.66453512356649469, 72.11062924793525042, 3.341973230705638898 ) ) ;
#14593 = CARTESIAN_POINT ( 'NONE',  ( 84.87297731598476958, 46.29707946066870505, 10.07320804996537689 ) ) ;
#14594 = CARTESIAN_POINT ( 'NONE',  ( -27.12601731895737700, 23.20384585402105770, -10.00000000000000000 ) ) ;
#14595 = VECTOR ( 'NONE', #42476, 1000.000000000000114 ) ;
#14596 = CARTESIAN_POINT ( 'NONE',  ( 191.3748554418409356, 282.8820735151286954, -16.91564750171852438 ) ) ;
#14597 = CARTESIAN_POINT ( 'NONE',  ( 82.66575685400569284, 54.08976349579732812, -15.88644314918171574 ) ) ;
#14598 = CARTESIAN_POINT ( 'NONE',  ( 71.43287601098374751, 221.2369531367911293, -4.594050593750048428 ) ) ;
#14599 = CARTESIAN_POINT ( 'NONE',  ( -13.51183432020139819, 142.4280072687214442, 0.000000000000000000 ) ) ;
#14600 = CARTESIAN_POINT ( 'NONE',  ( 147.4824818982269790, 275.1998434563504929, -4.972419998968698351 ) ) ;
#14601 = CARTESIAN_POINT ( 'NONE',  ( -13.79761285583127872, 128.9229902121449811, 8.559299291603829198E-14 ) ) ;
#14602 = EDGE_CURVE ( 'NONE', #92597, #15171, #7910, .T. ) ;
#14603 = LINE ( 'NONE', #60171, #70848 ) ;
#14604 = CARTESIAN_POINT ( 'NONE',  ( 207.1158949475991164, 271.9117422260973740, -5.823035679195911918 ) ) ;
#14605 = CARTESIAN_POINT ( 'NONE',  ( 65.72708745793390506, 69.07493967346769637, -0.1118595723326069880 ) ) ;
#14607 = CARTESIAN_POINT ( 'NONE',  ( -20.90861557574503848, 95.08343395685160715, 45.19941947175312436 ) ) ;
#14606 = CARTESIAN_POINT ( 'NONE',  ( 106.9582200821077578, 225.8927522451417929, -10.00000000000009237 ) ) ;
#14608 = CARTESIAN_POINT ( 'NONE',  ( 81.35748880148537410, 42.22347387491733173, -7.155507324468848296 ) ) ;
#14609 = EDGE_CURVE ( 'NONE', #20973, #31576, #40276, .T. ) ;
#14610 = CARTESIAN_POINT ( 'NONE',  ( 39.30595310148520838, 34.64441083166263979, -10.00000000000000533 ) ) ;
#14611 = CARTESIAN_POINT ( 'NONE',  ( 204.9365032683681704, 275.6865593441178817, -12.41571226031502206 ) ) ;
#14612 = CARTESIAN_POINT ( 'NONE',  ( -106.6146531411566798, 123.6868197944956620, 37.50000000000002132 ) ) ;
#14613 = LINE ( 'NONE', #84546, #67321 ) ;
#14614 = ADVANCED_FACE ( 'NONE', ( #79349 ), #17860, .T. ) ;
#14615 = CARTESIAN_POINT ( 'NONE',  ( 46.88655524640979166, 204.0024278399160949, -9.188101187500093303 ) ) ;
#14616 = CARTESIAN_POINT ( 'NONE',  ( 157.7861133721078772, 257.3534302411229646, 18.03837896619386783 ) ) ;
#14617 = CARTESIAN_POINT ( 'NONE',  ( 199.2515784447019200, 277.9484561788881933, 15.93523832605907664 ) ) ;
#14618 = CARTESIAN_POINT ( 'NONE',  ( 80.07311184616966671, 50.58256448429610685, -14.76394167379344857 ) ) ;
#14619 = CARTESIAN_POINT ( 'NONE',  ( -16.28802019041737026, 174.7365022471903444, 2.944929066748280225E-16 ) ) ;
#14620 = CARTESIAN_POINT ( 'NONE',  ( 49.51212862133765213, 190.2048013555409796, 4.594050593750051981 ) ) ;
#14621 = CARTESIAN_POINT ( 'NONE',  ( 21.69737781089059681, 21.03085787977762777, 9.188101187500006262 ) ) ;
#14622 = CARTESIAN_POINT ( 'NONE',  ( 151.3681950933278983, 268.4695907787949523, -15.50699599486383917 ) ) ;
#14623 = PLANE ( 'NONE',  #81497 ) ;
#14624 = CARTESIAN_POINT ( 'NONE',  ( 10.31635424878816742, 24.14336893147753926, 7.433330006724141015 ) ) ;
#14625 = CARTESIAN_POINT ( 'NONE',  ( 168.9579038699606315, 279.3139280689009070, 15.08363371378442608 ) ) ;
#14626 = CARTESIAN_POINT ( 'NONE',  ( 76.92864961180355010, 63.84291323147403574, 14.92053277014489687 ) ) ;
#14627 = DIRECTION ( 'NONE',  ( -0.5000000000000013323, 0.8660254037844380415, 0.000000000000000000 ) ) ;
#14628 = CARTESIAN_POINT ( 'NONE',  ( 178.8898168495310586, 276.3570583279081916, 16.31703817734112150 ) ) ;
#14629 = DIRECTION ( 'NONE',  ( -0.000000000000000000, 0.000000000000000000, -1.000000000000000000 ) ) ;
#14630 = CARTESIAN_POINT ( 'NONE',  ( 153.3530509526309515, 276.8034356616051355, 7.280424537284008402 ) ) ;
#14631 = CARTESIAN_POINT ( 'NONE',  ( 151.3998834813064036, 275.6155462708605342, 9.529510778888534261 ) ) ;
#14632 = CARTESIAN_POINT ( 'NONE',  ( 90.95479231155565003, 229.9865022471903160, 10.00000000000009237 ) ) ;
#14633 = CARTESIAN_POINT ( 'NONE',  ( 200.6097954076514895, 283.1806371883870383, 16.82611162221071766 ) ) ;
#14634 = EDGE_CURVE ( 'NONE', #33594, #82113, #58478, .T. ) ;
#14635 = CARTESIAN_POINT ( 'NONE',  ( 194.2178510179977025, 285.2388007311112119, -17.07337800795351512 ) ) ;
#14636 = ORIENTED_EDGE ( 'NONE', *, *, #57037, .T. ) ;
#14637 = CARTESIAN_POINT ( 'NONE',  ( 77.07931261141762036, 49.50410267394570951, 15.47847711487539257 ) ) ;
#14638 = ORIENTED_EDGE ( 'NONE', *, *, #25046, .F. ) ;
#14639 = CARTESIAN_POINT ( 'NONE',  ( 163.5580161323163111, 263.8619878914579431, 16.86834041886016777 ) ) ;
#14640 = CARTESIAN_POINT ( 'NONE',  ( 187.6409835355971438, 276.9958261499423315, -17.68842699041714184 ) ) ;
#14641 = FACE_OUTER_BOUND ( 'NONE', #61987, .T. ) ;
#14642 = ORIENTED_EDGE ( 'NONE', *, *, #97048, .T. ) ;
#14643 = PLANE ( 'NONE',  #53793 ) ;
#14645 = EDGE_CURVE ( 'NONE', #85510, #97286, #67547, .T. ) ;
#14644 = CARTESIAN_POINT ( 'NONE',  ( 32.00866654959714452, 120.8840912179599343, 59.99999999999999289 ) ) ;
#14646 = CARTESIAN_POINT ( 'NONE',  ( 194.2223991963907963, 294.2439319543634610, -14.97294938100067441 ) ) ;
#14647 = LINE ( 'NONE', #29843, #80587 ) ;
#14648 = DIRECTION ( 'NONE',  ( -0.8660254037844387076, -0.4999999999999998890, -0.000000000000000000 ) ) ;
#14649 = CARTESIAN_POINT ( 'NONE',  ( 204.8176812644112204, 275.8923650920285695, 14.65594551021579051 ) ) ;
#14650 = VERTEX_POINT ( 'NONE', #90941 ) ;
#14651 = CARTESIAN_POINT ( 'NONE',  ( 22.22900788544320605, 15.76004757982089544, 5.678558825948272215 ) ) ;
#14652 = CARTESIAN_POINT ( 'NONE',  ( 68.77081067755379706, 69.84697089389068481, -3.678078207114283238 ) ) ;
#14653 = FACE_OUTER_BOUND ( 'NONE', #34252, .T. ) ;
#14654 = EDGE_CURVE ( 'NONE', #28879, #90346, #5299, .T. ) ;
#14655 = ORIENTED_EDGE ( 'NONE', *, *, #28143, .F. ) ;
#14656 = CARTESIAN_POINT ( 'NONE',  ( 109.1931406464380530, 245.3967562850346837, -4.648177544792955347E-16 ) ) ;
#14657 = CARTESIAN_POINT ( 'NONE',  ( 206.8791291248445532, 272.3218326606039454, -10.16823074922856840 ) ) ;
#14658 = ORIENTED_EDGE ( 'NONE', *, *, #22404, .F. ) ;
#14659 = AXIS2_PLACEMENT_3D ( 'NONE', #62915, #3154, #41099 ) ;
#14660 = VERTEX_POINT ( 'NONE', #22483 ) ;
#14661 = CARTESIAN_POINT ( 'NONE',  ( 174.6137555705638249, 286.1945818789523628, 10.50642072453899090 ) ) ;
#14663 = CARTESIAN_POINT ( 'NONE',  ( 68.11396990062021928, 66.09066184282977474, -10.54551009860708355 ) ) ;
#14662 = CARTESIAN_POINT ( 'NONE',  ( 159.6624207053301063, 282.2709084101314829, -3.217951961837643982 ) ) ;
#14664 = CARTESIAN_POINT ( 'NONE',  ( 208.0006710756887287, 270.3792650189220126, -0.8737665032493013850 ) ) ;
#14665 = CARTESIAN_POINT ( 'NONE',  ( 164.4864504671816690, 245.7481059646165704, 6.337356894698421783 ) ) ;
#14666 = CARTESIAN_POINT ( 'NONE',  ( 159.5204760365350012, 254.3494259875849082, 16.90107507090185379 ) ) ;
#14667 = CARTESIAN_POINT ( 'NONE',  ( 164.5425133943092817, 265.0501716792783213, -16.62885785886519230 ) ) ;
#14668 = CARTESIAN_POINT ( 'NONE',  ( 138.6044920356617922, 241.6423013555409796, -4.594050593750043987 ) ) ;
#14669 = CARTESIAN_POINT ( 'NONE',  ( 159.5747039080428351, 254.6547520131815929, -15.43565639722316796 ) ) ;
#14670 = CARTESIAN_POINT ( 'NONE',  ( 195.7711535398184708, 291.1477395053983628, -15.80671369234383938 ) ) ;
#14671 = CARTESIAN_POINT ( 'NONE',  ( 71.83943283659645829, 200.0327760586659451, 1.948934522072303157E-15 ) ) ;
#14672 = VERTEX_POINT ( 'NONE', #99501 ) ;
#14673 = CARTESIAN_POINT ( 'NONE',  ( 178.9714194486930694, 253.6239517424200187, 1.422777586239305059 ) ) ;
#14674 = FACE_OUTER_BOUND ( 'NONE', #64447, .T. ) ;
#14675 = ORIENTED_EDGE ( 'NONE', *, *, #14170, .F. ) ;
#14676 = CARTESIAN_POINT ( 'NONE',  ( 160.3870543052771325, 253.9566894099726824, 15.32724566468392169 ) ) ;
#14677 = VERTEX_POINT ( 'NONE', #91418 ) ;
#14678 = FACE_BOUND ( 'NONE', #17660, .T. ) ;
#14679 = CARTESIAN_POINT ( 'NONE',  ( 66.43852593890612468, 67.87665097547890980, 6.658925527579347303 ) ) ;
#14680 = CARTESIAN_POINT ( 'NONE',  ( 190.5360041683329655, 260.2350817476381621, -0.09936466574572885846 ) ) ;
#14681 = CARTESIAN_POINT ( 'NONE',  ( -32.77609386396424185, 95.58753423100951352, 11.08839328151203851 ) ) ;
#14682 =( BOUNDED_CURVE ( )  B_SPLINE_CURVE ( 2, ( #70060, #677, #39647, #78694, #86332, #89806, #57863, #35565, #26980 ),
 .UNSPECIFIED., .F., .T. ) 
 B_SPLINE_CURVE_WITH_KNOTS ( ( 3, 2, 2, 2, 3 ),
 ( 0.9556451612903226200, 0.9569892473118279952, 0.9596774193548387455, 0.9623655913978494958, 0.9637096774193548709 ),
 .UNSPECIFIED. ) 
 CURVE ( )  GEOMETRIC_REPRESENTATION_ITEM ( )  RATIONAL_B_SPLINE_CURVE ( ( 0.9330127018922194093, 0.9330127018922194093, 1.000000000000000000, 0.8660254037844387076, 1.000000000000000000, 0.8660254037844387076, 1.000000000000000000, 0.9330127018922194093, 0.9330127018922194093 ) ) 
 REPRESENTATION_ITEM ( '' )  );
#14683 = CARTESIAN_POINT ( 'NONE',  ( 67.81833433099461672, 65.48244593839081062, 10.25897341332929003 ) ) ;
#14684 = CARTESIAN_POINT ( 'NONE',  ( 194.3562588153086779, 294.0120802933159325, 14.11474987148825200 ) ) ;
#14685 = DIRECTION ( 'NONE',  ( 1.000000000000000000, 0.000000000000000000, 0.000000000000000000 ) ) ;
#14686 = ORIENTED_EDGE ( 'NONE', *, *, #74528, .F. ) ;
#14687 = CARTESIAN_POINT ( 'NONE',  ( 161.9495997252073209, 250.1420603409351031, -13.99339207224158166 ) ) ;
#14688 = ORIENTED_EDGE ( 'NONE', *, *, #42973, .F. ) ;
#14689 = EDGE_CURVE ( 'NONE', #86588, #7077, #86052, .T. ) ;
#14690 = CARTESIAN_POINT ( 'NONE',  ( 76.22774175637606220, 51.62333717891167595, -16.17666187944767486 ) ) ;
#14691 = PLANE ( 'NONE',  #22310 ) ;
#14692 = CARTESIAN_POINT ( 'NONE',  ( 195.4492297588524821, 279.3069192732683064, 16.32671115009019758 ) ) ;
#14693 = CARTESIAN_POINT ( 'NONE',  ( 162.5087209356614437, 261.3603897694041507, 16.94627484035424203 ) ) ;
#14694 = CARTESIAN_POINT ( 'NONE',  ( 141.5541307454787727, 252.5333772461660260, 9.188101187500095079 ) ) ;
#14695 = VERTEX_POINT ( 'NONE', #9399 ) ;
#14696 = CARTESIAN_POINT ( 'NONE',  ( 88.25652195435415592, 44.39905568574920380, 4.349260828767086196 ) ) ;
#14697 = CARTESIAN_POINT ( 'NONE',  ( 182.0267153670255880, 257.6526772771978813, 6.606610945396032442 ) ) ;
#14698 = CARTESIAN_POINT ( 'NONE',  ( 155.5207183646172950, 261.6826666266933898, -16.99780945766855922 ) ) ;
#14699 = CARTESIAN_POINT ( 'NONE',  ( 153.3544108199959908, 265.0293642254135307, -17.49105661178601423 ) ) ;
#14700 = CARTESIAN_POINT ( 'NONE',  ( 79.52159056500875067, 59.38160983241339608, -16.21114012547523231 ) ) ;
#14701 = CARTESIAN_POINT ( 'NONE',  ( 69.02655799626819544, 67.42939723981996281, -8.834294664151611798 ) ) ;
#14702 = ORIENTED_EDGE ( 'NONE', *, *, #81736, .T. ) ;
#14703 = CARTESIAN_POINT ( 'NONE',  ( 195.7085553319017492, 265.4126769123801637, 4.537051660298946132 ) ) ;
#14704 = CARTESIAN_POINT ( 'NONE',  ( 147.9367384712558362, 275.7520979690174840, -3.798240563252472946 ) ) ;
#14705 = CARTESIAN_POINT ( 'NONE',  ( 196.4666053756248800, 263.7899124407235263, 2.070580867331794028 ) ) ;
#14706 = CARTESIAN_POINT ( 'NONE',  ( 80.83664057472495301, 50.73597435593438831, 14.66433228262979327 ) ) ;
#14707 = CARTESIAN_POINT ( 'NONE',  ( 73.34422642274553539, 69.17188908751711551, -9.931122192565558393 ) ) ;
#14708 = ORIENTED_EDGE ( 'NONE', *, *, #13245, .T. ) ;
#14709 = ADVANCED_FACE ( 'NONE', ( #7908 ), #38783, .T. ) ;
#14710 = CARTESIAN_POINT ( 'NONE',  ( 190.1696443193688708, 301.2635093119881162, -4.804312979389741223 ) ) ;
#14711 = CARTESIAN_POINT ( 'NONE',  ( 186.7554075434758545, 282.3000898601083577, 17.53539547572453827 ) ) ;
#14712 = CARTESIAN_POINT ( 'NONE',  ( 164.6649740431187183, 245.4388940607451843, -1.430729255012818557 ) ) ;
#14714 = FACE_BOUND ( 'NONE', #10895, .T. ) ;
#14713 = CARTESIAN_POINT ( 'NONE',  ( 154.9683083969241011, 262.2340116239618055, 18.33261662430134109 ) ) ;
#14715 = EDGE_CURVE ( 'NONE', #59283, #93478, #72409, .T. ) ;
#14716 = CARTESIAN_POINT ( 'NONE',  ( 28.54179425266445591, 16.28848085856231975, 1.475505719884397138E-15 ) ) ;
#14717 = CARTESIAN_POINT ( 'NONE',  ( 31.12960416526798468, 44.88710030135631257, 177.5919119679930134 ) ) ;
#14718 = CARTESIAN_POINT ( 'NONE',  ( -14.06329310883398875, 23.28858607597029007, 10.00000000000000000 ) ) ;
#14719 = CARTESIAN_POINT ( 'NONE',  ( 16.01772687902244741, 32.18080186712592905, 3.090169943749475401 ) ) ;
#14720 = CARTESIAN_POINT ( 'NONE',  ( 32.24342178309110096, 47.97677246190463052, -10.00000000000000000 ) ) ;
#14721 = EDGE_CURVE ( 'NONE', #28370, #70463, #82185, .T. ) ;
#14722 = AXIS2_PLACEMENT_3D ( 'NONE', #26999, #81236, #90331 ) ;
#14723 = CARTESIAN_POINT ( 'NONE',  ( 143.1869494737567265, 260.1427522451419350, -10.00000000000009415 ) ) ;
#14724 = CARTESIAN_POINT ( 'NONE',  ( 74.41009865654250177, 223.7677522451419350, -5.000000000000047962 ) ) ;
#14725 = EDGE_LOOP ( 'NONE', ( #93582, #68270, #68472, #91946 ) ) ;
#14726 = B_SPLINE_CURVE_WITH_KNOTS ( 'NONE', 3,
 ( #7234, #61922, #92384, #84781 ),
 .UNSPECIFIED., .F., .F.,
 ( 4, 4 ),
 ( 0.002373312334363397030, 0.007735900001989939878 ),
 .UNSPECIFIED. ) ;
#14727 = CARTESIAN_POINT ( 'NONE',  ( 66.46588474414394909, 67.86938339201618930, -6.704488035472810914 ) ) ;
#14728 = CARTESIAN_POINT ( 'NONE',  ( 73.11028533216558856, 70.59594333518880660, -7.866013523829703757 ) ) ;
#14729 = CARTESIAN_POINT ( 'NONE',  ( 202.5873807299470002, 274.2480181431063215, -12.90768986605086788 ) ) ;
#14730 = CARTESIAN_POINT ( 'NONE',  ( 184.7894305693181138, 292.1317680087225881, 12.52679022050396895 ) ) ;
#14731 = CARTESIAN_POINT ( 'NONE',  ( 4.315907217689738395, 182.4869531367911293, 4.594050593750046652 ) ) ;
#14732 = CARTESIAN_POINT ( 'NONE',  ( 24.34009904141853653, 32.79103043416549923, 8.090169943749478065 ) ) ;
#14733 = CARTESIAN_POINT ( 'NONE',  ( 84.12761100671502845, 42.09295748728150954, -2.591167056789191125 ) ) ;
#14734 = CARTESIAN_POINT ( 'NONE',  ( 170.1044942758423133, 270.7333397699701436, -17.30097750721906991 ) ) ;
#14735 = CARTESIAN_POINT ( 'NONE',  ( 132.5961804768574837, 237.3615022471901739, 5.000000000000051514 ) ) ;
#14736 = B_SPLINE_CURVE_WITH_KNOTS ( 'NONE', 3,
 ( #47884, #78826, #86972, #27619 ),
 .UNSPECIFIED., .F., .F.,
 ( 4, 4 ),
 ( 0.02417385730324417628, 0.03341671179551596732 ),
 .UNSPECIFIED. ) ;
#14737 = CARTESIAN_POINT ( 'NONE',  ( 179.4558704258684827, 255.0642153075463625, -4.031494673986889765 ) ) ;
#14738 = CARTESIAN_POINT ( 'NONE',  ( 191.2664131384496784, 261.1238491898760685, -1.547456513327413630 ) ) ;
#14739 = CARTESIAN_POINT ( 'NONE',  ( 182.6994280064950829, 295.4856873408559750, 1.017319240502663202 ) ) ;
#14740 = CARTESIAN_POINT ( 'NONE',  ( 55.51991954004235907, 212.8615022471903160, 5.000000000000046185 ) ) ;
#14741 = CARTESIAN_POINT ( 'NONE',  ( 170.8843335314017509, 274.4719442773359219, 17.28596511953734449 ) ) ;
#14742 = EDGE_CURVE ( 'NONE', #3124, #99043, #62572, .T. ) ;
#14743 = CARTESIAN_POINT ( 'NONE',  ( 190.5726849661229210, 300.5654224342945326, -0.2192718484028965964 ) ) ;
#14744 = CARTESIAN_POINT ( 'NONE',  ( 25.07406103223676652, 173.0327760586659451, 1.948934522072303157E-15 ) ) ;
#14745 = CARTESIAN_POINT ( 'NONE',  ( 73.27328646083023500, 70.16270934360544231, -9.274526489422589393 ) ) ;
#14746 = CARTESIAN_POINT ( 'NONE',  ( 30.83975393042360835, 33.50829794293883168, -10.00000000000000355 ) ) ;
#14747 = CARTESIAN_POINT ( 'NONE',  ( 36.01387044229257128, 42.83396525600393545, -2.839279412974133887 ) ) ;
#14748 = DIRECTION ( 'NONE',  ( 1.000000000000000000, 0.000000000000000000, 0.000000000000000000 ) ) ;
#14749 = CARTESIAN_POINT ( 'NONE',  ( 164.9836323268835940, 244.8869617230113249, -2.696511969808454534 ) ) ;
#14750 = DIRECTION ( 'NONE',  ( -0.8660254037844379305, -0.5000000000000014433, -0.000000000000000000 ) ) ;
#14751 = CARTESIAN_POINT ( 'NONE',  ( 202.1313593282997090, 279.2250639425520831, -15.94178289068968368 ) ) ;
#14752 = CARTESIAN_POINT ( 'NONE',  ( 180.0662822340164269, 262.4007578510376675, -14.24330825748563534 ) ) ;
#14753 = CARTESIAN_POINT ( 'NONE',  ( 18.36860284018464995, 32.64646525600389992, -2.839279412974133887 ) ) ;
#14754 = CARTESIAN_POINT ( 'NONE',  ( 190.5969391768923913, 300.5234129089444650, -0.7564693504096553500 ) ) ;
#14755 = CARTESIAN_POINT ( 'NONE',  ( 71.40405452044859658, 59.30247739756921987, 15.23691996167968910 ) ) ;
#14756 = CARTESIAN_POINT ( 'NONE',  ( 155.4812142336614329, 261.3456326552338282, 18.45193178807985745 ) ) ;
#14757 = EDGE_LOOP ( 'NONE', ( #29867, #53360, #89007, #11659, #56206, #27423 ) ) ;
#14758 = CARTESIAN_POINT ( 'NONE',  ( 153.6392919293977002, 266.5359356698173769, -16.75038546547492402 ) ) ;
#14759 = CARTESIAN_POINT ( 'NONE',  ( 37.10733492148454360, 81.41235766493377923, 59.99999999999999289 ) ) ;
#14760 = CARTESIAN_POINT ( 'NONE',  ( 75.18500952680872729, 53.63335195952274148, -16.53975160506809772 ) ) ;
#14761 = CARTESIAN_POINT ( 'NONE',  ( 81.54911411804300769, 41.98910540586440021, 7.610088923344967782 ) ) ;
#14762 = DIRECTION ( 'NONE',  ( 0.5242119900219298634, 0.000000000000000000, 0.8515878049369003389 ) ) ;
#14763 = ORIENTED_EDGE ( 'NONE', *, *, #32108, .F. ) ;
#14764 = CARTESIAN_POINT ( 'NONE',  ( 196.4104189369360256, 289.1535926469882725, -16.93751511765341533 ) ) ;
#14765 = CARTESIAN_POINT ( 'NONE',  ( 72.39511741677974044, 71.78066914166659274, -5.650358525013035482 ) ) ;
#14767 = CARTESIAN_POINT ( 'NONE',  ( 15.54467260552930341, 34.00295985972734059, -10.00000000000000000 ) ) ;
#14766 = B_SPLINE_CURVE_WITH_KNOTS ( 'NONE', 3,
 ( #17554, #33252, #56549, #8455, #71775, #25668, #54524, #55528, #23632, #70752, #16547, #46953, #1365, #86514, #56028, #77870, #1863, #17045, #39329, #78878, #31729, #93587, #9968, #18067, #71273, #32747, #87022, #63651, #48460, #24155, #64153, #79402, #2374, #31243, #48963, #38839, #69745, #356, #62130, #93076, #85505, #50447, #49956, #19080, #51443, #80914, #3860, #65645, #74285, #4353, #66154, #26658 ),
 .UNSPECIFIED., .F., .F.,
 ( 4, 2, 2, 2, 2, 2, 2, 2, 2, 2, 2, 2, 2, 2, 2, 2, 2, 2, 2, 2, 2, 2, 2, 2, 2, 4 ),
 ( 9.707348704973383356E-05, 0.001109464165947084092, 0.001362561835671441965, 0.001615659505395799838, 0.001742208340257978124, 0.001868757175120156844, 0.001995306009982335347, 0.002121854844844514500, 0.002374952514568721886, 0.002628050184292929706, 0.003134245523741467209, 0.004146636202638430760, 0.005159026881535394744, 0.005665222220983831200, 0.005918319890708004759, 0.006044868725570091104, 0.006171417560432177450, 0.006234691977863176388, 0.006297966395294174458, 0.006424515230156154118, 0.006677612899880115173, 0.006930710569604075361, 0.007183808239328036416, 0.007436905909051997471, 0.007690003578775958526, 0.008196198918223731450 ),
 .UNSPECIFIED. ) ;
#14768 = CARTESIAN_POINT ( 'NONE',  ( 154.8579861482817535, 262.4250953638155011, -17.69813260923097786 ) ) ;
#14769 = ORIENTED_EDGE ( 'NONE', *, *, #34866, .F. ) ;
#14770 = EDGE_LOOP ( 'NONE', ( #80188, #26634, #83374, #76057 ) ) ;
#14772 = CARTESIAN_POINT ( 'NONE',  ( -19.65312891409030271, 93.06504152958497400, 177.5919119679930134 ) ) ;
#14771 = DIRECTION ( 'NONE',  ( 0.000000000000000000, -0.000000000000000000, -1.000000000000000000 ) ) ;
#14773 = VERTEX_POINT ( 'NONE', #63090 ) ;
#14774 = CARTESIAN_POINT ( 'NONE',  ( 201.1679199471075492, 282.2139371290980989, -16.62385308864941535 ) ) ;
#14775 = CARTESIAN_POINT ( 'NONE',  ( 28.02677306626161879, 24.38052372038642091, 10.00000000000000533 ) ) ;
#14776 = CARTESIAN_POINT ( 'NONE',  ( 198.8028075628465103, 265.8836465705114165, -5.166853741832800218 ) ) ;
#14777 = CARTESIAN_POINT ( 'NONE',  ( 65.92723761088207368, 68.94945291059251247, -2.624861928015910895 ) ) ;
#14778 = ORIENTED_EDGE ( 'NONE', *, *, #25590, .F. ) ;
#14779 = CARTESIAN_POINT ( 'NONE',  ( 190.6084209867335915, 300.5035258309363826, -0.5505750481748228342 ) ) ;
#14780 = B_SPLINE_CURVE_WITH_KNOTS ( 'NONE', 3,
 ( #77268, #93504, #30677, #38756, #69659, #7361, #14954, #78784, #9369, #92993, #85936, #31644, #23547, #40248, #16461, #62544, #54438, #71189, #85414, #78279, #69160, #15962, #77787, #8864, #39730, #1784, #61053, #92026, #22572, #100090, #45844, #92504, #88945, #80829 ),
 .UNSPECIFIED., .F., .F.,
 ( 4, 2, 2, 2, 2, 2, 2, 2, 2, 2, 2, 2, 2, 2, 2, 2, 4 ),
 ( 0.003474253451082755413, 0.003638662506878291483, 0.003720867034776073612, 0.003803071562673856175, 0.003967480618469285993, 0.004131889674264716678, 0.004460707785855577180, 0.004789525897446437683, 0.005447162120628222873, 0.006104798343810008930, 0.007420070790173648699, 0.008077707013355505880, 0.008159911541253200840, 0.008201013805202004084, 0.008242116069150809063, 0.008406525124946115715, 0.008735343236536794939 ),
 .UNSPECIFIED. ) ;
#14781 = EDGE_CURVE ( 'NONE', #54956, #38929, #86353, .T. ) ;
#14782 = ORIENTED_EDGE ( 'NONE', *, *, #77995, .F. ) ;
#14783 = CARTESIAN_POINT ( 'NONE',  ( 206.2520115784021471, 273.4080321133600933, 11.69992874350409018 ) ) ;
#14784 = CARTESIAN_POINT ( 'NONE',  ( -32.37721085874458282, 42.92243475195172664, 59.99999999999999289 ) ) ;
#14785 = ORIENTED_EDGE ( 'NONE', *, *, #96460, .T. ) ;
#14786 = CARTESIAN_POINT ( 'NONE',  ( 149.6071296322179194, 271.5198456328920997, 12.75640156477042453 ) ) ;
#14787 = CARTESIAN_POINT ( 'NONE',  ( 172.7371573690596449, 271.6299009131761864, 17.79590902495428040 ) ) ;
#14788 = ORIENTED_EDGE ( 'NONE', *, *, #69711, .T. ) ;
#14789 = CARTESIAN_POINT ( 'NONE',  ( -10.97633901967424919, 72.03548929155091685, 14.69827683239626381 ) ) ;
#14790 = CARTESIAN_POINT ( 'NONE',  ( -54.45295541630240166, 33.76759809053437067, -10.00000000000000000 ) ) ;
#14791 = CARTESIAN_POINT ( 'NONE',  ( 78.52645726747817889, 47.93368687526088934, -14.49719720932383638 ) ) ;
#14792 = ORIENTED_EDGE ( 'NONE', *, *, #35208, .T. ) ;
#14793 = AXIS2_PLACEMENT_3D ( 'NONE', #45049, #21754, #60727 ) ;
#14794 = ORIENTED_EDGE ( 'NONE', *, *, #60944, .F. ) ;
#14795 = CARTESIAN_POINT ( 'NONE',  ( 72.55458512285707684, 59.16573985917453626, -15.46293891684866040 ) ) ;
#14796 = CARTESIAN_POINT ( 'NONE',  ( 146.8201187048455267, 276.3470901603510015, 4.112223577763169047 ) ) ;
#14797 = CARTESIAN_POINT ( 'NONE',  ( 147.8503508990560533, 274.5626756563852950, 7.845851077393495743 ) ) ;
#14798 = CARTESIAN_POINT ( 'NONE',  ( 190.7805732161387766, 300.2053494229706985, 4.237982805666590025 ) ) ;
#14799 = CARTESIAN_POINT ( 'NONE',  ( 170.6146439245076181, 275.3170351586339848, -16.42974606418417594 ) ) ;
#14800 = CARTESIAN_POINT ( 'NONE',  ( 147.0565364609189487, 275.9376025950204507, -0.7434588459654102310 ) ) ;
#14801 = CARTESIAN_POINT ( 'NONE',  ( 191.4082244002820516, 299.1182256826033949, -8.271837126846561361 ) ) ;
#14802 = CARTESIAN_POINT ( 'NONE',  ( -62.06645187246645889, 33.74130844118090522, -10.00000000000000000 ) ) ;
#14803 = CARTESIAN_POINT ( 'NONE',  ( 69.12388524367867149, 65.75570191728738223, 10.77047642910910952 ) ) ;
#14804 = CARTESIAN_POINT ( 'NONE',  ( 196.8435556370661459, 289.7039558245273838, -16.43899056939217118 ) ) ;
#14805 = CARTESIAN_POINT ( 'NONE',  ( 67.12926300868817009, 66.68692061479262634, 8.295177568791400446 ) ) ;
#14806 = CARTESIAN_POINT ( 'NONE',  ( 49.04287251715432205, 95.72274150194785136, -10.00000000000000000 ) ) ;
#14807 = CARTESIAN_POINT ( 'NONE',  ( 78.18799119024448885, 47.74668810756791970, 13.95283994106731207 ) ) ;
#14808 = ORIENTED_EDGE ( 'NONE', *, *, #64009, .T. ) ;
#14809 = CARTESIAN_POINT ( 'NONE',  ( 190.8303853669842738, 300.1190722468715535, -3.872629674854036086 ) ) ;
#14810 = CARTESIAN_POINT ( 'NONE',  ( 79.10982015350863605, 53.18341928809535091, -15.72547263405508744 ) ) ;
#14811 = CARTESIAN_POINT ( 'NONE',  ( 202.9971867686660687, 278.5713445860434376, 14.97348638629241790 ) ) ;
#14812 = CARTESIAN_POINT ( 'NONE',  ( 78.98931672906337553, 46.17816290900251630, 12.77312729586772555 ) ) ;
#14813 = CARTESIAN_POINT ( 'NONE',  ( 179.7037933464966670, 282.7974177266479501, -15.46501558881825744 ) ) ;
#14814 = CARTESIAN_POINT ( 'NONE',  ( 189.9718059322956094, 301.6061754500863117, -1.293200095882213185 ) ) ;
#14815 = CARTESIAN_POINT ( 'NONE',  ( 169.2550101512937033, 285.1084512606926751, -7.936393743500282483 ) ) ;
#14816 = ORIENTED_EDGE ( 'NONE', *, *, #83508, .T. ) ;
#14817 = CARTESIAN_POINT ( 'NONE',  ( 207.9743173328493526, 270.4249110404894054, -2.481515874287090639 ) ) ;
#14818 = CARTESIAN_POINT ( 'NONE',  ( 206.8317058779879574, 272.4039721336197317, -10.41591514895975834 ) ) ;
#14819 = CARTESIAN_POINT ( 'NONE',  ( 72.58296766565817393, 71.54644804895973209, 5.445337812415410816 ) ) ;
#14820 = CARTESIAN_POINT ( 'NONE',  ( 42.00631479827475800, 208.3927522451419918, 2.944929066748280225E-16 ) ) ;
#14821 = CARTESIAN_POINT ( 'NONE',  ( 119.1457234225564008, 239.5958772461660544, -9.188101187500095079 ) ) ;
#14822 = CARTESIAN_POINT ( 'NONE',  ( 175.9678885359534206, 274.3885454833871336, 17.74267894519478261 ) ) ;
#14823 = CARTESIAN_POINT ( 'NONE',  ( 50.53943819540625526, 89.99351993437284136, 10.00000000000000000 ) ) ;
#14824 = CARTESIAN_POINT ( 'NONE',  ( 196.4677102463732012, 290.3549391369982686, 16.45225250689336249 ) ) ;
#14825 = CARTESIAN_POINT ( 'NONE',  ( 175.3928363776315678, 253.5036201821030488, -3.893038171866270325 ) ) ;
#14826 = CARTESIAN_POINT ( 'NONE',  ( 43.26059451170998216, 183.5327760586659451, 1.948934522072303157E-15 ) ) ;
#14827 = DIRECTION ( 'NONE',  ( 1.000000000000000000, -7.930164461608259453E-16, 0.000000000000000000 ) ) ;
#14828 = ORIENTED_EDGE ( 'NONE', *, *, #61593, .T. ) ;
#14829 = CARTESIAN_POINT ( 'NONE',  ( 191.3888075987175341, 298.7058057693718069, 7.964122443251637762 ) ) ;
#14830 = CARTESIAN_POINT ( 'NONE',  ( 181.4151141111755123, 267.7021082867859718, 14.95001734426726259 ) ) ;
#14831 = B_SPLINE_SURFACE_WITH_KNOTS ( 'NONE', 3, 1, ( 
 ( #54040, #8961 ),
 ( #86030, #40837 ),
 ( #9473, #71783 ),
 ( #47451, #17562 ),
 ( #54533, #84995 ),
 ( #62139, #70252 ),
 ( #71281, #23146 ),
 ( #87030, #38850 ),
 ( #39337, #78380 ),
 ( #859, #46440 ),
 ( #77371, #31739 ),
 ( #48469, #32755 ),
 ( #30770, #32257 ),
 ( #77881, #62640 ),
 ( #39830, #24655 ),
 ( #40342, #61652 ),
 ( #92600, #7975 ),
 ( #85515, #70761 ),
 ( #15541, #93597 ),
 ( #94104, #365 ),
 ( #16060, #63158 ),
 ( #1374, #79410 ),
 ( #17054, #55538 ),
 ( #86522, #47945 ),
 ( #25153, #56037 ),
 ( #31252, #78886 ),
 ( #1872, #63659 ),
 ( #94600, #96610 ),
 ( #41855, #89518 ),
 ( #88030, #57550 ),
 ( #65159, #49967 ),
 ( #72290, #2893 ),
 ( #33262, #64674 ),
 ( #2382, #26665 ) ),
 .UNSPECIFIED., .T., .F., .F.,
 ( 4, 2, 2, 2, 2, 2, 2, 2, 2, 2, 2, 2, 2, 2, 2, 2, 4 ),
 ( 2, 2 ),
 ( 0.000000000000000000, 0.06250000000000000000, 0.1250000000000000000, 0.1875000000000000000, 0.2500000000000000000, 0.3125000000000000000, 0.3750000000000000000, 0.4375000000000000000, 0.5000000000000000000, 0.5625000000000000000, 0.6250000000000000000, 0.6875000000000000000, 0.7500000000000000000, 0.8125000000000000000, 0.8750000000000000000, 0.9375000000000000000, 1.000000000000000000 ),
 ( 0.000000000000000000, 1.000000000000000000 ),
 .UNSPECIFIED. ) ;
#14832 = EDGE_CURVE ( 'NONE', #69383, #69588, #16153, .T. ) ;
#14833 = FACE_BOUND ( 'NONE', #65518, .T. ) ;
#14834 = CARTESIAN_POINT ( 'NONE',  ( 190.5541309856500050, 300.5975588711562523, -4.167177996129430184 ) ) ;
#14835 = CARTESIAN_POINT ( 'NONE',  ( 97.79278455872236009, 237.2677522451419065, -5.000000000000047962 ) ) ;
#14836 = CARTESIAN_POINT ( 'NONE',  ( 84.14312167556933275, 48.98415679381830756, 0.000000000000000000 ) ) ;
#14837 = ADVANCED_FACE ( 'NONE', ( #85445 ), #93020, .F. ) ;
#14838 = CARTESIAN_POINT ( 'NONE',  ( 68.53315363119618553, 64.54459275260778384, -12.18798101231200448 ) ) ;
#14839 = CARTESIAN_POINT ( 'NONE',  ( 110.2779841299479955, 241.1427522451419065, 10.00000000000009237 ) ) ;
#14840 = EDGE_CURVE ( 'NONE', #63534, #99839, #43503, .T. ) ;
#14841 = LINE ( 'NONE', #76650, #38568 ) ;
#14842 = ORIENTED_EDGE ( 'NONE', *, *, #85523, .T. ) ;
#14843 = EDGE_CURVE ( 'NONE', #52194, #50951, #4777, .T. ) ;
#14844 = CARTESIAN_POINT ( 'NONE',  ( 156.2475800219573046, 280.1524317834912381, -1.584389128937929492 ) ) ;
#14845 = CARTESIAN_POINT ( 'NONE',  ( 79.60268825639580825, 47.69515478760800420, -14.06140264647798510 ) ) ;
#14846 = CARTESIAN_POINT ( 'NONE',  ( 17.60459192459599365, 168.7202760586659736, -5.415160957724236172E-17 ) ) ;
#14847 = CARTESIAN_POINT ( 'NONE',  ( 2.709347677296586987, 25.65659080271448644, -1.878358725466461243E-16 ) ) ;
#14848 = CARTESIAN_POINT ( 'NONE',  ( -15.28083007106358693, 105.8318407428233030, 44.04068696433692054 ) ) ;
#14849 = CARTESIAN_POINT ( 'NONE',  ( 146.9700173529739970, 276.0874580858064746, -5.099093031535578469 ) ) ;
#14850 = CARTESIAN_POINT ( 'NONE',  ( 73.19096742874920380, 69.77356361390103245, 9.106933955064157260 ) ) ;
#14852 = CARTESIAN_POINT ( 'NONE',  ( 74.27495573685767738, 207.5643266524160424, 9.188101187500095079 ) ) ;
#14851 = CARTESIAN_POINT ( 'NONE',  ( 206.9349434189263661, 269.8064106017384916, 1.784245431258210113 ) ) ;
#14853 = CARTESIAN_POINT ( 'NONE',  ( 161.3227470381586102, 251.2278010437646856, 14.45097375514160731 ) ) ;
#14854 = CARTESIAN_POINT ( 'NONE',  ( 74.25393038840245197, 55.45593832152543712, 16.12141555578006091 ) ) ;
#14855 = CARTESIAN_POINT ( 'NONE',  ( 69.03518170984699509, 64.49507618471645287, 12.45339560606362461 ) ) ;
#14856 = CARTESIAN_POINT ( 'NONE',  ( 147.8527080755910958, 276.5585929068648170, -2.411454450074328903 ) ) ;
#14857 = VERTEX_POINT ( 'NONE', #25605 ) ;
#14858 = CARTESIAN_POINT ( 'NONE',  ( 7.022496928113825199, 174.8615022471902591, -10.00000000000009592 ) ) ;
#14859 = CARTESIAN_POINT ( 'NONE',  ( 208.0692320075777957, 270.2605140014760536, 2.043861372130216569 ) ) ;
#14860 = CARTESIAN_POINT ( 'NONE',  ( 129.3483248890680954, 254.6744531367911577, 4.594050593750047540 ) ) ;
#14861 = CARTESIAN_POINT ( 'NONE',  ( 33.82173346387272517, 28.03085787977764909, 9.188101187500006262 ) ) ;
#14862 = CARTESIAN_POINT ( 'NONE',  ( 165.1934173706906392, 261.2005776251094744, -16.15582037233899726 ) ) ;
#14863 = CARTESIAN_POINT ( 'NONE',  ( 185.3203834979958344, 260.3518937614031188, 6.392263009190532586 ) ) ;
#14864 = DIRECTION ( 'NONE',  ( -0.2033683215378938036, 0.3522442655536374700, -0.9135454576426059736 ) ) ;
#14866 = FACE_OUTER_BOUND ( 'NONE', #30971, .T. ) ;
#14865 = CARTESIAN_POINT ( 'NONE',  ( 205.4659066454071876, 268.9227294828852450, 1.478439533706684017 ) ) ;
#14867 = CARTESIAN_POINT ( 'NONE',  ( 68.99533790586593796, 64.15022810885204763, 12.06270211734473463 ) ) ;
#14868 = VERTEX_POINT ( 'NONE', #95042 ) ;
#14869 = CARTESIAN_POINT ( 'NONE',  ( 75.36487073175837281, 53.53173320265494084, -16.04382577248123809 ) ) ;
#14870 = CARTESIAN_POINT ( 'NONE',  ( 164.1097555145034903, 246.4005607616103077, 8.441031814699046620 ) ) ;
#14871 = CARTESIAN_POINT ( 'NONE',  ( 73.37932691289753961, 66.58465441985281075, -12.76502462501827395 ) ) ;
#14872 = CARTESIAN_POINT ( 'NONE',  ( 172.8211258227677263, 268.6731136379477221, -17.49577356889009749 ) ) ;
#14873 = CARTESIAN_POINT ( 'NONE',  ( 193.9563577622949708, 270.9517976046026888, -13.72115171226643682 ) ) ;
#14874 = ORIENTED_EDGE ( 'NONE', *, *, #80771, .F. ) ;
#14875 = CARTESIAN_POINT ( 'NONE',  ( 207.0113543900018840, 272.0928117833072406, 7.993282520509792377 ) ) ;
#14876 = CARTESIAN_POINT ( 'NONE',  ( 168.0320555621825633, 281.9299508771385945, -10.97411773085330822 ) ) ;
#14877 = CARTESIAN_POINT ( 'NONE',  ( -22.42236680055709641, 157.8615022471902591, 0.000000000000000000 ) ) ;
#14878 = CARTESIAN_POINT ( 'NONE',  ( -73.81593683174931186, 48.72104262922892559, -10.00000000000000000 ) ) ;
#14879 = CARTESIAN_POINT ( 'NONE',  ( 91.22542524669037789, 230.1427522451419065, -10.00000000000009592 ) ) ;
#14880 = CARTESIAN_POINT ( 'NONE',  ( 67.32333946482658860, 68.49528494984309646, 5.140773697818922017 ) ) ;
#14881 = CARTESIAN_POINT ( 'NONE',  ( 201.2139346379346705, 282.1342373466909521, -16.65315141107179286 ) ) ;
#14882 = VERTEX_POINT ( 'NONE', #2824 ) ;
#14883 = DIRECTION ( 'NONE',  ( -0.000000000000000000, -0.000000000000000000, -1.000000000000000000 ) ) ;
#14884 = CARTESIAN_POINT ( 'NONE',  ( 164.7647380297938184, 248.9862001899016946, 10.10785415616959071 ) ) ;
#14885 = VERTEX_POINT ( 'NONE', #49396 ) ;
#14886 = CARTESIAN_POINT ( 'NONE',  ( 190.3572031550745294, 300.9386478791372497, 3.093832330100951378 ) ) ;
#14887 = CARTESIAN_POINT ( 'NONE',  ( 71.24177335598133709, 70.40240055988557799, 7.130317524929912665 ) ) ;
#14888 = CARTESIAN_POINT ( 'NONE',  ( 189.0406113324428077, 297.1088540668469591, 8.037437795754774683 ) ) ;
#14889 = ORIENTED_EDGE ( 'NONE', *, *, #99932, .F. ) ;
#14890 = CYLINDRICAL_SURFACE ( 'NONE', #34525, 70.00000000000002842 ) ;
#14891 = CARTESIAN_POINT ( 'NONE',  ( 164.4111102060550991, 279.1452848850144619, 13.51928863813949633 ) ) ;
#14892 = EDGE_CURVE ( 'NONE', #25891, #73044, #13209, .T. ) ;
#14893 = CARTESIAN_POINT ( 'NONE',  ( 149.3801359649374092, 271.9130101976182914, -11.41245530317637424 ) ) ;
#14894 = EDGE_CURVE ( 'NONE', #1725, #97001, #65093, .T. ) ;
#14895 = CARTESIAN_POINT ( 'NONE',  ( 69.40688464331348939, 62.76167709611338097, 13.18428418677036795 ) ) ;
#14896 = VERTEX_POINT ( 'NONE', #89449 ) ;
#14897 = CARTESIAN_POINT ( 'NONE',  ( 105.1810637865323628, 231.5333772461660828, 9.188101187500095079 ) ) ;
#14898 = CARTESIAN_POINT ( 'NONE',  ( 203.4303926360161086, 278.2952194811716709, 16.49722835243206021 ) ) ;
#14899 = CARTESIAN_POINT ( 'NONE',  ( 181.3308514678389258, 271.2102151123074805, -15.98608675868754680 ) ) ;
#14900 = CARTESIAN_POINT ( 'NONE',  ( 131.1144086761837571, 258.0530062829863027, -4.648177544792955347E-16 ) ) ;
#14901 = VERTEX_POINT ( 'NONE', #73704 ) ;
#14902 = VERTEX_POINT ( 'NONE', #80854 ) ;
#14903 = B_SPLINE_CURVE_WITH_KNOTS ( 'NONE', 3,
 ( #41411, #91782, #22348, #18641, #19649, #82481, #43906, #88092, #73339, #33852, #64737, #80980, #11044, #4419, #41921, #11546, #50026, #58599, #49520, #72857, #2960, #96663, #26234, #3446 ),
 .UNSPECIFIED., .F., .F.,
 ( 4, 2, 2, 2, 2, 2, 2, 2, 2, 2, 2, 4 ),
 ( 0.000000000000000000, 0.1250000000000058009, 0.2500000000000116018, 0.3750000000000174305, 0.4375000000000157097, 0.5000000000000139888, 0.5625000000000122125, 0.6250000000000104361, 0.6875000000000086597, 0.7500000000000068834, 0.8750000000000035527, 1.000000000000000000 ),
 .UNSPECIFIED. ) ;
#14904 = ORIENTED_EDGE ( 'NONE', *, *, #11465, .T. ) ;
#14905 = CARTESIAN_POINT ( 'NONE',  ( 80.99519602156757969, 48.45934176588340847, 13.51949272217580500 ) ) ;
#14906 = ORIENTED_EDGE ( 'NONE', *, *, #33038, .T. ) ;
#14907 = CARTESIAN_POINT ( 'NONE',  ( 69.29937091505746594, 69.83787342855333691, 4.724315302973998598 ) ) ;
#14908 = ORIENTED_EDGE ( 'NONE', *, *, #6783, .F. ) ;
#14909 = FACE_OUTER_BOUND ( 'NONE', #53553, .T. ) ;
#14910 = CARTESIAN_POINT ( 'NONE',  ( 165.4414073703629526, 271.0891460371367998, 16.46202333746585111 ) ) ;
#14912 = EDGE_CURVE ( 'NONE', #82888, #38166, #18052, .T. ) ;
#14911 = CARTESIAN_POINT ( 'NONE',  ( 170.8853045030261342, 283.1981579494924972, 11.95786326274130396 ) ) ;
#14913 = CARTESIAN_POINT ( 'NONE',  ( -23.56906976425110400, 99.73991939959820741, 45.19945594742419104 ) ) ;
#14914 = CARTESIAN_POINT ( 'NONE',  ( 68.37595286067593747, 68.37058859125058063, -6.769880321061123141 ) ) ;
#14915 = CARTESIAN_POINT ( 'NONE',  ( 204.2521851317371215, 272.5184155020062349, -10.97406441561872548 ) ) ;
#14916 = CARTESIAN_POINT ( 'NONE',  ( 13.17245041747802148, 29.64646525600389637, -2.839279412974133887 ) ) ;
#14917 = CARTESIAN_POINT ( 'NONE',  ( 198.8683739244561082, 276.4215138120039796, -15.93986209720707414 ) ) ;
#14918 = PLANE ( 'NONE',  #84039 ) ;
#14920 = ORIENTED_EDGE ( 'NONE', *, *, #22452, .F. ) ;
#14919 = CYLINDRICAL_SURFACE ( 'NONE', #8832, 10.00000000000001066 ) ;
#14921 = CARTESIAN_POINT ( 'NONE',  ( 162.8789161433191452, 248.5324370884573568, 9.731756914259689140 ) ) ;
#14922 = DIRECTION ( 'NONE',  ( -0.8263106059122556912, -0.5632146860273805622, 0.000000000000000000 ) ) ;
#14923 = LINE ( 'NONE', #6835, #91039 ) ;
#14924 = CARTESIAN_POINT ( 'NONE',  ( 82.79116273540778081, 45.87476224633662980, -10.81090643298098897 ) ) ;
#14925 = CARTESIAN_POINT ( 'NONE',  ( 170.4549130973286140, 255.0430615571639521, 11.26541777191281568 ) ) ;
#14926 = CARTESIAN_POINT ( 'NONE',  ( 194.8368544504894828, 263.2804105082292381, -0.7921045588880984978 ) ) ;
#14927 = ORIENTED_EDGE ( 'NONE', *, *, #59618, .T. ) ;
#14928 = CARTESIAN_POINT ( 'NONE',  ( 182.9621872738214279, 272.0904772814410535, -16.05491882940554760 ) ) ;
#14929 = CARTESIAN_POINT ( 'NONE',  ( 72.21059398248078764, 63.10797502098981937, -13.93913043402019447 ) ) ;
#14930 = CARTESIAN_POINT ( 'NONE',  ( -40.42249077443059235, 27.53003111760058630, -10.00000000000000000 ) ) ;
#14931 = CARTESIAN_POINT ( 'NONE',  ( 5.488910272031021442, 160.6427522451417644, 1.119607411625061291E-15 ) ) ;
#14932 = CARTESIAN_POINT ( 'NONE',  ( 196.0902246659342154, 269.6848923550738846, -11.36688942032260385 ) ) ;
#14933 = CARTESIAN_POINT ( 'NONE',  ( 174.5432515410337544, 282.4104588529930311, -15.15290805577315680 ) ) ;
#14934 = DIRECTION ( 'NONE',  ( 0.000000000000000000, -0.000000000000000000, -1.000000000000000000 ) ) ;
#14935 = CARTESIAN_POINT ( 'NONE',  ( 86.48597344569623147, 44.64948832258973255, -6.340490538666154308 ) ) ;
#14936 = CARTESIAN_POINT ( 'NONE',  ( 72.82183928371372872, 70.95611737677427300, 7.748181657111714138 ) ) ;
#14938 = CARTESIAN_POINT ( 'NONE',  ( 76.20595068776574976, 65.19451524589622693, 14.14378227490007056 ) ) ;
#14937 = CARTESIAN_POINT ( 'NONE',  ( -6.509410329615746171, 176.2369531367911293, -4.594050593750048428 ) ) ;
#14939 = CARTESIAN_POINT ( 'NONE',  ( 197.3327212804159103, 267.5970440452412049, 9.861675131224707513 ) ) ;
#14940 = VERTEX_POINT ( 'NONE', #72732 ) ;
#14941 = ORIENTED_EDGE ( 'NONE', *, *, #87572, .F. ) ;
#14942 = CARTESIAN_POINT ( 'NONE',  ( 51.80235952159637236, 80.00000000000000000, 10.00000000000000178 ) ) ;
#14943 = ADVANCED_FACE ( 'NONE', ( #87966 ), #96046, .F. ) ;
#14944 = CARTESIAN_POINT ( 'NONE',  ( 67.37294101383669442, 67.25214370961325017, -8.602411162679397094 ) ) ;
#14945 = CARTESIAN_POINT ( 'NONE',  ( 85.87487879953339132, 42.95715103324309325, 1.964983386555947842 ) ) ;
#14946 = CARTESIAN_POINT ( 'NONE',  ( 163.1438579415164156, 248.0735444329312713, -11.47272517958888116 ) ) ;
#14947 =( BOUNDED_CURVE ( )  B_SPLINE_CURVE ( 2, ( #74144, #74649, #21420, #82274, #43707, #67008, #97933, #28508, #59389, #90365, #52306, #44692, #90869 ),
 .UNSPECIFIED., .F., .T. ) 
 B_SPLINE_CURVE_WITH_KNOTS ( ( 3, 2, 2, 2, 2, 2, 3 ),
 ( 0.7875000000000000888, 0.7900000000000000355, 0.7950000000000000400, 0.8000000000000000444, 0.8050000000000000488, 0.8100000000000000533, 0.8125000000000000000 ),
 .UNSPECIFIED. ) 
 CURVE ( )  GEOMETRIC_REPRESENTATION_ITEM ( )  RATIONAL_B_SPLINE_CURVE ( ( 0.9755282581475767101, 0.9755282581475772652, 1.000000000000000000, 0.9510565162951535312, 1.000000000000000000, 0.9510565162951535312, 1.000000000000000000, 0.9510565162951535312, 1.000000000000000000, 0.9510565162951535312, 1.000000000000000000, 0.9755282581475768211, 0.9755282581475768211 ) ) 
 REPRESENTATION_ITEM ( '' )  );
#14948 = DIRECTION ( 'NONE',  ( 1.000000000000000000, 0.000000000000000000, 0.000000000000000000 ) ) ;
#14949 = CARTESIAN_POINT ( 'NONE',  ( 153.6013573859479209, 279.1680573449844474, 3.826191094887242183 ) ) ;
#14950 = CARTESIAN_POINT ( 'NONE',  ( 13.49027706508988089, 190.8464784336661637, 1.353441290958777525E-15 ) ) ;
#14951 = CARTESIAN_POINT ( 'NONE',  ( 114.8970466070627907, 227.9548013555409796, -4.594050593750042211 ) ) ;
#14952 = CARTESIAN_POINT ( 'NONE',  ( 182.0607763290098262, 294.6140211400301610, -6.481743162254417712 ) ) ;
#14953 = CARTESIAN_POINT ( 'NONE',  ( 196.3249884498792994, 275.2518087180711177, 16.06659936265807431 ) ) ;
#14954 = CARTESIAN_POINT ( 'NONE',  ( 153.5230417281645714, 274.1903830991208793, -12.08502709614621651 ) ) ;
#14955 = EDGE_CURVE ( 'NONE', #38181, #24509, #4286, .T. ) ;
#14956 = B_SPLINE_CURVE_WITH_KNOTS ( 'NONE', 3,
 ( #69274, #84032, #61169, #76404, #61668, #92618, #22185, #15558, #68276, #75403, #77391, #7470, #75912, #38364, #53569, #45469, #6979, #37371, #30279, #52569, #67787, #99695, #14591, #84521, #15067, #45956, #76873, #5986, #83525, #23166, #36882, #98713, #30788, #99198, #29299, #54058, #60161, #85014, #21690, #14089, #44974, #29784, #6492, #60656, #91612, #53079, #36697, #66117, #36201, #66614 ),
 .UNSPECIFIED., .F., .F.,
 ( 4, 2, 2, 2, 2, 2, 2, 2, 2, 2, 2, 2, 2, 2, 2, 2, 2, 2, 2, 2, 2, 2, 2, 2, 4 ),
 ( 0.0003739468527002533975, 0.0008345414556833621964, 0.001064838757174917192, 0.001295136058666471971, 0.001410284709412328724, 0.001525433360158185044, 0.001640582010904041797, 0.001755730661649898116, 0.001986027963141681445, 0.002216325264633465207, 0.003137514470600615869, 0.004058703676567767399, 0.004979892882534918928, 0.005440487485518494259, 0.005670784787010286696, 0.005785933437756182914, 0.005843507763129083751, 0.005901082088501983722, 0.005958656413874884560, 0.006016230739247785397, 0.006131379389993588808, 0.006361676691485088075, 0.006822271294468086611, 0.007282865897451086881, 0.007743460500434085417 ),
 .UNSPECIFIED. ) ;
#14957 = B_SPLINE_CURVE_WITH_KNOTS ( 'NONE', 3,
 ( #68743, #23624, #54518, #99666, #85496, #30252, #92110, #53540, #16045, #46947, #61635, #85385, #53430, #38727, #46836, #92965, #84379, #31122, #76740, #37724, #100060, #44833, #76266, #15931, #13951, #91992, #69631, #7333, #90994, #5853, #54410, #23022, #92475, #75766, #30645, #77238, #61532, #53915, #60524, #36737, #6839, #52438, #91477, #22544, #240, #62013, #14452, #83386 ),
 .UNSPECIFIED., .F., .F.,
 ( 4, 2, 2, 2, 2, 2, 2, 2, 2, 2, 2, 2, 2, 2, 2, 2, 2, 2, 2, 2, 2, 2, 2, 4 ),
 ( 0.001525744563423052889, 0.001989215674126778178, 0.002452686784830503466, 0.002684422340182411430, 0.002800290117858385795, 0.002916157895534359727, 0.003032025673210333658, 0.003147893450886307155, 0.003379629006238109735, 0.003843100116941790354, 0.004306571227645470540, 0.005233513449052831779, 0.006160455670460193017, 0.006623926781163830269, 0.007087397891867466652, 0.007203265669543395047, 0.007261199558381358811, 0.007319133447219321707, 0.007550869002571125588, 0.007782604557922930336, 0.008014340113274735083, 0.008246075668626538097, 0.008477811223978342844, 0.008941282334681908972 ),
 .UNSPECIFIED. ) ;
#14958 = CARTESIAN_POINT ( 'NONE',  ( 125.6883311748214425, 231.8262482093457493, 3.021315404115420679E-15 ) ) ;
#14959 = CARTESIAN_POINT ( 'NONE',  ( 190.7350272470297341, 299.8690974414012089, -4.572277333844146696 ) ) ;
#14960 = CARTESIAN_POINT ( 'NONE',  ( -22.20871200244593879, 23.11170711957622004, 10.00000000000000000 ) ) ;
#14961 = CARTESIAN_POINT ( 'NONE',  ( 68.90560621877193626, 63.79076715805909004, -12.30144644517787711 ) ) ;
#14962 = CARTESIAN_POINT ( 'NONE',  ( 184.3272200602622775, 274.5360433806101241, 16.60951854980709541 ) ) ;
#14963 = CARTESIAN_POINT ( 'NONE',  ( 82.83468505418072425, 48.81772959092904784, 13.64447714929874067 ) ) ;
#14964 = CARTESIAN_POINT ( 'NONE',  ( 70.98683038387876820, 61.11472152276905234, -14.49225651734632692 ) ) ;
#14965 = CARTESIAN_POINT ( 'NONE',  ( 73.21854134910928735, 68.38249955197431973, 11.21855355596820480 ) ) ;
#14966 = CARTESIAN_POINT ( 'NONE',  ( 164.9407228494403057, 249.8614573468021547, -10.59005222520834621 ) ) ;
#14967 = DIRECTION ( 'NONE',  ( -0.000000000000000000, 0.000000000000000000, -1.000000000000000000 ) ) ;
#14968 = CARTESIAN_POINT ( 'NONE',  ( 72.06470348997973474, 72.25603645428110156, 1.367373202405273602 ) ) ;
#14969 = CARTESIAN_POINT ( 'NONE',  ( 43.53192288983094471, 62.93782412512172186, -10.00000000000000000 ) ) ;
#14970 = DIRECTION ( 'NONE',  ( 0.8660254037844387076, 0.4999999999999998890, 0.000000000000000000 ) ) ;
#14971 = ORIENTED_EDGE ( 'NONE', *, *, #87627, .F. ) ;
#14972 = CARTESIAN_POINT ( 'NONE',  ( 159.1344352748853055, 279.7114264697810313, -10.00621538743078354 ) ) ;
#14973 = DIRECTION ( 'NONE',  ( 0.4527707594502572985, 0.8916269620120498285, 0.000000000000000000 ) ) ;
#14974 = CARTESIAN_POINT ( 'NONE',  ( 99.20033616346982797, 218.8923013555410080, 4.594050593750050204 ) ) ;
#14975 = CARTESIAN_POINT ( 'NONE',  ( 14.33134397731654630, 13.98920272979924917, 7.433330006724137462 ) ) ;
#14976 = CARTESIAN_POINT ( 'NONE',  ( 77.18523492127140173, 59.47428895107222502, -16.40887739104300991 ) ) ;
#14977 = DIRECTION ( 'NONE',  ( -1.000000000000000000, 0.000000000000000000, 0.000000000000000000 ) ) ;
#14978 = AXIS2_PLACEMENT_3D ( 'NONE', #47021, #55597, #1932 ) ;
#14980 = CARTESIAN_POINT ( 'NONE',  ( 113.7185830531895903, 224.9155109091896634, 2.679491924311254714 ) ) ;
#14979 = LINE ( 'NONE', #91529, #58171 ) ;
#14981 = CARTESIAN_POINT ( 'NONE',  ( 196.7270510492836877, 289.9057476898814230, 17.95127088795220160 ) ) ;
#14982 = CARTESIAN_POINT ( 'NONE',  ( 190.9513712376748060, 261.2677970607517182, -4.679362068315001899 ) ) ;
#14983 = CARTESIAN_POINT ( 'NONE',  ( 196.5475899070771675, 290.2165835061676944, -17.89382743182097002 ) ) ;
#14984 = CARTESIAN_POINT ( 'NONE',  ( 36.18707552304946518, 42.93396525600392977, 2.839279412974139660 ) ) ;
#14985 = CARTESIAN_POINT ( 'NONE',  ( 192.4867975473904949, 297.2500821921321972, -13.04960750009181325 ) ) ;
#14986 = CARTESIAN_POINT ( 'NONE',  ( -38.35373792487678202, 26.90998726756845727, -10.00000000000000000 ) ) ;
#14987 = ORIENTED_EDGE ( 'NONE', *, *, #30883, .F. ) ;
#14988 = CARTESIAN_POINT ( 'NONE',  ( 28.23826220571969969, 31.70171378149920471, -9.188101187500004485 ) ) ;
#14989 = CARTESIAN_POINT ( 'NONE',  ( 179.0715434446022130, 280.8390982330867587, 16.22398002533389771 ) ) ;
#14990 = CARTESIAN_POINT ( 'NONE',  ( 197.1680355107441471, 268.3962010867043659, 9.346870724141478348 ) ) ;
#14991 = CARTESIAN_POINT ( 'NONE',  ( 196.4242782546697015, 290.4301655533025155, -16.42402868779123537 ) ) ;
#14992 = DIRECTION ( 'NONE',  ( 0.000000000000000000, 0.000000000000000000, 1.000000000000000000 ) ) ;
#14993 = CARTESIAN_POINT ( 'NONE',  ( 159.6419305724666344, 254.1390605605417079, 16.92015248457581933 ) ) ;
#14994 = CARTESIAN_POINT ( 'NONE',  ( 182.8336677718184546, 264.3499445543482693, -13.07731979293364866 ) ) ;
#14995 = CARTESIAN_POINT ( 'NONE',  ( 169.3689075499657122, 251.9910147621546344, -8.596408333947868741 ) ) ;
#14996 = CARTESIAN_POINT ( 'NONE',  ( -34.42581292930597670, 25.91608375674935161, -10.00000000000000000 ) ) ;
#14997 = ADVANCED_BREP_SHAPE_REPRESENTATION ( '', ( #46005, #68784 ), #2502 ) ;
#14998 = VERTEX_POINT ( 'NONE', #95560 ) ;
#14999 = CARTESIAN_POINT ( 'NONE',  ( 73.03785937943386841, 69.69865149502336976, 9.683281169778272357 ) ) ;
#15000 = CARTESIAN_POINT ( 'NONE',  ( 33.10965510200716722, 34.51421378149920827, -9.188101187500004485 ) ) ;
#15001 = EDGE_LOOP ( 'NONE', ( #41421, #29984, #28274, #83222 ) ) ;
#15002 = FACE_OUTER_BOUND ( 'NONE', #74541, .T. ) ;
#15003 = CARTESIAN_POINT ( 'NONE',  ( 87.27998730159347929, 43.91877473756031947, 2.943096442281895264 ) ) ;
#15004 = VERTEX_POINT ( 'NONE', #80343 ) ;
#15005 = CARTESIAN_POINT ( 'NONE',  ( 206.8217325168575371, 270.0045844243117017, 3.350393751014514532 ) ) ;
#15006 = CARTESIAN_POINT ( 'NONE',  ( 48.77433535142598231, 99.76555324011610537, -10.00000000000000000 ) ) ;
#15007 = CARTESIAN_POINT ( 'NONE',  ( 193.7694484332697016, 280.6102121743993507, -17.05218128339958383 ) ) ;
#15008 = CARTESIAN_POINT ( 'NONE',  ( 153.8558716659707954, 264.1608085621786586, -16.57261382954067130 ) ) ;
#15009 = CARTESIAN_POINT ( 'NONE',  ( 200.7694952279801157, 282.9040289856181403, -17.94628235092568502 ) ) ;
#15010 = EDGE_CURVE ( 'NONE', #75521, #61222, #64605, .T. ) ;
#15011 = CARTESIAN_POINT ( 'NONE',  ( 81.49256741308062146, 59.57505144466710334, 0.05226423163382182269 ) ) ;
#15012 = CARTESIAN_POINT ( 'NONE',  ( 81.30975366074838462, 56.24313983998633404, -16.44754541364716971 ) ) ;
#15013 = EDGE_CURVE ( 'NONE', #44296, #22415, #26106, .T. ) ;
#15014 = DIRECTION ( 'NONE',  ( 0.000000000000000000, 0.000000000000000000, 1.000000000000000000 ) ) ;
#15015 = ORIENTED_EDGE ( 'NONE', *, *, #98097, .F. ) ;
#15016 = CARTESIAN_POINT ( 'NONE',  ( 195.0619961850419486, 291.0373835071860640, 16.42391134123714380 ) ) ;
#15017 = ORIENTED_EDGE ( 'NONE', *, *, #11480, .T. ) ;
#15018 = ORIENTED_EDGE ( 'NONE', *, *, #9448, .F. ) ;
#15019 = CARTESIAN_POINT ( 'NONE',  ( 198.0204369024629045, 286.8851334562542092, 16.94118585317415082 ) ) ;
#15020 = CARTESIAN_POINT ( 'NONE',  ( -41.62359735524142934, 26.60228115600143184, 10.00000000000000000 ) ) ;
#15022 = CARTESIAN_POINT ( 'NONE',  ( 165.6600941239869087, 274.7658140146604637, -15.24034129512801528 ) ) ;
#15021 = DIRECTION ( 'NONE',  ( 0.8845109580947929651, -0.1124011590738235450, 0.4527762631246172731 ) ) ;
#15023 = CARTESIAN_POINT ( 'NONE',  ( 164.9825360643182535, 244.8888605054729624, -1.157747536866345461 ) ) ;
#15024 = CARTESIAN_POINT ( 'NONE',  ( 197.4084121877038172, 273.1799603734787638, -13.34748769055383200 ) ) ;
#15025 = CARTESIAN_POINT ( 'NONE',  ( 77.10851993703164453, 59.99585613907493098, -15.93770053271873621 ) ) ;
#15026 = CARTESIAN_POINT ( 'NONE',  ( 82.42863484518792916, 40.95299279291557326, 1.014380864406314808 ) ) ;
#15028 = EDGE_CURVE ( 'NONE', #76220, #61239, #86804, .T. ) ;
#15027 = CARTESIAN_POINT ( 'NONE',  ( 171.3928239984006723, 250.3015599828365509, -5.796133048607560845 ) ) ;
#15029 = CARTESIAN_POINT ( 'NONE',  ( 77.05758262809833070, 63.67252911167651774, -14.99652361060851646 ) ) ;
#15030 = CARTESIAN_POINT ( 'NONE',  ( 183.4471554107105931, 284.5186797981741620, -15.10776214044594745 ) ) ;
#15031 = CARTESIAN_POINT ( 'NONE',  ( 114.1117772151768577, 242.8149278399161233, -9.188101187500095079 ) ) ;
#15032 = VERTEX_POINT ( 'NONE', #96537 ) ;
#15033 = CARTESIAN_POINT ( 'NONE',  ( 183.4504012090349931, 260.3740723431718607, -9.329707687019228146 ) ) ;
#15034 = CARTESIAN_POINT ( 'NONE',  ( 35.45274159363147959, 38.65586893147759184, -7.433330006724137462 ) ) ;
#15035 = CARTESIAN_POINT ( 'NONE',  ( 188.3932030005877323, 273.5611838242375597, 15.65614328840583092 ) ) ;
#15036 = ORIENTED_EDGE ( 'NONE', *, *, #73888, .T. ) ;
#15037 = AXIS2_PLACEMENT_3D ( 'NONE', #48522, #2945, #34310 ) ;
#15038 = VERTEX_POINT ( 'NONE', #27108 ) ;
#15039 = CARTESIAN_POINT ( 'NONE',  ( 162.8643913348946342, 249.0653215557598799, -10.24700337220267166 ) ) ;
#15040 = CARTESIAN_POINT ( 'NONE',  ( 121.7448624948184204, 229.5494855054051584, -2.679491924311248496 ) ) ;
#15041 = DIRECTION ( 'NONE',  ( 0.000000000000000000, 0.6788029332000655724, -0.7343204871709539949 ) ) ;
#15042 = CARTESIAN_POINT ( 'NONE',  ( 147.4451090059320109, 275.2645752046312850, 3.125785074907880823 ) ) ;
#15043 = CARTESIAN_POINT ( 'NONE',  ( 206.0946696452135427, 273.6805563358039421, -10.19627505985792837 ) ) ;
#15044 = CARTESIAN_POINT ( 'NONE',  ( 13.35896364390118052, 31.21091486745859811, -1.111400068045478839E-16 ) ) ;
#15045 = EDGE_CURVE ( 'NONE', #49678, #16991, #32381, .T. ) ;
#15046 = ORIENTED_EDGE ( 'NONE', *, *, #7153, .T. ) ;
#15047 = CARTESIAN_POINT ( 'NONE',  ( 195.1394560277449841, 292.6555429290298207, 16.72738487262295948 ) ) ;
#15048 = ORIENTED_EDGE ( 'NONE', *, *, #90256, .F. ) ;
#15049 = LINE ( 'NONE', #89269, #55849 ) ;
#15050 = DIRECTION ( 'NONE',  ( -0.8660254037844399289, -0.4999999999999976130, 0.000000000000000000 ) ) ;
#15051 = ORIENTED_EDGE ( 'NONE', *, *, #60788, .F. ) ;
#15052 = CARTESIAN_POINT ( 'NONE',  ( 191.7251117466753101, 267.4289849328922628, -12.63340514153103200 ) ) ;
#15053 = AXIS2_PLACEMENT_3D ( 'NONE', #56101, #23209, #17113 ) ;
#15054 = CARTESIAN_POINT ( 'NONE',  ( 152.0354063984034951, 267.3139468990199816, -16.99296076417658341 ) ) ;
#15055 = CARTESIAN_POINT ( 'NONE',  ( 158.4595209236517519, 263.4143799451769041, 17.55458220974047379 ) ) ;
#15056 = CARTESIAN_POINT ( 'NONE',  ( 168.5910505471324257, 286.4687829538495976, 8.106709794022206594 ) ) ;
#15058 = CARTESIAN_POINT ( 'NONE',  ( 157.1870951989065190, 280.8757593961267389, 6.041051901132188817 ) ) ;
#15057 = CARTESIAN_POINT ( 'NONE',  ( 184.3873580908706913, 288.5454924782333705, -13.82082247699642430 ) ) ;
#15059 = CARTESIAN_POINT ( 'NONE',  ( 153.4542976351440302, 264.8563551865710224, -17.11782692037292009 ) ) ;
#15060 = ORIENTED_EDGE ( 'NONE', *, *, #9254, .T. ) ;
#15061 = CARTESIAN_POINT ( 'NONE',  ( 190.4240181651484818, 300.8229208869809668, -4.214281362166949485 ) ) ;
#15063 = CARTESIAN_POINT ( 'NONE',  ( 72.35643307556982506, 65.56020265574198902, 12.51768452229861772 ) ) ;
#15062 = B_SPLINE_SURFACE_WITH_KNOTS ( 'NONE', 3, 1, ( 
 ( #89912, #91399 ),
 ( #5280, #59951 ),
 ( #52359, #90426 ),
 ( #74701, #36159 ),
 ( #28564, #35672 ),
 ( #83307, #84308 ),
 ( #67063, #97986 ),
 ( #68557, #37163 ),
 ( #28068, #13386 ),
 ( #20492, #91908 ),
 ( #13868, #44748 ),
 ( #52857, #68062 ),
 ( #21964, #82332 ),
 ( #51363, #76193 ),
 ( #98985, #83808 ),
 ( #29569, #60444 ),
 ( #22464, #14372 ),
 ( #45258, #6768 ),
 ( #37646, #99483 ),
 ( #30058, #1169 ),
 ( #17354, #69559 ),
 ( #8269, #15340 ),
 ( #55828, #46235 ),
 ( #63461, #46758 ),
 ( #92403, #62435 ),
 ( #71079, #7761 ),
 ( #165, #76665 ),
 ( #86822, #70047 ),
 ( #77160, #1680 ),
 ( #38655, #92891 ),
 ( #77686, #8760 ) ),
 .UNSPECIFIED., .F., .F., .F.,
 ( 4, 3, 3, 3, 3, 3, 3, 3, 3, 3, 4 ),
 ( 2, 2 ),
 ( 0.000000000000000000, 0.1122669598086808440, 0.2243161639709783939, 0.3396355846219274444, 0.4553962076585297836, 0.5677860799922560542, 0.6749047109689785273, 0.7773884377078629226, 0.8775581155834549785, 0.9782364162378116568, 1.000000000000000000 ),
 ( 0.000000000000000000, 1.000000000000000000 ),
 .UNSPECIFIED. ) ;
#15064 = EDGE_CURVE ( 'NONE', #1376, #77230, #88973, .T. ) ;
#15065 = CARTESIAN_POINT ( 'NONE',  ( 82.07581200760314744, 41.13792279056817591, -3.429577836730589802 ) ) ;
#15066 = CYLINDRICAL_SURFACE ( 'NONE', #14093, 10.00000000000010658 ) ;
#15067 = CARTESIAN_POINT ( 'NONE',  ( 190.0718168876597076, 270.6242987759774223, -14.12311039011201785 ) ) ;
#15068 = DIRECTION ( 'NONE',  ( 0.000000000000000000, 0.000000000000000000, 1.000000000000000000 ) ) ;
#15069 = FACE_OUTER_BOUND ( 'NONE', #66109, .T. ) ;
#15070 = CARTESIAN_POINT ( 'NONE',  ( 35.94413697178374889, 184.8927522451418213, 10.00000000000009948 ) ) ;
#15071 = EDGE_CURVE ( 'NONE', #68127, #14885, #20369, .T. ) ;
#15072 = CARTESIAN_POINT ( 'NONE',  ( 191.3337820289262936, 282.9518992253598526, -16.81566807114812789 ) ) ;
#15073 = CARTESIAN_POINT ( 'NONE',  ( 73.92817530304030527, 65.74941589806995523, -13.53337586798867065 ) ) ;
#15074 = CARTESIAN_POINT ( 'NONE',  ( 75.49289073487081225, 205.2048013555409796, 4.594050593750051981 ) ) ;
#15075 = DIRECTION ( 'NONE',  ( -0.4527707594502665689, -0.8916269620120450545, 0.000000000000000000 ) ) ;
#15076 = CARTESIAN_POINT ( 'NONE',  ( 193.0761489135300906, 296.2292956824684893, -11.99675185248219655 ) ) ;
#15077 = CARTESIAN_POINT ( 'NONE',  ( 208.3699316049496133, 269.7396870210121733, -1.898463622294385811 ) ) ;
#15078 = DIRECTION ( 'NONE',  ( -0.000000000000000000, -0.000000000000000000, 1.000000000000000000 ) ) ;
#15079 = EDGE_CURVE ( 'NONE', #78966, #84837, #28582, .T. ) ;
#15080 = CARTESIAN_POINT ( 'NONE',  ( 161.6127771116929921, 250.7254542206800352, -12.96229604595372464 ) ) ;
#15081 = CARTESIAN_POINT ( 'NONE',  ( -22.42236680055709641, 157.8615022471902591, 0.000000000000000000 ) ) ;
#15083 = CARTESIAN_POINT ( 'NONE',  ( 75.88740524811866806, 51.50386128526941576, 15.70536156696038965 ) ) ;
#15082 = CARTESIAN_POINT ( 'NONE',  ( 73.24862708662814725, 69.62355710376385787, -9.916407523326116191 ) ) ;
#15084 = EDGE_CURVE ( 'NONE', #86525, #99556, #19130, .T. ) ;
#15085 = DIRECTION ( 'NONE',  ( 0.000000000000000000, -0.000000000000000000, 1.000000000000000000 ) ) ;
#15086 = CARTESIAN_POINT ( 'NONE',  ( 164.5204976463763558, 245.6891345203973174, -4.279147110458541903 ) ) ;
#15087 = CARTESIAN_POINT ( 'NONE',  ( 196.3341081413628899, 290.5863447708742342, 16.12390540996472410 ) ) ;
#15088 = CARTESIAN_POINT ( 'NONE',  ( 71.74723311883084875, 72.17470677413867008, 3.272391839458893781 ) ) ;
#15089 = CARTESIAN_POINT ( 'NONE',  ( 25.77753312492912841, 179.5643266524160140, -9.188101187500093303 ) ) ;
#15090 = CARTESIAN_POINT ( 'NONE',  ( 47.26526781268299260, 210.3464784336661637, 1.353441290958777327E-15 ) ) ;
#15091 = CARTESIAN_POINT ( 'NONE',  ( 157.7529601300917363, 257.4108533407307959, 16.91445305439664892 ) ) ;
#15092 = CARTESIAN_POINT ( 'NONE',  ( 49.28760614098965220, 105.1966139777580338, -10.00000000000000000 ) ) ;
#15093 = CARTESIAN_POINT ( 'NONE',  ( 165.0642700556339264, 248.7133924234977371, -9.523431784498571417 ) ) ;
#15094 = CARTESIAN_POINT ( 'NONE',  ( -8.493791556357338735, 159.2365022471901739, -10.00000000000009059 ) ) ;
#15095 = DIRECTION ( 'NONE',  ( 0.4999999999999998890, -0.8660254037844385966, 0.000000000000000000 ) ) ;
#15096 = CARTESIAN_POINT ( 'NONE',  ( 24.28581821943125263, 16.94754757982089544, 5.678558825948272215 ) ) ;
#15097 = CARTESIAN_POINT ( 'NONE',  ( -4.331504796628791176, 156.7592609112379876, 2.679491924311251605 ) ) ;
#15098 = CARTESIAN_POINT ( 'NONE',  ( -17.22621437785049636, 170.8615022471903160, 5.000000000000046185 ) ) ;
#15099 = CARTESIAN_POINT ( 'NONE',  ( 13.18987451683679524, 19.56628583063839244, 9.188101187500006262 ) ) ;
#15100 = CARTESIAN_POINT ( 'NONE',  ( 55.22204975783502334, 208.8149278399160664, 9.188101187500093303 ) ) ;
#15101 = CARTESIAN_POINT ( 'NONE',  ( 175.5847330776380204, 258.8848994771980188, -13.61208222109076615 ) ) ;
#15102 = CARTESIAN_POINT ( 'NONE',  ( 75.58789875694216676, 56.96802034365616407, 16.56515463127572119 ) ) ;
#15103 = CARTESIAN_POINT ( 'NONE',  ( 159.9014600375868440, 253.6895423408921886, 15.57825579621527368 ) ) ;
#15104 = CARTESIAN_POINT ( 'NONE',  ( 72.81957114983744361, 62.23005867720106465, 14.49872350333313697 ) ) ;
#15105 = CARTESIAN_POINT ( 'NONE',  ( 201.5827075904949766, 281.4955038563991252, 16.28834193516912165 ) ) ;
#15106 = CARTESIAN_POINT ( 'NONE',  ( 79.13150298882169409, 55.44825781748590288, -16.08240833089401534 ) ) ;
#15107 = CARTESIAN_POINT ( 'NONE',  ( 116.1416978049531110, 237.8615022471902307, -10.00000000000009592 ) ) ;
#15108 = CARTESIAN_POINT ( 'NONE',  ( 200.5810378487751393, 283.2304467414622877, 18.38516374632547112 ) ) ;
#15109 = CARTESIAN_POINT ( 'NONE',  ( 165.1536807772045279, 269.6115192885357033, -16.29157638650531226 ) ) ;
#15110 = ORIENTED_EDGE ( 'NONE', *, *, #20664, .F. ) ;
#15111 = CARTESIAN_POINT ( 'NONE',  ( 76.91885953472434778, 49.85770563519495369, 15.12061930091973849 ) ) ;
#15112 = ORIENTED_EDGE ( 'NONE', *, *, #549, .F. ) ;
#15113 = CARTESIAN_POINT ( 'NONE',  ( 206.6703863510205679, 272.6833857505801006, -10.72500664779635393 ) ) ;
#15114 = CARTESIAN_POINT ( 'NONE',  ( 188.9750831269214757, 277.9074358098590096, -16.52746066141228809 ) ) ;
#15115 = CARTESIAN_POINT ( 'NONE',  ( 170.3489334754653441, 276.6636095645281443, 16.60343083925547347 ) ) ;
#15116 = VERTEX_POINT ( 'NONE', #58957 ) ;
#15118 = ORIENTED_EDGE ( 'NONE', *, *, #30523, .F. ) ;
#15117 = AXIS2_PLACEMENT_3D ( 'NONE', #59830, #48, #44124 ) ;
#15119 = CARTESIAN_POINT ( 'NONE',  ( 79.09330386122300638, 46.17864056469723977, -12.73155772710657452 ) ) ;
#15120 = CARTESIAN_POINT ( 'NONE',  ( 194.2154056360670040, 294.2560451561701029, -15.66696967429384557 ) ) ;
#15121 = CARTESIAN_POINT ( 'NONE',  ( 177.1487090986248063, 274.7577274326447991, -16.88435297823402337 ) ) ;
#15122 = EDGE_LOOP ( 'NONE', ( #95573, #82669, #4592, #37798 ) ) ;
#15123 = CARTESIAN_POINT ( 'NONE',  ( 24.30746885452586525, 16.96004757982090183, -5.678558825948275768 ) ) ;
#15124 = CARTESIAN_POINT ( 'NONE',  ( 75.59055352145890083, 57.67694070126884753, 16.07306487193169531 ) ) ;
#15125 = DIRECTION ( 'NONE',  ( -0.2270762630343793331, 0.9738769792773321887, 0.000000000000000000 ) ) ;
#15126 = LINE ( 'NONE', #75983, #3575 ) ;
#15127 = ORIENTED_EDGE ( 'NONE', *, *, #39516, .T. ) ;
#15128 = CARTESIAN_POINT ( 'NONE',  ( 141.1607630391569330, 240.7592609112380160, 2.679491924311254714 ) ) ;
#15129 = FACE_OUTER_BOUND ( 'NONE', #80493, .T. ) ;
#15130 = ORIENTED_EDGE ( 'NONE', *, *, #84448, .T. ) ;
#15131 = DIRECTION ( 'NONE',  ( 1.000000000000000000, 0.000000000000000000, 0.000000000000000000 ) ) ;
#15133 = CARTESIAN_POINT ( 'NONE',  ( 67.70227059457259600, 65.68093037200397077, -10.72427208149578881 ) ) ;
#15132 = CARTESIAN_POINT ( 'NONE',  ( 24.08514838022782811, 55.05848426107617399, 59.99999999999999289 ) ) ;
#15134 = CARTESIAN_POINT ( 'NONE',  ( 162.6262389125959373, 248.9700868899859074, -10.50380342094597808 ) ) ;
#15135 = CARTESIAN_POINT ( 'NONE',  ( 163.7064929935861244, 247.0990319366274548, 6.401263337036986023 ) ) ;
#15136 = CARTESIAN_POINT ( 'NONE',  ( 188.6905595153717741, 295.3522105695485607, -11.31054681824411290 ) ) ;
#15137 = CARTESIAN_POINT ( 'NONE',  ( 161.7922706396030605, 263.4318561585560587, -17.02534324577779401 ) ) ;
#15139 = EDGE_CURVE ( 'NONE', #94007, #97001, #89929, .T. ) ;
#15138 = CARTESIAN_POINT ( 'NONE',  ( 142.3122500695552048, 240.7202760586659736, -5.415160957724236172E-17 ) ) ;
#15140 = CARTESIAN_POINT ( 'NONE',  ( 176.7284915028678824, 269.1415778121231597, 16.10409147245672301 ) ) ;
#15141 = CARTESIAN_POINT ( 'NONE',  ( 195.8006847607455825, 290.9998369522246549, -15.91509253693118531 ) ) ;
#15142 = CARTESIAN_POINT ( 'NONE',  ( 64.74832919946385346, 214.3149278399160949, -9.188101187500095079 ) ) ;
#15144 = ORIENTED_EDGE ( 'NONE', *, *, #60920, .F. ) ;
#15143 = B_SPLINE_CURVE_WITH_KNOTS ( 'NONE', 3,
 ( #46986, #78912, #63684, #64184 ),
 .UNSPECIFIED., .F., .F.,
 ( 4, 4 ),
 ( 0.000000000000000000, 0.003498996904287751328 ),
 .UNSPECIFIED. ) ;
#15145 = DIRECTION ( 'NONE',  ( 0.000000000000000000, 0.000000000000000000, 1.000000000000000000 ) ) ;
#15146 = DIRECTION ( 'NONE',  ( -0.8660254037844387076, -0.4999999999999998890, -0.000000000000000000 ) ) ;
#15147 = CARTESIAN_POINT ( 'NONE',  ( 205.1956247482881110, 271.9973608250444954, 9.678236287800089599 ) ) ;
#15148 = ORIENTED_EDGE ( 'NONE', *, *, #95793, .F. ) ;
#15149 = CARTESIAN_POINT ( 'NONE',  ( 168.0439751434946629, 261.0016734627291726, -16.81520615430363108 ) ) ;
#15150 = VERTEX_POINT ( 'NONE', #67579 ) ;
#15151 = ORIENTED_EDGE ( 'NONE', *, *, #68316, .F. ) ;
#15152 = FACE_BOUND ( 'NONE', #70336, .T. ) ;
#15153 = CARTESIAN_POINT ( 'NONE',  ( 67.06310037049678385, 67.63674953590368943, 6.653793825411979945 ) ) ;
#15154 = CARTESIAN_POINT ( 'NONE',  ( 197.5324136461498767, 286.6052654224091611, 16.91853012670608791 ) ) ;
#15155 = EDGE_CURVE ( 'NONE', #90942, #83096, #76208, .T. ) ;
#15156 = CARTESIAN_POINT ( 'NONE',  ( 82.20453289287176801, 41.97260302554307287, -6.936896895868616575 ) ) ;
#15157 = CARTESIAN_POINT ( 'NONE',  ( 81.35074466249913883, 55.80872010294902452, 16.38725056492407361 ) ) ;
#15158 = CARTESIAN_POINT ( 'NONE',  ( 193.7261517370125432, 295.1034577671335342, 14.97744313279139661 ) ) ;
#15159 = DIRECTION ( 'NONE',  ( -0.9607486656258008573, -0.2774202615135435979, 0.000000000000000000 ) ) ;
#15160 = EDGE_CURVE ( 'NONE', #81343, #94798, #79621, .T. ) ;
#15161 = CARTESIAN_POINT ( 'NONE',  ( 74.35571174875622091, 222.9244531367911293, -4.594050593750046652 ) ) ;
#15162 = ORIENTED_EDGE ( 'NONE', *, *, #99895, .F. ) ;
#15163 = CARTESIAN_POINT ( 'NONE',  ( 24.82038151633537026, 14.73415679381822230, 1.333680081654574804E-15 ) ) ;
#15164 = CARTESIAN_POINT ( 'NONE',  ( 200.4026220252542032, 283.5394720126751622, -17.02811402915289918 ) ) ;
#15165 = EDGE_LOOP ( 'NONE', ( #95589, #17480, #98037, #15341 ) ) ;
#15166 = CARTESIAN_POINT ( 'NONE',  ( 76.09110705058404278, 51.50373584443451591, -16.16844731949881719 ) ) ;
#15167 = LINE ( 'NONE', #76979, #36853 ) ;
#15168 = CARTESIAN_POINT ( 'NONE',  ( 165.2054706378175126, 285.1533889500111627, 0.5060398096789098243 ) ) ;
#15169 = LINE ( 'NONE', #494, #60658 ) ;
#15170 = CARTESIAN_POINT ( 'NONE',  ( 34.97213163436671124, 51.32435524152969464, 10.00000000000000000 ) ) ;
#15171 = VERTEX_POINT ( 'NONE', #82836 ) ;
#15172 = CARTESIAN_POINT ( 'NONE',  ( 84.75572546936606955, 43.74292620480390781, -6.422790150011197241 ) ) ;
#15173 = CARTESIAN_POINT ( 'NONE',  ( 156.6685347489093090, 274.1288574488814902, 13.57745094969755328 ) ) ;
#15174 = CARTESIAN_POINT ( 'NONE',  ( 178.0315741628076012, 287.5935043698759728, -13.06113257055532451 ) ) ;
#15175 = CARTESIAN_POINT ( 'NONE',  ( 153.4361244163197000, 264.8878321249116539, -17.23169627811277493 ) ) ;
#15176 = CARTESIAN_POINT ( 'NONE',  ( 72.65255621578388912, 70.92891038547531934, 7.631180297043458793 ) ) ;
#15177 = AXIS2_PLACEMENT_3D ( 'NONE', #21755, #36953, #83098 ) ;
#15178 = CARTESIAN_POINT ( 'NONE',  ( 72.23816834301878487, 67.09684945540639944, -11.28492405425373768 ) ) ;
#15179 = ORIENTED_EDGE ( 'NONE', *, *, #91860, .F. ) ;
#15180 = CARTESIAN_POINT ( 'NONE',  ( 196.2350291401047571, 264.4780031501763347, 5.359379669934941859 ) ) ;
#15181 = EDGE_CURVE ( 'NONE', #72513, #2782, #74761, .T. ) ;
#15182 = CARTESIAN_POINT ( 'NONE',  ( 82.20432729060250665, 218.2677522451418497, 10.00000000000009592 ) ) ;
#15183 = CARTESIAN_POINT ( 'NONE',  ( 191.2190380946134951, 260.9445496458436651, 3.106810577783889915 ) ) ;
#15184 = CARTESIAN_POINT ( 'NONE',  ( 81.39610991623023040, 53.46539056111136290, 15.50635795318955701 ) ) ;
#15185 = CARTESIAN_POINT ( 'NONE',  ( 84.06604358195920668, 51.46910565605918464, 14.65639964578790888 ) ) ;
#15186 = CARTESIAN_POINT ( 'NONE',  ( 198.9686279331660899, 265.4156631160248025, 0.08760027866574053579 ) ) ;
#15187 = ORIENTED_EDGE ( 'NONE', *, *, #99295, .T. ) ;
#15188 = AXIS2_PLACEMENT_3D ( 'NONE', #100020, #67603, #68598 ) ;
#15189 = CARTESIAN_POINT ( 'NONE',  ( 190.3625087333586521, 300.9294583479858147, -4.271886578030237303 ) ) ;
#15190 = EDGE_CURVE ( 'NONE', #73044, #3083, #88070, .T. ) ;
#15191 = CARTESIAN_POINT ( 'NONE',  ( -13.95037114427627500, 103.3647202663174056, 44.05931802377998707 ) ) ;
#15192 = EDGE_CURVE ( 'NONE', #66165, #15491, #47454, .T. ) ;
#15193 = CARTESIAN_POINT ( 'NONE',  ( 82.47021907082941539, 53.30441442868470858, -15.33472904691311456 ) ) ;
#15195 = CARTESIAN_POINT ( 'NONE',  ( 73.90603277580463271, 55.10673587672410889, 16.60184368115057651 ) ) ;
#15194 = DIRECTION ( 'NONE',  ( 0.3535533905932665699, -0.6123724356957869208, -0.7071067811865576758 ) ) ;
#15196 = EDGE_CURVE ( 'NONE', #6903, #23257, #78298, .T. ) ;
#15197 = EDGE_CURVE ( 'NONE', #71865, #23641, #42599, .T. ) ;
#15198 = CARTESIAN_POINT ( 'NONE',  ( 23.71749583336532297, 25.64441083166261492, -10.00000000000000533 ) ) ;
#15199 = CARTESIAN_POINT ( 'NONE',  ( 26.41785753015494009, 179.3927522451418213, -10.00000000000009237 ) ) ;
#15200 = CARTESIAN_POINT ( 'NONE',  ( 163.7895146392965842, 284.0257305568636070, -3.118330620146652077 ) ) ;
#15201 = DIRECTION ( 'NONE',  ( 0.000000000000000000, -0.000000000000000000, -1.000000000000000000 ) ) ;
#15202 = CARTESIAN_POINT ( 'NONE',  ( 159.2876523829509665, 254.7526883847961017, 15.64395448151312351 ) ) ;
#15203 = CARTESIAN_POINT ( 'NONE',  ( -7.320788502016136512, 157.3923013555410080, 4.594050593750050204 ) ) ;
#15204 = CARTESIAN_POINT ( 'NONE',  ( 189.0622672619279001, 295.6589450522362199, -11.52442905864715250 ) ) ;
#15205 = VERTEX_POINT ( 'NONE', #61955 ) ;
#15206 = B_SPLINE_CURVE_WITH_KNOTS ( 'NONE', 3,
 ( #98994, #60959, #99492, #38146, #61462, #21007, #59454, #52866, #83817, #76676 ),
 .UNSPECIFIED., .F., .F.,
 ( 4, 2, 2, 2, 4 ),
 ( 0.000000000000000000, 0.2500000000000000000, 0.5000000000000000000, 0.7500000000000000000, 1.000000000000000000 ),
 .UNSPECIFIED. ) ;
#15207 = CARTESIAN_POINT ( 'NONE',  ( 178.8238403317331233, 256.6237485836615519, 8.676301928053684165 ) ) ;
#15208 = CARTESIAN_POINT ( 'NONE',  ( 72.44129552685038220, 70.67501955208014408, -7.848061272651219333 ) ) ;
#15209 = CARTESIAN_POINT ( 'NONE',  ( -17.43550054826663498, 104.2312461070085021, 44.57229221387615326 ) ) ;
#15210 = CARTESIAN_POINT ( 'NONE',  ( 9.512059640396367755, 185.4869531367911293, 4.594050593750046652 ) ) ;
#15211 = CARTESIAN_POINT ( 'NONE',  ( 176.1988396708435687, 265.5930599550684406, -16.16477898283384107 ) ) ;
#15212 = CARTESIAN_POINT ( 'NONE',  ( 179.8452673937777320, 274.4601373947340335, -16.56085817225330103 ) ) ;
#15213 = CARTESIAN_POINT ( 'NONE',  ( 26.07214984898741150, 33.79103043416550634, 8.090169943749478065 ) ) ;
#15214 = CARTESIAN_POINT ( 'NONE',  ( 187.1412927779018673, 261.9835105880691231, -10.20549468610707322 ) ) ;
#15215 = CARTESIAN_POINT ( 'NONE',  ( 173.2317256228830047, 272.4512950130714444, -16.36800549663501769 ) ) ;
#15216 = PLANE ( 'NONE',  #52303 ) ;
#15217 = CARTESIAN_POINT ( 'NONE',  ( 175.6012255355377931, 253.3303057574685226, -3.452269288186304408 ) ) ;
#15218 = LINE ( 'NONE', #46113, #11275 ) ;
#15219 = CARTESIAN_POINT ( 'NONE',  ( 183.0280766574859399, 295.8866060358298569, 1.576309391735440046 ) ) ;
#15220 = CARTESIAN_POINT ( 'NONE',  ( 73.27344031762339682, 213.1115022471902591, 10.00000000000009592 ) ) ;
#15221 = CARTESIAN_POINT ( 'NONE',  ( 34.14357333472769085, 43.21091486745863364, 7.012934429366973338E-14 ) ) ;
#15222 = CARTESIAN_POINT ( 'NONE',  ( 189.8171280724701546, 301.8740853621098950, -0.4360232994423257624 ) ) ;
#15223 = CARTESIAN_POINT ( 'NONE',  ( 28.72751893051112049, 178.2048013555409796, 4.594050593750051981 ) ) ;
#15224 = CARTESIAN_POINT ( 'NONE',  ( 66.93805147409950962, 68.00539448811831278, 6.966594628907381903 ) ) ;
#15225 = ADVANCED_FACE ( 'NONE', ( #7271 ), #88701, .T. ) ;
#15226 = SURFACE_STYLE_USAGE ( .BOTH. , #39517 ) ;
#15227 = CARTESIAN_POINT ( 'NONE',  ( 205.5636066921878466, 271.2094078441786564, -6.548282385051860999 ) ) ;
#15228 = CARTESIAN_POINT ( 'NONE',  ( 199.0773057068961123, 285.8349872121713702, -17.17316764978006560 ) ) ;
#15229 = CARTESIAN_POINT ( 'NONE',  ( 165.0156970625405108, 244.8314239717225007, -1.890480716182876719 ) ) ;
#15230 = CARTESIAN_POINT ( 'NONE',  ( 187.4731087846878381, 267.6488792197166617, 13.31701845521303618 ) ) ;
#15231 = CARTESIAN_POINT ( 'NONE',  ( 202.8814167162130673, 278.7900253483502411, -15.09576271200930719 ) ) ;
#15232 = CARTESIAN_POINT ( 'NONE',  ( 163.7573486046460971, 281.3881871899058638, 8.856914258957445441 ) ) ;
#15233 = APPLICATION_PROTOCOL_DEFINITION ( 'draft international standard', 'automotive_design', 1998, #62128 ) ;
#15234 = CARTESIAN_POINT ( 'NONE',  ( 18.13223351794271565, 28.65586893147756342, -7.433330006724137462 ) ) ;
#15235 = CARTESIAN_POINT ( 'NONE',  ( 190.0515794655415789, 301.4680036374047063, -1.296825456579539626 ) ) ;
#15236 = CARTESIAN_POINT ( 'NONE',  ( 194.5051734451974426, 293.7541525883582381, 14.61790433731063921 ) ) ;
#15237 = ORIENTED_EDGE ( 'NONE', *, *, #12227, .T. ) ;
#15238 = CARTESIAN_POINT ( 'NONE',  ( 166.5497620933320775, 284.9599651698292178, -8.643830016708903941 ) ) ;
#15239 = DIRECTION ( 'NONE',  ( 0.1548189829846108034, -0.9879428538673736826, 0.000000000000000000 ) ) ;
#15240 = CARTESIAN_POINT ( 'NONE',  ( 81.62555094951984813, 42.60298488570899877, 7.525266644112702075 ) ) ;
#15241 = CARTESIAN_POINT ( 'NONE',  ( 41.25821923120311396, 128.0827283385945918, 10.00000000000000000 ) ) ;
#15242 = ORIENTED_EDGE ( 'NONE', *, *, #95173, .F. ) ;
#15244 = DIRECTION ( 'NONE',  ( 0.2237140788069379993, 0.9746548163034761680, 0.000000000000000000 ) ) ;
#15243 =( BOUNDED_CURVE ( )  B_SPLINE_CURVE ( 2, ( #14506, #23080, #7907, #77816, #15993, #69688, #22598, #76794, #293 ),
 .UNSPECIFIED., .F., .T. ) 
 B_SPLINE_CURVE_WITH_KNOTS ( ( 3, 2, 2, 2, 3 ),
 ( 0.9637096774193548709, 0.9650537634408602461, 0.9677419354838709964, 0.9704301075268817467, 0.9717741935483871218 ),
 .UNSPECIFIED. ) 
 CURVE ( )  GEOMETRIC_REPRESENTATION_ITEM ( )  RATIONAL_B_SPLINE_CURVE ( ( 0.9330127018922194093, 0.9330127018922194093, 1.000000000000000000, 0.8660254037844387076, 1.000000000000000000, 0.8660254037844387076, 1.000000000000000000, 0.9330127018922194093, 0.9330127018922194093 ) ) 
 REPRESENTATION_ITEM ( '' )  );
#15245 = CARTESIAN_POINT ( 'NONE',  ( 71.12243608386381766, 71.25991561840170618, -3.643341247755859325 ) ) ;
#15246 = CARTESIAN_POINT ( 'NONE',  ( 76.93391092271131981, 63.83843569504302451, 14.92315812435476019 ) ) ;
#15247 = CARTESIAN_POINT ( 'NONE',  ( 180.8079597460555306, 256.9122500747120057, -7.784400698518015638 ) ) ;
#15248 = CIRCLE ( 'NONE', #52436, 0.1418229129681591871 ) ;
#15249 = ORIENTED_EDGE ( 'NONE', *, *, #63976, .F. ) ;
#15251 = LINE ( 'NONE', #1594, #13558 ) ;
#15250 = CARTESIAN_POINT ( 'NONE',  ( -19.65312891409030271, 93.06504152958497400, 10.00000000000000888 ) ) ;
#15252 = ORIENTED_EDGE ( 'NONE', *, *, #19172, .T. ) ;
#15253 = CARTESIAN_POINT ( 'NONE',  ( 191.5694344253287511, 298.8390017285333897, 8.250976118904059575 ) ) ;
#15254 = CARTESIAN_POINT ( 'NONE',  ( 81.91486247953744737, 58.84361493377822683, 0.3596699001693273168 ) ) ;
#15255 = CARTESIAN_POINT ( 'NONE',  ( 80.01151941643857413, 58.12832627190487500, 16.26807764006944979 ) ) ;
#15256 = LINE ( 'NONE', #61367, #88860 ) ;
#15257 = ORIENTED_EDGE ( 'NONE', *, *, #94219, .T. ) ;
#15258 = CARTESIAN_POINT ( 'NONE',  ( 190.5674408456512765, 300.5745055173924811, -0.9151048603553563199 ) ) ;
#15260 = EDGE_CURVE ( 'NONE', #45441, #99285, #83545, .T. ) ;
#15259 = VECTOR ( 'NONE', #44923, 1000.000000000000341 ) ;
#15261 = CARTESIAN_POINT ( 'NONE',  ( 196.6288634187112052, 290.0758136547079289, -16.31544900032282186 ) ) ;
#15262 = ORIENTED_EDGE ( 'NONE', *, *, #99216, .F. ) ;
#15263 = CARTESIAN_POINT ( 'NONE',  ( 157.3412122618683497, 258.1240215684019290, 16.75554199904894048 ) ) ;
#15264 = CARTESIAN_POINT ( 'NONE',  ( 74.60601093365112035, 63.68499727765737362, 14.35797525815900144 ) ) ;
#15265 = ORIENTED_EDGE ( 'NONE', *, *, #69517, .T. ) ;
#15266 = CARTESIAN_POINT ( 'NONE',  ( 149.7162292714551199, 271.3308795146458010, 12.12826134257344357 ) ) ;
#15267 = CARTESIAN_POINT ( 'NONE',  ( 0.000000000000000000, 0.000000000000000000, -36.50000000000000000 ) ) ;
#15268 = ORIENTED_EDGE ( 'NONE', *, *, #11780, .F. ) ;
#15269 = EDGE_CURVE ( 'NONE', #89471, #13779, #44989, .T. ) ;
#15270 = CARTESIAN_POINT ( 'NONE',  ( -4.991637333140347188, 76.62020665819028409, 14.32149113796480577 ) ) ;
#15271 = CARTESIAN_POINT ( 'NONE',  ( 34.29273532275193759, 21.92755873383628185, 6.180339887498953466 ) ) ;
#15272 = DIRECTION ( 'NONE',  ( -0.7061384650677094976, -0.7080737730998225565, 0.000000000000000000 ) ) ;
#15273 = CARTESIAN_POINT ( 'NONE',  ( 83.14160737058271877, 52.20232750492525753, 14.81664504224666778 ) ) ;
#15274 = VERTEX_POINT ( 'NONE', #53587 ) ;
#15275 = EDGE_CURVE ( 'NONE', #99556, #19691, #39706, .T. ) ;
#15276 = ORIENTED_EDGE ( 'NONE', *, *, #18587, .T. ) ;
#15277 = CARTESIAN_POINT ( 'NONE',  ( 86.95487931624934674, 46.48160929640930306, 8.961892044152525827 ) ) ;
#15278 = CARTESIAN_POINT ( 'NONE',  ( 82.07407170904370730, 42.67750543218616599, -7.226825756593194150 ) ) ;
#15279 = CARTESIAN_POINT ( 'NONE',  ( 177.8194257969418288, 292.8449071177858514, 6.006967295066290013 ) ) ;
#15280 = CARTESIAN_POINT ( 'NONE',  ( 190.1730848958311810, 301.2575500587478814, 0.2415986433272204748 ) ) ;
#15281 = CARTESIAN_POINT ( 'NONE',  ( 148.9719199701866899, 272.6200610409887872, 12.59512981512031438 ) ) ;
#15282 = CARTESIAN_POINT ( 'NONE',  ( 171.2772883960535921, 275.5355528887071728, -15.97953745914274393 ) ) ;
#15283 = CARTESIAN_POINT ( 'NONE',  ( 146.9919008828670712, 276.0495547001825116, -0.7851837772504084434 ) ) ;
#15284 = CARTESIAN_POINT ( 'NONE',  ( 191.8329718516215223, 298.3825415164982928, -8.871589506312979267 ) ) ;
#15285 = CARTESIAN_POINT ( 'NONE',  ( 163.4342283790118699, 257.8248486636775851, 15.55239418657778039 ) ) ;
#15286 = DIRECTION ( 'NONE',  ( -0.5369817302126890235, 0.8435938723211464652, 0.000000000000000000 ) ) ;
#15287 = CARTESIAN_POINT ( 'NONE',  ( -22.42236680055709641, 157.8615022471902591, 0.000000000000000000 ) ) ;
#15288 = CARTESIAN_POINT ( 'NONE',  ( 74.01371779070863965, 64.71087909724029430, -13.67405404575846184 ) ) ;
#15289 = CARTESIAN_POINT ( 'NONE',  ( 77.96593341510595110, 47.91059554715139512, 14.09972309609993424 ) ) ;
#15290 = ORIENTED_EDGE ( 'NONE', *, *, #82176, .T. ) ;
#15291 = CARTESIAN_POINT ( 'NONE',  ( 190.7169416771396584, 300.3155624814804128, -4.593597193813289792 ) ) ;
#15292 = CARTESIAN_POINT ( 'NONE',  ( 82.87719117936363489, 41.29838300305157617, -1.984818766237280485 ) ) ;
#15293 = CARTESIAN_POINT ( 'NONE',  ( 87.37223321024185907, 44.84069173413745091, -6.683519980512460101 ) ) ;
#15294 = CARTESIAN_POINT ( 'NONE',  ( 78.92186904685135573, 46.24801581213586132, 12.84669794032027212 ) ) ;
#15295 = CARTESIAN_POINT ( 'NONE',  ( 191.9984247749195561, 297.6035878492737083, -10.02952061679425455 ) ) ;
#15296 = CARTESIAN_POINT ( 'NONE',  ( 83.61754957953866096, 52.24592005514148951, -14.70745080183155906 ) ) ;
#15297 = CARTESIAN_POINT ( 'NONE',  ( 168.6359126097832473, 286.3801639820744640, -8.064224562910773386 ) ) ;
#15298 = ORIENTED_EDGE ( 'NONE', *, *, #76052, .T. ) ;
#15299 = CARTESIAN_POINT ( 'NONE',  ( 207.8136982414359579, 270.7031114674828700, -0.9536989003868096004 ) ) ;
#15300 = EDGE_CURVE ( 'NONE', #94383, #88861, #37826, .T. ) ;
#15301 = CARTESIAN_POINT ( 'NONE',  ( 72.50318959249285911, 71.67715071215087619, 6.033079537162486794 ) ) ;
#15302 = CARTESIAN_POINT ( 'NONE',  ( 51.02741275436270030, 200.2677522451418781, 10.00000000000009592 ) ) ;
#15303 = CARTESIAN_POINT ( 'NONE',  ( 125.9924764494033980, 252.7369531367911293, -4.594050593750048428 ) ) ;
#15304 = CARTESIAN_POINT ( 'NONE',  ( 199.1526122334580862, 285.7045524820243259, -17.32174362185583050 ) ) ;
#15305 = DIRECTION ( 'NONE',  ( -0.5000000000000011102, -0.8660254037844380415, 0.000000000000000000 ) ) ;
#15306 = CARTESIAN_POINT ( 'NONE',  ( 196.2255671652529259, 290.7743432561995860, 16.01325193769018185 ) ) ;
#15307 = CARTESIAN_POINT ( 'NONE',  ( 175.3637715581867553, 253.4841092191606435, -3.886637052182763785 ) ) ;
#15308 = CARTESIAN_POINT ( 'NONE',  ( 46.94050828626382099, 210.1589784336661637, -6.496448406907675876E-16 ) ) ;
#15309 = CARTESIAN_POINT ( 'NONE',  ( 178.8042996781391594, 291.7804106544875253, -6.068280820113288065 ) ) ;
#15310 = CARTESIAN_POINT ( 'NONE',  ( 68.56611454130262473, 66.34273538077306398, -9.815413640989422817 ) ) ;
#15311 = ORIENTED_EDGE ( 'NONE', *, *, #85316, .T. ) ;
#15312 = CARTESIAN_POINT ( 'NONE',  ( 71.88285097721950478, 66.11705595339820718, 11.91407432373335240 ) ) ;
#15313 = CARTESIAN_POINT ( 'NONE',  ( 74.40645258968876874, 67.99769933107435804, -11.66855138296962480 ) ) ;
#15314 = ADVANCED_FACE ( 'NONE', ( #37879 ), #22709, .T. ) ;
#15315 = DIRECTION ( 'NONE',  ( 0.000000000000000000, 0.000000000000000000, -1.000000000000000000 ) ) ;
#15316 = DIRECTION ( 'NONE',  ( 1.000000000000000000, 0.000000000000000000, 0.000000000000000000 ) ) ;
#15317 = CARTESIAN_POINT ( 'NONE',  ( -24.55113401881919089, 60.19361660390018898, -10.00000000000000000 ) ) ;
#15318 = VECTOR ( 'NONE', #36728, 1000.000000000000114 ) ;
#15319 = FACE_OUTER_BOUND ( 'NONE', #16277, .T. ) ;
#15320 = LINE ( 'NONE', #70030, #33761 ) ;
#15321 = CARTESIAN_POINT ( 'NONE',  ( 116.4844995237365453, 231.3927522451418497, 10.00000000000009592 ) ) ;
#15322 = CARTESIAN_POINT ( 'NONE',  ( 42.57599984984017993, 32.78052372038644791, -10.00000000000000355 ) ) ;
#15323 = ORIENTED_EDGE ( 'NONE', *, *, #66396, .T. ) ;
#15324 = AXIS2_PLACEMENT_3D ( 'NONE', #915, #90796, #414 ) ;
#15325 = B_SPLINE_CURVE_WITH_KNOTS ( 'NONE', 3,
 ( #65534, #27051, #57933, #88915, #19476, #81283, #11857, #96986, #42714, #27558, #17439, #45217, #37119, #89874, #99442, #44214, #14329, #13827, #60403, #82287, #44706, #19950, #36118, #83768, #97949, #90383, #4750, #68025, #51843, #20959, #58904, #81776, #67022, #6731, #21433, #13348, #28029, #82782, #12350, #67522, #89399, #28522, #35633, #43215, #91359, #21923, #12860, #52320, #98452, #59405 ),
 .UNSPECIFIED., .F., .F.,
 ( 4, 2, 2, 2, 2, 2, 2, 2, 2, 2, 2, 2, 2, 2, 2, 2, 2, 2, 2, 2, 2, 2, 2, 2, 4 ),
 ( 0.0007932220939086581961, 0.0009974390316302987787, 0.001099547500491155662, 0.001201655969352012545, 0.001303764438212869428, 0.001405872907073726311, 0.001610089844795440078, 0.002018523720238867610, 0.002426957595682295143, 0.003243825346569043956, 0.004060693097455792336, 0.004877560848342540716, 0.005285994723785950034, 0.005490211661507618697, 0.005592320130368408360, 0.005643374364798802757, 0.005694428599229196288, 0.005796537068089966868, 0.005898645536950736581, 0.006102862474672225701, 0.006511296350115173583, 0.006715513287836669641, 0.006919730225558166567, 0.007123947163279662625, 0.007328164101001158684 ),
 .UNSPECIFIED. ) ;
#15326 = CARTESIAN_POINT ( 'NONE',  ( 163.2437751800324293, 247.9004826992694461, 9.806027032984305336 ) ) ;
#15327 = CARTESIAN_POINT ( 'NONE',  ( 154.1805642697389658, 264.0898361600615090, 16.66230817378441387 ) ) ;
#15328 = B_SPLINE_CURVE_WITH_KNOTS ( 'NONE', 3,
 ( #54993, #100127, #40281, #30713 ),
 .UNSPECIFIED., .F., .F.,
 ( 4, 4 ),
 ( 0.008674612601377954327, 0.01501830814127132901 ),
 .UNSPECIFIED. ) ;
#15329 = ADVANCED_FACE ( 'NONE', ( #45973 ), #7490, .F. ) ;
#15330 = CARTESIAN_POINT ( 'NONE',  ( 22.82720022358212120, 193.1744531367911293, 4.594050593750047540 ) ) ;
#15331 = CARTESIAN_POINT ( 'NONE',  ( 8.736352098677466316, 26.81751292744054638, -6.180339887498951690 ) ) ;
#15332 = CARTESIAN_POINT ( 'NONE',  ( 192.1647585107599525, 272.2333635845343451, 15.21426396329954045 ) ) ;
#15333 = CARTESIAN_POINT ( 'NONE',  ( 146.8358616138309571, 276.3198226421291679, 4.054088818585255716 ) ) ;
#15334 = CARTESIAN_POINT ( 'NONE',  ( 73.07852875935716952, 69.76346136681742394, 9.633212380859575319 ) ) ;
#15336 = CARTESIAN_POINT ( 'NONE',  ( 61.36533069198963375, 215.4244531367911293, -4.594050593750046652 ) ) ;
#15335 = CARTESIAN_POINT ( 'NONE',  ( 175.9267864427629036, 287.0167237252017571, 10.52631150458905651 ) ) ;
#15337 = CARTESIAN_POINT ( 'NONE',  ( 161.1027382213887336, 251.6088674925233022, 13.55451100897754557 ) ) ;
#15338 = CARTESIAN_POINT ( 'NONE',  ( 73.03390162335675484, 57.22514805668252080, 15.90373071166581020 ) ) ;
#15339 = LINE ( 'NONE', #30565, #81286 ) ;
#15340 = CARTESIAN_POINT ( 'NONE',  ( 66.58138301798484804, 68.33132062184148481, -4.336431400097447764 ) ) ;
#15341 = ORIENTED_EDGE ( 'NONE', *, *, #49055, .F. ) ;
#15342 = CARTESIAN_POINT ( 'NONE',  ( 26.07505581137152006, 175.8615022471901739, 5.000000000000051514 ) ) ;
#15343 = CARTESIAN_POINT ( 'NONE',  ( 164.2647213391612979, 246.1321520798662164, -5.830872732487307530 ) ) ;
#15344 = CARTESIAN_POINT ( 'NONE',  ( 149.6191658661038559, 251.0643266524160140, 9.188101187500095079 ) ) ;
#15345 = CARTESIAN_POINT ( 'NONE',  ( 23.88951478931043937, 35.83396525600391413, -2.839279412974133887 ) ) ;
#15346 = CARTESIAN_POINT ( 'NONE',  ( 164.1633302916340824, 260.5967636326182628, -16.15833842069452686 ) ) ;
#15347 = CARTESIAN_POINT ( 'NONE',  ( 189.1076172387113843, 261.3318216691852172, 6.756518968376207468 ) ) ;
#15348 = CARTESIAN_POINT ( 'NONE',  ( 205.7668501412109663, 274.2483563724483133, 11.09689540819876896 ) ) ;
#15350 = CARTESIAN_POINT ( 'NONE',  ( 105.0000000000000000, 4.999999999999999112, -14.21260523776213347 ) ) ;
#15349 = CARTESIAN_POINT ( 'NONE',  ( 88.18856786306730555, 43.91052089632135136, 2.508363019901202140 ) ) ;
#15351 = CARTESIAN_POINT ( 'NONE',  ( 68.68990518416599400, 64.09702660386993500, 11.96895164568068104 ) ) ;
#15352 = VERTEX_POINT ( 'NONE', #48509 ) ;
#15353 = CARTESIAN_POINT ( 'NONE',  ( 80.40629399489428408, 48.06278861952080916, 14.00309965006242230 ) ) ;
#15354 = CARTESIAN_POINT ( 'NONE',  ( 0.000000000000000000, 0.000000000000000000, 0.000000000000000000 ) ) ;
#15355 = CARTESIAN_POINT ( 'NONE',  ( 181.8264173286149799, 287.9594419360853976, 13.67222989781667586 ) ) ;
#15356 = FACE_BOUND ( 'NONE', #47426, .T. ) ;
#15357 = CARTESIAN_POINT ( 'NONE',  ( 13.89351337401799391, 10.94754757982088123, 5.678558825948272215 ) ) ;
#15358 = ORIENTED_EDGE ( 'NONE', *, *, #55587, .F. ) ;
#15359 = CARTESIAN_POINT ( 'NONE',  ( 159.8751497196749654, 253.7351131482786855, 15.29343696838486544 ) ) ;
#15360 = AXIS2_PLACEMENT_3D ( 'NONE', #96940, #42668, #27506 ) ;
#15361 = CARTESIAN_POINT ( 'NONE',  ( 167.7953476065451639, 282.2792976936870559, -12.21232899106869851 ) ) ;
#15362 = CARTESIAN_POINT ( 'NONE',  ( 204.7764732025852084, 275.9637395487929439, -14.02287343454361412 ) ) ;
#15363 = CARTESIAN_POINT ( 'NONE',  ( 57.56414817410227869, 217.3207943907111996, 18.47570218321542868 ) ) ;
#15364 = LINE ( 'NONE', #38162, #55271 ) ;
#15365 = CARTESIAN_POINT ( 'NONE',  ( 40.97244913529674193, 182.9155109091896065, 2.679491924311254714 ) ) ;
#15366 = CARTESIAN_POINT ( 'NONE',  ( 207.6050568035884680, 271.0644890383991310, -1.456818755242089702 ) ) ;
#15367 = CARTESIAN_POINT ( 'NONE',  ( 152.6873874250818517, 266.1846826352417565, -16.66598363829485763 ) ) ;
#15368 = ORIENTED_EDGE ( 'NONE', *, *, #1703, .T. ) ;
#15369 = CARTESIAN_POINT ( 'NONE',  ( 190.8064681396529068, 281.0104612406800015, 16.65631368068653728 ) ) ;
#15370 = DIRECTION ( 'NONE',  ( -0.8660254037844390407, -0.4999999999999992228, 0.000000000000000000 ) ) ;
#15371 = VERTEX_POINT ( 'NONE', #77914 ) ;
#15372 = CARTESIAN_POINT ( 'NONE',  ( 190.8153366230912411, 300.1451374358846920, 3.771947273125533684 ) ) ;
#15373 = CARTESIAN_POINT ( 'NONE',  ( 23.52344096658254102, 21.78052372038640883, -10.00000000000000355 ) ) ;
#15374 = CARTESIAN_POINT ( 'NONE',  ( 189.1789294126936340, 297.1237049920401887, 8.136854452066948795 ) ) ;
#15375 = EDGE_LOOP ( 'NONE', ( #17623, #22369, #68101, #82286 ) ) ;
#15376 = FACE_OUTER_BOUND ( 'NONE', #94847, .T. ) ;
#15377 = CARTESIAN_POINT ( 'NONE',  ( 79.48567122603782309, 59.58331865380349512, -16.19020142938439477 ) ) ;
#15378 = CARTESIAN_POINT ( 'NONE',  ( 8.320926099340340443, 27.73705186507752174, -3.090169943749475845 ) ) ;
#15379 = LINE ( 'NONE', #62476, #73923 ) ;
#15380 = CARTESIAN_POINT ( 'NONE',  ( 69.57577311412531174, 62.66348738126951901, 13.87209483570389779 ) ) ;
#15381 = ORIENTED_EDGE ( 'NONE', *, *, #74236, .T. ) ;
#15382 = CARTESIAN_POINT ( 'NONE',  ( 103.3411068992554220, 218.2202760586659167, -5.415160957724236172E-17 ) ) ;
#15383 = CARTESIAN_POINT ( 'NONE',  ( 192.6946760137320780, 261.4813915186712165, 3.932628284434791966E-12 ) ) ;
#15384 = CARTESIAN_POINT ( 'NONE',  ( 150.7254409736883645, 269.5828735707850683, 14.54962197351449049 ) ) ;
#15385 = CARTESIAN_POINT ( 'NONE',  ( 142.4134467818605572, 241.4824982072973967, 3.021315404115420679E-15 ) ) ;
#15386 = ORIENTED_EDGE ( 'NONE', *, *, #1993, .T. ) ;
#15387 = B_SPLINE_CURVE_WITH_KNOTS ( 'NONE', 3,
 ( #34826, #66731, #81977, #81481, #65726, #11563, #65238 ),
 .UNSPECIFIED., .F., .F.,
 ( 4, 3, 4 ),
 ( 0.000000000000000000, 0.001498044977021306765, 0.002672006358302393171 ),
 .UNSPECIFIED. ) ;
#15388 = ORIENTED_EDGE ( 'NONE', *, *, #79719, .T. ) ;
#15389 = EDGE_CURVE ( 'NONE', #44921, #87111, #42065, .T. ) ;
#15390 = ORIENTED_EDGE ( 'NONE', *, *, #63166, .F. ) ;
#15391 = CARTESIAN_POINT ( 'NONE',  ( 72.80832253034486712, 58.87847187791489745, 15.58086070995311978 ) ) ;
#15392 = AXIS2_PLACEMENT_3D ( 'NONE', #26519, #73130, #89842 ) ;
#15393 = ORIENTED_EDGE ( 'NONE', *, *, #96548, .T. ) ;
#15394 = EDGE_CURVE ( 'NONE', #91009, #24841, #31779, .T. ) ;
#15395 = CARTESIAN_POINT ( 'NONE',  ( 69.98230802859291089, 70.60635815750532629, 3.580953781081825493 ) ) ;
#15396 = ORIENTED_EDGE ( 'NONE', *, *, #19961, .F. ) ;
#15397 = CARTESIAN_POINT ( 'NONE',  ( 164.2647213391612979, 246.1321520798662164, -5.830872732487307530 ) ) ;
#15398 = CARTESIAN_POINT ( 'NONE',  ( 82.75467282439718986, 47.54992309942269912, 12.26659463265117900 ) ) ;
#15399 = EDGE_CURVE ( 'NONE', #49104, #29135, #5828, .T. ) ;
#15401 = CARTESIAN_POINT ( 'NONE',  ( 167.7775688379433348, 281.0729446972871415, 11.62645973616006501 ) ) ;
#15400 = B_SPLINE_CURVE_WITH_KNOTS ( 'NONE', 3,
 ( #14953, #76765, #7360, #38244, #69159, #100089, #92502, #23048, #53945, #84903, #47842, #32662, #46863, #71691, #70146, #93502, #78782, #33165, #8861, #39236, #8372, #70659, #758, #63562, #77785, #94006, #31642, #40246, #86933, #23545, #54436, #85412, #71187, #62542, #55438, #64069, #85934, #1273, #86427, #32157, #16459, #16952, #95013, #24061, #1782, #9367 ),
 .UNSPECIFIED., .F., .F.,
 ( 4, 2, 2, 2, 2, 2, 2, 2, 2, 2, 2, 2, 2, 2, 2, 2, 2, 2, 2, 2, 2, 2, 4 ),
 ( 0.002967356509382767290, 0.003167624148080007852, 0.003367891786777247980, 0.003468025606125868261, 0.003568159425474488541, 0.003668293244823108822, 0.003768427064171732573, 0.003968694702869130994, 0.004168962341566530283, 0.004569497618961164062, 0.005370568173750500142, 0.006171638728539835354, 0.006972709283329171434, 0.007773779838118506647, 0.007873913657467229710, 0.007974047476815952773, 0.007999080931653133539, 0.008024114386490314305, 0.008074181296164674101, 0.008174315115513393695, 0.008574850392908331051, 0.008975385670303270141, 0.009375920947698207497 ),
 .UNSPECIFIED. ) ;
#15402 = EDGE_CURVE ( 'NONE', #24115, #90465, #50470, .T. ) ;
#15403 = CARTESIAN_POINT ( 'NONE',  ( 148.0637215040603394, 274.1931069276759558, -7.795633835291665648 ) ) ;
#15404 = CARTESIAN_POINT ( 'NONE',  ( 82.65530164897143095, 54.02391170524479946, -15.49949047637507782 ) ) ;
#15405 = CARTESIAN_POINT ( 'NONE',  ( 78.32669662580138947, 55.90372456675076762, -16.57385434309017924 ) ) ;
#15406 = CARTESIAN_POINT ( 'NONE',  ( 17.03285546273658113, 12.76004757982088655, 5.678558825948272215 ) ) ;
#15407 = LINE ( 'NONE', #46302, #38070 ) ;
#15408 = CARTESIAN_POINT ( 'NONE',  ( 80.74762043199122274, 57.32811249769932971, 16.57232535949600916 ) ) ;
#15410 = EDGE_LOOP ( 'NONE', ( #43278, #46679, #23857, #44056 ) ) ;
#15409 = CARTESIAN_POINT ( 'NONE',  ( 9.891206074601820220, 186.5177522451419065, 5.000000000000046185 ) ) ;
#15411 = B_SPLINE_CURVE_WITH_KNOTS ( 'NONE', 3,
 ( #34011, #8688, #86748, #25385, #49200, #94821, #55756, #1095, #95353, #94326, #72001, #63386, #71007, #10200, #80134, #64896 ),
 .UNSPECIFIED., .F., .F.,
 ( 4, 2, 2, 2, 2, 2, 2, 4 ),
 ( 1.387778780781445676E-17, 0.0004582705960242376567, 0.0006874058940363459141, 0.0009165411920484541715, 0.001145676490060562212, 0.001374811788072670578, 0.001603947086084778727, 0.001833082384096887093 ),
 .UNSPECIFIED. ) ;
#15412 = CARTESIAN_POINT ( 'NONE',  ( 163.3854574543125580, 247.6550818016845597, 10.82482370245618775 ) ) ;
#15413 = CARTESIAN_POINT ( 'NONE',  ( 45.05398624838444022, 26.41603393254328935, -1.583844403245362020 ) ) ;
#15414 = CARTESIAN_POINT ( 'NONE',  ( 80.30437888069963037, 44.85419571244045045, 11.14874347110982988 ) ) ;
#15415 = CARTESIAN_POINT ( 'NONE',  ( 67.80205187238352948, 65.98368644125179117, -10.46800807810757483 ) ) ;
#15416 = CARTESIAN_POINT ( 'NONE',  ( 200.2631011806900005, 283.7811292041749311, 18.23377125296567058 ) ) ;
#15417 = CARTESIAN_POINT ( 'NONE',  ( 194.5211191180186745, 263.4685241113479606, -0.7776144546925115586 ) ) ;
#15418 = ORIENTED_EDGE ( 'NONE', *, *, #93104, .T. ) ;
#15419 = CARTESIAN_POINT ( 'NONE',  ( 155.1975950535502591, 261.8368754851878180, -18.50127729957631928 ) ) ;
#15420 = CARTESIAN_POINT ( 'NONE',  ( -6.887318171848119341, 24.23892674679880699, -10.00000000000000000 ) ) ;
#15421 = PLANE ( 'NONE',  #38633 ) ;
#15422 = CARTESIAN_POINT ( 'NONE',  ( 2.963002844326352747, 172.5177522451418781, -10.00000000000009592 ) ) ;
#15423 = CARTESIAN_POINT ( 'NONE',  ( 84.07169456928664886, 219.3458772461660544, 9.188101187500095079 ) ) ;
#15424 = CARTESIAN_POINT ( 'NONE',  ( 82.66995253617540129, 53.27399894339424691, -15.29269040213952913 ) ) ;
#15425 = CARTESIAN_POINT ( 'NONE',  ( 173.3452888887486552, 252.5859834778788695, -8.152990710749371317 ) ) ;
#15426 = CARTESIAN_POINT ( 'NONE',  ( 169.9924644626855468, 280.7086247968809403, -14.18413335164717992 ) ) ;
#15427 = CARTESIAN_POINT ( 'NONE',  ( 72.67799729538583620, 70.93760247754363490, 7.641220802698788894 ) ) ;
#15429 = CARTESIAN_POINT ( 'NONE',  ( 110.9455453822464790, 234.8615022471902591, -10.00000000000009592 ) ) ;
#15428 = CARTESIAN_POINT ( 'NONE',  ( 8.456677953475336906, 181.8149278399161233, 9.188101187500093303 ) ) ;
#15430 = CIRCLE ( 'NONE', #41333, 70.00000000000001421 ) ;
#15431 = CARTESIAN_POINT ( 'NONE',  ( 185.4344586771987338, 295.2833515559589728, 8.292135446962131340 ) ) ;
#15432 = EDGE_LOOP ( 'NONE', ( #21065, #21405, #16540, #80527 ) ) ;
#15433 = ORIENTED_EDGE ( 'NONE', *, *, #79059, .F. ) ;
#15434 = CARTESIAN_POINT ( 'NONE',  ( 32.30839531297598910, 123.0650415295850593, -25.00000000000000000 ) ) ;
#15435 = DIRECTION ( 'NONE',  ( 0.4999999999999998890, -0.8660254037844385966, 0.000000000000000000 ) ) ;
#15436 = CARTESIAN_POINT ( 'NONE',  ( 85.74869351040513266, 46.00941097376583855, -9.208016345952161785 ) ) ;
#15437 = CARTESIAN_POINT ( 'NONE',  ( 205.2391015854675516, 275.1624436846170738, -14.01434138479280911 ) ) ;
#15438 = CARTESIAN_POINT ( 'NONE',  ( -71.36129514276956343, 45.88172302328153052, -10.00000000000000000 ) ) ;
#15439 = CARTESIAN_POINT ( 'NONE',  ( 82.78295361368475369, 43.37803873317465531, 7.757655889806053473 ) ) ;
#15440 = CARTESIAN_POINT ( 'NONE',  ( 150.3289749894144336, 276.6211844997497451, 3.694860788824919418 ) ) ;
#15441 = CARTESIAN_POINT ( 'NONE',  ( 19.44454881187291662, 182.0333772461660544, 9.188101187500095079 ) ) ;
#15442 = CARTESIAN_POINT ( 'NONE',  ( 118.1174918034448922, 232.8768266524160140, 9.188101187500098632 ) ) ;
#15443 = DIRECTION ( 'NONE',  ( 0.000000000000000000, -0.4385670422228087340, -0.8986984752829710876 ) ) ;
#15444 = CARTESIAN_POINT ( 'NONE',  ( 183.0115390112375167, 257.7047719680322757, -2.320578905925934965 ) ) ;
#15445 = DIRECTION ( 'NONE',  ( 0.5000000000000014433, -0.8660254037844378194, 0.000000000000000000 ) ) ;
#15446 = CARTESIAN_POINT ( 'NONE',  ( 175.2976095297026973, 281.1217093493183938, -14.67621037160238373 ) ) ;
#15447 = ADVANCED_FACE ( 'NONE', ( #94635 ), #78928, .F. ) ;
#15448 = CARTESIAN_POINT ( 'NONE',  ( -10.27112140336314994, 171.0024278399161233, -9.188101187500093303 ) ) ;
#15449 = CARTESIAN_POINT ( 'NONE',  ( 157.3412122618683497, 258.1240215684019290, 16.75554199904894048 ) ) ;
#15450 = CARTESIAN_POINT ( 'NONE',  ( 194.2764122224708103, 294.1503786489221284, 15.46903869661980835 ) ) ;
#15451 = CARTESIAN_POINT ( 'NONE',  ( 161.1492466472929266, 251.5283125358769212, -13.33353587056634915 ) ) ;
#15452 = VECTOR ( 'NONE', #76098, 1000.000000000000000 ) ;
#15453 = CARTESIAN_POINT ( 'NONE',  ( 82.64400278703348590, 48.09335400213094402, 13.25860807430423272 ) ) ;
#15454 = CARTESIAN_POINT ( 'NONE',  ( 147.6054094044680198, 274.9869267698931594, -8.596541856229405809 ) ) ;
#15455 = CARTESIAN_POINT ( 'NONE',  ( 190.4966860832860220, 262.7064732693366409, 8.377472714625252337 ) ) ;
#15456 = CARTESIAN_POINT ( 'NONE',  ( 171.6100400556340162, 279.8152386110159000, 13.99908611435833983 ) ) ;
#15457 = CARTESIAN_POINT ( 'NONE',  ( 185.4867332780130766, 297.4061142773095412, 5.671143563000668131 ) ) ;
#15458 = CARTESIAN_POINT ( 'NONE',  ( 69.22118451730979416, 69.17181481221663830, 6.156610956507596377 ) ) ;
#15459 = CARTESIAN_POINT ( 'NONE',  ( 190.5969391768923913, 300.5234129089444650, -0.7564693504096553500 ) ) ;
#15460 = CARTESIAN_POINT ( 'NONE',  ( 180.7719503181222080, 266.8161623102827775, -14.72789016211928370 ) ) ;
#15461 = VERTEX_POINT ( 'NONE', #42378 ) ;
#15462 = CIRCLE ( 'NONE', #72132, 70.00000000000001421 ) ;
#15463 = CARTESIAN_POINT ( 'NONE',  ( 74.30578394237890905, 58.31684474416242381, 16.33455613536389350 ) ) ;
#15464 = CARTESIAN_POINT ( 'NONE',  ( 207.5230514910949182, 271.2065264061283756, 2.678931747975364708 ) ) ;
#15465 = CARTESIAN_POINT ( 'NONE',  ( 184.9512090389555397, 269.4173353161797877, 15.97780096459446320 ) ) ;
#15466 = EDGE_CURVE ( 'NONE', #18179, #29839, #64196, .T. ) ;
#15467 = CARTESIAN_POINT ( 'NONE',  ( 97.03527265400872182, 217.6423013555409796, -4.594050593750043987 ) ) ;
#15468 = CARTESIAN_POINT ( 'NONE',  ( 16.65397613197454518, 21.56628583063840310, 9.188101187500006262 ) ) ;
#15469 = CARTESIAN_POINT ( 'NONE',  ( 151.2057546125658973, 268.7509459446807227, 15.78031848731319187 ) ) ;
#15470 = DIRECTION ( 'NONE',  ( 0.9963824715083259287, -0.08498217737243619896, 0.000000000000000000 ) ) ;
#15472 = CARTESIAN_POINT ( 'NONE',  ( 194.7690439115086178, 278.9149514252409290, 16.30030903610881055 ) ) ;
#15471 = CARTESIAN_POINT ( 'NONE',  ( 66.49460505587296666, 68.77342561816206512, 2.322209999061914498 ) ) ;
#15473 = CARTESIAN_POINT ( 'NONE',  ( 202.2429319221604374, 271.5051878758352473, -9.789492590983266851 ) ) ;
#15474 = CARTESIAN_POINT ( 'NONE',  ( 151.0426280674448378, 269.0334894088936153, -15.84467774422408581 ) ) ;
#15475 = CARTESIAN_POINT ( 'NONE',  ( 77.32817876982271343, 63.13942984521013813, 15.61058464551962288 ) ) ;
#15476 = CARTESIAN_POINT ( 'NONE',  ( 57.25197034761130510, 193.8615022471901739, 5.000000000000051514 ) ) ;
#15477 = CARTESIAN_POINT ( 'NONE',  ( 35.32779635548150310, 39.13478043621390867, 8.090169943749478065 ) ) ;
#15478 = DIRECTION ( 'NONE',  ( -0.6602847420308685100, -0.7510153523339117010, 0.000000000000000000 ) ) ;
#15479 = ORIENTED_EDGE ( 'NONE', *, *, #91225, .T. ) ;
#15480 = CARTESIAN_POINT ( 'NONE',  ( 163.6671909760687527, 256.2992013055660436, -14.91259676482536456 ) ) ;
#15481 = CARTESIAN_POINT ( 'NONE',  ( 28.93108252874724684, 32.10171378149919974, 9.188101187500008038 ) ) ;
#15482 = CARTESIAN_POINT ( 'NONE',  ( 198.2505066714982149, 285.2670451491296149, 0.000000000000000000 ) ) ;
#15483 = CARTESIAN_POINT ( 'NONE',  ( 160.8891438268352374, 281.0495864612497599, 9.578199528566821996 ) ) ;
#15484 = CARTESIAN_POINT ( 'NONE',  ( 30.45139999638899653, 75.71324894449729470, 59.99999999999999289 ) ) ;
#15485 = ORIENTED_EDGE ( 'NONE', *, *, #44110, .T. ) ;
#15486 = CARTESIAN_POINT ( 'NONE',  ( 152.8239686330211953, 275.0022943016427348, 10.78622480446937537 ) ) ;
#15487 = DIRECTION ( 'NONE',  ( 0.4999999999999998335, -0.8660254037844388186, 0.000000000000000000 ) ) ;
#15488 = CARTESIAN_POINT ( 'NONE',  ( 179.9008876211633492, 262.7362030500133301, -12.76817184108253223 ) ) ;
#15489 = CARTESIAN_POINT ( 'NONE',  ( 169.3738444220689416, 252.1525573315904296, -8.754927670012239815 ) ) ;
#15490 = CARTESIAN_POINT ( 'NONE',  ( 192.3606619183491091, 297.4685555102766443, 10.99569063633359889 ) ) ;
#15491 = VERTEX_POINT ( 'NONE', #18105 ) ;
#15492 = B_SPLINE_CURVE_WITH_KNOTS ( 'NONE', 3,
 ( #95147, #19124, #49999, #73310 ),
 .UNSPECIFIED., .F., .F.,
 ( 4, 4 ),
 ( 0.02338672457796607887, 0.03261727987500769727 ),
 .UNSPECIFIED. ) ;
#15493 = CARTESIAN_POINT ( 'NONE',  ( 187.5741477178530374, 278.9861021591872259, 17.66168452547810475 ) ) ;
#15494 = CARTESIAN_POINT ( 'NONE',  ( 30.49295849316677831, 39.64646525600392835, -2.839279412974133887 ) ) ;
#15495 = ORIENTED_EDGE ( 'NONE', *, *, #73942, .F. ) ;
#15496 = CARTESIAN_POINT ( 'NONE',  ( 178.2005841394030199, 289.7860138253658420, 11.11017618330963508 ) ) ;
#15497 = LINE ( 'NONE', #55005, #80738 ) ;
#15498 = ORIENTED_EDGE ( 'NONE', *, *, #63187, .F. ) ;
#15499 = CARTESIAN_POINT ( 'NONE',  ( 86.51873334781436142, 47.12553361672021879, -10.58414027450333528 ) ) ;
#15500 = CARTESIAN_POINT ( 'NONE',  ( 9.807469842037885854, 42.32143348850679132, 59.99999999999999289 ) ) ;
#15501 = CARTESIAN_POINT ( 'NONE',  ( 85.04850917506151120, 49.90949791588273143, 13.51477744872044262 ) ) ;
#15502 = CARTESIAN_POINT ( 'NONE',  ( 153.3124474400112831, 265.1020469316042636, -17.30303149702894316 ) ) ;
#15503 = CARTESIAN_POINT ( 'NONE',  ( 88.41177868068123757, 44.08414425260226466, -2.750064808092239410 ) ) ;
#15504 = DIRECTION ( 'NONE',  ( -1.000000000000000000, 0.000000000000000000, 0.000000000000000000 ) ) ;
#15505 = DIRECTION ( 'NONE',  ( 0.8660254037844380415, 0.5000000000000012212, 0.000000000000000000 ) ) ;
#15506 = CARTESIAN_POINT ( 'NONE',  ( 81.44563236102617054, 56.14986361120382696, -16.42609089136781009 ) ) ;
#15507 = CARTESIAN_POINT ( 'NONE',  ( 71.40858655494352547, 63.62864610033815183, -13.92573448899003274 ) ) ;
#15508 = ORIENTED_EDGE ( 'NONE', *, *, #45457, .F. ) ;
#15510 = AXIS2_PLACEMENT_3D ( 'NONE', #97926, #27029, #28501 ) ;
#15509 = CARTESIAN_POINT ( 'NONE',  ( 196.1763519989319775, 290.2392196892972720, 16.27711669441661613 ) ) ;
#15511 = ORIENTED_EDGE ( 'NONE', *, *, #72839, .F. ) ;
#15512 = EDGE_LOOP ( 'NONE', ( #1210, #71858, #53994, #14135 ) ) ;
#15513 = CARTESIAN_POINT ( 'NONE',  ( 169.3676301360849550, 269.0840628972123341, 17.25023024943055461 ) ) ;
#15514 = ORIENTED_EDGE ( 'NONE', *, *, #81979, .T. ) ;
#15515 = CARTESIAN_POINT ( 'NONE',  ( 190.2731979903009858, 300.2022605500126815, -3.404760317914321988 ) ) ;
#15516 = CARTESIAN_POINT ( 'NONE',  ( 205.9447606851647947, 273.9402062711180861, -10.75123264850128102 ) ) ;
#15517 = CARTESIAN_POINT ( 'NONE',  ( 197.5123600491583034, 273.2865668918312281, -13.38184978029139671 ) ) ;
#15518 = CARTESIAN_POINT ( 'NONE',  ( -19.65312891409030271, 93.06504152958497400, 177.5919119679930134 ) ) ;
#15519 = CARTESIAN_POINT ( 'NONE',  ( 82.80834019656774103, 40.61763827593378551, 0.9796441576777050741 ) ) ;
#15520 = CARTESIAN_POINT ( 'NONE',  ( 171.6426604480640776, 250.7983711109617673, -5.691410925449850389 ) ) ;
#15521 = EDGE_CURVE ( 'NONE', #73618, #43232, #10500, .T. ) ;
#15522 = DIRECTION ( 'NONE',  ( 0.4999999999999992784, -0.8660254037844390407, 0.000000000000000000 ) ) ;
#15523 = CARTESIAN_POINT ( 'NONE',  ( 183.6291305219023968, 284.8155054853089609, -15.01443082426404985 ) ) ;
#15524 = CARTESIAN_POINT ( 'NONE',  ( 120.7155680147981940, 234.3768266524159856, 9.188101187500098632 ) ) ;
#15525 = CARTESIAN_POINT ( 'NONE',  ( 184.5558809902196344, 261.3976952126757851, -9.110542280346439981 ) ) ;
#15526 = CARTESIAN_POINT ( 'NONE',  ( 43.56148901884012048, 27.01110640527296169, 2.839279412974134775 ) ) ;
#15527 = CARTESIAN_POINT ( 'NONE',  ( 177.3582130212591608, 288.8584996472486068, -9.346563926071064898 ) ) ;
#15528 = ORIENTED_EDGE ( 'NONE', *, *, #46843, .F. ) ;
#15529 = CIRCLE ( 'NONE', #78631, 0.1418229129680828593 ) ;
#15530 = CARTESIAN_POINT ( 'NONE',  ( 86.84459937989694822, 45.86515160798009560, -8.194834137214424885 ) ) ;
#15531 = CARTESIAN_POINT ( 'NONE',  ( 74.77113966951148427, 63.06429047545149302, -14.66048351875234523 ) ) ;
#15532 = DIRECTION ( 'NONE',  ( 1.000000000000000000, 0.000000000000000000, 0.000000000000000000 ) ) ;
#15533 = CARTESIAN_POINT ( 'NONE',  ( 192.1032606970431971, 297.9143875035085784, 11.39438513385636043 ) ) ;
#15534 = CARTESIAN_POINT ( 'NONE',  ( 72.46461309515387939, 63.44911742965013701, 13.84624394093605027 ) ) ;
#15535 = CARTESIAN_POINT ( 'NONE',  ( 66.77752810875767864, 68.40544692769400115, 4.459354299965320401 ) ) ;
#15536 = CARTESIAN_POINT ( 'NONE',  ( 177.1467926689314538, 288.7641837594472349, -9.305349299006246966 ) ) ;
#15537 = ORIENTED_EDGE ( 'NONE', *, *, #24439, .T. ) ;
#15538 = CARTESIAN_POINT ( 'NONE',  ( 29.80052344588228408, 32.90829794293883026, 10.00000000000000355 ) ) ;
#15539 =( BOUNDED_CURVE ( )  B_SPLINE_CURVE ( 2, ( #87162, #49576, #80529, #49091, #3506, #55659, #95236, #72415, #33907, #65281, #96222, #64795, #94721 ),
 .UNSPECIFIED., .F., .T. ) 
 B_SPLINE_CURVE_WITH_KNOTS ( ( 3, 2, 2, 2, 2, 2, 3 ),
 ( 0.5875000000000000222, 0.5899999999999999689, 0.5949999999999999734, 0.5999999999999999778, 0.6049999999999999822, 0.6099999999999999867, 0.6125000000000000444 ),
 .UNSPECIFIED. ) 
 CURVE ( )  GEOMETRIC_REPRESENTATION_ITEM ( )  RATIONAL_B_SPLINE_CURVE ( ( 0.9755282581475767101, 0.9755282581475772652, 1.000000000000000000, 0.9510565162951535312, 1.000000000000000000, 0.9510565162951535312, 1.000000000000000000, 0.9510565162951535312, 1.000000000000000000, 0.9510565162951535312, 1.000000000000000000, 0.9755282581475761550, 0.9755282581475767101 ) ) 
 REPRESENTATION_ITEM ( '' )  );
#15540 = EDGE_LOOP ( 'NONE', ( #21084, #10354, #27539, #8056 ) ) ;
#15541 = CARTESIAN_POINT ( 'NONE',  ( 194.7576540903134799, 293.3168432830895540, -14.62421624641040196 ) ) ;
#15542 = FACE_OUTER_BOUND ( 'NONE', #7173, .T. ) ;
#15543 = ORIENTED_EDGE ( 'NONE', *, *, #53881, .F. ) ;
#15544 = FACE_OUTER_BOUND ( 'NONE', #20807, .T. ) ;
#15545 = CARTESIAN_POINT ( 'NONE',  ( 158.2756371360163143, 277.3693515115958235, 10.25742348846014984 ) ) ;
#15546 = PLANE ( 'NONE',  #96769 ) ;
#15547 = CARTESIAN_POINT ( 'NONE',  ( 190.0667283601964357, 259.9641452334862493, -5.090329199819447104E-14 ) ) ;
#15548 = CARTESIAN_POINT ( 'NONE',  ( 163.0683798854284703, 248.2042762609320903, 11.26611642476872710 ) ) ;
#15550 = CARTESIAN_POINT ( 'NONE',  ( 69.62688595351798426, 63.12627229902661696, -13.61770258999189309 ) ) ;
#15549 = DIRECTION ( 'NONE',  ( 0.7235470741700457120, 0.1663964660674585594, 0.6699192843471722947 ) ) ;
#15551 = CARTESIAN_POINT ( 'NONE',  ( 152.8328714238065515, 265.9326969577624027, -16.29536156676786263 ) ) ;
#15552 = VERTEX_POINT ( 'NONE', #2929 ) ;
#15553 = CARTESIAN_POINT ( 'NONE',  ( 190.1813752874636805, 301.2431906792259042, -4.710625539811892359 ) ) ;
#15554 = CARTESIAN_POINT ( 'NONE',  ( 170.6178593158246315, 266.5408558992322696, -17.65857870869936974 ) ) ;
#15555 = CARTESIAN_POINT ( 'NONE',  ( 186.7785090572402282, 262.7977421546021333, -9.006081414252482986 ) ) ;
#15556 = CARTESIAN_POINT ( 'NONE',  ( 182.7953794973296056, 276.1600416569049230, -16.45808333016647040 ) ) ;
#15557 = CARTESIAN_POINT ( 'NONE',  ( 40.70814378237798081, 60.14496435084704018, -10.00000000000000000 ) ) ;
#15558 = CARTESIAN_POINT ( 'NONE',  ( 192.7870477231578548, 271.6154284180436775, -14.94562697032598741 ) ) ;
#15559 = CARTESIAN_POINT ( 'NONE',  ( 164.0781508658037637, 275.4055464209769752, 15.63836535835214114 ) ) ;
#15560 = CARTESIAN_POINT ( 'NONE',  ( 83.37188637347107090, 43.51478601198282803, 7.417674380252161193 ) ) ;
#15561 = CARTESIAN_POINT ( 'NONE',  ( 27.30738562583555762, 198.1199935810940929, 2.679491924311251605 ) ) ;
#15562 = CARTESIAN_POINT ( 'NONE',  ( 73.97124227054526102, 68.60621492378263042, 10.89700218101527085 ) ) ;
#15563 = DIRECTION ( 'NONE',  ( 0.000000000000000000, -0.000000000000000000, 1.000000000000000000 ) ) ;
#15564 = CARTESIAN_POINT ( 'NONE',  ( 82.66149664020484522, 53.53843108144140928, -15.73363621927586742 ) ) ;
#15565 = CARTESIAN_POINT ( 'NONE',  ( 68.21243081460160340, 216.3149278399160664, 9.188101187500093303 ) ) ;
#15566 = CARTESIAN_POINT ( 'NONE',  ( 67.16503064337793205, 66.61400111815741809, 8.426382589595288408 ) ) ;
#15567 = CARTESIAN_POINT ( 'NONE',  ( 192.5076277540105423, 297.2140032159341558, -13.10094381206144298 ) ) ;
#15568 = CARTESIAN_POINT ( 'NONE',  ( 50.32376711733572705, 209.8615022471902876, 5.000000000000046185 ) ) ;
#15569 = CARTESIAN_POINT ( 'NONE',  ( 154.8786460229866577, 262.3893114111486398, -18.06164891362396929 ) ) ;
#15571 = EDGE_CURVE ( 'NONE', #37717, #90330, #26505, .T. ) ;
#15570 = VECTOR ( 'NONE', #66865, 1000.000000000000000 ) ;
#15572 = CARTESIAN_POINT ( 'NONE',  ( 207.2707369601997982, 271.6435479931266173, -5.381413637561199614 ) ) ;
#15573 = DIRECTION ( 'NONE',  ( 1.000000000000000000, 0.000000000000000000, 0.000000000000000000 ) ) ;
#15574 = VECTOR ( 'NONE', #8222, 1000.000000000000000 ) ;
#15575 = LINE ( 'NONE', #31285, #84145 ) ;
#15577 = DIRECTION ( 'NONE',  ( -0.000000000000000000, -0.000000000000000000, -1.000000000000000000 ) ) ;
#15576 = CARTESIAN_POINT ( 'NONE',  ( 73.09452573934707686, 69.60050248057373778, -9.839270276345128963 ) ) ;
#15578 = CARTESIAN_POINT ( 'NONE',  ( 169.5608527833963421, 251.6396950762901952, -9.960993533446050208 ) ) ;
#15579 = CARTESIAN_POINT ( 'NONE',  ( 164.7508860646548783, 245.2900900744633930, -5.203382148009804808 ) ) ;
#15580 = CARTESIAN_POINT ( 'NONE',  ( 157.0935036675524827, 258.5530654392286465, 17.32636058289560665 ) ) ;
#15581 = AXIS2_PLACEMENT_3D ( 'NONE', #74879, #13573, #53539 ) ;
#15582 = LINE ( 'NONE', #78418, #80326 ) ;
#15583 = EDGE_CURVE ( 'NONE', #11680, #75397, #15492, .T. ) ;
#15584 = CARTESIAN_POINT ( 'NONE',  ( 161.8408514536557163, 250.3304178724980318, -14.12919723462510646 ) ) ;
#15585 = CARTESIAN_POINT ( 'NONE',  ( 35.38456857845647363, 200.4244531367911293, -4.594050593750046652 ) ) ;
#15586 = ADVANCED_FACE ( 'NONE', ( #72830 ), #3902, .F. ) ;
#15587 = CARTESIAN_POINT ( 'NONE',  ( 49.32242524243604720, 199.2833772461660828, -9.188101187500095079 ) ) ;
#15588 = CARTESIAN_POINT ( 'NONE',  ( 48.43557798863805886, 76.81918075477977936, -10.00000000000000000 ) ) ;
#15589 = CARTESIAN_POINT ( 'NONE',  ( 88.53016884517781193, 43.88792164385783678, -0.09627500500477706447 ) ) ;
#15590 = CARTESIAN_POINT ( 'NONE',  ( 4.654322096184512425, 26.18528772668515714, -1.583844403245363575 ) ) ;
#15591 = CARTESIAN_POINT ( 'NONE',  ( 146.0739611433025686, 245.9548013555409796, -4.594050593750042211 ) ) ;
#15592 = CARTESIAN_POINT ( 'NONE',  ( -19.65312891409030271, 93.06504152958497400, -10.00000000000000888 ) ) ;
#15593 = CARTESIAN_POINT ( 'NONE',  ( 14.65434579541623172, 189.2677522451419065, -5.000000000000047962 ) ) ;
#15594 = CARTESIAN_POINT ( 'NONE',  ( 30.20304716546516133, 19.29860640527293469, -2.839279412974138328 ) ) ;
#15595 = CARTESIAN_POINT ( 'NONE',  ( -4.215479392844351914, 156.8262482093458061, -4.415768667553307481E-15 ) ) ;
#15596 = CARTESIAN_POINT ( 'NONE',  ( 149.1939152435731728, 272.2355539484436235, -11.44223522189843933 ) ) ;
#15597 = CARTESIAN_POINT ( 'NONE',  ( 16.58301002715608519, 15.28920272979925876, -7.433330006724141015 ) ) ;
#15598 = CARTESIAN_POINT ( 'NONE',  ( 59.55217677675724275, 211.3149278399160949, -9.188101187500095079 ) ) ;
#15599 = CARTESIAN_POINT ( 'NONE',  ( 77.22913030991912819, 63.42231615505745879, 15.12051831926749834 ) ) ;
#15600 = CARTESIAN_POINT ( 'NONE',  ( 74.14312167556930433, 66.30466486950707861, 1.224646799147354045E-15 ) ) ;
#15601 = VECTOR ( 'NONE', #91592, 1000.000000000000227 ) ;
#15602 = CARTESIAN_POINT ( 'NONE',  ( 198.2040940955416488, 287.3474340887963763, 16.95806375232200480 ) ) ;
#15603 = LINE ( 'NONE', #40403, #84602 ) ;
#15604 = CARTESIAN_POINT ( 'NONE',  ( 153.2966090711206846, 276.8115077458087399, 7.191393513384046088 ) ) ;
#15605 = AXIS2_PLACEMENT_3D ( 'NONE', #84424, #14970, #45857 ) ;
#15606 = CARTESIAN_POINT ( 'NONE',  ( 77.04458465457972238, 56.18878383020774692, -16.16646171855996172 ) ) ;
#15607 = CARTESIAN_POINT ( 'NONE',  ( 87.65828818788342858, 45.19712344130779513, -6.201442590288507972 ) ) ;
#15608 = CARTESIAN_POINT ( 'NONE',  ( 110.9455453822464790, 234.8615022471902591, -10.00000000000009592 ) ) ;
#15609 = CARTESIAN_POINT ( 'NONE',  ( 200.6800100461949228, 283.0590218669948399, 18.32402613046234308 ) ) ;
#15610 = CARTESIAN_POINT ( 'NONE',  ( 164.3706594650489023, 245.9486618633701482, -1.665857659249071698 ) ) ;
#15611 = ORIENTED_EDGE ( 'NONE', *, *, #38962, .F. ) ;
#15612 = CARTESIAN_POINT ( 'NONE',  ( 77.32596066893822240, 49.50693989401381856, 14.91615350571074927 ) ) ;
#15613 = CARTESIAN_POINT ( 'NONE',  ( 200.2093391412865060, 269.7417714514684803, 10.46510648850140157 ) ) ;
#15614 = ORIENTED_EDGE ( 'NONE', *, *, #60944, .T. ) ;
#15615 = CARTESIAN_POINT ( 'NONE',  ( 206.2313482792274328, 273.4438219973828268, -9.403385562213845361 ) ) ;
#15616 = CARTESIAN_POINT ( 'NONE',  ( 193.6523268064705974, 293.2313262976975352, 15.26490498002906193 ) ) ;
#15617 = CARTESIAN_POINT ( 'NONE',  ( 70.66454081066896720, 68.90461880718730470, -8.132011908148811585 ) ) ;
#15618 = EDGE_LOOP ( 'NONE', ( #32380, #66362, #40554, #3637 ) ) ;
#15619 = CARTESIAN_POINT ( 'NONE',  ( 173.3120886762449686, 251.6182065839331301, 0.03490652146819783752 ) ) ;
#15620 = ORIENTED_EDGE ( 'NONE', *, *, #34946, .F. ) ;
#15621 = CARTESIAN_POINT ( 'NONE',  ( -19.51228460464733416, 93.04840965836413602, 59.99999999999999289 ) ) ;
#15622 = CARTESIAN_POINT ( 'NONE',  ( 147.9133274879049793, 274.4535970048112290, -9.359166267164972908 ) ) ;
#15623 = FACE_OUTER_BOUND ( 'NONE', #6696, .T. ) ;
#15624 = ORIENTED_EDGE ( 'NONE', *, *, #91376, .T. ) ;
#15625 = CARTESIAN_POINT ( 'NONE',  ( 28.45357225853751260, 28.37878583063842441, 9.188101187500006262 ) ) ;
#15626 = CARTESIAN_POINT ( 'NONE',  ( 75.76995552607449724, 58.63049212716732228, 15.98588464947494892 ) ) ;
#15627 = CARTESIAN_POINT ( 'NONE',  ( 156.9763224152064822, 271.9908631200777904, -15.29896765642516776 ) ) ;
#15628 = CARTESIAN_POINT ( 'NONE',  ( 6.406750531224583156, 186.0530062829863027, -4.648177544792955347E-16 ) ) ;
#15629 = EDGE_CURVE ( 'NONE', #57163, #35859, #66195, .T. ) ;
#15630 = EDGE_CURVE ( 'NONE', #59206, #98946, #84458, .T. ) ;
#15631 = ORIENTED_EDGE ( 'NONE', *, *, #23766, .T. ) ;
#15632 = CARTESIAN_POINT ( 'NONE',  ( 140.3904091109174317, 241.8615022471902023, 5.000000000000051514 ) ) ;
#15633 = CARTESIAN_POINT ( 'NONE',  ( -21.75249381947928740, 146.7012482093458914, -48.95643923738973768 ) ) ;
#15634 = ORIENTED_EDGE ( 'NONE', *, *, #93815, .F. ) ;
#15635 = EDGE_CURVE ( 'NONE', #4619, #11450, #78327, .T. ) ;
#15636 = CARTESIAN_POINT ( 'NONE',  ( 172.1836633629298206, 284.9661130839314751, 10.60870986581373820 ) ) ;
#15638 = DIRECTION ( 'NONE',  ( 0.000000000000000000, -0.000000000000000000, -1.000000000000000000 ) ) ;
#15637 = CARTESIAN_POINT ( 'NONE',  ( 67.83068094623702393, 65.48536241154209847, 10.26294962280224965 ) ) ;
#15639 = DIRECTION ( 'NONE',  ( 1.000000000000000000, 0.000000000000000000, 0.000000000000000000 ) ) ;
#15640 = CARTESIAN_POINT ( 'NONE',  ( 163.9942050550062049, 246.6007000282974673, 5.791111691696777974 ) ) ;
#15641 = CARTESIAN_POINT ( 'NONE',  ( 187.1243084772174825, 293.7649743884641111, -10.81561194776973700 ) ) ;
#15642 = CARTESIAN_POINT ( 'NONE',  ( 164.3068057902571582, 265.7701674460021195, -17.51175939818463334 ) ) ;
#15643 = CARTESIAN_POINT ( 'NONE',  ( 140.2550926398021147, 251.7833772461660544, -9.188101187500095079 ) ) ;
#15644 = EDGE_CURVE ( 'NONE', #90262, #94724, #57851, .T. ) ;
#15645 = DIRECTION ( 'NONE',  ( 1.000000000000000000, 1.156482317317871331E-15, 0.000000000000000000 ) ) ;
#15646 = CARTESIAN_POINT ( 'NONE',  ( 179.3255745279743394, 258.5940977613889231, 9.670503133756291447 ) ) ;
#15647 = CARTESIAN_POINT ( 'NONE',  ( 66.23672358827711548, 218.2369531367911293, -4.594050593750048428 ) ) ;
#15648 = VERTEX_POINT ( 'NONE', #25586 ) ;
#15649 = CARTESIAN_POINT ( 'NONE',  ( 151.0715479399129606, 268.9833987204304435, 14.24612252017116987 ) ) ;
#15650 = DIRECTION ( 'NONE',  ( 0.000000000000000000, 0.000000000000000000, -1.000000000000000000 ) ) ;
#15651 = CARTESIAN_POINT ( 'NONE',  ( -8.406493707509316238, 25.24382671950691304, 10.00000000000000000 ) ) ;
#15652 = AXIS2_PLACEMENT_3D ( 'NONE', #79935, #88551, #96632 ) ;
#15653 = ORIENTED_EDGE ( 'NONE', *, *, #2576, .T. ) ;
#15654 = CARTESIAN_POINT ( 'NONE',  ( 157.4139724630872195, 257.9979972031215425, -18.09067551972931653 ) ) ;
#15655 = AXIS2_PLACEMENT_3D ( 'NONE', #48174, #25897, #56263 ) ;
#15656 = ORIENTED_EDGE ( 'NONE', *, *, #56489, .F. ) ;
#15657 = ORIENTED_EDGE ( 'NONE', *, *, #16416, .F. ) ;
#15658 = EDGE_CURVE ( 'NONE', #21882, #85237, #52365, .T. ) ;
#15659 = CARTESIAN_POINT ( 'NONE',  ( 66.78892157389906004, 67.90037632253439881, 7.001642916364290592 ) ) ;
#15660 = EDGE_CURVE ( 'NONE', #65907, #50908, #91619, .T. ) ;
#15661 = CARTESIAN_POINT ( 'NONE',  ( 197.8751239397817301, 286.8074493601922654, 16.93281720670876922 ) ) ;
#15663 = B_SPLINE_SURFACE_WITH_KNOTS ( 'NONE', 3, 1, ( 
 ( #94438, #94940 ),
 ( #24992, #8802 ),
 ( #25504, #17919 ),
 ( #18925, #88367 ),
 ( #41183, #72120 ),
 ( #64509, #33612 ),
 ( #56889, #49799 ),
 ( #41690, #18419 ),
 ( #49309, #72633 ),
 ( #34117, #95954 ),
 ( #26515, #57392 ),
 ( #39670, #70598 ),
 ( #32088, #93945 ),
 ( #20920, #81737 ),
 ( #66493, #12822 ),
 ( #74116, #3719 ),
 ( #98413, #74625 ),
 ( #19437, #43173 ),
 ( #89837, #80761 ),
 ( #59877, #51280 ),
 ( #90844, #44173 ),
 ( #82249, #27515 ),
 ( #5198, #66982 ),
 ( #36577, #4710 ),
 ( #27989, #27011 ),
 ( #19915, #59365 ),
 ( #67483, #50786 ),
 ( #35596, #96444 ),
 ( #57895, #97420 ),
 ( #11820, #73609 ),
 ( #82745, #58385 ) ),
 .UNSPECIFIED., .F., .F., .F.,
 ( 4, 3, 3, 3, 3, 3, 3, 3, 3, 3, 4 ),
 ( 2, 2 ),
 ( 0.000000000000000000, 0.1122669598086764586, 0.2243161639709642108, 0.3396355846219141217, 0.4553962076585162944, 0.5677860799922443968, 0.6749047109689607638, 0.7773884377078399410, 0.8775581155834293323, 0.9782364162377974459, 1.000000000000000000 ),
 ( 0.000000000000000000, 1.000000000000000000 ),
 .UNSPECIFIED. ) ;
#15662 = CARTESIAN_POINT ( 'NONE',  ( 191.1192699377806719, 299.6187094927299199, -9.526914969203620132 ) ) ;
#15664 = CARTESIAN_POINT ( 'NONE',  ( -67.91103796225580425, 44.10201266000169795, -10.00000000000000000 ) ) ;
#15665 = CARTESIAN_POINT ( 'NONE',  ( 84.38804523167981131, 47.38734847442095344, -11.44389121885481764 ) ) ;
#15666 = CARTESIAN_POINT ( 'NONE',  ( 70.39359452487714464, 63.86253493995260300, 12.85482810418176491 ) ) ;
#15667 = CARTESIAN_POINT ( 'NONE',  ( 81.01380268399661588, 208.3923013555409796, 4.594050593750050204 ) ) ;
#15668 = ORIENTED_EDGE ( 'NONE', *, *, #91252, .F. ) ;
#15669 = ORIENTED_EDGE ( 'NONE', *, *, #67651, .F. ) ;
#15670 = CARTESIAN_POINT ( 'NONE',  ( 15.64201941024748521, 32.52903772873357724, -1.583844403245363575 ) ) ;
#15671 = LINE ( 'NONE', #84140, #80296 ) ;
#15672 = ORIENTED_EDGE ( 'NONE', *, *, #72839, .T. ) ;
#15673 = DIRECTION ( 'NONE',  ( -1.000000000000000000, 0.000000000000000000, 0.000000000000000000 ) ) ;
#15674 = CARTESIAN_POINT ( 'NONE',  ( 75.96213316711562413, 65.70078031631311433, -14.22672748915905316 ) ) ;
#15675 = CARTESIAN_POINT ( 'NONE',  ( 164.4573439719129340, 245.7985198932525748, 1.541132361166968501 ) ) ;
#15677 = VECTOR ( 'NONE', #32021, 1000.000000000000000 ) ;
#15676 = CARTESIAN_POINT ( 'NONE',  ( -31.52638293593248164, 93.28895303089220192, 44.04053121186087338 ) ) ;
#15678 = CARTESIAN_POINT ( 'NONE',  ( 207.3895038639124095, 270.9794483157102150, -1.916867053770541007 ) ) ;
#15679 = CARTESIAN_POINT ( 'NONE',  ( 147.4771145948261051, 275.6046598944997186, -0.0007385123558252784009 ) ) ;
#15680 = VERTEX_POINT ( 'NONE', #11406 ) ;
#15681 = VECTOR ( 'NONE', #64904, 1000.000000000000114 ) ;
#15682 = CARTESIAN_POINT ( 'NONE',  ( 82.07714787726266081, 43.65997060240250249, -8.726277158289674318 ) ) ;
#15683 = CARTESIAN_POINT ( 'NONE',  ( 185.3858643910043327, 260.1458795028655118, 6.052290864491880029 ) ) ;
#15684 = DIRECTION ( 'NONE',  ( 0.9981280818701453450, 0.06115825522547521653, 0.000000000000000000 ) ) ;
#15685 = CARTESIAN_POINT ( 'NONE',  ( 153.3859906278383676, 264.9746663937372091, -17.41799046551451013 ) ) ;
#15686 = AXIS2_PLACEMENT_3D ( 'NONE', #27385, #58270, #89246 ) ;
#15687 = CARTESIAN_POINT ( 'NONE',  ( 72.60199962089298253, 70.74354872798666349, 7.145580164668644763 ) ) ;
#15688 = CARTESIAN_POINT ( 'NONE',  ( 67.90243728005769697, 67.41594138055857854, -7.898924796095583289 ) ) ;
#15689 = DIRECTION ( 'NONE',  ( 0.8660254037844384856, 0.5000000000000002220, 0.000000000000000000 ) ) ;
#15690 = CARTESIAN_POINT ( 'NONE',  ( 147.7917198021585534, 275.6304213403500398, -3.790807063116589770 ) ) ;
#15691 = PLANE ( 'NONE',  #98066 ) ;
#15692 = CARTESIAN_POINT ( 'NONE',  ( 188.2520712372829621, 265.6420100395978920, -13.17850047611677766 ) ) ;
#15693 = CARTESIAN_POINT ( 'NONE',  ( 83.67218728734262356, 52.30219252426102372, 14.72955347366556111 ) ) ;
#15694 = FACE_BOUND ( 'NONE', #45535, .T. ) ;
#15695 = EDGE_LOOP ( 'NONE', ( #10930, #76813, #79490, #432 ) ) ;
#15696 = CARTESIAN_POINT ( 'NONE',  ( -16.11791840453430780, 102.2811357711566131, 44.54428794602774389 ) ) ;
#15697 = EDGE_CURVE ( 'NONE', #19691, #53889, #56599, .T. ) ;
#15698 = CARTESIAN_POINT ( 'NONE',  ( 157.8043799545718286, 257.3217915922150496, -17.97575562758749257 ) ) ;
#15700 = CARTESIAN_POINT ( 'NONE',  ( 73.60243789457724972, 55.52622633506491212, 16.10732509438123827 ) ) ;
#15699 = CARTESIAN_POINT ( 'NONE',  ( 155.6276701977099890, 261.0919634844306643, 17.49722577287685255 ) ) ;
#15701 = CARTESIAN_POINT ( 'NONE',  ( 60.28305926085675992, 215.6115022471903160, -5.000000000000047962 ) ) ;
#15702 = EDGE_CURVE ( 'NONE', #45792, #59362, #48888, .T. ) ;
#15703 = CARTESIAN_POINT ( 'NONE',  ( 29.75882387383049377, 25.38052372038642091, 10.00000000000000533 ) ) ;
#15704 = LINE ( 'NONE', #77536, #33573 ) ;
#15705 = DIRECTION ( 'NONE',  ( -0.000000000000000000, -0.000000000000000000, 1.000000000000000000 ) ) ;
#15706 = CARTESIAN_POINT ( 'NONE',  ( 192.2580028094575653, 262.1757339090664800, 3.009676160147899182 ) ) ;
#15707 = CARTESIAN_POINT ( 'NONE',  ( -10.94779052401099051, 173.6744531367911293, 4.594050593750047540 ) ) ;
#15708 = CARTESIAN_POINT ( 'NONE',  ( 191.6148588865760871, 296.7603242537468873, -11.89382487812838995 ) ) ;
#15709 = VERTEX_POINT ( 'NONE', #10389 ) ;
#15710 = EDGE_CURVE ( 'NONE', #41871, #16265, #9413, .T. ) ;
#15711 = CARTESIAN_POINT ( 'NONE',  ( 174.8527186269040783, 255.3323168797083156, 8.645391441763411677 ) ) ;
#15712 = DIRECTION ( 'NONE',  ( -1.000000000000000000, 0.000000000000000000, 0.000000000000000000 ) ) ;
#15713 = CYLINDRICAL_SURFACE ( 'NONE', #61431, 1.449999999999993072 ) ;
#15714 = CARTESIAN_POINT ( 'NONE',  ( 28.21305602519035460, 187.0958772461660544, -9.188101187500095079 ) ) ;
#15715 = CARTESIAN_POINT ( 'NONE',  ( 76.95483076014906487, 63.96668203270510134, -15.25269828761453894 ) ) ;
#15716 = VECTOR ( 'NONE', #66689, 1000.000000000000000 ) ;
#15717 = CARTESIAN_POINT ( 'NONE',  ( 181.9564645032531018, 275.7194610820193361, -16.43226933849268789 ) ) ;
#15718 = CARTESIAN_POINT ( 'NONE',  ( 34.28597393419622819, 20.76426979415091978, 3.090169943749476733 ) ) ;
#15719 = CARTESIAN_POINT ( 'NONE',  ( 125.2349645446897171, 243.1115022471902591, 10.00000000000009592 ) ) ;
#15720 = CARTESIAN_POINT ( 'NONE',  ( 170.1675564235169418, 270.7386499948772780, -16.98440315941436651 ) ) ;
#15721 = VECTOR ( 'NONE', #27752, 1000.000000000000000 ) ;
#15722 = CARTESIAN_POINT ( 'NONE',  ( 138.0629658346988151, 250.5177522451418213, -10.00000000000009592 ) ) ;
#15723 = CARTESIAN_POINT ( 'NONE',  ( 83.57010898113827579, 45.17450624426406591, 10.33823738828239591 ) ) ;
#15724 = EDGE_CURVE ( 'NONE', #54703, #17355, #72201, .T. ) ;
#15725 = CARTESIAN_POINT ( 'NONE',  ( 164.5546760946605787, 285.7985264595317290, -4.260912962880108346 ) ) ;
#15726 = ADVANCED_FACE ( 'NONE', ( #80321 ), #41767, .F. ) ;
#15727 = VECTOR ( 'NONE', #87673, 1000.000000000000000 ) ;
#15728 = CARTESIAN_POINT ( 'NONE',  ( 68.07728789491670796, 220.1115022471903160, -5.000000000000047962 ) ) ;
#15729 = CYLINDRICAL_SURFACE ( 'NONE', #33679, 17.82106496071139645 ) ;
#15730 = CARTESIAN_POINT ( 'NONE',  ( 35.46636587765004123, 179.0327760586659736, 1.948934522072303157E-15 ) ) ;
#15731 = CARTESIAN_POINT ( 'NONE',  ( 72.51946054628301397, 70.67701989327741785, -7.917356521280773940 ) ) ;
#15732 = FILL_AREA_STYLE_COLOUR ( '', #100233 ) ;
#15733 = CARTESIAN_POINT ( 'NONE',  ( 151.4428545556028780, 268.3402767968688067, -15.03309903163500749 ) ) ;
#15734 = CYLINDRICAL_SURFACE ( 'NONE', #95264, 10.00000000000001066 ) ;
#15735 = CARTESIAN_POINT ( 'NONE',  ( 162.5812779487254147, 280.2977391392396953, -9.910640860102120087 ) ) ;
#15736 = CARTESIAN_POINT ( 'NONE',  ( 163.7166294601506991, 282.3380383384618995, 10.03031969300557513 ) ) ;
#15737 = CARTESIAN_POINT ( 'NONE',  ( 22.06543860749898300, 21.24335787977763346, -9.188101187500008038 ) ) ;
#15738 = CARTESIAN_POINT ( 'NONE',  ( 190.2476911738421848, 301.1283281946692796, -1.360079143321618611 ) ) ;
#15739 = CARTESIAN_POINT ( 'NONE',  ( 71.42966913292450215, 59.23173737558743568, 15.76165678759474886 ) ) ;
#15740 = CARTESIAN_POINT ( 'NONE',  ( 188.8132345201846931, 270.2707858497124676, -15.13545237428995094 ) ) ;
#15741 = EDGE_LOOP ( 'NONE', ( #2451, #44939, #62871, #19315 ) ) ;
#15742 = AXIS2_PLACEMENT_3D ( 'NONE', #33356, #62233, #95207 ) ;
#15743 = CARTESIAN_POINT ( 'NONE',  ( 14.52619969316804394, 14.10170272979925699, -7.433330006724141015 ) ) ;
#15744 = CARTESIAN_POINT ( 'NONE',  ( 75.29051265121657366, 53.62752787197079130, -16.53442706284598174 ) ) ;
#15745 = CARTESIAN_POINT ( 'NONE',  ( 198.4097421844162170, 265.0824675037606539, -3.039349057205883664 ) ) ;
#15746 = CARTESIAN_POINT ( 'NONE',  ( 81.55469672513726209, 42.53656836688637810, 7.482253779589008502 ) ) ;
#15747 = EDGE_CURVE ( 'NONE', #25763, #29087, #2287, .T. ) ;
#15748 = CARTESIAN_POINT ( 'NONE',  ( 161.3261849411383650, 273.2032229615781489, 15.91718547624222957 ) ) ;
#15749 = VERTEX_POINT ( 'NONE', #19510 ) ;
#15750 = CARTESIAN_POINT ( 'NONE',  ( 23.64814127513161068, 118.0650415295850308, 40.00000000000000000 ) ) ;
#15751 = CARTESIAN_POINT ( 'NONE',  ( 172.0418500013140033, 261.1904116954747224, 16.05919355830004847 ) ) ;
#15752 = DIRECTION ( 'NONE',  ( 0.8660254037844385966, 0.5000000000000002220, 3.252519625699450438E-16 ) ) ;
#15753 = CARTESIAN_POINT ( 'NONE',  ( 85.95899798769401912, 43.49248111663925442, 5.533741676130133236 ) ) ;
#15754 = EDGE_LOOP ( 'NONE', ( #86624, #73741, #30060, #69024 ) ) ;
#15755 = VERTEX_POINT ( 'NONE', #26588 ) ;
#15756 = ADVANCED_FACE ( 'NONE', ( #42259 ), #57461, .F. ) ;
#15757 = VECTOR ( 'NONE', #94283, 1000.000000000000114 ) ;
#15759 = CARTESIAN_POINT ( 'NONE',  ( 85.51332262388091010, 42.92838935012721180, -2.942937653912271578 ) ) ;
#15758 = CARTESIAN_POINT ( 'NONE',  ( 202.0119585509590934, 280.0399447494788205, 15.93797677053798623 ) ) ;
#15760 = ORIENTED_EDGE ( 'NONE', *, *, #81804, .T. ) ;
#15761 = CARTESIAN_POINT ( 'NONE',  ( 201.4066285247549786, 281.8004817444100354, -17.79749223817309201 ) ) ;
#15762 = DIRECTION ( 'NONE',  ( 0.2398044646550112069, 0.9708212084269294273, 0.000000000000000000 ) ) ;
#15763 = CARTESIAN_POINT ( 'NONE',  ( 72.84093999285123289, 56.97456911661188883, -16.40692799644482847 ) ) ;
#15764 = DIRECTION ( 'NONE',  ( -0.000000000000000000, -1.000000000000000000, -0.000000000000000000 ) ) ;
#15765 = ORIENTED_EDGE ( 'NONE', *, *, #37760, .F. ) ;
#15766 = CARTESIAN_POINT ( 'NONE',  ( 189.8171280724701546, 301.8740853621098950, -0.4360232994423257624 ) ) ;
#15767 = ADVANCED_FACE ( 'NONE', ( #80837 ), #50368, .T. ) ;
#15768 = EDGE_CURVE ( 'NONE', #90969, #70646, #34669, .T. ) ;
#15769 = VERTEX_POINT ( 'NONE', #73684 ) ;
#15770 = CARTESIAN_POINT ( 'NONE',  ( 195.8248271798537417, 291.4684452715354155, 17.35175160929494709 ) ) ;
#15771 = EDGE_CURVE ( 'NONE', #30236, #68451, #3523, .T. ) ;
#15772 = CARTESIAN_POINT ( 'NONE',  ( 164.2090401137261892, 246.2285947913476889, -5.787448100099915393 ) ) ;
#15773 = ORIENTED_EDGE ( 'NONE', *, *, #26322, .T. ) ;
#15774 = CARTESIAN_POINT ( 'NONE',  ( 26.79248755578709762, 33.65586893147757763, -7.433330006724137462 ) ) ;
#15775 = DIRECTION ( 'NONE',  ( -0.8660254037844379305, -0.5000000000000014433, -0.000000000000000000 ) ) ;
#15776 = LINE ( 'NONE', #7687, #27252 ) ;
#15777 = VERTEX_POINT ( 'NONE', #64079 ) ;
#15778 = CARTESIAN_POINT ( 'NONE',  ( -4.653128914090328472, 78.33390353417378549, 13.90751606465751777 ) ) ;
#15779 = CARTESIAN_POINT ( 'NONE',  ( 159.7588695950563817, 254.4119446770600064, 15.33386816469749903 ) ) ;
#15780 = DIRECTION ( 'NONE',  ( 1.000000000000000000, 0.000000000000000000, 0.000000000000000000 ) ) ;
#15781 = LINE ( 'NONE', #7692, #62456 ) ;
#15782 = ORIENTED_EDGE ( 'NONE', *, *, #99902, .F. ) ;
#15783 = VERTEX_POINT ( 'NONE', #35669 ) ;
#15784 = DIRECTION ( 'NONE',  ( -0.9347244501068304734, -0.3553733281669903543, 0.000000000000000000 ) ) ;
#15785 = PLANE ( 'NONE',  #84954 ) ;
#15786 = CARTESIAN_POINT ( 'NONE',  ( 190.4750160083620472, 300.7345900314585947, -1.159659205620361400 ) ) ;
#15787 = VECTOR ( 'NONE', #4892, 1000.000000000000000 ) ;
#15788 = EDGE_LOOP ( 'NONE', ( #84141, #91108, #7710 ) ) ;
#15789 = CARTESIAN_POINT ( 'NONE',  ( 149.6896757981861583, 271.3768714794653647, 12.49809796062302603 ) ) ;
#15790 = CARTESIAN_POINT ( 'NONE',  ( 170.7330658761331676, 275.4497203906630602, -16.60568353338077685 ) ) ;
#15791 = CARTESIAN_POINT ( 'NONE',  ( 161.8935665241663457, 250.2391126920490194, -13.69501063978231770 ) ) ;
#15792 = CARTESIAN_POINT ( 'NONE',  ( 147.5749551500760788, 275.0396750858066639, -4.254929048021584670 ) ) ;
#15793 = CARTESIAN_POINT ( 'NONE',  ( 161.3390181621638533, 256.5413485146231096, 15.77656010779211826 ) ) ;
#15794 = VECTOR ( 'NONE', #67800, 1000.000000000000114 ) ;
#15795 = CARTESIAN_POINT ( 'NONE',  ( 70.45330330358065396, 68.59310515512933648, 8.429446140656228437 ) ) ;
#15796 = CARTESIAN_POINT ( 'NONE',  ( 88.35671610020233402, 228.4865022471903160, 10.00000000000009415 ) ) ;
#15797 = CARTESIAN_POINT ( 'NONE',  ( 67.52858891722985391, 67.09395499530575080, 8.947318060521286753 ) ) ;
#15798 = CARTESIAN_POINT ( 'NONE',  ( 68.53194582573554783, 65.67665921644565685, -10.48464730244969800 ) ) ;
#15799 = CARTESIAN_POINT ( 'NONE',  ( 78.40134077247404321, 47.78707627181417905, 13.91009550459359900 ) ) ;
#15800 = AXIS2_PLACEMENT_3D ( 'NONE', #13161, #28846, #44014 ) ;
#15801 = CARTESIAN_POINT ( 'NONE',  ( 115.8441751185107478, 231.5643266524159856, 9.188101187500095079 ) ) ;
#15802 = ORIENTED_EDGE ( 'NONE', *, *, #61947, .F. ) ;
#15803 = CARTESIAN_POINT ( 'NONE',  ( 191.1747001918821525, 299.5227014763493116, -9.654804683100723040 ) ) ;
#15804 = CARTESIAN_POINT ( 'NONE',  ( 69.55597381272447421, 63.29032634764875098, 12.91558643708738252 ) ) ;
#15805 = CARTESIAN_POINT ( 'NONE',  ( 87.40678246761487458, 44.84425702272720571, -6.651126967624185760 ) ) ;
#15806 = PLANE ( 'NONE',  #66774 ) ;
#15807 = DIRECTION ( 'NONE',  ( -0.8660254037844379305, -0.5000000000000014433, -0.000000000000000000 ) ) ;
#15808 = CARTESIAN_POINT ( 'NONE',  ( 83.91859562547405460, 51.78473283747415934, -14.45112324054444564 ) ) ;
#15809 = CARTESIAN_POINT ( 'NONE',  ( 167.1442095974935569, 284.0302014969162769, -8.032154302468351048 ) ) ;
#15810 = EDGE_LOOP ( 'NONE', ( #17648, #1129, #54369, #36084 ) ) ;
#15811 = CARTESIAN_POINT ( 'NONE',  ( 72.13858704899024588, 72.77662068827325470, 2.033788753608857291E-15 ) ) ;
#15812 = AXIS2_PLACEMENT_3D ( 'NONE', #74680, #57950, #5256 ) ;
#15813 = CARTESIAN_POINT ( 'NONE',  ( 72.03640812230088386, 71.62847206889918539, 5.517176230632446554 ) ) ;
#15814 = CARTESIAN_POINT ( 'NONE',  ( 44.53222222597941027, 196.5177522451418781, -10.00000000000009592 ) ) ;
#15815 = CARTESIAN_POINT ( 'NONE',  ( 134.5719744753492364, 242.3768266524160140, -9.188101187500093303 ) ) ;
#15816 = CARTESIAN_POINT ( 'NONE',  ( 189.7493380202622291, 294.8126471784881915, -12.68491631734921299 ) ) ;
#15817 = AXIS2_PLACEMENT_3D ( 'NONE', #54123, #38935, #77468 ) ;
#15818 = CARTESIAN_POINT ( 'NONE',  ( 186.1974923302803973, 296.9264864461521256, 4.665697376584795109 ) ) ;
#15819 = CARTESIAN_POINT ( 'NONE',  ( 187.6338304778425936, 281.4993805173464807, -17.52881113060309204 ) ) ;
#15820 = CARTESIAN_POINT ( 'NONE',  ( 82.80564809338142140, 40.64392876451551473, -1.326136484204850197 ) ) ;
#15821 = CARTESIAN_POINT ( 'NONE',  ( 52.54321753458319932, 191.9548013555410080, -4.594050593750042211 ) ) ;
#15822 = CONICAL_SURFACE ( 'NONE', #14179, 10.00000000000000711, 0.7853981633974608245 ) ;
#15823 = CARTESIAN_POINT ( 'NONE',  ( 85.67146519243034675, 48.43225591334719837, -12.22341872913518301 ) ) ;
#15824 = VERTEX_POINT ( 'NONE', #20489 ) ;
#15825 = CARTESIAN_POINT ( 'NONE',  ( 71.81168878175323300, 65.89568737772486884, 12.05079262845972998 ) ) ;
#15826 = CARTESIAN_POINT ( 'NONE',  ( 88.06671310400491848, 44.64817415083963681, -4.178514498757152751 ) ) ;
#15827 = CARTESIAN_POINT ( 'NONE',  ( 155.8152618860606253, 260.7670451491295012, 0.000000000000000000 ) ) ;
#15828 = CARTESIAN_POINT ( 'NONE',  ( -19.65312891409030271, 93.06504152958497400, 60.00000000000000000 ) ) ;
#15829 = CARTESIAN_POINT ( 'NONE',  ( 151.3159053224887600, 278.6181574046168521, -1.690837018209672582 ) ) ;
#15830 = CARTESIAN_POINT ( 'NONE',  ( 183.5794699052420071, 296.1068241588955061, -6.177496795926971984 ) ) ;
#15831 = CARTESIAN_POINT ( 'NONE',  ( 178.4121483706975653, 261.1686503152587875, 12.25625725717337744 ) ) ;
#15832 = VECTOR ( 'NONE', #81546, 1000.000000000000114 ) ;
#15833 = CARTESIAN_POINT ( 'NONE',  ( 115.9793180381956716, 227.7677522451417929, -5.000000000000041744 ) ) ;
#15834 = DIRECTION ( 'NONE',  ( 0.5000000000000048850, -0.8660254037844358210, 0.000000000000000000 ) ) ;
#15835 = ORIENTED_EDGE ( 'NONE', *, *, #37375, .T. ) ;
#15836 = ADVANCED_FACE ( 'NONE', ( #12898 ), #82329, .F. ) ;
#15837 = CARTESIAN_POINT ( 'NONE',  ( 202.4017613376760494, 280.0768611521521620, 15.73960524502980540 ) ) ;
#15838 = CARTESIAN_POINT ( 'NONE',  ( 88.02404992778008364, 44.67257770573197462, 4.293538178122671134 ) ) ;
#15839 = CARTESIAN_POINT ( 'NONE',  ( 38.38920161542251464, 180.7202760586659451, -5.415160957724236172E-17 ) ) ;
#15840 = CARTESIAN_POINT ( 'NONE',  ( 9.637550907572093095, 29.65659080271449710, -1.878358725466461243E-16 ) ) ;
#15841 = CARTESIAN_POINT ( 'NONE',  ( 45.88188149789386472, 72.29567966924399514, 10.00000000000000000 ) ) ;
#15842 = FACE_OUTER_BOUND ( 'NONE', #59445, .T. ) ;
#15843 = CARTESIAN_POINT ( 'NONE',  ( 73.20446552614963309, 69.86374744967437778, 9.599577609524185817 ) ) ;
#15845 = CARTESIAN_POINT ( 'NONE',  ( 67.34675250658217749, 203.5643266524159856, -9.188101187500093303 ) ) ;
#15844 = CARTESIAN_POINT ( 'NONE',  ( 195.1280934431195249, 275.0822181618672175, -16.22170959459208461 ) ) ;
#15846 = CARTESIAN_POINT ( 'NONE',  ( 161.0952649348064938, 251.6218116045831437, 13.81854265722852482 ) ) ;
#15847 = CARTESIAN_POINT ( 'NONE',  ( 73.16956295240451880, 57.33411781474711688, 16.38320611732891408 ) ) ;
#15848 = ADVANCED_FACE ( 'NONE', ( #67060 ), #55811, .F. ) ;
#15849 = CARTESIAN_POINT ( 'NONE',  ( -29.49634561128635468, 95.76491754085807884, 44.62645301900288075 ) ) ;
#15850 = CARTESIAN_POINT ( 'NONE',  ( 17.31863740857695078, 12.12755873383625271, -6.180339887498949025 ) ) ;
#15851 =( BOUNDED_CURVE ( )  B_SPLINE_CURVE ( 2, ( #50532, #26752, #33875, #56128, #95198, #11567, #81489, #72880, #34349 ),
 .UNSPECIFIED., .F., .T. ) 
 B_SPLINE_CURVE_WITH_KNOTS ( ( 3, 2, 2, 2, 3 ),
 ( 0.3830645161290322509, 0.3844086021505376261, 0.3870967741935483764, 0.3897849462365591267, 0.3911290322580645018 ),
 .UNSPECIFIED. ) 
 CURVE ( )  GEOMETRIC_REPRESENTATION_ITEM ( )  RATIONAL_B_SPLINE_CURVE ( ( 0.9330127018922194093, 0.9330127018922194093, 1.000000000000000000, 0.8660254037844387076, 1.000000000000000000, 0.8660254037844387076, 1.000000000000000000, 0.9330127018922194093, 0.9330127018922194093 ) ) 
 REPRESENTATION_ITEM ( '' )  );
#15852 = ORIENTED_EDGE ( 'NONE', *, *, #62897, .T. ) ;
#15853 = ADVANCED_FACE ( 'NONE', ( #41515 ), #91905, .T. ) ;
#15854 = CARTESIAN_POINT ( 'NONE',  ( 164.5236374827232169, 268.7060415519879371, 16.63096613792822254 ) ) ;
#15855 = CARTESIAN_POINT ( 'NONE',  ( 38.12724268070496692, 179.4865022471901455, 1.119607411625061291E-15 ) ) ;
#15856 = CARTESIAN_POINT ( 'NONE',  ( 163.0309151244508712, 248.2691671304387739, 11.27270415168660200 ) ) ;
#15857 = CARTESIAN_POINT ( 'NONE',  ( 147.8871150585349881, 250.0643266524159287, -9.188101187500093303 ) ) ;
#15858 = CARTESIAN_POINT ( 'NONE',  ( 33.49394369984602804, 21.19860640527294038, 2.839279412974134775 ) ) ;
#15859 = CARTESIAN_POINT ( 'NONE',  ( 164.0938789702753411, 260.4145277690955140, -16.14174696660529307 ) ) ;
#15860 = CARTESIAN_POINT ( 'NONE',  ( 188.9667663523237024, 261.8616926428981628, 6.534948879020797463 ) ) ;
#15861 = CARTESIAN_POINT ( 'NONE',  ( 164.5648480107187197, 245.6123174360222094, 3.015887571020871238 ) ) ;
#15862 = CARTESIAN_POINT ( 'NONE',  ( 70.81858580497740263, 71.13538289942123072, 4.973410337506771306 ) ) ;
#15863 = CARTESIAN_POINT ( 'NONE',  ( 66.52957814384430435, 68.80191156052306667, 2.274549643663521969 ) ) ;
#15864 = VERTEX_POINT ( 'NONE', #99479 ) ;
#15865 = DIRECTION ( 'NONE',  ( 0.000000000000000000, 0.000000000000000000, 1.000000000000000000 ) ) ;
#15866 = AXIS2_PLACEMENT_3D ( 'NONE', #15267, #1096, #69484 ) ;
#15867 = CARTESIAN_POINT ( 'NONE',  ( 149.7543087857887656, 247.2677522451417929, -5.000000000000041744 ) ) ;
#15868 = CARTESIAN_POINT ( 'NONE',  ( -27.42236680055714260, 166.5217562850347406, 1.224646799147364892E-15 ) ) ;
#15869 = CARTESIAN_POINT ( 'NONE',  ( 17.70402515066951565, 13.14754757982089117, -5.678558825948275768 ) ) ;
#15870 = ORIENTED_EDGE ( 'NONE', *, *, #22958, .T. ) ;
#15871 = CARTESIAN_POINT ( 'NONE',  ( 206.9645602195919025, 272.1738616639552220, 7.969428354269253667 ) ) ;
#15872 = CARTESIAN_POINT ( 'NONE',  ( 88.29045754653738243, 44.33610290606567617, -2.255006784116474261 ) ) ;
#15873 = CARTESIAN_POINT ( 'NONE',  ( 71.55389639452418749, 72.40420208557205228, 1.000837480472114294 ) ) ;
#15874 = CARTESIAN_POINT ( 'NONE',  ( 152.8107382695299918, 265.9710327055011589, 16.32045346488711246 ) ) ;
#15875 = FACE_OUTER_BOUND ( 'NONE', #41022, .T. ) ;
#15876 = CARTESIAN_POINT ( 'NONE',  ( 163.4218292706009095, 247.5920839679097014, -10.44611490715852042 ) ) ;
#15877 = CARTESIAN_POINT ( 'NONE',  ( 200.9061540366740246, 282.6673289856585143, -18.13083321883407351 ) ) ;
#15878 = ORIENTED_EDGE ( 'NONE', *, *, #69578, .T. ) ;
#15879 = VECTOR ( 'NONE', #30098, 999.9999999999998863 ) ;
#15880 = EDGE_LOOP ( 'NONE', ( #43705, #10807, #51572, #57771 ) ) ;
#15881 = ADVANCED_FACE ( 'NONE', ( #49136 ), #56676, .F. ) ;
#15882 = CARTESIAN_POINT ( 'NONE',  ( 21.15788363470973366, 37.74176219324819215, 10.00000000000000000 ) ) ;
#15883 = CARTESIAN_POINT ( 'NONE',  ( 72.91019467649705632, 70.83288342014805039, 7.292254455461825380 ) ) ;
#15884 = ORIENTED_EDGE ( 'NONE', *, *, #22472, .T. ) ;
#15885 = CARTESIAN_POINT ( 'NONE',  ( 19.21972384509095733, 29.83478043621388309, -8.090169943749479842 ) ) ;
#15886 = CARTESIAN_POINT ( 'NONE',  ( 81.87732929995556219, 45.42932287087572973, -10.88775556568189629 ) ) ;
#15887 = ORIENTED_EDGE ( 'NONE', *, *, #67637, .F. ) ;
#15888 = CARTESIAN_POINT ( 'NONE',  ( -19.65312891409030271, 93.06504152958497400, 177.5919119679930134 ) ) ;
#15889 = CARTESIAN_POINT ( 'NONE',  ( 79.29973261757049841, 59.57579620614539806, -16.53044932756548846 ) ) ;
#15890 = VECTOR ( 'NONE', #54085, 1000.000000000000000 ) ;
#15891 = EDGE_CURVE ( 'NONE', #43419, #38467, #57710, .T. ) ;
#15892 = CARTESIAN_POINT ( 'NONE',  ( 14.26779446008844587, 16.43677371833800294, -10.00000000000000355 ) ) ;
#15893 = CARTESIAN_POINT ( 'NONE',  ( 85.37820560265511460, 47.12669036677656464, -11.24746114250747553 ) ) ;
#15894 = CARTESIAN_POINT ( 'NONE',  ( 69.95523204132881290, 62.90150226506938225, 13.86126985482015961 ) ) ;
#15895 = ORIENTED_EDGE ( 'NONE', *, *, #26890, .T. ) ;
#15896 = CARTESIAN_POINT ( 'NONE',  ( 203.6828132253460240, 277.8580141955760041, 15.80358291857228359 ) ) ;
#15897 = CARTESIAN_POINT ( 'NONE',  ( 137.7923328995641157, 240.3615022471902023, 5.000000000000051514 ) ) ;
#15898 = CARTESIAN_POINT ( 'NONE',  ( 191.5544531425776427, 298.8649500714207647, 8.366689293739112188 ) ) ;
#15899 = CARTESIAN_POINT ( 'NONE',  ( 102.3056452726415984, 218.3262482093457493, 3.021315404115420679E-15 ) ) ;
#15900 = B_SPLINE_SURFACE_WITH_KNOTS ( 'NONE', 3, 1, ( 
 ( #91029, #35789 ),
 ( #73800, #27205 ),
 ( #21113, #59059 ),
 ( #43379, #75808 ),
 ( #44376, #29198 ),
 ( #34783, #83424 ),
 ( #97140, #74818 ),
 ( #51991, #89075 ),
 ( #50483, #35290 ),
 ( #90543, #4906 ),
 ( #27709, #89549 ),
 ( #21593, #13990 ),
 ( #12008, #5889 ),
 ( #82930, #74323 ),
 ( #13506, #52476 ),
 ( #75308, #58092 ),
 ( #66197, #65684 ),
 ( #59567, #66686 ),
 ( #44869, #96640 ),
 ( #36779, #67687 ),
 ( #58576, #19625 ),
 ( #98616, #81438 ),
 ( #42866, #90030 ),
 ( #4391, #97619 ),
 ( #20111, #50980 ),
 ( #81932, #12508 ),
 ( #20604, #13016 ),
 ( #43876, #5398 ),
 ( #36282, #67181 ),
 ( #98105, #28687 ),
 ( #22580, #93516 ) ),
 .UNSPECIFIED., .F., .F., .F.,
 ( 4, 3, 3, 3, 3, 3, 3, 3, 3, 3, 4 ),
 ( 2, 2 ),
 ( 0.000000000000000000, 0.1333490885032312667, 0.3007194338854344284, 0.4699862290245184759, 0.5844252810809397181, 0.6686540514502811172, 0.7354980260655615831, 0.8028463152565572525, 0.8633854507757208196, 0.9437142632667274711, 1.000000000000000000 ),
 ( 0.000000000000000000, 1.000000000000000000 ),
 .UNSPECIFIED. ) ;
#15901 = ORIENTED_EDGE ( 'NONE', *, *, #100085, .F. ) ;
#15902 = EDGE_CURVE ( 'NONE', #89249, #36835, #34886, .T. ) ;
#15903 = EDGE_LOOP ( 'NONE', ( #74102, #22754, #32143, #46101 ) ) ;
#15904 = EDGE_LOOP ( 'NONE', ( #34238, #21935, #8811, #86497 ) ) ;
#15905 = CARTESIAN_POINT ( 'NONE',  ( 74.55670760492021998, 66.78977310388269473, 12.65506860017463175 ) ) ;
#15906 = VERTEX_POINT ( 'NONE', #82072 ) ;
#15907 = DIRECTION ( 'NONE',  ( -0.000000000000000000, 0.000000000000000000, -1.000000000000000000 ) ) ;
#15908 = VERTEX_POINT ( 'NONE', #23690 ) ;
#15909 = CARTESIAN_POINT ( 'NONE',  ( 208.0045976720423084, 270.3724639545367836, 2.002128742561712471 ) ) ;
#15910 = VECTOR ( 'NONE', #13655, 1000.000000000000000 ) ;
#15911 = CARTESIAN_POINT ( 'NONE',  ( 82.57448465555356165, 47.03648843181296257, 11.94445601533793422 ) ) ;
#15912 = CARTESIAN_POINT ( 'NONE',  ( 165.0407670381244145, 270.9616198530111433, 16.81988890767253864 ) ) ;
#15913 = DIRECTION ( 'NONE',  ( 0.4999999999999998890, -0.8660254037844385966, 0.000000000000000000 ) ) ;
#15914 = CARTESIAN_POINT ( 'NONE',  ( 148.2352135776142177, 273.8960739431854563, -9.245976304249309052 ) ) ;
#15915 = CARTESIAN_POINT ( 'NONE',  ( 174.6053779230379632, 290.0266613665239106, 6.313546118724348233 ) ) ;
#15916 = CARTESIAN_POINT ( 'NONE',  ( 158.9428945936735715, 255.3498263921298985, -17.51518199015400512 ) ) ;
#15917 = FACE_OUTER_BOUND ( 'NONE', #63871, .T. ) ;
#15918 = CARTESIAN_POINT ( 'NONE',  ( 14.66813190280496570, 26.65586893147755276, -7.433330006724137462 ) ) ;
#15919 = VECTOR ( 'NONE', #98723, 1000.000000000000000 ) ;
#15920 = FACE_OUTER_BOUND ( 'NONE', #45808, .T. ) ;
#15921 = CARTESIAN_POINT ( 'NONE',  ( 80.02165461388095480, 57.57226732806288538, 16.59957571444259017 ) ) ;
#15923 = ORIENTED_EDGE ( 'NONE', *, *, #54019, .F. ) ;
#15922 = CARTESIAN_POINT ( 'NONE',  ( 198.3449891235413531, 287.1033967417670283, 16.95540786497457120 ) ) ;
#15924 = CARTESIAN_POINT ( 'NONE',  ( 191.1269952354458610, 299.6053288846700866, 6.026773553208284007 ) ) ;
#15925 = DIRECTION ( 'NONE',  ( -1.000000000000000000, -9.785293164091933533E-14, 0.000000000000000000 ) ) ;
#15926 = CARTESIAN_POINT ( 'NONE',  ( 159.5221561062548972, 254.3465160214695118, -16.91023001054109542 ) ) ;
#15927 = DIRECTION ( 'NONE',  ( 0.4999999999999998890, -0.8660254037844385966, 0.000000000000000000 ) ) ;
#15928 = CARTESIAN_POINT ( 'NONE',  ( 68.04067724501535963, 66.09559063115733579, -10.49573481652158335 ) ) ;
#15929 = EDGE_CURVE ( 'NONE', #17145, #22043, #45760, .T. ) ;
#15930 = CARTESIAN_POINT ( 'NONE',  ( 170.8004095096928836, 255.2646207969754357, 11.24633423646908703 ) ) ;
#15931 = CARTESIAN_POINT ( 'NONE',  ( 159.4594236750365326, 281.8839243825340191, 2.078914130625487910 ) ) ;
#15932 = EDGE_LOOP ( 'NONE', ( #7580, #9185, #65774, #51167 ) ) ;
#15933 = CARTESIAN_POINT ( 'NONE',  ( 155.7713280489876695, 260.8431407871109968, -18.06005460683174491 ) ) ;
#15934 = CARTESIAN_POINT ( 'NONE',  ( -22.42236680055709641, 157.8615022471902591, 0.000000000000000000 ) ) ;
#15936 = EDGE_CURVE ( 'NONE', #69110, #23277, #77427, .T. ) ;
#15935 = DIRECTION ( 'NONE',  ( 0.4999999999999992784, -0.8660254037844390407, 0.000000000000000000 ) ) ;
#15937 = CARTESIAN_POINT ( 'NONE',  ( 3.035171627975005837, 185.8927522451419350, 2.944929066748280225E-16 ) ) ;
#15938 = CARTESIAN_POINT ( 'NONE',  ( 91.59511671678144751, 229.8149278399160949, 9.188101187500093303 ) ) ;
#15939 = CARTESIAN_POINT ( 'NONE',  ( 82.47990923055493795, 40.99821503651507015, -1.212878302331509728 ) ) ;
#15940 = CIRCLE ( 'NONE', #11205, 11.89249999999999652 ) ;
#15941 = DIRECTION ( 'NONE',  ( -0.8660254037844392627, -0.4999999999999987232, 0.000000000000000000 ) ) ;
#15942 = CARTESIAN_POINT ( 'NONE',  ( 164.0095377641384857, 246.5741429970625802, -8.745455945562961020 ) ) ;
#15943 = VECTOR ( 'NONE', #26428, 1000.000000000000000 ) ;
#15944 = CARTESIAN_POINT ( 'NONE',  ( 72.42968441479126795, 70.75204143367579945, 7.711333220305022884 ) ) ;
#15946 = CARTESIAN_POINT ( 'NONE',  ( 75.69465226566293836, 65.43705427022661070, 14.28313312794709589 ) ) ;
#15945 = CARTESIAN_POINT ( 'NONE',  ( 5.858601742122021783, 180.3149278399161233, 9.188101187500093303 ) ) ;
#15947 = CARTESIAN_POINT ( 'NONE',  ( 181.4577051398952108, 255.5722452524177299, 4.229640769421640911 ) ) ;
#15948 = ORIENTED_EDGE ( 'NONE', *, *, #84676, .T. ) ;
#15949 = AXIS2_PLACEMENT_3D ( 'NONE', #9932, #31206, #62597 ) ;
#15950 = VERTEX_POINT ( 'NONE', #45985 ) ;
#15951 = CARTESIAN_POINT ( 'NONE',  ( 25.96864935082048831, 154.0458036431183189, 21.50000000000008527 ) ) ;
#15952 = CARTESIAN_POINT ( 'NONE',  ( 201.3212028412432062, 267.0810577319301160, -3.784738031960614091 ) ) ;
#15953 = DIRECTION ( 'NONE',  ( 0.4999999999999998890, -0.8660254037844385966, 0.000000000000000000 ) ) ;
#15954 = CARTESIAN_POINT ( 'NONE',  ( 202.7185166046502331, 279.5282249361877120, -16.86058306256609640 ) ) ;
#15955 = AXIS2_PLACEMENT_3D ( 'NONE', #20006, #12917, #74721 ) ;
#15956 = CARTESIAN_POINT ( 'NONE',  ( 94.62744204236609846, 213.8932355074535394, -2.679491924311248496 ) ) ;
#15957 = CARTESIAN_POINT ( 'NONE',  ( 169.8466615877324841, 251.3021325278160134, 9.294982655322041154 ) ) ;
#15958 = CARTESIAN_POINT ( 'NONE',  ( 35.03300607999280913, 191.0333772461660544, 9.188101187500095079 ) ) ;
#15959 = CARTESIAN_POINT ( 'NONE',  ( 122.7720312530212396, 247.8149278399160949, 9.188101187500093303 ) ) ;
#15960 = FACE_OUTER_BOUND ( 'NONE', #45661, .T. ) ;
#15961 = ORIENTED_EDGE ( 'NONE', *, *, #18900, .T. ) ;
#15962 = CARTESIAN_POINT ( 'NONE',  ( 150.4814168194272099, 271.9348575896366924, -11.67596527614399982 ) ) ;
#15963 = FACE_OUTER_BOUND ( 'NONE', #69956, .T. ) ;
#15964 = VECTOR ( 'NONE', #46095, 1000.000000000000000 ) ;
#15965 = CARTESIAN_POINT ( 'NONE',  ( 170.3178023250738420, 289.0326318653803241, -4.561300590322002080 ) ) ;
#15966 = CARTESIAN_POINT ( 'NONE',  ( -110.0000000000000426, 0.000000000000000000, -9.212605237762121035 ) ) ;
#15967 = CARTESIAN_POINT ( 'NONE',  ( 193.9844289374573520, 294.6561085335266625, 15.49818881749970245 ) ) ;
#15968 = CARTESIAN_POINT ( 'NONE',  ( 207.8232941427535536, 270.6864908788566026, -6.505149060073906142 ) ) ;
#15969 = CARTESIAN_POINT ( 'NONE',  ( 194.3442947553755005, 294.0328026529847421, -15.97648891113594871 ) ) ;
#15970 = CARTESIAN_POINT ( 'NONE',  ( 148.3874010092782498, 273.6324775792697892, -8.328854486678444857 ) ) ;
#15971 = CARTESIAN_POINT ( 'NONE',  ( 72.46146760938286491, 66.06259922122619344, 12.76239748237539473 ) ) ;
#15972 = CARTESIAN_POINT ( 'NONE',  ( 74.05623475345210238, 67.87786276047000911, -11.59565021290446651 ) ) ;
#15973 = CARTESIAN_POINT ( 'NONE',  ( -22.42236680055709641, 157.8615022471902591, 0.000000000000000000 ) ) ;
#15974 = ADVANCED_FACE ( 'NONE', ( #47011 ), #54585, .T. ) ;
#15975 = CARTESIAN_POINT ( 'NONE',  ( 71.06456094586361871, 71.36015830129700532, 3.098779000439031428 ) ) ;
#15977 = B_SPLINE_CURVE_WITH_KNOTS ( 'NONE', 3,
 ( #12803, #43667, #19421, #35073, #65480, #65979, #58369, #2707, #56873, #87857, #49783, #49292, #80231, #89345, #72616, #95937 ),
 .UNSPECIFIED., .F., .F.,
 ( 4, 2, 2, 2, 2, 2, 2, 4 ),
 ( 0.000000000000000000, 0.0003786681000626436911, 0.0007573362001252873822, 0.001136004300187931073, 0.001514672400250574764, 0.001893340500313218456, 0.002272008600375862147, 0.003029344800501141289 ),
 .UNSPECIFIED. ) ;
#15976 = CARTESIAN_POINT ( 'NONE',  ( 190.0515794655415789, 301.4680036374047063, -1.296825456579539626 ) ) ;
#15978 = PLANE ( 'NONE',  #90085 ) ;
#15979 = CARTESIAN_POINT ( 'NONE',  ( 152.7901873964250115, 266.7870861983042801, -15.84272339013448949 ) ) ;
#15980 = EDGE_CURVE ( 'NONE', #94954, #43596, #71164, .T. ) ;
#15981 = CARTESIAN_POINT ( 'NONE',  ( 163.7085541710205234, 247.0954618725873217, -6.713544974106887331 ) ) ;
#15983 = EDGE_CURVE ( 'NONE', #39764, #30496, #51573, .T. ) ;
#15982 = CARTESIAN_POINT ( 'NONE',  ( 182.6387802082273879, 268.5597891637301586, 15.04617342855019047 ) ) ;
#15984 = CARTESIAN_POINT ( 'NONE',  ( 112.6237299221286321, 226.6423013555409796, -4.594050593750043987 ) ) ;
#15985 = CARTESIAN_POINT ( 'NONE',  ( 10.20631340951632104, 27.93396525600388713, 2.839279412974139660 ) ) ;
#15986 = CARTESIAN_POINT ( 'NONE',  ( 191.5451565139252068, 298.8810523045859213, 7.782291334092181323 ) ) ;
#15987 = DIRECTION ( 'NONE',  ( -1.000000000000000000, 0.000000000000000000, 0.000000000000000000 ) ) ;
#15989 = CARTESIAN_POINT ( 'NONE',  ( 193.7944905295941567, 278.3514127848527551, 16.31057853467515173 ) ) ;
#15988 = CARTESIAN_POINT ( 'NONE',  ( 12.48001537019352369, 22.90829794293879473, 10.00000000000000355 ) ) ;
#15990 = CARTESIAN_POINT ( 'NONE',  ( 190.8671785295675818, 300.0553446199063501, -7.998068249277817898 ) ) ;
#15991 = B_SPLINE_CURVE_WITH_KNOTS ( 'NONE', 3,
 ( #56987, #95565, #9404, #80348 ),
 .UNSPECIFIED., .F., .F.,
 ( 4, 4 ),
 ( 0.007815255211040535860, 0.01599263494101685681 ),
 .UNSPECIFIED. ) ;
#15992 = CARTESIAN_POINT ( 'NONE',  ( 150.7133245577828689, 269.6038598187387834, -14.58664962216439598 ) ) ;
#15993 = CARTESIAN_POINT ( 'NONE',  ( 142.1224599184862711, 252.8615022471902307, -10.00000000000009592 ) ) ;
#15994 = CARTESIAN_POINT ( 'NONE',  ( 82.06353261700769508, 41.00057011406286733, -2.892018250819532454 ) ) ;
#15995 = CARTESIAN_POINT ( 'NONE',  ( 38.43992769770077444, 34.14441083166263979, 10.00000000000000533 ) ) ;
#15996 = CARTESIAN_POINT ( 'NONE',  ( 30.80155721116056355, 46.36891074996812989, -10.00000000000000000 ) ) ;
#15997 = ORIENTED_EDGE ( 'NONE', *, *, #28444, .T. ) ;
#15998 = CARTESIAN_POINT ( 'NONE',  ( 192.9843945815383108, 267.1901746418614039, 11.24122804034830203 ) ) ;
#15999 = CARTESIAN_POINT ( 'NONE',  ( 70.99925208767550089, 64.35626315177518109, -13.34609736598558172 ) ) ;
#16000 = CARTESIAN_POINT ( 'NONE',  ( 80.93303655709135569, 47.13181478245343925, 13.26053224286359544 ) ) ;
#16001 = ORIENTED_EDGE ( 'NONE', *, *, #17356, .F. ) ;
#16002 = CARTESIAN_POINT ( 'NONE',  ( 86.10128179547638183, 47.01522930412664181, 10.71950609365847384 ) ) ;
#16003 = CARTESIAN_POINT ( 'NONE',  ( 183.2250948126493881, 264.4847478218908918, -13.17622970261022530 ) ) ;
#16004 = DIRECTION ( 'NONE',  ( -0.8660254037844378194, -0.5000000000000014433, -0.000000000000000000 ) ) ;
#16005 = DIRECTION ( 'NONE',  ( -0.4805540241036398430, -0.8769651246872924855, 0.000000000000000000 ) ) ;
#16006 = VERTEX_POINT ( 'NONE', #63712 ) ;
#16007 = EDGE_CURVE ( 'NONE', #24573, #29268, #63209, .T. ) ;
#16008 = CARTESIAN_POINT ( 'NONE',  ( 187.2487605686656309, 278.8013110013918094, 17.16344444290080418 ) ) ;
#16009 = AXIS2_PLACEMENT_3D ( 'NONE', #66538, #12354, #34638 ) ;
#16010 = CARTESIAN_POINT ( 'NONE',  ( 44.10936046141049616, 26.26216523072498887, -2.296566073217252530E-15 ) ) ;
#16011 = VERTEX_POINT ( 'NONE', #55586 ) ;
#16012 = CARTESIAN_POINT ( 'NONE',  ( 167.6769706185343409, 249.8146627436505867, 6.781605082613990199 ) ) ;
#16013 = ADVANCED_FACE ( 'NONE', ( #86570 ), #7499, .T. ) ;
#16014 = FACE_OUTER_BOUND ( 'NONE', #48619, .T. ) ;
#16015 = VERTEX_POINT ( 'NONE', #47998 ) ;
#16016 = AXIS2_PLACEMENT_3D ( 'NONE', #25709, #64703, #78412 ) ;
#16017 = CARTESIAN_POINT ( 'NONE',  ( 86.22341231051544241, 46.94107917315361078, -10.56950783746433764 ) ) ;
#16018 = CARTESIAN_POINT ( 'NONE',  ( 159.1305474299093135, 255.0248021455850846, 16.88467499060716648 ) ) ;
#16019 = CYLINDRICAL_SURFACE ( 'NONE', #31565, 17.82106496071139645 ) ;
#16020 = CARTESIAN_POINT ( 'NONE',  ( 80.44297273216874089, 44.73620253192707708, -11.65665792466250039 ) ) ;
#16021 = VECTOR ( 'NONE', #7734, 1000.000000000000000 ) ;
#16022 = VECTOR ( 'NONE', #43217, 1000.000000000000000 ) ;
#16023 = CARTESIAN_POINT ( 'NONE',  ( 44.74566838383860556, 28.76004757982093807, 5.678558825948272215 ) ) ;
#16024 = CARTESIAN_POINT ( 'NONE',  ( 148.1316126177475496, 276.0755160693871630, 5.020219949272568094 ) ) ;
#16025 = ORIENTED_EDGE ( 'NONE', *, *, #70870, .F. ) ;
#16026 = CARTESIAN_POINT ( 'NONE',  ( 162.6619436536031174, 249.4045681345386072, 10.74432698607139614 ) ) ;
#16027 = ORIENTED_EDGE ( 'NONE', *, *, #57557, .F. ) ;
#16028 = CARTESIAN_POINT ( 'NONE',  ( 77.13982593033820478, 49.36145032405385535, -14.90501067692936310 ) ) ;
#16029 = VERTEX_POINT ( 'NONE', #85043 ) ;
#16030 = CARTESIAN_POINT ( 'NONE',  ( 169.8597199083751832, 269.3794817305624747, 17.64580905768150032 ) ) ;
#16032 = CARTESIAN_POINT ( 'NONE',  ( 78.40326579531324569, 49.68334333693088212, 14.77346682042102621 ) ) ;
#16031 = VECTOR ( 'NONE', #65607, 999.9999999999998863 ) ;
#16033 = ORIENTED_EDGE ( 'NONE', *, *, #3619, .F. ) ;
#16034 = PLANE ( 'NONE',  #84801 ) ;
#16035 = CARTESIAN_POINT ( 'NONE',  ( 206.3559632282955647, 273.2279825742143089, -11.28941701449801904 ) ) ;
#16036 = CARTESIAN_POINT ( 'NONE',  ( 190.4649878924934683, 300.7519592376469291, 1.979076455900417919 ) ) ;
#16037 = CARTESIAN_POINT ( 'NONE',  ( 190.0340467409721441, 301.4983712071542641, 4.077645795029533282 ) ) ;
#16038 = CARTESIAN_POINT ( 'NONE',  ( 79.25874806327021815, 46.14125615598921115, 12.64021366946045433 ) ) ;
#16039 = CARTESIAN_POINT ( 'NONE',  ( 170.8196951477767982, 250.8282041339933244, -5.540778955988154841 ) ) ;
#16040 = DIRECTION ( 'NONE',  ( -1.000000000000000000, 0.000000000000000000, 0.000000000000000000 ) ) ;
#16041 = CARTESIAN_POINT ( 'NONE',  ( 183.4484973779139523, 284.6930032971759488, -15.01462800346279280 ) ) ;
#16042 = B_SPLINE_CURVE_WITH_KNOTS ( 'NONE', 3,
 ( #37945, #52160, #68856, #83108 ),
 .UNSPECIFIED., .F., .F.,
 ( 4, 4 ),
 ( 8.774936542010898348E-05, 0.008022331835684331364 ),
 .UNSPECIFIED. ) ;
#16043 = CARTESIAN_POINT ( 'NONE',  ( 130.0524911732904343, 236.7048013555409796, 4.594050593750051981 ) ) ;
#16044 = CARTESIAN_POINT ( 'NONE',  ( 186.9756763787170257, 262.2700035475498339, -10.24646055643486520 ) ) ;
#16045 = CARTESIAN_POINT ( 'NONE',  ( 161.2265274951298863, 283.7633814984351375, 2.173529036228213140 ) ) ;
#16046 = CARTESIAN_POINT ( 'NONE',  ( 180.5872800571609389, 291.4665845829162549, -9.750679543141076877 ) ) ;
#16047 = EDGE_CURVE ( 'NONE', #32489, #43945, #22719, .T. ) ;
#16048 = EDGE_LOOP ( 'NONE', ( #69460, #32230, #25895, #72622 ) ) ;
#16049 = VECTOR ( 'NONE', #14382, 1000.000000000000227 ) ;
#16050 = CARTESIAN_POINT ( 'NONE',  ( 200.0716132454348894, 273.8135256567975375, 13.71647348634510877 ) ) ;
#16051 = CARTESIAN_POINT ( 'NONE',  ( 178.8491990207230344, 254.9654333574110012, 1.324507615027452845 ) ) ;
#16052 = CARTESIAN_POINT ( 'NONE',  ( -12.68721568607400485, 24.67147432707382748, -10.00000000000000000 ) ) ;
#16053 = CARTESIAN_POINT ( 'NONE',  ( 206.7325995683429767, 270.5756292972641859, -5.459556455514786855 ) ) ;
#16054 = CARTESIAN_POINT ( 'NONE',  ( 71.76582198392000578, 60.80067951720612029, 14.81518451064557063 ) ) ;
#16055 = CARTESIAN_POINT ( 'NONE',  ( 201.1388841337167435, 282.2642286331299601, -18.17233400608081340 ) ) ;
#16056 = CARTESIAN_POINT ( 'NONE',  ( 78.54814453918285722, 52.73914818458334963, 16.14325216142513497 ) ) ;
#16057 = DIRECTION ( 'NONE',  ( -1.000000000000000000, -1.156482317317871331E-15, 0.000000000000000000 ) ) ;
#16058 = CARTESIAN_POINT ( 'NONE',  ( 156.0507216674837707, 279.5060275253360373, 7.618106348741741307 ) ) ;
#16059 = VERTEX_POINT ( 'NONE', #53598 ) ;
#16060 = CARTESIAN_POINT ( 'NONE',  ( 194.6310785344323904, 293.5360785768717165, -14.54510914272505495 ) ) ;
#16061 = CARTESIAN_POINT ( 'NONE',  ( 152.8623378685196030, 273.8643641423199711, 12.12982893395569306 ) ) ;
#16062 = ORIENTED_EDGE ( 'NONE', *, *, #13762, .F. ) ;
#16063 = CARTESIAN_POINT ( 'NONE',  ( 188.0407104400106846, 266.0414501920158727, -11.72547689681096905 ) ) ;
#16064 = CARTESIAN_POINT ( 'NONE',  ( 156.9004364869687436, 276.5848328012408501, 10.23493742149738672 ) ) ;
#16065 = CARTESIAN_POINT ( 'NONE',  ( 195.7309803721981609, 265.3211447974111934, 4.250103213233941801 ) ) ;
#16066 = CARTESIAN_POINT ( 'NONE',  ( 190.0340467409721441, 301.4983712071542641, 4.077645795029533282 ) ) ;
#16067 = CARTESIAN_POINT ( 'NONE',  ( 204.6508828921556074, 273.0178721416635881, -9.847606913800847295 ) ) ;
#16069 = CARTESIAN_POINT ( 'NONE',  ( 151.4352391397386555, 275.0282326485918247, -9.505706171079989275 ) ) ;
#16068 = CARTESIAN_POINT ( 'NONE',  ( 164.2092836438689005, 283.3451842658567443, -6.697959257182540149 ) ) ;
#16070 = CARTESIAN_POINT ( 'NONE',  ( 200.9521687275011175, 282.5876292032514243, -18.16013154125647944 ) ) ;
#16071 = ORIENTED_EDGE ( 'NONE', *, *, #7409, .T. ) ;
#16072 = CARTESIAN_POINT ( 'NONE',  ( 204.8438479865957333, 272.6835259793063528, -9.477213056041572159 ) ) ;
#16073 = CARTESIAN_POINT ( 'NONE',  ( 71.98782200592057734, 64.37985811868047392, 13.14021211575542836 ) ) ;
#16074 = CARTESIAN_POINT ( 'NONE',  ( 186.7654524502822539, 262.6710075733441272, -8.886537497778370209 ) ) ;
#16075 = CARTESIAN_POINT ( 'NONE',  ( 192.3193821777917947, 275.6344104414516778, -15.92451825442405955 ) ) ;
#16076 = CARTESIAN_POINT ( 'NONE',  ( 2.814886498931689296, 38.86145383009443321, 59.99999999999999289 ) ) ;
#16077 = CARTESIAN_POINT ( 'NONE',  ( 162.5887743522035294, 284.9919049736276975, -2.844505511527740005 ) ) ;
#16078 = CARTESIAN_POINT ( 'NONE',  ( 153.1164404339926080, 265.4415410246681972, 16.15325778160653414 ) ) ;
#16079 = CARTESIAN_POINT ( 'NONE',  ( 201.5036534377215958, 270.3153034880852488, -10.25451236307256409 ) ) ;
#16080 = CARTESIAN_POINT ( 'NONE',  ( 74.40269252765078534, 68.37285155744012854, 11.32427007268841912 ) ) ;
#16081 = CARTESIAN_POINT ( 'NONE',  ( 71.39461857329790462, 71.57943448657258045, -3.153141937835415742 ) ) ;
#16082 = CARTESIAN_POINT ( 'NONE',  ( 67.87888135928258748, 66.79448504996196334, -9.615113643841004532 ) ) ;
#16083 = CARTESIAN_POINT ( 'NONE',  ( 89.53865347855843027, 216.3768266524159856, 9.188101187500098632 ) ) ;
#16084 = PLANE ( 'NONE',  #662 ) ;
#16085 = CARTESIAN_POINT ( 'NONE',  ( 193.1444937042664094, 296.1109190324805240, -12.15243020627156767 ) ) ;
#16086 = CARTESIAN_POINT ( 'NONE',  ( 163.3939361803663246, 247.6403962173759226, -10.78041711314006790 ) ) ;
#16088 = CARTESIAN_POINT ( 'NONE',  ( 155.4495868485232108, 261.4004128932040203, -18.48326470492642315 ) ) ;
#16087 = VECTOR ( 'NONE', #26217, 1000.000000000000000 ) ;
#16089 = VECTOR ( 'NONE', #45606, 1000.000000000000000 ) ;
#16090 = CARTESIAN_POINT ( 'NONE',  ( 78.47204957586916407, 57.63415352787896495, 16.22432601261093765 ) ) ;
#16091 = CARTESIAN_POINT ( 'NONE',  ( 84.85515811532782493, 50.28810280189843240, -13.38803942659112423 ) ) ;
#16092 = CARTESIAN_POINT ( 'NONE',  ( 78.00383892016681386, 61.98526604297752129, 15.67820829689503270 ) ) ;
#16094 = CARTESIAN_POINT ( 'NONE',  ( 75.91040063343092470, 51.47081534094227351, 15.69546924919345088 ) ) ;
#16093 = CARTESIAN_POINT ( 'NONE',  ( 73.38763933171604492, 69.17329012685399903, -9.958834189398086068 ) ) ;
#16095 = CARTESIAN_POINT ( 'NONE',  ( 161.7570549189561859, 250.4755577280957652, 14.23709397115338682 ) ) ;
#16096 = CARTESIAN_POINT ( 'NONE',  ( 196.9080397933726942, 269.7016881256661804, 12.39056067425276630 ) ) ;
#16097 = CARTESIAN_POINT ( 'NONE',  ( 205.0902471979347581, 275.4202670467537359, -13.79912452887783303 ) ) ;
#16098 = EDGE_CURVE ( 'NONE', #10423, #17015, #9530, .T. ) ;
#16099 = CARTESIAN_POINT ( 'NONE',  ( 196.1241105319816143, 290.9500712997905794, 15.97146679939154268 ) ) ;
#16100 = CARTESIAN_POINT ( 'NONE',  ( 190.1321413272149812, 298.8808762037565430, -8.148410351609143731 ) ) ;
#16101 = CARTESIAN_POINT ( 'NONE',  ( 161.5757715694810770, 250.7895496999525449, -14.51803553215175135 ) ) ;
#16102 = ADVANCED_FACE ( 'NONE', ( #54089 ), #17616, .T. ) ;
#16103 = VECTOR ( 'NONE', #61095, 1000.000000000000000 ) ;
#16104 = CARTESIAN_POINT ( 'NONE',  ( 29.07873433320978052, 199.8464784336661353, 1.353441290958777327E-15 ) ) ;
#16105 = ADVANCED_FACE ( 'NONE', ( #71834 ), #41903, .F. ) ;
#16106 = CARTESIAN_POINT ( 'NONE',  ( 60.25564886944957976, 217.8464784336661637, 1.353441290958777327E-15 ) ) ;
#16107 = DIRECTION ( 'NONE',  ( -1.000000000000000000, 0.000000000000000000, 0.000000000000000000 ) ) ;
#16108 = CARTESIAN_POINT ( 'NONE',  ( 88.25809008468522165, 43.73205518618092214, 0.2003341539982116393 ) ) ;
#16109 = DIRECTION ( 'NONE',  ( 1.000000000000000000, 4.999968693044007408E-13, 0.000000000000000000 ) ) ;
#16110 = CARTESIAN_POINT ( 'NONE',  ( 146.6963301283313967, 249.3768266524160140, 9.188101187500098632 ) ) ;
#16112 = CARTESIAN_POINT ( 'NONE',  ( 77.07877823284091789, 49.44627466125040627, 15.45926714762989995 ) ) ;
#16111 = PLANE ( 'NONE',  #12867 ) ;
#16114 = AXIS2_PLACEMENT_3D ( 'NONE', #12535, #97164, #27730 ) ;
#16113 = CARTESIAN_POINT ( 'NONE',  ( 44.44706364856356373, 64.93738052781137071, 177.5919119679930134 ) ) ;
#16115 = CARTESIAN_POINT ( 'NONE',  ( 23.51484842749693627, 36.68290643055188838, 3.479690158560446702E-15 ) ) ;
#16116 = CARTESIAN_POINT ( 'NONE',  ( 136.7639277290221855, 239.7677522451417929, -5.000000000000041744 ) ) ;
#16117 = CARTESIAN_POINT ( 'NONE',  ( 82.21566304485764931, 47.23221333006363665, -12.24838049750184865 ) ) ;
#16118 = CARTESIAN_POINT ( 'NONE',  ( 12.64980493759981250, 22.70171378149918340, -9.188101187500004485 ) ) ;
#16119 = CARTESIAN_POINT ( 'NONE',  ( 63.01627839189497138, 213.3149278399160949, 9.188101187500093303 ) ) ;
#16120 = CARTESIAN_POINT ( 'NONE',  ( 77.05907617643467233, 63.75643696445189335, 14.97702801636213543 ) ) ;
#16121 = DIRECTION ( 'NONE',  ( -0.8660254037844387076, -0.4999999999999998890, -0.000000000000000000 ) ) ;
#16122 = CARTESIAN_POINT ( 'NONE',  ( 159.5764336135613632, 254.2525046211064819, 15.32981087583629076 ) ) ;
#16123 = FACE_OUTER_BOUND ( 'NONE', #76108, .T. ) ;
#16124 = CARTESIAN_POINT ( 'NONE',  ( 201.4731444478667015, 281.6852727860684240, 16.40638429239196938 ) ) ;
#16125 = CARTESIAN_POINT ( 'NONE',  ( 80.56811894275233499, 54.89951299323676182, -15.91924062418832087 ) ) ;
#16126 = CARTESIAN_POINT ( 'NONE',  ( 108.4196379545419120, 226.7365022471902307, -10.00000000000009059 ) ) ;
#16127 = CARTESIAN_POINT ( 'NONE',  ( 181.7815785431583038, 276.1505370498239813, -17.81783396216490445 ) ) ;
#16128 = CARTESIAN_POINT ( 'NONE',  ( 207.6727254509676186, 270.9472835030587703, 7.315149605389819953 ) ) ;
#16129 = ORIENTED_EDGE ( 'NONE', *, *, #10322, .F. ) ;
#16130 = CARTESIAN_POINT ( 'NONE',  ( 77.26634761542135266, 49.24219256474607676, 15.35008689065183418 ) ) ;
#16131 = CARTESIAN_POINT ( 'NONE',  ( 82.09463905232223624, 54.09232422927597383, 15.61698559803690145 ) ) ;
#16132 = ORIENTED_EDGE ( 'NONE', *, *, #69593, .T. ) ;
#16133 = CARTESIAN_POINT ( 'NONE',  ( 206.8791291248445532, 272.3218326606039454, -10.16823074922856840 ) ) ;
#16134 = CARTESIAN_POINT ( 'NONE',  ( 190.1532766730107085, 279.2606816812074726, -17.72189159620656440 ) ) ;
#16135 = CARTESIAN_POINT ( 'NONE',  ( 69.28962944736927909, 68.84243576899710604, -6.877947330648720659 ) ) ;
#16136 = ORIENTED_EDGE ( 'NONE', *, *, #22842, .F. ) ;
#16137 = CARTESIAN_POINT ( 'NONE',  ( 173.4291969867144587, 251.4074785162788714, 0.3572428630574652209 ) ) ;
#16138 = VERTEX_POINT ( 'NONE', #64721 ) ;
#16139 = CARTESIAN_POINT ( 'NONE',  ( 79.55352191442486287, 46.24377923495724474, -13.19933309463437432 ) ) ;
#16140 = CARTESIAN_POINT ( 'NONE',  ( 194.7576540903134799, 293.3168432830895540, -14.62421624641040196 ) ) ;
#16141 = FACE_OUTER_BOUND ( 'NONE', #37914, .T. ) ;
#16142 = ORIENTED_EDGE ( 'NONE', *, *, #43882, .F. ) ;
#16143 = CARTESIAN_POINT ( 'NONE',  ( 33.16918417342686354, 21.01110640527294038, 2.839279412974134775 ) ) ;
#16144 = CARTESIAN_POINT ( 'NONE',  ( 79.74329520344379318, 44.92144841624061513, 11.49897470811640332 ) ) ;
#16145 = CARTESIAN_POINT ( 'NONE',  ( 100.8442274002074441, 217.4824982072973683, 3.021315404115420679E-15 ) ) ;
#16146 = CARTESIAN_POINT ( 'NONE',  ( 75.05448840609841454, 66.98218832618682939, -13.15900604923073658 ) ) ;
#16147 = ORIENTED_EDGE ( 'NONE', *, *, #31701, .F. ) ;
#16148 = CARTESIAN_POINT ( 'NONE',  ( 41.60633307851366425, 35.97253583063844928, -10.00000000000000533 ) ) ;
#16149 = B_SPLINE_CURVE_WITH_KNOTS ( 'NONE', 3,
 ( #20719, #45483, #44485, #76418 ),
 .UNSPECIFIED., .F., .F.,
 ( 4, 4 ),
 ( 0.01434568471657762107, 0.02303913993019953560 ),
 .UNSPECIFIED. ) ;
#16150 = CARTESIAN_POINT ( 'NONE',  ( -11.77978294824862893, 175.5530062829863311, 1.347971487989956912E-14 ) ) ;
#16151 = ORIENTED_EDGE ( 'NONE', *, *, #51623, .T. ) ;
#16152 = CARTESIAN_POINT ( 'NONE',  ( -86.81108781737714253, 0.000000000000000000, -9.212605237762131694 ) ) ;
#16153 =( BOUNDED_CURVE ( )  B_SPLINE_CURVE ( 2, ( #62072, #94532, #55965, #16983, #53973, #55472, #86458, #47874, #1806 ),
 .UNSPECIFIED., .F., .T. ) 
 B_SPLINE_CURVE_WITH_KNOTS ( ( 3, 2, 2, 2, 3 ),
 ( 0.6169354838709677491, 0.6182795698924731242, 0.6209677419354838745, 0.6236559139784946248, 0.6250000000000000000 ),
 .UNSPECIFIED. ) 
 CURVE ( )  GEOMETRIC_REPRESENTATION_ITEM ( )  RATIONAL_B_SPLINE_CURVE ( ( 0.9330127018922194093, 0.9330127018922194093, 1.000000000000000000, 0.8660254037844387076, 1.000000000000000000, 0.8660254037844387076, 1.000000000000000000, 0.9330127018922194093, 0.9330127018922194093 ) ) 
 REPRESENTATION_ITEM ( '' )  );
#16155 = CARTESIAN_POINT ( 'NONE',  ( 68.10039974585599509, 65.18542567973285884, -10.72853162865224341 ) ) ;
#16154 = CARTESIAN_POINT ( 'NONE',  ( 67.77450396239858321, 65.65200295091629812, 10.05452136947112329 ) ) ;
#16156 = CARTESIAN_POINT ( 'NONE',  ( 81.42484531195619013, 55.17584661510441890, -15.93226465548353410 ) ) ;
#16157 = CARTESIAN_POINT ( 'NONE',  ( 164.3010377730689981, 246.0692501711882869, 7.247566249275159578 ) ) ;
#16158 = PLANE ( 'NONE',  #70696 ) ;
#16159 = CARTESIAN_POINT ( 'NONE',  ( 157.0887340267001946, 258.5613266995183039, -17.61824281915036394 ) ) ;
#16160 = CARTESIAN_POINT ( 'NONE',  ( 133.0017827873424494, 259.8464784336661637, 1.353441290958777525E-15 ) ) ;
#16161 = AXIS2_PLACEMENT_3D ( 'NONE', #55278, #78114, #76607 ) ;
#16162 = CARTESIAN_POINT ( 'NONE',  ( 206.4680688164142168, 270.6138877121450150, 2.724256221002448797 ) ) ;
#16163 = CARTESIAN_POINT ( 'NONE',  ( 182.0101398577191958, 260.3743076433015062, 9.429781970683626113 ) ) ;
#16164 = CARTESIAN_POINT ( 'NONE',  ( 87.45434598099585344, 230.4869531367911293, 4.594050593750046652 ) ) ;
#16165 = EDGE_LOOP ( 'NONE', ( #5958, #28491, #54778, #100295 ) ) ;
#16166 = CARTESIAN_POINT ( 'NONE',  ( 190.9501423151522772, 299.9116471280854626, 8.746938802470586083 ) ) ;
#16167 = CARTESIAN_POINT ( 'NONE',  ( 78.18465668123985779, 61.71620641638569538, -16.11691968629958183 ) ) ;
#16168 = EDGE_CURVE ( 'NONE', #94179, #89471, #94345, .T. ) ;
#16169 = ORIENTED_EDGE ( 'NONE', *, *, #50258, .F. ) ;
#16170 = CARTESIAN_POINT ( 'NONE',  ( 195.8309633264585727, 291.4578171538532274, -15.70624013417040743 ) ) ;
#16171 = ORIENTED_EDGE ( 'NONE', *, *, #37885, .F. ) ;
#16172 = ORIENTED_EDGE ( 'NONE', *, *, #9759, .T. ) ;
#16173 = CARTESIAN_POINT ( 'NONE',  ( 80.09120749856195687, 44.41673742825525295, -10.86461196121643979 ) ) ;
#16174 = CARTESIAN_POINT ( 'NONE',  ( 193.2980202556421432, 268.5488920227266476, -13.18347973120535599 ) ) ;
#16175 = CARTESIAN_POINT ( 'NONE',  ( 146.9235493515124062, 276.1679430252639804, 0.7994986043261682607 ) ) ;
#16176 = CARTESIAN_POINT ( 'NONE',  ( 81.04919588797569929, 56.11257561189316334, 16.10755627670017276 ) ) ;
#16177 = CARTESIAN_POINT ( 'NONE',  ( 52.32645086003936541, 201.0177522451418497, -10.00000000000009592 ) ) ;
#16178 = CARTESIAN_POINT ( 'NONE',  ( -22.42236680055709641, 157.8615022471902591, 0.000000000000000000 ) ) ;
#16179 = CARTESIAN_POINT ( 'NONE',  ( 80.33713356334875755, 211.0643266524159856, -9.188101187500093303 ) ) ;
#16180 = ORIENTED_EDGE ( 'NONE', *, *, #41613, .F. ) ;
#16181 = ADVANCED_FACE ( 'NONE', ( #95670 ), #64209, .F. ) ;
#16182 = VECTOR ( 'NONE', #99200, 1000.000000000000114 ) ;
#16183 = ORIENTED_EDGE ( 'NONE', *, *, #64204, .T. ) ;
#16184 = B_SPLINE_SURFACE_WITH_KNOTS ( 'NONE', 3, 1, ( 
 ( #17666, #87637 ),
 ( #17151, #47055 ),
 ( #71376, #86123 ),
 ( #57141, #88122 ),
 ( #48564, #24751 ),
 ( #40441, #95208 ),
 ( #56652, #25253 ),
 ( #55632, #32850 ),
 ( #70350, #31838 ),
 ( #55138, #1965 ),
 ( #64768, #77969 ),
 ( #62741, #40931 ),
 ( #9577, #79505 ),
 ( #18165, #86617 ),
 ( #962, #63759 ),
 ( #25777, #94692 ),
 ( #56136, #1474 ),
 ( #26265, #49065 ),
 ( #79999, #10568 ),
 ( #10066, #48049 ),
 ( #2476, #41443 ),
 ( #24260, #72383 ),
 ( #8564, #47548 ),
 ( #33357, #64257 ),
 ( #2993, #33883 ),
 ( #78475, #95717 ),
 ( #9062, #39929 ),
 ( #70866, #32355 ),
 ( #63256, #4449 ),
 ( #42922, #19679 ),
 ( #67242, #36340 ),
 ( #42434, #80504 ),
 ( #43442, #27264 ),
 ( #35349, #50540 ) ),
 .UNSPECIFIED., .T., .F., .F.,
 ( 4, 2, 2, 2, 2, 2, 2, 2, 2, 2, 2, 2, 2, 2, 2, 2, 4 ),
 ( 2, 2 ),
 ( 0.000000000000000000, 0.06250000000000000000, 0.1250000000000000000, 0.1875000000000000000, 0.2500000000000000000, 0.3125000000000000000, 0.3750000000000000000, 0.4375000000000000000, 0.5000000000000000000, 0.5625000000000000000, 0.6250000000000000000, 0.6875000000000000000, 0.7500000000000000000, 0.8125000000000000000, 0.8750000000000000000, 0.9375000000000000000, 1.000000000000000000 ),
 ( 0.000000000000000000, 1.000000000000000000 ),
 .UNSPECIFIED. ) ;
#16185 = CARTESIAN_POINT ( 'NONE',  ( 200.9211856235105529, 282.6412935135391535, -18.21488537951028519 ) ) ;
#16186 = VERTEX_POINT ( 'NONE', #26218 ) ;
#16187 = EDGE_CURVE ( 'NONE', #8050, #58060, #56088, .T. ) ;
#16188 = CARTESIAN_POINT ( 'NONE',  ( 76.45843591644145931, 51.61599511231165138, -15.65747087338039556 ) ) ;
#16189 = CARTESIAN_POINT ( 'NONE',  ( 76.24945506196253575, 64.85903190964545217, -14.33188622986231842 ) ) ;
#16190 = CARTESIAN_POINT ( 'NONE',  ( 206.9678007395010013, 269.7219839212710326, -0.02000383387707006105 ) ) ;
#16191 = CYLINDRICAL_SURFACE ( 'NONE', #4061, 70.00000000000002842 ) ;
#16192 = CARTESIAN_POINT ( 'NONE',  ( 160.9324095734352511, 260.4995019621508163, 16.69280320549395924 ) ) ;
#16193 = ORIENTED_EDGE ( 'NONE', *, *, #67692, .T. ) ;
#16194 = CARTESIAN_POINT ( 'NONE',  ( 192.5672132233574700, 296.7161803602032819, 11.26440590052197521 ) ) ;
#16195 = DIRECTION ( 'NONE',  ( -0.000000000000000000, 0.000000000000000000, 1.000000000000000000 ) ) ;
#16196 = CARTESIAN_POINT ( 'NONE',  ( 47.05668214639808866, 76.45164061169337799, -10.00000000000000000 ) ) ;
#16197 = CARTESIAN_POINT ( 'NONE',  ( 152.8651171364917900, 265.8768457450651113, -16.25664868183201861 ) ) ;
#16198 = FACE_OUTER_BOUND ( 'NONE', #37089, .T. ) ;
#16199 = CARTESIAN_POINT ( 'NONE',  ( 138.9086373102437051, 262.5530062829863027, -4.648177544792955347E-16 ) ) ;
#16200 = ORIENTED_EDGE ( 'NONE', *, *, #98920, .T. ) ;
#16201 = CARTESIAN_POINT ( 'NONE',  ( 195.8856561536922811, 265.4848694841979864, 4.430043780811904419 ) ) ;
#16202 = CARTESIAN_POINT ( 'NONE',  ( 85.30758498749676733, 213.3927522451418213, 10.00000000000009948 ) ) ;
#16203 = CARTESIAN_POINT ( 'NONE',  ( 15.54467260552930341, 34.00295985972733348, -10.00000000000000000 ) ) ;
#16204 = CARTESIAN_POINT ( 'NONE',  ( 187.8780304577002198, 266.2815348468194543, -12.02982252659589868 ) ) ;
#16205 = CARTESIAN_POINT ( 'NONE',  ( 198.5685943996323886, 266.1185824620975495, 1.314686358112626685 ) ) ;
#16206 = CARTESIAN_POINT ( 'NONE',  ( 156.8545567402366316, 272.5222548076167755, 14.36144970815616695 ) ) ;
#16207 = EDGE_LOOP ( 'NONE', ( #18482, #15048, #95457, #65736 ) ) ;
#16208 = PLANE ( 'NONE',  #74040 ) ;
#16209 = CARTESIAN_POINT ( 'NONE',  ( 202.4017613376760494, 280.0768611521521620, 15.73960524502980540 ) ) ;
#16210 = CARTESIAN_POINT ( 'NONE',  ( 198.2505066714982149, 285.2670451491296149, 0.000000000000000000 ) ) ;
#16212 = FACE_BOUND ( 'NONE', #64423, .T. ) ;
#16211 = CARTESIAN_POINT ( 'NONE',  ( 177.6568436143930967, 264.5527407949075496, -15.77239500404458283 ) ) ;
#16213 = CARTESIAN_POINT ( 'NONE',  ( 199.2490371652133945, 281.9579806773367068, -16.60615833393185525 ) ) ;
#16214 = EDGE_CURVE ( 'NONE', #57637, #89739, #3434, .T. ) ;
#16215 = CARTESIAN_POINT ( 'NONE',  ( 32.56068451518306262, 20.92755873383627829, 6.180339887498953466 ) ) ;
#16216 = CARTESIAN_POINT ( 'NONE',  ( 172.3003440879262484, 275.1291536054555422, 16.73320108566939268 ) ) ;
#16217 = CARTESIAN_POINT ( 'NONE',  ( 166.0707157462996406, 285.6421157637285546, -3.164261021881538571 ) ) ;
#16218 = CARTESIAN_POINT ( 'NONE',  ( 126.4618338667176403, 250.4865022471902876, -10.00000000000009592 ) ) ;
#16219 = CARTESIAN_POINT ( 'NONE',  ( 191.8419389717784327, 261.4849666034271536, 3.078932809042389529 ) ) ;
#16220 = LINE ( 'NONE', #86183, #7626 ) ;
#16221 = CARTESIAN_POINT ( 'NONE',  ( -4.696256414383327638, 180.3464784336661637, 1.353441290958777327E-15 ) ) ;
#16222 = CARTESIAN_POINT ( 'NONE',  ( 73.84070662262635665, 224.9860189848785126, -2.679491924311252493 ) ) ;
#16223 = ORIENTED_EDGE ( 'NONE', *, *, #21918, .T. ) ;
#16224 = ADVANCED_FACE ( 'NONE', ( #18627 ), #71231, .F. ) ;
#16225 = AXIS2_PLACEMENT_3D ( 'NONE', #88089, #71847, #95174 ) ;
#16226 = EDGE_CURVE ( 'NONE', #63171, #81636, #23739, .T. ) ;
#16227 = DIRECTION ( 'NONE',  ( 0.4999999999999998890, -0.8660254037844385966, 0.000000000000000000 ) ) ;
#16228 = CARTESIAN_POINT ( 'NONE',  ( -19.65312891409030271, 93.06504152958497400, -10.00000000000000888 ) ) ;
#16229 = CYLINDRICAL_SURFACE ( 'NONE', #89078, 17.82106496071139645 ) ;
#16230 = CARTESIAN_POINT ( 'NONE',  ( 12.11013585174968554, 186.9869531367911293, 4.594050593750046652 ) ) ;
#16231 = CARTESIAN_POINT ( 'NONE',  ( 24.34009904141853653, 32.79103043416549923, 8.090169943749478065 ) ) ;
#16232 = CARTESIAN_POINT ( 'NONE',  ( 34.35958382788741261, 28.03677371833804699, 10.00000000000000533 ) ) ;
#16233 = CARTESIAN_POINT ( 'NONE',  ( 85.71989473008328275, 42.74111325103400105, -0.5968306828680215448 ) ) ;
#16234 = CARTESIAN_POINT ( 'NONE',  ( 147.2937583206075942, 275.5267222813735088, 0.1877253132609109920 ) ) ;
#16235 = CARTESIAN_POINT ( 'NONE',  ( 84.48912213214688904, 47.60039072597393073, 12.10431667099950559 ) ) ;
#16236 = CARTESIAN_POINT ( 'NONE',  ( 190.2350275263131607, 261.6741793222014962, -0.7552779011735962778 ) ) ;
#16237 = VECTOR ( 'NONE', #47103, 1000.000000000000114 ) ;
#16238 = CARTESIAN_POINT ( 'NONE',  ( 69.44849478424205813, 224.2365022471903160, 2.944929066748280225E-16 ) ) ;
#16239 = CARTESIAN_POINT ( 'NONE',  ( 72.88390603025270309, 66.33307502503427600, -12.19624667911425853 ) ) ;
#16240 = CARTESIAN_POINT ( 'NONE',  ( 203.3784415195017061, 270.0710565943527399, 6.595345848229188235 ) ) ;
#16241 = CARTESIAN_POINT ( 'NONE',  ( 20.95974617273066443, 195.1589784336661637, -6.496448406907675876E-16 ) ) ;
#16242 = CARTESIAN_POINT ( 'NONE',  ( 72.81630190666361102, 70.85884106002269789, -7.900673142507896429 ) ) ;
#16243 = CARTESIAN_POINT ( 'NONE',  ( 127.3278592705020742, 250.9865022471903160, 10.00000000000009415 ) ) ;
#16244 = CARTESIAN_POINT ( 'NONE',  ( 164.5139018292655919, 259.6662038739244736, -17.01387605652571366 ) ) ;
#16245 = CARTESIAN_POINT ( 'NONE',  ( 150.9003228897357189, 269.2799692068659283, -14.30003212299500781 ) ) ;
#16246 = CARTESIAN_POINT ( 'NONE',  ( 67.27399870575082730, 66.42956969496371755, -8.768125640873389415 ) ) ;
#16247 = CARTESIAN_POINT ( 'NONE',  ( 155.3738696901333469, 261.5315588585399951, 17.02116401938635804 ) ) ;
#16248 = DIRECTION ( 'NONE',  ( -0.2359789242578323731, -0.9717581732643756354, 0.000000000000000000 ) ) ;
#16249 = CARTESIAN_POINT ( 'NONE',  ( 163.1096457525017627, 281.1598135738970541, -10.26398345759424657 ) ) ;
#16250 = DIRECTION ( 'NONE',  ( 0.000000000000000000, 1.000000000000000000, 0.000000000000000000 ) ) ;
#16251 = CARTESIAN_POINT ( 'NONE',  ( 20.33338779993010803, 20.24335787977762990, -9.188101187500008038 ) ) ;
#16252 = CARTESIAN_POINT ( 'NONE',  ( 162.8037981520209314, 248.6625452659484381, 9.809699077002424161 ) ) ;
#16253 = CARTESIAN_POINT ( 'NONE',  ( 185.9817139542059579, 267.6581844819601770, -14.98798611928668301 ) ) ;
#16254 = ORIENTED_EDGE ( 'NONE', *, *, #84044, .T. ) ;
#16255 = CARTESIAN_POINT ( 'NONE',  ( 185.3296124515819372, 291.1871008657900006, 13.45743802455416827 ) ) ;
#16256 = CARTESIAN_POINT ( 'NONE',  ( 11.67313376208572961, 15.24335787977761569, -9.188101187500008038 ) ) ;
#16257 = CARTESIAN_POINT ( 'NONE',  ( 76.98116725474599775, 58.55206284898313385, -16.09923721801287755 ) ) ;
#16258 = CARTESIAN_POINT ( 'NONE',  ( 71.95319803722021845, 72.64445964553972601, -0.8526933041427806614 ) ) ;
#16259 = EDGE_LOOP ( 'NONE', ( #63860, #39585, #4981, #58759 ) ) ;
#16260 = CARTESIAN_POINT ( 'NONE',  ( 82.81737761406506593, 40.62361263874299055, 0.9906565629087065172 ) ) ;
#16261 = CARTESIAN_POINT ( 'NONE',  ( 72.48661302258760486, 71.52526770760660213, -5.337229783571237007 ) ) ;
#16262 = CARTESIAN_POINT ( 'NONE',  ( 85.41264917886874741, 49.08844855121448347, 12.38516025679438748 ) ) ;
#16263 = CARTESIAN_POINT ( 'NONE',  ( 85.68486538673562336, 43.15900242217779237, 5.076191362464745893 ) ) ;
#16264 = ORIENTED_EDGE ( 'NONE', *, *, #35895, .T. ) ;
#16265 = VERTEX_POINT ( 'NONE', #78807 ) ;
#16267 = CARTESIAN_POINT ( 'NONE',  ( 84.22353192663439359, 42.61057292944220620, -4.410993892459540433 ) ) ;
#16266 = CARTESIAN_POINT ( 'NONE',  ( 189.5147274052520174, 274.6873094654737315, -16.11146568285224134 ) ) ;
#16268 = ORIENTED_EDGE ( 'NONE', *, *, #23012, .F. ) ;
#16269 = CARTESIAN_POINT ( 'NONE',  ( 151.4281781455628675, 268.3656970847310390, 15.24742929158552585 ) ) ;
#16270 = CARTESIAN_POINT ( 'NONE',  ( 71.85441816053061359, 72.14404838950795806, -3.648524940272755757 ) ) ;
#16271 = CARTESIAN_POINT ( 'NONE',  ( 80.12977496600375105, 58.13812068622525686, 16.26683105399684237 ) ) ;
#16272 = DIRECTION ( 'NONE',  ( 1.804112415015878984E-15, -1.000000000000000000, 0.000000000000000000 ) ) ;
#16273 = CARTESIAN_POINT ( 'NONE',  ( 190.4281805785508084, 300.8157113754859893, -1.233909217199055774 ) ) ;
#16274 = CARTESIAN_POINT ( 'NONE',  ( 149.2593905435863348, 272.1221474021800759, -12.98626158366800176 ) ) ;
#16275 = CARTESIAN_POINT ( 'NONE',  ( 180.4421801628115816, 287.0161100701561736, -13.61753346319509639 ) ) ;
#16276 = EDGE_CURVE ( 'NONE', #47888, #17056, #83011, .T. ) ;
#16277 = EDGE_LOOP ( 'NONE', ( #83135, #13444, #82374, #93054, #60738, #76939, #68674, #10080, #79877, #64648, #24374, #52130, #10825, #93028, #37621, #78797, #58298, #31817, #52377, #80992, #88709, #42275, #16409, #85900, #1738, #70330, #85131, #60510, #99747, #66854, #66621, #74758, #30408, #86994, #51289, #23484, #42067, #74603, #51418, #81899, #69105, #25516, #70136, #63413, #93769, #90995, #94210, #15508, #23396, #16921, #74011, #60497, #16033 ) ) ;
#16278 = CARTESIAN_POINT ( 'NONE',  ( -19.65312891409030271, 93.06504152958497400, -10.00000000000000888 ) ) ;
#16279 = CARTESIAN_POINT ( 'NONE',  ( 82.81737761406506593, 40.62361263874299055, 0.9906565629087087377 ) ) ;
#16280 = EDGE_LOOP ( 'NONE', ( #29778, #11803, #8452, #10733 ) ) ;
#16281 = CARTESIAN_POINT ( 'NONE',  ( 22.20737081713591010, 33.79752408145593279, -5.678558825948271327 ) ) ;
#16282 = CARTESIAN_POINT ( 'NONE',  ( 159.4285914931787431, 254.5085746851079023, 15.41072477910873673 ) ) ;
#16283 = DIRECTION ( 'NONE',  ( -0.8615733660689046669, -0.5076330711061851630, 0.000000000000000000 ) ) ;
#16284 = EDGE_CURVE ( 'NONE', #78948, #41197, #46889, .T. ) ;
#16285 = CARTESIAN_POINT ( 'NONE',  ( 66.20992061623260838, 209.0333772461660544, 9.188101187500095079 ) ) ;
#16286 = EDGE_LOOP ( 'NONE', ( #21432, #74517, #22618, #14675 ) ) ;
#16287 = DIRECTION ( 'NONE',  ( -1.000000000000000000, 0.000000000000000000, 0.000000000000000000 ) ) ;
#16288 = CARTESIAN_POINT ( 'NONE',  ( 159.6684720758726144, 254.4985299059416377, 15.35327236017407948 ) ) ;
#16289 = CARTESIAN_POINT ( 'NONE',  ( 98.13012578506970840, 215.9155109091896065, 2.679491924311254714 ) ) ;
#16290 = CARTESIAN_POINT ( 'NONE',  ( 173.0447734647070206, 271.2248508029067011, 16.42412328953864886 ) ) ;
#16291 = VERTEX_POINT ( 'NONE', #63086 ) ;
#16292 = ORIENTED_EDGE ( 'NONE', *, *, #58622, .T. ) ;
#16293 = CYLINDRICAL_SURFACE ( 'NONE', #10869, 17.82106496071139645 ) ;
#16294 = CARTESIAN_POINT ( 'NONE',  ( 190.4240181651484818, 300.8229208869809668, -4.214281362166949485 ) ) ;
#16295 = CARTESIAN_POINT ( 'NONE',  ( 148.0389988358468827, 274.2359278451201590, 7.783622668412842671 ) ) ;
#16296 = ORIENTED_EDGE ( 'NONE', *, *, #94321, .T. ) ;
#16297 = CARTESIAN_POINT ( 'NONE',  ( 148.9232972370683399, 272.7042780851529642, 12.27045554427055940 ) ) ;
#16298 = LINE ( 'NONE', #62379, #76058 ) ;
#16299 = EDGE_CURVE ( 'NONE', #39606, #43165, #99014, .T. ) ;
#16300 = CARTESIAN_POINT ( 'NONE',  ( 49.07456115661582174, 91.13648234292965356, -10.00000000000000000 ) ) ;
#16301 = CARTESIAN_POINT ( 'NONE',  ( 147.5381343315788172, 275.1034506142203782, -4.056595942992749393 ) ) ;
#16302 = B_SPLINE_CURVE_WITH_KNOTS ( 'NONE', 3,
 ( #63512, #15905, #31099, #70098, #93955, #9317, #46286, #84851, #86878, #40191, #71639, #39183, #2233, #61505, #92454, #53892, #16408, #8810, #71132, #55882, #55388, #78728, #39678, #94450, #32098, #70606, #7818, #708, #77215, #1735, #85356, #1219, #63010, #23492, #32615, #86375, #16904, #25005, #77733, #47303, #8319, #31592, #15391, #17410, #48320, #62486 ),
 .UNSPECIFIED., .F., .F.,
 ( 4, 1, 2, 2, 1, 2, 2, 1, 1, 2, 2, 1, 1, 2, 2, 1, 1, 2, 2, 1, 1, 1, 2, 2, 1, 1, 1, 2, 2, 4 ),
 ( 0.000000000000000000, 0.06250000000001654232, 0.09375000000002257916, 0.1250000000000286160, 0.1875000000000436595, 0.2187500000000511813, 0.2500000000000586753, 0.3125000000000699441, 0.3437500000000737188, 0.3593750000000733302, 0.3750000000000729972, 0.4375000000000655032, 0.4687500000000641154, 0.4843750000000648370, 0.5000000000000656142, 0.5625000000000563993, 0.5937500000000521805, 0.6093750000000500711, 0.6250000000000478506, 0.6875000000000371925, 0.7187500000000308642, 0.7343750000000281997, 0.7421875000000267564, 0.7500000000000254241, 0.8125000000000149880, 0.8437500000000102141, 0.8593750000000084377, 0.8671875000000078826, 0.8750000000000074385, 1.000000000000000000 ),
 .UNSPECIFIED. ) ;
#16303 = CARTESIAN_POINT ( 'NONE',  ( 160.2788325581946083, 255.7866659750827694, 16.08102370418938065 ) ) ;
#16304 = CARTESIAN_POINT ( 'NONE',  ( 70.14042535710315462, 67.96861681286139856, 9.010985477280877731 ) ) ;
#16305 = CARTESIAN_POINT ( 'NONE',  ( 82.15890019083936124, 42.36938956976207749, -7.663980805570597354 ) ) ;
#16306 = CARTESIAN_POINT ( 'NONE',  ( 164.2897805489690768, 249.8104079013010335, 11.36607573508163505 ) ) ;
#16307 = CARTESIAN_POINT ( 'NONE',  ( 198.2505066714982149, 285.2670451491296149, 0.000000000000000000 ) ) ;
#16308 = CARTESIAN_POINT ( 'NONE',  ( 78.56257306381201033, 47.97152266697279543, 13.95721769279705171 ) ) ;
#16309 = CARTESIAN_POINT ( 'NONE',  ( 112.1907172202364080, 226.3923013555410080, 4.594050593750050204 ) ) ;
#16310 = EDGE_LOOP ( 'NONE', ( #56375, #26252, #12815, #94819 ) ) ;
#16311 = CARTESIAN_POINT ( 'NONE',  ( 191.8000917695741805, 298.4394914891611847, -9.452573400474340914 ) ) ;
#16312 = CARTESIAN_POINT ( 'NONE',  ( -1.662747857324051282, 91.90478749174060624, 1.836970198720990540E-15 ) ) ;
#16313 = CARTESIAN_POINT ( 'NONE',  ( 191.2002274372966610, 261.5526795057712661, 5.342804824337664016 ) ) ;
#16314 = ADVANCED_FACE ( 'NONE', ( #42273 ), #11421, .T. ) ;
#16315 = CARTESIAN_POINT ( 'NONE',  ( 203.5477091018662748, 278.0920214017542662, -16.09930363698006062 ) ) ;
#16316 = EDGE_CURVE ( 'NONE', #67853, #25891, #11754, .T. ) ;
#16317 = CARTESIAN_POINT ( 'NONE',  ( 204.5133713884061706, 276.4194452585140311, 14.87364779308245843 ) ) ;
#16318 = FACE_OUTER_BOUND ( 'NONE', #43917, .T. ) ;
#16319 = CIRCLE ( 'NONE', #35703, 70.00000000000001421 ) ;
#16320 = CARTESIAN_POINT ( 'NONE',  ( 168.9493557510702146, 284.9254214029872401, -7.956471245316214969 ) ) ;
#16321 = ORIENTED_EDGE ( 'NONE', *, *, #96781, .T. ) ;
#16322 = CARTESIAN_POINT ( 'NONE',  ( 207.7837159184916231, 270.7550423741513441, -2.369602332675663448 ) ) ;
#16323 = CARTESIAN_POINT ( 'NONE',  ( 72.31970296779593355, 71.55818645699302749, 5.058004163053099411 ) ) ;
#16324 = CARTESIAN_POINT ( 'NONE',  ( 165.0831640657340529, 244.7145676943567878, -1.661138566959525775 ) ) ;
#16325 = CARTESIAN_POINT ( 'NONE',  ( 125.6409139509397050, 243.3458772461660544, 9.188101187500095079 ) ) ;
#16326 = DIRECTION ( 'NONE',  ( 0.8660254037844395958, 0.4999999999999985567, 0.000000000000000000 ) ) ;
#16327 = CARTESIAN_POINT ( 'NONE',  ( 88.05624235485146301, 44.55787864911079765, -5.145732200269208079 ) ) ;
#16328 = CARTESIAN_POINT ( 'NONE',  ( 188.0361769804965206, 281.7550819701144746, -17.70093714309158983 ) ) ;
#16329 = LINE ( 'NONE', #78145, #88768 ) ;
#16330 = CARTESIAN_POINT ( 'NONE',  ( 50.64826632015721231, 209.2369531367911293, -4.594050593750048428 ) ) ;
#16331 = FACE_OUTER_BOUND ( 'NONE', #13177, .T. ) ;
#16332 = VERTEX_POINT ( 'NONE', #17490 ) ;
#16333 = CARTESIAN_POINT ( 'NONE',  ( 70.50184245679560036, 61.65203380429616686, 14.13751713409887323 ) ) ;
#16334 = CARTESIAN_POINT ( 'NONE',  ( 196.3249884498792994, 275.2518087180711177, 16.06659936265807431 ) ) ;
#16335 = EDGE_CURVE ( 'NONE', #86137, #6903, #20609, .T. ) ;
#16336 = DIRECTION ( 'NONE',  ( -0.2502735827033041316, -0.9681751565707789053, 0.000000000000000000 ) ) ;
#16337 = DIRECTION ( 'NONE',  ( -1.000000000000000000, 0.000000000000000000, 0.000000000000000000 ) ) ;
#16338 = DIRECTION ( 'NONE',  ( -0.9377374661009826307, -0.3473448497826164827, 0.000000000000000000 ) ) ;
#16339 = B_SPLINE_CURVE_WITH_KNOTS ( 'NONE', 3,
 ( #1110, #92835, #31988, #23386, #93849, #15790, #24403, #78619, #40079, #14799, #38078, #22893, #71024, #32510, #91842, #85245, #22403, #15282, #68991, #92344, #46177, #7699, #77097, #69497, #110, #30995, #61880, #54276, #94836, #88263, #64405, #4094, #56287, #87285, #10214, #18315, #10712, #17816, #25399, #2114, #34496, #33509, #95854, #48717, #32996, #72016, #26411, #11226, #3617, #72530 ),
 .UNSPECIFIED., .F., .F.,
 ( 4, 2, 2, 2, 2, 2, 2, 2, 2, 2, 2, 2, 2, 2, 2, 2, 2, 2, 2, 2, 2, 2, 2, 2, 4 ),
 ( 0.0001408704111295071184, 0.001152638629686134064, 0.001658522738964416082, 0.001784993766284012282, 0.001911464793603608048, 0.002037935820923203814, 0.002164406848242800014, 0.002417348902882022772, 0.002670290957521245529, 0.003176175066799552700, 0.004187943285356238166, 0.005199711503912924498, 0.005705595613191308431, 0.005958537667830458330, 0.006211479722469609964, 0.006274715236129331519, 0.006337950749789053075, 0.006401186263448773762, 0.006464421777108495318, 0.006717363831747565420, 0.007223247941025566846, 0.007476189995664625672, 0.007729132050303684498, 0.007982074104942744192, 0.008235016159581802150 ),
 .UNSPECIFIED. ) ;
#16340 = CARTESIAN_POINT ( 'NONE',  ( 154.8579861482817535, 262.4250953638155011, -17.69813260923097786 ) ) ;
#16341 = CARTESIAN_POINT ( 'NONE',  ( 155.7075129258784614, 270.0159152318828433, -14.86779825989652259 ) ) ;
#16342 = ADVANCED_FACE ( 'NONE', ( #96532 ), #18008, .F. ) ;
#16343 = CARTESIAN_POINT ( 'NONE',  ( 115.9793180381955580, 247.7677522451419065, -5.000000000000047962 ) ) ;
#16344 = CARTESIAN_POINT ( 'NONE',  ( 194.6516423578734702, 293.0856640331928702, -14.71461979434458200 ) ) ;
#16345 = ORIENTED_EDGE ( 'NONE', *, *, #7583, .F. ) ;
#16346 = EDGE_CURVE ( 'NONE', #58893, #32206, #10905, .T. ) ;
#16347 = CARTESIAN_POINT ( 'NONE',  ( 162.6626107288841467, 248.9070890562113902, 10.12509462564867313 ) ) ;
#16348 = CARTESIAN_POINT ( 'NONE',  ( 88.05313862314940820, 44.74715133896623342, 4.488002289119355837 ) ) ;
#16349 = CARTESIAN_POINT ( 'NONE',  ( 16.08835327644320401, 192.3464784336661637, 1.353441290958777327E-15 ) ) ;
#16350 = CARTESIAN_POINT ( 'NONE',  ( 9.964077338596862177, 24.49103043416547365, -8.090169943749479842 ) ) ;
#16351 = CARTESIAN_POINT ( 'NONE',  ( -17.42236680055705023, 149.2012482093457777, 0.000000000000000000 ) ) ;
#16352 = CARTESIAN_POINT ( 'NONE',  ( -70.89022602266993545, 47.22876919346843749, -10.00000000000000000 ) ) ;
#16353 = CARTESIAN_POINT ( 'NONE',  ( 72.25139993921258963, 72.08772000594029805, 3.145145327714725880 ) ) ;
#16354 = EDGE_CURVE ( 'NONE', #86855, #23257, #9058, .T. ) ;
#16356 = CARTESIAN_POINT ( 'NONE',  ( 60.25564886944957976, 217.8464784336661637, 1.353441290958777327E-15 ) ) ;
#16355 = DIRECTION ( 'NONE',  ( 0.000000000000000000, 0.000000000000000000, 1.000000000000000000 ) ) ;
#16357 = CARTESIAN_POINT ( 'NONE',  ( 174.1648641962809450, 288.5940705739083683, 7.621244220064776087 ) ) ;
#16358 = CARTESIAN_POINT ( 'NONE',  ( 184.7539679289934611, 257.4663050619941487, 1.389359455806087995 ) ) ;
#16359 = FACE_OUTER_BOUND ( 'NONE', #94069, .T. ) ;
#16360 = CARTESIAN_POINT ( 'NONE',  ( 161.6505112061591376, 251.4379174015757883, -12.98887274494184041 ) ) ;
#16361 = ORIENTED_EDGE ( 'NONE', *, *, #70034, .F. ) ;
#16362 = B_SPLINE_CURVE_WITH_KNOTS ( 'NONE', 3,
 ( #13850, #28544, #38998, #23803, #46599, #5259, #5747, #35656, #36141, #59426, #20472, #43239, #90903, #20980, #90404, #44727, #51862, #97484, #29550, #98967, #82801, #67543, #44235, #75661, #75173, #68045, #6245, #37143, #98474, #21453, #91381, #23301, #54190, #85155, #77532, #74182, #69904, #517, #31405, #54692, #12374, #28049, #89895, #86671, #71428, #24318, #25307, #25833, #39988, #55684, #85676, #55193 ),
 .UNSPECIFIED., .F., .F.,
 ( 4, 2, 2, 2, 2, 2, 2, 2, 2, 2, 2, 2, 2, 2, 2, 2, 2, 2, 2, 2, 2, 2, 2, 2, 2, 4 ),
 ( 0.0001758988993951120044, 0.0006622138821329520090, 0.001148528864870791959, 0.001391686356239734161, 0.001513265101924233125, 0.001634843847608731873, 0.001756422593293230621, 0.001878001338977729586, 0.002121158830346824876, 0.002607473813085065331, 0.003093788795823305786, 0.004066418761299786695, 0.005039048726776266737, 0.005525363709514587857, 0.005768521200883747549, 0.005890099946568327395, 0.006011678692252908109, 0.006072468065095169842, 0.006133257437937432444, 0.006254836183622050454, 0.006497993674991226626, 0.006741151166360403665, 0.006984308657729579838, 0.007227466149098756877, 0.007470623640467933917, 0.007956938623206325292 ),
 .UNSPECIFIED. ) ;
#16363 = CARTESIAN_POINT ( 'NONE',  ( 162.6576765882541054, 267.6039545257508507, 16.48102639217245624 ) ) ;
#16364 = CARTESIAN_POINT ( 'NONE',  ( 18.20865839366279459, 187.9865022471902876, 10.00000000000009237 ) ) ;
#16365 = CARTESIAN_POINT ( 'NONE',  ( 146.4255236417662616, 255.3458772461660260, 9.188101187500095079 ) ) ;
#16366 = CARTESIAN_POINT ( 'NONE',  ( 202.8499463704053198, 279.3005819042728604, 17.04674939340617001 ) ) ;
#16367 = CARTESIAN_POINT ( 'NONE',  ( -14.92600794870451253, 168.3149278399160664, 9.188101187500093303 ) ) ;
#16368 = CARTESIAN_POINT ( 'NONE',  ( 29.97031301328857467, 32.70171378149920827, -9.188101187500004485 ) ) ;
#16369 = DIRECTION ( 'NONE',  ( 0.000000000000000000, 0.000000000000000000, 1.000000000000000000 ) ) ;
#16370 = CARTESIAN_POINT ( 'NONE',  ( 188.7194914702840549, 261.8282078956012242, 6.495625297079970828 ) ) ;
#16371 = CARTESIAN_POINT ( 'NONE',  ( 74.74743988288986429, 202.4155109091896065, 2.679491924311254714 ) ) ;
#16372 = CARTESIAN_POINT ( 'NONE',  ( 185.9427433571077586, 257.7868782628476083, -2.501399907045548598 ) ) ;
#16373 = CARTESIAN_POINT ( 'NONE',  ( 65.98930969947784320, 69.00056210431527859, 2.540950622023999461 ) ) ;
#16374 = ORIENTED_EDGE ( 'NONE', *, *, #55451, .T. ) ;
#16375 = LINE ( 'NONE', #25475, #64927 ) ;
#16376 = CARTESIAN_POINT ( 'NONE',  ( 184.5944248404513246, 287.4419850773005010, 15.55097255147333435 ) ) ;
#16377 = CARTESIAN_POINT ( 'NONE',  ( 181.3234608124392366, 287.3713783320475841, 13.33777075617584984 ) ) ;
#16378 = CARTESIAN_POINT ( 'NONE',  ( 196.6472778906841086, 289.6559313043970860, 16.38098019016104345 ) ) ;
#16379 = CARTESIAN_POINT ( 'NONE',  ( 10.59179830548347745, 18.06628583063839599, -9.188101187500006262 ) ) ;
#16380 = CARTESIAN_POINT ( 'NONE',  ( 160.4502686134403007, 252.7389780038842844, 16.14074205763531111 ) ) ;
#16381 = CARTESIAN_POINT ( 'NONE',  ( 88.28100378030374884, 44.27701181192854563, -1.950484388336117814 ) ) ;
#16382 = DIRECTION ( 'NONE',  ( 0.000000000000000000, -0.000000000000000000, 1.000000000000000000 ) ) ;
#16383 = CARTESIAN_POINT ( 'NONE',  ( -19.65312891409030271, 93.06504152958497400, -10.00000000000000888 ) ) ;
#16384 = CARTESIAN_POINT ( 'NONE',  ( 191.6256142097132908, 298.3549236037118817, 8.658380026548993413 ) ) ;
#16385 = CARTESIAN_POINT ( 'NONE',  ( 163.3020905273760093, 247.7994775548095845, -11.05431316445765155 ) ) ;
#16386 = CIRCLE ( 'NONE', #47186, 0.1418229129681557177 ) ;
#16387 = CARTESIAN_POINT ( 'NONE',  ( 162.7020145476934090, 284.0983276010327359, 6.051621772638641872 ) ) ;
#16388 = ORIENTED_EDGE ( 'NONE', *, *, #95050, .T. ) ;
#16389 = ORIENTED_EDGE ( 'NONE', *, *, #62910, .T. ) ;
#16390 = CARTESIAN_POINT ( 'NONE',  ( 155.8021524857682039, 277.1561808410325511, -10.39920598458100542 ) ) ;
#16391 = CARTESIAN_POINT ( 'NONE',  ( 73.02574606114626476, 70.77724550349999788, 7.489232062110982469 ) ) ;
#16392 = VERTEX_POINT ( 'NONE', #27102 ) ;
#16393 = CARTESIAN_POINT ( 'NONE',  ( 17.41845772768865075, 33.55466486950699334, -1.111400068045478839E-16 ) ) ;
#16394 = DIRECTION ( 'NONE',  ( -0.8660254037844378194, -0.5000000000000014433, -0.000000000000000000 ) ) ;
#16395 = ORIENTED_EDGE ( 'NONE', *, *, #62765, .F. ) ;
#16396 = CARTESIAN_POINT ( 'NONE',  ( 68.75007899452677407, 64.17077260193588018, -11.93723544003106696 ) ) ;
#16397 = LINE ( 'NONE', #55376, #41083 ) ;
#16398 = CARTESIAN_POINT ( 'NONE',  ( 188.3784916956350344, 286.3721210266486992, -16.81851773412965301 ) ) ;
#16399 = CARTESIAN_POINT ( 'NONE',  ( 84.89575725111018301, 47.24063678070221783, -11.59919686242552217 ) ) ;
#16400 = CARTESIAN_POINT ( 'NONE',  ( 69.61300338435667356, 62.66305564137741868, 13.88455583225131917 ) ) ;
#16401 = EDGE_LOOP ( 'NONE', ( #16887, #11710, #47561, #60855 ) ) ;
#16402 = CARTESIAN_POINT ( 'NONE',  ( -38.61298035630893111, 26.97617139035147460, -10.00000000000000000 ) ) ;
#16403 = CARTESIAN_POINT ( 'NONE',  ( 190.7779368023172708, 300.2099158256590385, 8.142228434510803581 ) ) ;
#16404 = CARTESIAN_POINT ( 'NONE',  ( 31.86369474034375671, 37.13478043621390157, 8.090169943749478065 ) ) ;
#16405 = ORIENTED_EDGE ( 'NONE', *, *, #38607, .T. ) ;
#16406 = ORIENTED_EDGE ( 'NONE', *, *, #51647, .F. ) ;
#16407 = ORIENTED_EDGE ( 'NONE', *, *, #34981, .F. ) ;
#16408 = CARTESIAN_POINT ( 'NONE',  ( 73.92771649931930256, 63.77271023027558527, 14.14211124488107174 ) ) ;
#16409 = ORIENTED_EDGE ( 'NONE', *, *, #56772, .F. ) ;
#16410 = CARTESIAN_POINT ( 'NONE',  ( 183.2186634280558053, 270.7509055985178179, 17.09995095404208953 ) ) ;
#16411 = VERTEX_POINT ( 'NONE', #40270 ) ;
#16412 = CARTESIAN_POINT ( 'NONE',  ( 164.4963285489318991, 245.7309966251440301, -6.672251175510283794 ) ) ;
#16413 = CARTESIAN_POINT ( 'NONE',  ( 49.66226845319755512, 83.29899382260626339, -10.00000000000000000 ) ) ;
#16414 = CARTESIAN_POINT ( 'NONE',  ( 169.9746517273565871, 283.3628436921554226, 12.55872587313221445 ) ) ;
#16415 = CARTESIAN_POINT ( 'NONE',  ( -19.63800298229563523, 92.92402754151969191, 59.99999999999999289 ) ) ;
#16416 = EDGE_CURVE ( 'NONE', #31700, #48297, #38264, .T. ) ;
#16417 = CARTESIAN_POINT ( 'NONE',  ( 82.64074333392795779, 53.51963485226765016, -15.73164264726942640 ) ) ;
#16418 = CARTESIAN_POINT ( 'NONE',  ( 197.7365809935693051, 288.1571905346162339, -17.55295824978644958 ) ) ;
#16419 = FACE_OUTER_BOUND ( 'NONE', #56705, .T. ) ;
#16420 = B_SPLINE_CURVE_WITH_KNOTS ( 'NONE', 3,
 ( #99580, #30672, #14477, #13493 ),
 .UNSPECIFIED., .F., .F.,
 ( 4, 4 ),
 ( 0.000000000000000000, 0.006832007640786700794 ),
 .UNSPECIFIED. ) ;
#16421 = CARTESIAN_POINT ( 'NONE',  ( 26.03951966209473312, 17.96004757982090538, -5.678558825948276656 ) ) ;
#16422 = CARTESIAN_POINT ( 'NONE',  ( 198.3572878714705610, 277.3135066751846125, -15.31504719882579302 ) ) ;
#16423 = CARTESIAN_POINT ( 'NONE',  ( 191.6434079017471959, 298.2851893172241944, -8.812442504271411181 ) ) ;
#16425 = ORIENTED_EDGE ( 'NONE', *, *, #59885, .F. ) ;
#16424 = CARTESIAN_POINT ( 'NONE',  ( 206.7596416265183734, 271.4678399409689291, 6.202658291405857227 ) ) ;
#16426 = CARTESIAN_POINT ( 'NONE',  ( 155.8152618860606253, 260.7670451491295012, 0.000000000000000000 ) ) ;
#16427 = CARTESIAN_POINT ( 'NONE',  ( 159.7132918459648181, 254.0154592091499239, -16.90058287995827158 ) ) ;
#16428 = ADVANCED_FACE ( 'NONE', ( #57986 ), #88968, .F. ) ;
#16429 = CARTESIAN_POINT ( 'NONE',  ( -22.42236680055709641, 157.8615022471902591, 0.000000000000000000 ) ) ;
#16430 = CARTESIAN_POINT ( 'NONE',  ( 84.83256327216713544, 45.63739360033983417, -9.320991929122717679 ) ) ;
#16431 = ADVANCED_FACE ( 'NONE', ( #50383 ), #95036, .F. ) ;
#16432 = CARTESIAN_POINT ( 'NONE',  ( 161.5504728662519369, 250.8333683393111926, 12.94300825113363373 ) ) ;
#16433 = CARTESIAN_POINT ( 'NONE',  ( 191.2038183216754987, 261.2453028453169281, -0.002002736021087949715 ) ) ;
#16434 =( BOUNDED_CURVE ( )  B_SPLINE_CURVE ( 2, ( #42567, #89734, #50186, #5579, #73500, #82137, #97807, #90736, #51694 ),
 .UNSPECIFIED., .F., .T. ) 
 B_SPLINE_CURVE_WITH_KNOTS ( ( 3, 2, 2, 2, 3 ),
 ( 0.1975806451612903136, 0.1989247311827956888, 0.2016129032258064391, 0.2043010752688172171, 0.2056451612903225923 ),
 .UNSPECIFIED. ) 
 CURVE ( )  GEOMETRIC_REPRESENTATION_ITEM ( )  RATIONAL_B_SPLINE_CURVE ( ( 0.9330127018922194093, 0.9330127018922194093, 1.000000000000000000, 0.8660254037844387076, 1.000000000000000000, 0.8660254037844387076, 1.000000000000000000, 0.9330127018922194093, 0.9330127018922194093 ) ) 
 REPRESENTATION_ITEM ( '' )  );
#16435 = ORIENTED_EDGE ( 'NONE', *, *, #57421, .T. ) ;
#16436 = CARTESIAN_POINT ( 'NONE',  ( 155.3935616475962149, 261.4974513877137952, -18.59422973016237890 ) ) ;
#16437 = DIRECTION ( 'NONE',  ( 0.7646402761589956576, 0.6444573283589029034, 0.000000000000000000 ) ) ;
#16438 = CYLINDRICAL_SURFACE ( 'NONE', #20874, 10.00000000000010658 ) ;
#16439 = CARTESIAN_POINT ( 'NONE',  ( 5.633247839328319628, 187.3927522451419634, 2.944929066748280225E-16 ) ) ;
#16440 = CARTESIAN_POINT ( 'NONE',  ( 91.51436070488293240, 214.4548013555409796, -4.594050593750042211 ) ) ;
#16441 = CARTESIAN_POINT ( 'NONE',  ( 82.12886798991216608, 40.75801620276044446, -0.7528608118565335294 ) ) ;
#16442 = CARTESIAN_POINT ( 'NONE',  ( 50.37091257173480585, 98.81520120758277415, 10.00000000000000000 ) ) ;
#16443 = CARTESIAN_POINT ( 'NONE',  ( 167.0158807670456440, 278.2951364720916558, -13.37185693470555137 ) ) ;
#16445 = DIRECTION ( 'NONE',  ( 0.1887253692075823441, -0.9820299053580097137, 0.000000000000000000 ) ) ;
#16444 = CARTESIAN_POINT ( 'NONE',  ( 12.46239254174337852, 171.8768266524160140, -9.188101187500091527 ) ) ;
#16446 = CARTESIAN_POINT ( 'NONE',  ( 161.2313178023453588, 251.3861611254901618, 13.12937145726518473 ) ) ;
#16447 = ORIENTED_EDGE ( 'NONE', *, *, #20153, .F. ) ;
#16448 = ORIENTED_EDGE ( 'NONE', *, *, #67714, .F. ) ;
#16449 = FACE_OUTER_BOUND ( 'NONE', #37908, .T. ) ;
#16450 =( BOUNDED_CURVE ( )  B_SPLINE_CURVE ( 2, ( #30543, #8247, #37625, #91375, #640, #85282, #92380, #38626, #7229 ),
 .UNSPECIFIED., .F., .T. ) 
 B_SPLINE_CURVE_WITH_KNOTS ( ( 3, 2, 2, 2, 3 ),
 ( 0.2137096774193548432, 0.2150537634408602183, 0.2177419354838709686, 0.2204301075268817189, 0.2217741935483870941 ),
 .UNSPECIFIED. ) 
 CURVE ( )  GEOMETRIC_REPRESENTATION_ITEM ( )  RATIONAL_B_SPLINE_CURVE ( ( 0.9330127018922194093, 0.9330127018922194093, 1.000000000000000000, 0.8660254037844387076, 1.000000000000000000, 0.8660254037844387076, 1.000000000000000000, 0.9330127018922194093, 0.9330127018922194093 ) ) 
 REPRESENTATION_ITEM ( '' )  );
#16451 = CARTESIAN_POINT ( 'NONE',  ( 84.56802347276283172, 46.19559949517749686, -10.17660803681333626 ) ) ;
#16452 = CARTESIAN_POINT ( 'NONE',  ( 85.04462449185939477, 45.37010230792124332, 8.864637975708317796 ) ) ;
#16453 = CIRCLE ( 'NONE', #74703, 17.82106496071138935 ) ;
#16454 = CARTESIAN_POINT ( 'NONE',  ( 207.8718670335145475, 270.6023601641878713, -6.322166851501095586 ) ) ;
#16455 = CARTESIAN_POINT ( 'NONE',  ( 90.16093569141993669, 222.8615022471902591, -10.00000000000009592 ) ) ;
#16456 = CARTESIAN_POINT ( 'NONE',  ( 74.42329672017201858, 68.02203094029241015, -11.65569731704910694 ) ) ;
#16457 = EDGE_CURVE ( 'NONE', #61410, #77081, #63587, .T. ) ;
#16458 = CARTESIAN_POINT ( 'NONE',  ( 40.22915850269944116, 194.0333772461660544, 9.188101187500095079 ) ) ;
#16459 = CARTESIAN_POINT ( 'NONE',  ( 199.7050857508973536, 277.1576266663558386, 15.11540184541819976 ) ) ;
#16460 = ORIENTED_EDGE ( 'NONE', *, *, #7400, .T. ) ;
#16461 = CARTESIAN_POINT ( 'NONE',  ( 152.9972683157861013, 273.5452038669419608, -11.80502568439283095 ) ) ;
#16462 = EDGE_CURVE ( 'NONE', #58717, #8050, #69993, .T. ) ;
#16463 = EDGE_CURVE ( 'NONE', #32845, #71681, #58906, .T. ) ;
#16464 = CARTESIAN_POINT ( 'NONE',  ( 175.2015549758991426, 281.4682759215078249, -14.19524567657169634 ) ) ;
#16465 = CARTESIAN_POINT ( 'NONE',  ( 196.0034224882197975, 291.1591091234520263, 17.53794140922627776 ) ) ;
#16466 = CARTESIAN_POINT ( 'NONE',  ( 38.90713653809340400, 79.99999999999998579, -10.00000000000000000 ) ) ;
#16467 = CARTESIAN_POINT ( 'NONE',  ( 67.64427519302456915, 199.8615022471901739, 5.000000000000051514 ) ) ;
#16468 = CARTESIAN_POINT ( 'NONE',  ( 186.2100982136382186, 283.2556687510013944, 16.40921232443700717 ) ) ;
#16469 = CARTESIAN_POINT ( 'NONE',  ( 194.4826705584825390, 293.7931287314651740, -16.11258321617245315 ) ) ;
#16470 = EDGE_CURVE ( 'NONE', #85165, #29132, #22696, .T. ) ;
#16471 = EDGE_CURVE ( 'NONE', #80971, #74122, #20000, .T. ) ;
#16472 = CARTESIAN_POINT ( 'NONE',  ( 189.4853509765368926, 263.0536865835545086, 7.945816303330112795 ) ) ;
#16473 = CARTESIAN_POINT ( 'NONE',  ( 168.6336870076176808, 278.4479093902589284, 14.14941165673452161 ) ) ;
#16474 = CARTESIAN_POINT ( 'NONE',  ( 80.44215978124604760, 58.39441083166273216, 0.000000000000000000 ) ) ;
#16475 = CARTESIAN_POINT ( 'NONE',  ( 69.84036666288623962, 69.98366574888289904, 5.148563393720963610 ) ) ;
#16476 = CARTESIAN_POINT ( 'NONE',  ( 190.3144310910409445, 301.0127312671879167, -1.334877248546042949 ) ) ;
#16477 = PLANE ( 'NONE',  #25313 ) ;
#16478 = VERTEX_POINT ( 'NONE', #25336 ) ;
#16479 = CARTESIAN_POINT ( 'NONE',  ( -14.67426454553563708, 35.33509950918588061, 59.99999999999999289 ) ) ;
#16480 = CARTESIAN_POINT ( 'NONE',  ( 163.7038023771459052, 247.1036922210055025, -6.448491958542482472 ) ) ;
#16481 = CARTESIAN_POINT ( 'NONE',  ( 181.3555717946182426, 267.9129953831518378, 15.03121414418437141 ) ) ;
#16482 = CARTESIAN_POINT ( 'NONE',  ( 120.4179585561885659, 231.1423013555409796, -4.594050593750043987 ) ) ;
#16483 = CARTESIAN_POINT ( 'NONE',  ( 11.45782370926791849, 18.56628583063839244, 9.188101187500006262 ) ) ;
#16484 = CARTESIAN_POINT ( 'NONE',  ( 191.1489696025915919, 299.5672681643093256, 8.892130899335590755 ) ) ;
#16485 = LINE ( 'NONE', #94526, #29005 ) ;
#16487 = CARTESIAN_POINT ( 'NONE',  ( 194.4026365859849932, 278.7051034128888318, 16.29805033731604169 ) ) ;
#16486 = FACE_OUTER_BOUND ( 'NONE', #37660, .T. ) ;
#16488 = CARTESIAN_POINT ( 'NONE',  ( 204.2346432313999571, 272.7292428585745370, -9.744538825520306702 ) ) ;
#16489 = CARTESIAN_POINT ( 'NONE',  ( 191.3704903915450188, 262.8878367245375784, -4.354269820778342570 ) ) ;
#16490 = DIRECTION ( 'NONE',  ( 1.000000000000000000, -1.189524669241238790E-13, 0.000000000000000000 ) ) ;
#16491 = CARTESIAN_POINT ( 'NONE',  ( 106.0200258946745322, 242.0177522451419350, 5.000000000000046185 ) ) ;
#16492 = CARTESIAN_POINT ( 'NONE',  ( 67.28077729273597640, 69.97196434288713363, 0.1681859604356396032 ) ) ;
#16493 = VERTEX_POINT ( 'NONE', #30073 ) ;
#16494 = CARTESIAN_POINT ( 'NONE',  ( 192.4371825538271992, 267.1441898236624297, 11.03930663723062011 ) ) ;
#16495 = AXIS2_PLACEMENT_3D ( 'NONE', #19555, #72760, #50415 ) ;
#16496 = CARTESIAN_POINT ( 'NONE',  ( -19.65312891409030271, 93.06504152958497400, 10.00000000000000888 ) ) ;
#16497 = CARTESIAN_POINT ( 'NONE',  ( 82.18936110093612513, 52.64993106124108380, 15.54926669311582188 ) ) ;
#16498 = ORIENTED_EDGE ( 'NONE', *, *, #35836, .T. ) ;
#16499 = B_SPLINE_SURFACE_WITH_KNOTS ( 'NONE', 3, 1, ( 
 ( #23909, #8224 ),
 ( #85786, #70512 ),
 ( #24419, #63913 ),
 ( #33524, #55296 ),
 ( #62913, #2131 ),
 ( #62396, #93352 ),
 ( #16317, #40602 ),
 ( #41097, #55786 ),
 ( #86276, #9220 ),
 ( #56304, #39591 ),
 ( #94852, #86779 ),
 ( #56809, #78133 ),
 ( #48217, #71038 ),
 ( #25412, #18335 ),
 ( #16812, #40096 ),
 ( #43601, #90258 ),
 ( #97338, #49712 ),
 ( #4109, #74538 ),
 ( #20326, #42107 ),
 ( #59280, #11731 ),
 ( #89758, #50212 ),
 ( #81653, #73041 ),
 ( #72547, #88278 ),
 ( #81165, #65414 ),
 ( #51196, #74028 ),
 ( #18831, #34514 ),
 ( #95870, #41604 ),
 ( #80667, #11244 ),
 ( #58303, #96357 ),
 ( #4616, #89279 ),
 ( #5116, #73527 ),
 ( #64925, #65904 ),
 ( #12226, #19828 ),
 ( #35997, #43085 ) ),
 .UNSPECIFIED., .T., .F., .F.,
 ( 4, 2, 2, 2, 2, 2, 2, 2, 2, 2, 2, 2, 2, 2, 2, 2, 4 ),
 ( 2, 2 ),
 ( 0.000000000000000000, 0.06250000000000000000, 0.1250000000000000000, 0.1875000000000000000, 0.2500000000000000000, 0.3125000000000000000, 0.3750000000000000000, 0.4375000000000000000, 0.5000000000000000000, 0.5625000000000000000, 0.6250000000000000000, 0.6875000000000000000, 0.7500000000000000000, 0.8125000000000000000, 0.8750000000000000000, 0.9375000000000000000, 1.000000000000000000 ),
 ( 0.000000000000000000, 1.000000000000000000 ),
 .UNSPECIFIED. ) ;
#16500 = CARTESIAN_POINT ( 'NONE',  ( 75.91502559367474134, 65.16891969575354437, -14.48077610374784996 ) ) ;
#16501 = CARTESIAN_POINT ( 'NONE',  ( 180.2632815608440637, 290.9457125825060189, -11.14479853889756988 ) ) ;
#16502 = DIRECTION ( 'NONE',  ( -0.4330127018922203530, 0.7500000000000046629, 0.4999999999999919509 ) ) ;
#16503 = CARTESIAN_POINT ( 'NONE',  ( 74.94245617315240793, 53.14056109367614056, -16.50934518181217925 ) ) ;
#16504 = LINE ( 'NONE', #802, #27403 ) ;
#16505 = ORIENTED_EDGE ( 'NONE', *, *, #9431, .T. ) ;
#16506 = CARTESIAN_POINT ( 'NONE',  ( 184.9912140082997780, 297.8717511433786171, -3.135484508529590819 ) ) ;
#16507 = CARTESIAN_POINT ( 'NONE',  ( 32.39821438149254362, 40.74646525600392977, 2.839279412974139660 ) ) ;
#16508 = ORIENTED_EDGE ( 'NONE', *, *, #69063, .F. ) ;
#16509 = CARTESIAN_POINT ( 'NONE',  ( 78.44787846840736734, 61.26446607870955319, 16.23792605971962999 ) ) ;
#16510 = EDGE_CURVE ( 'NONE', #2250, #25608, #33443, .T. ) ;
#16511 = CARTESIAN_POINT ( 'NONE',  ( -44.49648453423614569, 28.96346851210257967, -10.00000000000000000 ) ) ;
#16512 = CARTESIAN_POINT ( 'NONE',  ( 199.0226767019651106, 265.2340503415149442, -1.818814813163766475 ) ) ;
#16513 = ORIENTED_EDGE ( 'NONE', *, *, #20961, .T. ) ;
#16514 = CARTESIAN_POINT ( 'NONE',  ( 86.30773806088525646, 46.95517243064260526, -10.53307507464019821 ) ) ;
#16515 = CARTESIAN_POINT ( 'NONE',  ( 159.9040744856012850, 255.4269131533854420, 16.38690128260775936 ) ) ;
#16516 = CARTESIAN_POINT ( 'NONE',  ( 204.1780753366177237, 277.0001950557890495, 14.05599973203924158 ) ) ;
#16517 = CARTESIAN_POINT ( 'NONE',  ( 88.36930832042526163, 44.08004549128393990, -2.853748190838125254 ) ) ;
#16518 = CARTESIAN_POINT ( 'NONE',  ( 172.0910100529608258, 260.0785035667472584, 15.53398388876759206 ) ) ;
#16519 = CARTESIAN_POINT ( 'NONE',  ( 79.36263291408793918, 45.67866562566761957, -12.88899626193393821 ) ) ;
#16520 = CARTESIAN_POINT ( 'NONE',  ( 203.3684377202211522, 278.4025285431072803, -16.56116267537666076 ) ) ;
#16521 = ORIENTED_EDGE ( 'NONE', *, *, #7043, .T. ) ;
#16522 = EDGE_LOOP ( 'NONE', ( #24736, #14578, #49050, #97638 ) ) ;
#16523 = CARTESIAN_POINT ( 'NONE',  ( 195.9433989068402298, 290.8109596964202979, 15.97351100229838039 ) ) ;
#16524 = VERTEX_POINT ( 'NONE', #22476 ) ;
#16525 = CARTESIAN_POINT ( 'NONE',  ( 77.24698020313218194, 49.64373807359542212, -15.49284761250392428 ) ) ;
#16526 = ORIENTED_EDGE ( 'NONE', *, *, #46324, .F. ) ;
#16527 = CARTESIAN_POINT ( 'NONE',  ( 86.97822204926990253, 45.79386009709899952, -8.643660422075560845 ) ) ;
#16528 = CARTESIAN_POINT ( 'NONE',  ( 78.57569412390834884, 50.34383551948430835, 14.98634759621179136 ) ) ;
#16529 = VERTEX_POINT ( 'NONE', #7266 ) ;
#16530 = CARTESIAN_POINT ( 'NONE',  ( 80.87517248313827167, 58.64441083166272506, 0.000000000000000000 ) ) ;
#16531 = CARTESIAN_POINT ( 'NONE',  ( 164.2904957002474191, 246.0875095769322911, -1.594749884056509748 ) ) ;
#16532 = CARTESIAN_POINT ( 'NONE',  ( 189.9106593378625689, 301.7120844583541839, 2.757488645815840744 ) ) ;
#16533 = LINE ( 'NONE', #70737, #39944 ) ;
#16534 = CARTESIAN_POINT ( 'NONE',  ( 82.30540685579956062, 40.88228610481488801, 1.021405830961136685 ) ) ;
#16535 = CARTESIAN_POINT ( 'NONE',  ( 167.6408814478219256, 249.1979298630905362, -5.423656658118427565 ) ) ;
#16536 = CARTESIAN_POINT ( 'NONE',  ( 76.94978126365660387, 62.92300403630901684, -15.24643684403981858 ) ) ;
#16537 = EDGE_CURVE ( 'NONE', #22359, #33337, #16637, .T. ) ;
#16538 = CARTESIAN_POINT ( 'NONE',  ( 154.2046094046408768, 279.5503029169213391, 2.157256874705086869 ) ) ;
#16539 = CARTESIAN_POINT ( 'NONE',  ( 125.6409139509397050, 243.3458772461660544, 9.188101187500095079 ) ) ;
#16540 = ORIENTED_EDGE ( 'NONE', *, *, #67351, .F. ) ;
#16541 = CARTESIAN_POINT ( 'NONE',  ( 183.8986139101176036, 260.8653061663941912, -9.197505754419971424 ) ) ;
#16542 = CARTESIAN_POINT ( 'NONE',  ( 39.98734656443052415, 28.80170272979929535, 7.433330006724137462 ) ) ;
#16543 = ORIENTED_EDGE ( 'NONE', *, *, #80813, .F. ) ;
#16544 = CARTESIAN_POINT ( 'NONE',  ( 155.3053666857671260, 275.9298431561234111, 11.76907774355536418 ) ) ;
#16545 = CARTESIAN_POINT ( 'NONE',  ( 200.1572343898514816, 273.9495814528414144, 13.62147189966721683 ) ) ;
#16546 = CARTESIAN_POINT ( 'NONE',  ( 177.5773431977876839, 253.6316530246629952, 1.366461747843389807 ) ) ;
#16547 = CARTESIAN_POINT ( 'NONE',  ( 174.2556954761228383, 290.5492199356207834, -4.866737863781906981 ) ) ;
#16548 = CARTESIAN_POINT ( 'NONE',  ( 192.7328199212471134, 296.8239589408137249, 11.25304608637181225 ) ) ;
#16549 = CARTESIAN_POINT ( 'NONE',  ( -169.5327448629461742, 46.94652375874896677, 30.52142883766498827 ) ) ;
#16550 = EDGE_CURVE ( 'NONE', #23594, #32604, #93962, .T. ) ;
#16551 = CARTESIAN_POINT ( 'NONE',  ( 80.95762699323942968, 43.02477363226272189, 9.576251469719451848 ) ) ;
#16552 = CARTESIAN_POINT ( 'NONE',  ( 173.4599143460859239, 287.1962067271440446, -9.656697716713990687 ) ) ;
#16553 = CARTESIAN_POINT ( 'NONE',  ( 194.7368014691935514, 293.3529610823404710, 16.16394032022910920 ) ) ;
#16554 = EDGE_CURVE ( 'NONE', #76220, #37198, #72232, .T. ) ;
#16555 = CARTESIAN_POINT ( 'NONE',  ( 183.6215648671697522, 257.5753772875778509, -6.308267261209747012 ) ) ;
#16556 = ADVANCED_FACE ( 'NONE', ( #77171 ), #53850, .F. ) ;
#16557 = ORIENTED_EDGE ( 'NONE', *, *, #91175, .F. ) ;
#16558 = DIRECTION ( 'NONE',  ( -0.4755282581475737680, 0.8236391035463299648, -0.3090169943749573878 ) ) ;
#16559 = CARTESIAN_POINT ( 'NONE',  ( 151.0149486366368023, 272.2794807016773575, 11.70507281214681861 ) ) ;
#16560 = ORIENTED_EDGE ( 'NONE', *, *, #11590, .F. ) ;
#16561 = DIRECTION ( 'NONE',  ( 1.000000000000000000, 0.000000000000000000, 0.000000000000000000 ) ) ;
#16562 = B_SPLINE_CURVE_WITH_KNOTS ( 'NONE', 3,
 ( #55524, #16544, #56544, #94091 ),
 .UNSPECIFIED., .F., .F.,
 ( 4, 4 ),
 ( 0.006736008396846960601, 0.01176074928893414140 ),
 .UNSPECIFIED. ) ;
#16563 = CARTESIAN_POINT ( 'NONE',  ( 81.22979812886450190, 55.45288652294036780, -16.34461090620093771 ) ) ;
#16564 = CARTESIAN_POINT ( 'NONE',  ( 191.6240736048601718, 298.7443638935011450, -10.89653124444694932 ) ) ;
#16565 = CARTESIAN_POINT ( 'NONE',  ( 190.1751179328237242, 301.2540287353828035, 3.252640783176552475 ) ) ;
#16566 = CARTESIAN_POINT ( 'NONE',  ( 70.18948356013267187, 71.57821204930945669, -1.478097172221414013 ) ) ;
#16568 = CARTESIAN_POINT ( 'NONE',  ( 154.7234497803183331, 277.1669817346232207, -8.779482032178238526 ) ) ;
#16567 = CARTESIAN_POINT ( 'NONE',  ( 161.8372659878727973, 281.7041345820564970, -6.599806340034523267 ) ) ;
#16569 = CARTESIAN_POINT ( 'NONE',  ( 152.6740002182599767, 266.2078699576288159, -17.16212636348624088 ) ) ;
#16570 = ORIENTED_EDGE ( 'NONE', *, *, #14398, .F. ) ;
#16571 = CARTESIAN_POINT ( 'NONE',  ( 146.8358616138309571, 276.3198226421291679, 4.054088818585255716 ) ) ;
#16572 = CARTESIAN_POINT ( 'NONE',  ( 164.3663504224794565, 247.9561253440330972, -9.019399920391260039 ) ) ;
#16573 = DIRECTION ( 'NONE',  ( 0.000000000000000000, 0.000000000000000000, 1.000000000000000000 ) ) ;
#16574 = CARTESIAN_POINT ( 'NONE',  ( 87.86584501647516277, 43.90525888894924833, 0.3790033701962610135 ) ) ;
#16575 = CARTESIAN_POINT ( 'NONE',  ( 188.5957227590319292, 298.5807065412511179, -4.256663340113655103 ) ) ;
#16576 = CARTESIAN_POINT ( 'NONE',  ( 192.1640094933931096, 297.8091675017319062, 12.36911124822534447 ) ) ;
#16577 = CARTESIAN_POINT ( 'NONE',  ( 204.7200661083698776, 274.0614395018808978, 12.25436898028725530 ) ) ;
#16578 = CARTESIAN_POINT ( 'NONE',  ( 73.99564936472528132, 68.61382277044870648, 10.90295599471779120 ) ) ;
#16579 = CARTESIAN_POINT ( 'NONE',  ( 69.97271289134489791, 71.02073340580969329, -1.163651360304144511 ) ) ;
#16580 = ADVANCED_FACE ( 'NONE', ( #14866 ), #40526, .T. ) ;
#16581 = B_SPLINE_CURVE_WITH_KNOTS ( 'NONE', 3,
 ( #40853, #71799, #10484, #26186, #41362, #70778, #2911, #70267, #94614, #47960, #64179, #78902, #33804, #64687, #95637, #63174, #95127, #47471, #16075, #875, #25693, #62660, #93612, #86539, #55062, #78394, #9489, #8975, #80427, #73784, #89057, #11991, #19608, #28171, #36263, #5377, #34767, #4374, #57565, #20586, #82435, #67164, #28663, #72814, #58076, #18594, #49472, #65667 ),
 .UNSPECIFIED., .F., .F.,
 ( 4, 2, 2, 2, 2, 2, 2, 2, 2, 2, 2, 2, 2, 2, 2, 2, 2, 2, 2, 2, 2, 2, 2, 4 ),
 ( 0.0005625401255440777831, 0.0009993461653160591509, 0.001217749185202049618, 0.001326950695145041490, 0.001436152205088033363, 0.001545353715031025236, 0.001654555224974016891, 0.001872958244859952498, 0.002309764284631770151, 0.003183376364175405891, 0.004056988443719042499, 0.004930600523262678239, 0.005367406563034496543, 0.005585809582920406129, 0.005695011092863360921, 0.005749611847834837017, 0.005804212602806313979, 0.005858813357777790942, 0.005913414112749267905, 0.006022615622692071777, 0.006241018642577681255, 0.006677824682348895008, 0.007114630722120110495, 0.007551436761891325115 ),
 .UNSPECIFIED. ) ;
#16582 = CARTESIAN_POINT ( 'NONE',  ( 0.9064528339360315989, 162.1423013555410080, -4.594050593750043987 ) ) ;
#16583 = CARTESIAN_POINT ( 'NONE',  ( 99.30858933894288043, 218.9548013555409511, -4.594050593750042211 ) ) ;
#16584 = CARTESIAN_POINT ( 'NONE',  ( 67.16256804578091533, 66.80979783321161847, 8.146902435796070208 ) ) ;
#16585 = CARTESIAN_POINT ( 'NONE',  ( 146.9370072200009645, 276.1446333132804511, -3.799807221059707363 ) ) ;
#16586 = LINE ( 'NONE', #71308, #5869 ) ;
#16587 = CARTESIAN_POINT ( 'NONE',  ( 154.9048824156581361, 262.3438686460345366, -17.40627786727128168 ) ) ;
#16588 = VECTOR ( 'NONE', #85261, 1000.000000000000114 ) ;
#16589 = CARTESIAN_POINT ( 'NONE',  ( 161.8882824960653579, 250.2482648971885340, -13.83574485983625557 ) ) ;
#16590 = CARTESIAN_POINT ( 'NONE',  ( 163.0683798854284703, 248.2042762609320903, 11.26611642476872710 ) ) ;
#16591 = CARTESIAN_POINT ( 'NONE',  ( -50.24117156905492720, 92.72553494444620981, 36.50000000000000000 ) ) ;
#16592 = LINE ( 'NONE', #18102, #100140 ) ;
#16593 = CARTESIAN_POINT ( 'NONE',  ( 180.2909215930809523, 290.7362029762227849, 9.342184055492005257 ) ) ;
#16594 = CARTESIAN_POINT ( 'NONE',  ( 169.2536829177031450, 252.1151759106098211, -8.809847033144830419 ) ) ;
#16595 = CARTESIAN_POINT ( 'NONE',  ( 164.3239256700930468, 246.0296071706643772, -4.221892678519003184 ) ) ;
#16596 = CARTESIAN_POINT ( 'NONE',  ( 196.0355168007595523, 291.1035201434990540, 17.55377893960077884 ) ) ;
#16597 = DIRECTION ( 'NONE',  ( 1.000000000000000000, 0.000000000000000000, 0.000000000000000000 ) ) ;
#16598 = CARTESIAN_POINT ( 'NONE',  ( 207.7296438747196134, 270.8486979012336633, -6.692930657757584001 ) ) ;
#16599 = CARTESIAN_POINT ( 'NONE',  ( 33.89617418964321871, 196.5024278399160949, -9.188101187500093303 ) ) ;
#16600 = CARTESIAN_POINT ( 'NONE',  ( 71.67687952550437558, 206.0643266524160140, 9.188101187500095079 ) ) ;
#16601 = CARTESIAN_POINT ( 'NONE',  ( 66.04860371747962233, 197.3932355074535678, -2.679491924311248496 ) ) ;
#16602 = CARTESIAN_POINT ( 'NONE',  ( 88.23407674691928548, 43.71813397101750098, 0.1961470715255511643 ) ) ;
#16603 = CARTESIAN_POINT ( 'NONE',  ( 101.8522786425098730, 229.6115022471902307, 10.00000000000009592 ) ) ;
#16605 = CARTESIAN_POINT ( 'NONE',  ( 70.98065340298427373, 71.07006770911269200, -5.392052274046765348 ) ) ;
#16604 = CARTESIAN_POINT ( 'NONE',  ( 71.92536400468701174, 72.18844424196340981, -3.635291937859653544 ) ) ;
#16606 = B_SPLINE_CURVE_WITH_KNOTS ( 'NONE', 3,
 ( #51893, #35690, #81338, #19020 ),
 .UNSPECIFIED., .F., .F.,
 ( 4, 4 ),
 ( 0.009370377214594900056, 0.01414487375777262641 ),
 .UNSPECIFIED. ) ;
#16607 = EDGE_CURVE ( 'NONE', #6688, #78977, #76679, .T. ) ;
#16608 = CARTESIAN_POINT ( 'NONE',  ( 196.2367626659915345, 269.4862306000135845, -10.76191796027563896 ) ) ;
#16609 = CARTESIAN_POINT ( 'NONE',  ( 24.26418115112394602, 34.98502408145593279, -5.678558825948271327 ) ) ;
#16610 = CARTESIAN_POINT ( 'NONE',  ( 198.6363782946250183, 286.5986958926748116, -18.50260615857378355 ) ) ;
#16611 = CARTESIAN_POINT ( 'NONE',  ( 196.3286486926436680, 290.5958008134369948, -16.58330917766970458 ) ) ;
#16612 = CARTESIAN_POINT ( 'NONE',  ( 17.70402515066951565, 13.14754757982089295, -5.678558825948276656 ) ) ;
#16613 = CARTESIAN_POINT ( 'NONE',  ( 67.69866210081085001, 200.7048013555409796, 4.594050593750051981 ) ) ;
#16614 = CARTESIAN_POINT ( 'NONE',  ( 170.7953178271928039, 255.2457615276028093, -12.92277808742838374 ) ) ;
#16615 = CARTESIAN_POINT ( 'NONE',  ( 202.8151641853381477, 279.3608264160075692, -16.28741359973609448 ) ) ;
#16616 = CARTESIAN_POINT ( 'NONE',  ( 197.8809552785519656, 287.9071269377202498, 17.61728046362068412 ) ) ;
#16617 = CARTESIAN_POINT ( 'NONE',  ( 69.53570971148970159, 62.57802854026397910, -13.90760378158714161 ) ) ;
#16618 = CARTESIAN_POINT ( 'NONE',  ( 198.9738057768446993, 281.0626889417751499, 17.36572826697628003 ) ) ;
#16619 = CARTESIAN_POINT ( 'NONE',  ( 75.82058630256133824, 56.59402139164659218, -16.13716463214695906 ) ) ;
#16620 = CARTESIAN_POINT ( 'NONE',  ( 87.65075002439434115, 44.95127668719692338, -6.583683359477274344 ) ) ;
#16621 = CARTESIAN_POINT ( 'NONE',  ( 104.8833675557553704, 241.3615022471903160, 5.000000000000046185 ) ) ;
#16622 = CARTESIAN_POINT ( 'NONE',  ( 161.8662906133268393, 250.2863559554455719, 14.03735902266321744 ) ) ;
#16623 = CARTESIAN_POINT ( 'NONE',  ( 164.9779129355220562, 244.8968679994381148, -1.771286574179712803 ) ) ;
#16624 = ORIENTED_EDGE ( 'NONE', *, *, #30604, .T. ) ;
#16625 = CARTESIAN_POINT ( 'NONE',  ( 77.42326786333445909, 49.55262521988469615, 14.91231252120838846 ) ) ;
#16626 = CARTESIAN_POINT ( 'NONE',  ( 187.3515396730908265, 272.9474742628501645, 15.64971660612648030 ) ) ;
#16627 = ORIENTED_EDGE ( 'NONE', *, *, #11154, .T. ) ;
#16628 = CARTESIAN_POINT ( 'NONE',  ( 206.8851632406098702, 272.3113812655195716, -9.957011741946159233 ) ) ;
#16629 = CARTESIAN_POINT ( 'NONE',  ( 190.1002787791093738, 279.3508125853905426, -17.07129022450704525 ) ) ;
#16630 = CARTESIAN_POINT ( 'NONE',  ( 73.50461245277466560, 72.41059528448880656, 0.000000000000000000 ) ) ;
#16631 = VERTEX_POINT ( 'NONE', #15350 ) ;
#16632 = CARTESIAN_POINT ( 'NONE',  ( 173.2992619767147744, 251.6738639471601857, -0.1807056420497624716 ) ) ;
#16633 = ORIENTED_EDGE ( 'NONE', *, *, #42572, .F. ) ;
#16634 = CARTESIAN_POINT ( 'NONE',  ( 72.49672817265226854, 71.70303783552662935, 5.966909785267804800 ) ) ;
#16635 = CARTESIAN_POINT ( 'NONE',  ( 194.9385458806846430, 293.0035295114944347, -15.70518692812489192 ) ) ;
#16636 = DIRECTION ( 'NONE',  ( -0.8660254037844387076, -0.4999999999999998890, -0.000000000000000000 ) ) ;
#16637 = CIRCLE ( 'NONE', #26336, 70.00000000000001421 ) ;
#16638 = ORIENTED_EDGE ( 'NONE', *, *, #1993, .F. ) ;
#16639 = CARTESIAN_POINT ( 'NONE',  ( 29.31959766232195008, 28.87878583063843152, -9.188101187500006262 ) ) ;
#16640 = CARTESIAN_POINT ( 'NONE',  ( 26.34568874650619463, 186.0177522451418497, -10.00000000000009592 ) ) ;
#16641 = CARTESIAN_POINT ( 'NONE',  ( 74.94692089407369906, 66.84572622250873053, -13.20830831734917865 ) ) ;
#16642 = CARTESIAN_POINT ( 'NONE',  ( 77.54361356138011274, 49.75803992512373952, -14.96129575302290249 ) ) ;
#16643 = VECTOR ( 'NONE', #16382, 1000.000000000000000 ) ;
#16644 = ORIENTED_EDGE ( 'NONE', *, *, #65419, .F. ) ;
#16645 = LINE ( 'NONE', #33874, #17420 ) ;
#16646 = B_SPLINE_CURVE_WITH_KNOTS ( 'NONE', 3,
 ( #42539, #18773, #25880, #18276, #27856, #64360, #10172, #49171, #80106, #57246, #19291, #80608, #96296, #41548, #41039, #11185, #71975, #72987, #89227, #3095, #88721, #3578, #19776, #50158, #34459, #73472, #26865, #4055, #81110, #57744, #65842, #96806, #27365, #58248, #81597, #12166, #98272, #68836, #59222, #20268, #90198, #97775, #91681, #12677, #14152, #7041, #52633, #60718, #59738, #44031 ),
 .UNSPECIFIED., .F., .F.,
 ( 4, 2, 2, 2, 2, 2, 2, 2, 2, 2, 2, 2, 2, 2, 2, 2, 2, 2, 2, 2, 2, 2, 2, 2, 4 ),
 ( 0.0005940201049859090802, 0.001027528587323273124, 0.001244282828491905489, 0.001352659949076183941, 0.001461037069660462394, 0.001569414190244740846, 0.001677791310829019299, 0.001894545551997614367, 0.002328054034334755065, 0.003195070999009091972, 0.004062087963683428879, 0.004929104928357765786, 0.005362613410694924698, 0.005579367651863502420, 0.005687744772447786076, 0.005741933332739927037, 0.005796121893032067998, 0.005850310453324208959, 0.005904499013616349920, 0.006012876134200668271, 0.006229630375369433343, 0.006663138857707095325, 0.006879893098875905499, 0.007096647340044715674, 0.007530155822382190306 ),
 .UNSPECIFIED. ) ;
#16647 = CARTESIAN_POINT ( 'NONE',  ( 160.1795347027651815, 282.8633239002924711, 5.491715875156680582 ) ) ;
#16648 = ORIENTED_EDGE ( 'NONE', *, *, #58669, .T. ) ;
#16649 = CARTESIAN_POINT ( 'NONE',  ( 170.8148024314547797, 284.7141682455830960, 10.99588700018169618 ) ) ;
#16651 = CARTESIAN_POINT ( 'NONE',  ( 68.23134756035658199, 65.67744778407723061, -10.30070688804788759 ) ) ;
#16650 = CARTESIAN_POINT ( 'NONE',  ( 67.77223724734612631, 65.62443007439019027, 10.08236501146177311 ) ) ;
#16652 = CARTESIAN_POINT ( 'NONE',  ( 163.4178923001155681, 247.5989030008181260, -10.38047187240561442 ) ) ;
#16653 = CARTESIAN_POINT ( 'NONE',  ( 185.2391986358457530, 295.7873944733689768, 8.585680893828113724 ) ) ;
#16654 = CARTESIAN_POINT ( 'NONE',  ( 70.79254675561878685, 71.95096862338711219, -1.204795362960673355 ) ) ;
#16655 = CARTESIAN_POINT ( 'NONE',  ( 157.3661765229227285, 258.0807821998820373, -18.27254492731150748 ) ) ;
#16656 = CARTESIAN_POINT ( 'NONE',  ( 147.8871150585349881, 250.0643266524159571, -9.188101187500093303 ) ) ;
#16657 = CARTESIAN_POINT ( 'NONE',  ( 206.4855316718497704, 270.5831568970470471, 2.844589147210771163 ) ) ;
#16658 = VECTOR ( 'NONE', #93679, 1000.000000000000000 ) ;
#16659 = CARTESIAN_POINT ( 'NONE',  ( 79.27109561811333549, 59.78567773455861811, 16.51039248270449278 ) ) ;
#16660 = CARTESIAN_POINT ( 'NONE',  ( 89.53865347855843027, 216.3768266524159856, 9.188101187500098632 ) ) ;
#16661 = ORIENTED_EDGE ( 'NONE', *, *, #9635, .F. ) ;
#16662 = CARTESIAN_POINT ( 'NONE',  ( 191.3638605175971747, 299.1950661814348678, 7.382965314423603154 ) ) ;
#16663 = CARTESIAN_POINT ( 'NONE',  ( 77.96041703586088545, 62.15569039082562597, -15.98643159653562940 ) ) ;
#16664 = ORIENTED_EDGE ( 'NONE', *, *, #98727, .F. ) ;
#16665 = CARTESIAN_POINT ( 'NONE',  ( 195.3366900501289081, 292.3139235812797097, -16.23544628325368677 ) ) ;
#16666 = ORIENTED_EDGE ( 'NONE', *, *, #23575, .F. ) ;
#16667 = VERTEX_POINT ( 'NONE', #32934 ) ;
#16668 = CARTESIAN_POINT ( 'NONE',  ( 79.90085239356115210, 44.63345658378899117, -11.16155600664863812 ) ) ;
#16669 = DIRECTION ( 'NONE',  ( 1.000000000000000000, 0.000000000000000000, 0.000000000000000000 ) ) ;
#16670 = B_SPLINE_CURVE_WITH_KNOTS ( 'NONE', 3,
 ( #26984, #58842, #65971, #20890 ),
 .UNSPECIFIED., .F., .F.,
 ( 4, 4 ),
 ( 0.01149519226291654053, 0.01747808870979753251 ),
 .UNSPECIFIED. ) ;
#16671 = CARTESIAN_POINT ( 'NONE',  ( -19.65312891409030271, 93.06504152958497400, 59.99999999999999289 ) ) ;
#16672 = CARTESIAN_POINT ( 'NONE',  ( -48.10310308390612022, 75.88598450110713145, -10.00000000000000000 ) ) ;
#16673 = CARTESIAN_POINT ( 'NONE',  ( 85.74833574201379349, 47.06672189974739950, -10.43935527095086613 ) ) ;
#16674 = EDGE_CURVE ( 'NONE', #35319, #1341, #29585, .T. ) ;
#16675 = CYLINDRICAL_SURFACE ( 'NONE', #22056, 17.82106496071139645 ) ;
#16676 = CARTESIAN_POINT ( 'NONE',  ( 85.69549220138247847, 220.2833772461660544, -9.188101187500095079 ) ) ;
#16677 = ORIENTED_EDGE ( 'NONE', *, *, #2397, .F. ) ;
#16678 = EDGE_CURVE ( 'NONE', #47832, #39418, #67354, .T. ) ;
#16679 = ORIENTED_EDGE ( 'NONE', *, *, #63333, .F. ) ;
#16681 = EDGE_CURVE ( 'NONE', #40696, #81604, #23658, .T. ) ;
#16680 = CARTESIAN_POINT ( 'NONE',  ( 208.0006710756887287, 270.3792650189220126, -0.8737665032493013850 ) ) ;
#16682 = ORIENTED_EDGE ( 'NONE', *, *, #60800, .T. ) ;
#16683 = B_SPLINE_CURVE_WITH_KNOTS ( 'NONE', 3,
 ( #27791, #59662, #27296, #88652 ),
 .UNSPECIFIED., .F., .F.,
 ( 4, 4 ),
 ( 0.003490422054099921560, 0.008938099447508861262 ),
 .UNSPECIFIED. ) ;
#16684 = CARTESIAN_POINT ( 'NONE',  ( 26.11609497015385983, 119.4899152597536869, -54.99999999999999289 ) ) ;
#16685 = EDGE_CURVE ( 'NONE', #82885, #18415, #35514, .T. ) ;
#16686 = CARTESIAN_POINT ( 'NONE',  ( 75.84116199970137018, 65.13315491392486933, -14.47742810051069284 ) ) ;
#16687 = CARTESIAN_POINT ( 'NONE',  ( 198.4864866673927963, 270.7146468523363865, -12.49260379043138158 ) ) ;
#16688 = CARTESIAN_POINT ( 'NONE',  ( 182.6190391695882624, 260.4331822435277104, -11.41224075906783497 ) ) ;
#16689 = CARTESIAN_POINT ( 'NONE',  ( 88.00526762198180108, 44.79707723138842113, 4.734962078095950488 ) ) ;
#16690 = ORIENTED_EDGE ( 'NONE', *, *, #81302, .T. ) ;
#16691 = CARTESIAN_POINT ( 'NONE',  ( 189.3799976626108048, 295.0441500152971344, 11.39732311151665733 ) ) ;
#16692 = CARTESIAN_POINT ( 'NONE',  ( 185.8665295013605601, 259.3226075094696057, 5.962194205549277370 ) ) ;
#16693 = CARTESIAN_POINT ( 'NONE',  ( 206.2809287719926488, 273.3579460648492159, -10.70911012174624588 ) ) ;
#16694 = CARTESIAN_POINT ( 'NONE',  ( 147.7893382324786273, 275.1191502349608982, -4.499236673701186184 ) ) ;
#16695 = CARTESIAN_POINT ( 'NONE',  ( -11.40312891409031693, 78.77562236714182120, 59.99999999999999289 ) ) ;
#16696 = CARTESIAN_POINT ( 'NONE',  ( 72.52401626864599393, 70.66912915067958068, 7.194662573583692655 ) ) ;
#16697 = CARTESIAN_POINT ( 'NONE',  ( 195.6914848190668863, 279.7035040353765680, -17.46620344769279853 ) ) ;
#16698 = ORIENTED_EDGE ( 'NONE', *, *, #50936, .F. ) ;
#16699 = CARTESIAN_POINT ( 'NONE',  ( 49.91331508509971115, 100.8438505198844553, -10.00000000000000000 ) ) ;
#16700 = CARTESIAN_POINT ( 'NONE',  ( 161.2799361541916028, 251.3019516699124836, 14.40628917569557110 ) ) ;
#16701 = CARTESIAN_POINT ( 'NONE',  ( 86.22410369846130607, 45.53897050033827298, 8.200890175624763856 ) ) ;
#16702 = CARTESIAN_POINT ( 'NONE',  ( 187.4537318743986987, 265.8610463774303980, -11.83450410342445736 ) ) ;
#16703 = CARTESIAN_POINT ( 'NONE',  ( 199.0746189151364831, 265.2438329385483939, 1.559867394473611002 ) ) ;
#16704 = CARTESIAN_POINT ( 'NONE',  ( 68.11396990072299218, 66.09066184265174115, -10.54551009852403709 ) ) ;
#16705 = ORIENTED_EDGE ( 'NONE', *, *, #88378, .T. ) ;
#16706 = CARTESIAN_POINT ( 'NONE',  ( 202.4323889586180201, 280.0238125565655878, 15.69595176008160919 ) ) ;
#16707 = VECTOR ( 'NONE', #66705, 999.9999999999998863 ) ;
#16708 = CARTESIAN_POINT ( 'NONE',  ( 207.1601050488701503, 271.8351680844880889, 6.320235450527015075 ) ) ;
#16710 = DIRECTION ( 'NONE',  ( -0.8660254037844379305, -0.5000000000000014433, -0.000000000000000000 ) ) ;
#16709 = CARTESIAN_POINT ( 'NONE',  ( 177.4388027723078665, 264.4896303202365857, -15.65959907089493619 ) ) ;
#16711 = CARTESIAN_POINT ( 'NONE',  ( 199.1807827224510845, 281.9190771098037658, -16.60222886460724112 ) ) ;
#16712 = CARTESIAN_POINT ( 'NONE',  ( 25.26661199696083671, 36.36126292948895866, 6.180339887498949913 ) ) ;
#16713 = CARTESIAN_POINT ( 'NONE',  ( 172.0224699280288974, 275.0334117845947617, 16.95724843200788712 ) ) ;
#16714 = CARTESIAN_POINT ( 'NONE',  ( 163.3157238902107906, 283.7599821633143051, -3.437047550650083938 ) ) ;
#16715 = FACE_OUTER_BOUND ( 'NONE', #27527, .T. ) ;
#16716 = CARTESIAN_POINT ( 'NONE',  ( 192.0091641151854844, 261.6684110230355600, 3.065581067129474757 ) ) ;
#16717 = CARTESIAN_POINT ( 'NONE',  ( 186.5128128464827455, 296.3652354721813822, -8.829210103799347564 ) ) ;
#16718 = CARTESIAN_POINT ( 'NONE',  ( 4.614210867829412699, 161.2202760586659451, -5.415160957724236172E-17 ) ) ;
#16719 = CARTESIAN_POINT ( 'NONE',  ( 82.88857619529979104, 50.60347501890201016, 14.14623256037462795 ) ) ;
#16720 = ORIENTED_EDGE ( 'NONE', *, *, #12481, .F. ) ;
#16721 = EDGE_CURVE ( 'NONE', #7348, #56899, #5122, .T. ) ;
#16723 = CARTESIAN_POINT ( 'NONE',  ( 175.2285374422532414, 254.6787769949789322, 9.431799880968993577 ) ) ;
#16722 = VECTOR ( 'NONE', #65493, 1000.000000000000000 ) ;
#16724 = CARTESIAN_POINT ( 'NONE',  ( 203.5726949774746117, 269.0034548673361883, -6.096665150295551783 ) ) ;
#16725 = CARTESIAN_POINT ( 'NONE',  ( 81.83010596707761408, 41.21765235792337734, 5.778278449264639960 ) ) ;
#16726 = CARTESIAN_POINT ( 'NONE',  ( 27.18482440607883888, 180.3768266524160140, 9.188101187500096856 ) ) ;
#16727 = EDGE_CURVE ( 'NONE', #49424, #26012, #11819, .T. ) ;
#16728 = CARTESIAN_POINT ( 'NONE',  ( -11.40312891409031693, 78.77562236714182120, 59.99999999999999289 ) ) ;
#16729 = CARTESIAN_POINT ( 'NONE',  ( 25.64143417502910083, 37.73705186507756082, -3.090169943749475845 ) ) ;
#16730 = CARTESIAN_POINT ( 'NONE',  ( 85.14475835685283300, 42.48365458255290150, -1.347915880835522717 ) ) ;
#16731 = CARTESIAN_POINT ( 'NONE',  ( 146.8859094598974480, 276.2331372299326517, -0.7994986043261681496 ) ) ;
#16732 = CARTESIAN_POINT ( 'NONE',  ( 14.08707949041329144, 167.3932355074535394, -2.679491924311274254 ) ) ;
#16733 = B_SPLINE_SURFACE_WITH_KNOTS ( 'NONE', 3, 1, ( 
 ( #54997, #7923 ),
 ( #62088, #30717 ),
 ( #47399, #311 ),
 ( #78325, #61598 ),
 ( #39774, #91548 ),
 ( #77315, #84946 ),
 ( #53008, #83959 ),
 ( #45405, #76336 ),
 ( #6909, #37797 ),
 ( #38798, #92067 ),
 ( #92549, #7402 ),
 ( #15490, #46390 ),
 ( #69703, #31198 ),
 ( #16997, #73224 ),
 ( #49407, #71228 ),
 ( #94049, #18523 ),
 ( #9925, #63603 ),
 ( #40786, #78828 ),
 ( #32703, #65108 ),
 ( #47886, #57493 ),
 ( #86974, #48918 ),
 ( #1820, #86470 ),
 ( #80354, #25097 ),
 ( #94543, #56502 ),
 ( #19035, #3336 ),
 ( #56994, #2837 ),
 ( #32201, #72230 ),
 ( #95572, #26615 ),
 ( #26117, #49907 ),
 ( #34213, #55483 ),
 ( #87976, #2327 ),
 ( #88473, #9410 ),
 ( #55979, #17506 ),
 ( #48412, #95056 ) ),
 .UNSPECIFIED., .T., .F., .F.,
 ( 4, 2, 2, 2, 2, 2, 2, 2, 2, 2, 2, 2, 2, 2, 2, 2, 4 ),
 ( 2, 2 ),
 ( 0.000000000000000000, 0.06250000000000000000, 0.1250000000000000000, 0.1875000000000000000, 0.2500000000000000000, 0.3125000000000000000, 0.3750000000000000000, 0.4375000000000000000, 0.5000000000000000000, 0.5625000000000000000, 0.6250000000000000000, 0.6875000000000000000, 0.7500000000000000000, 0.8125000000000000000, 0.8750000000000000000, 0.9375000000000000000, 1.000000000000000000 ),
 ( 0.000000000000000000, 1.000000000000000000 ),
 .UNSPECIFIED. ) ;
#16734 = CARTESIAN_POINT ( 'NONE',  ( 186.9002619757878279, 295.9402723794265171, -7.697862465556936762 ) ) ;
#16735 = CARTESIAN_POINT ( 'NONE',  ( 73.16956295238907160, 57.33411781477383329, 16.38320611710937058 ) ) ;
#16736 = CARTESIAN_POINT ( 'NONE',  ( -35.89898968889473707, 24.97633462685642414, 177.5919119679930134 ) ) ;
#16738 =( BOUNDED_CURVE ( )  B_SPLINE_CURVE ( 2, ( #23305, #78536, #47110, #93764, #77010, #16218, #54194, #24322, #86181 ),
 .UNSPECIFIED., .F., .T. ) 
 B_SPLINE_CURVE_WITH_KNOTS ( ( 3, 2, 2, 2, 3 ),
 ( 0.8830645161290322509, 0.8844086021505376261, 0.8870967741935483764, 0.8897849462365591267, 0.8911290322580645018 ),
 .UNSPECIFIED. ) 
 CURVE ( )  GEOMETRIC_REPRESENTATION_ITEM ( )  RATIONAL_B_SPLINE_CURVE ( ( 0.9330127018922194093, 0.9330127018922194093, 1.000000000000000000, 0.8660254037844387076, 1.000000000000000000, 0.8660254037844387076, 1.000000000000000000, 0.9330127018922194093, 0.9330127018922194093 ) ) 
 REPRESENTATION_ITEM ( '' )  );
#16737 = CARTESIAN_POINT ( 'NONE',  ( 60.71607196274899110, 215.8615022471903160, 5.000000000000046185 ) ) ;
#16739 = CARTESIAN_POINT ( 'NONE',  ( 73.88098677858248209, 66.09861445257523371, -12.79634476329270498 ) ) ;
#16740 = CARTESIAN_POINT ( 'NONE',  ( 203.5026800799811895, 269.8567082039247111, 6.928182654214480429 ) ) ;
#16741 = CARTESIAN_POINT ( 'NONE',  ( 41.71789998727770410, 185.7048013555409796, 4.594050593750051981 ) ) ;
#16742 = LINE ( 'NONE', #35816, #79567 ) ;
#16743 = EDGE_CURVE ( 'NONE', #9173, #30330, #24735, .T. ) ;
#16744 = CARTESIAN_POINT ( 'NONE',  ( 204.5222561433589021, 270.7959794724876588, -6.481264364560415103 ) ) ;
#16745 = CARTESIAN_POINT ( 'NONE',  ( 175.8062715677771166, 253.2953273735088544, -6.838868645307838001 ) ) ;
#16746 = CARTESIAN_POINT ( 'NONE',  ( 67.06380573374150345, 66.82000881363511269, -8.954971976866424654 ) ) ;
#16747 = CARTESIAN_POINT ( 'NONE',  ( 6.060800048784472871, 162.7592609112380444, 2.679491924311254714 ) ) ;
#16748 = CARTESIAN_POINT ( 'NONE',  ( 202.8902555442842868, 278.4536566332962479, -15.11955846344091547 ) ) ;
#16749 = LINE ( 'NONE', #71968, #64998 ) ;
#16750 = CARTESIAN_POINT ( 'NONE',  ( 24.83671989960918935, 22.84335787977763488, 9.188101187500006262 ) ) ;
#16751 = CARTESIAN_POINT ( 'NONE',  ( 203.0535368433499457, 278.9479528611958585, 16.46202213522710167 ) ) ;
#16752 = CARTESIAN_POINT ( 'NONE',  ( 149.4171629335945681, 271.8488776066536730, -11.42564036194071520 ) ) ;
#16753 = CARTESIAN_POINT ( 'NONE',  ( 186.7162059521595836, 267.9499891762567358, -15.17631223955298303 ) ) ;
#16754 = VERTEX_POINT ( 'NONE', #31269 ) ;
#16755 = LINE ( 'NONE', #23345, #48437 ) ;
#16756 = CARTESIAN_POINT ( 'NONE',  ( 71.50396643458246615, 72.35543200887750004, -1.254608710098219060 ) ) ;
#16757 = ORIENTED_EDGE ( 'NONE', *, *, #42541, .T. ) ;
#16758 = CARTESIAN_POINT ( 'NONE',  ( 23.45662567177863167, 195.8967562850347122, -4.648177544792955347E-16 ) ) ;
#16759 = CARTESIAN_POINT ( 'NONE',  ( 69.36456772554703321, 70.60618739324945636, -1.417523587071017444 ) ) ;
#16760 = CARTESIAN_POINT ( 'NONE',  ( 190.7779368023172708, 300.2099158256590385, 8.142228434510803581 ) ) ;
#16761 = CARTESIAN_POINT ( 'NONE',  ( 178.8559941927174748, 256.9455126458981340, -7.290009489429222889 ) ) ;
#16762 = ORIENTED_EDGE ( 'NONE', *, *, #64850, .F. ) ;
#16763 = VERTEX_POINT ( 'NONE', #62155 ) ;
#16765 = CARTESIAN_POINT ( 'NONE',  ( 85.07154897650163150, 42.80747891370868530, -3.465323602608772369 ) ) ;
#16764 = DIRECTION ( 'NONE',  ( -0.8660254037844377084, -0.5000000000000014433, -0.000000000000000000 ) ) ;
#16766 = VERTEX_POINT ( 'NONE', #93102 ) ;
#16767 = CARTESIAN_POINT ( 'NONE',  ( 45.56060369728960069, 26.70852965304483106, 1.583844403245330712 ) ) ;
#16768 = CARTESIAN_POINT ( 'NONE',  ( 71.71105958810139214, 72.07721142573539908, -3.586786881503329472 ) ) ;
#16769 = DIRECTION ( 'NONE',  ( 0.000000000000000000, 0.000000000000000000, -1.000000000000000000 ) ) ;
#16770 = CARTESIAN_POINT ( 'NONE',  ( 2.966658798487924908, 25.21091486745858035, 1.000260061240931054E-15 ) ) ;
#16771 = CARTESIAN_POINT ( 'NONE',  ( 148.0389988358468827, 274.2359278451201590, 7.783622668412842671 ) ) ;
#16772 = CARTESIAN_POINT ( 'NONE',  ( 196.2421909983451940, 290.7455499326673021, -17.31908925000307065 ) ) ;
#16774 = AXIS2_PLACEMENT_3D ( 'NONE', #66345, #58723, #89698 ) ;
#16773 = CARTESIAN_POINT ( 'NONE',  ( 181.1477013271936016, 287.8971774238942203, -14.15342935774602218 ) ) ;
#16775 = VERTEX_POINT ( 'NONE', #58791 ) ;
#16776 = DIRECTION ( 'NONE',  ( 1.000000000000000000, 1.070572202317114942E-14, 0.000000000000000000 ) ) ;
#16777 = DIRECTION ( 'NONE',  ( -0.4851478631379979034, 0.8403007481384877631, 0.2419218955996582654 ) ) ;
#16778 = ORIENTED_EDGE ( 'NONE', *, *, #13820, .T. ) ;
#16779 = CARTESIAN_POINT ( 'NONE',  ( 32.62131273085646654, 21.76004757982090965, 5.678558825948272215 ) ) ;
#16780 = EDGE_CURVE ( 'NONE', #63237, #15171, #19450, .T. ) ;
#16781 = CARTESIAN_POINT ( 'NONE',  ( 198.2040940955416488, 287.3474340887963763, 16.95806375232200480 ) ) ;
#16782 = CARTESIAN_POINT ( 'NONE',  ( 72.44129552685039641, 70.67501955208014408, -7.848061272651214004 ) ) ;
#16783 = CARTESIAN_POINT ( 'NONE',  ( 56.60219097117523290, 212.6744531367911293, 4.594050593750047540 ) ) ;
#16784 = EDGE_LOOP ( 'NONE', ( #10998, #40926, #11071, #97205 ) ) ;
#16785 = CARTESIAN_POINT ( 'NONE',  ( 74.41008358870023187, 68.25813196090381041, 11.92500230979622522 ) ) ;
#16786 = CARTESIAN_POINT ( 'NONE',  ( 29.77967365985639248, 29.14441083166262203, 10.00000000000000533 ) ) ;
#16787 = CARTESIAN_POINT ( 'NONE',  ( 197.9637121306999461, 287.7637878651254937, 17.83088679657193865 ) ) ;
#16788 = CARTESIAN_POINT ( 'NONE',  ( 176.3169295130042258, 273.0865261982322636, 16.85758906909942567 ) ) ;
#16789 = ORIENTED_EDGE ( 'NONE', *, *, #82260, .F. ) ;
#16790 = AXIS2_PLACEMENT_3D ( 'NONE', #72998, #57258, #34955 ) ;
#16791 = CARTESIAN_POINT ( 'NONE',  ( 190.5346086712997078, 299.7911943260875205, 5.206985090025521679 ) ) ;
#16792 = VECTOR ( 'NONE', #27204, 1000.000000000000000 ) ;
#16793 = LINE ( 'NONE', #77618, #70382 ) ;
#16794 = CARTESIAN_POINT ( 'NONE',  ( 78.63295798250021562, 57.35503737189328177, 16.60795452140541784 ) ) ;
#16795 = ORIENTED_EDGE ( 'NONE', *, *, #97129, .F. ) ;
#16796 = CARTESIAN_POINT ( 'NONE',  ( 110.0998739067015606, 222.8262482093458061, 3.021315404115420679E-15 ) ) ;
#16797 = CARTESIAN_POINT ( 'NONE',  ( 175.6063544791335573, 254.0105997054014040, 8.344378697908656051 ) ) ;
#16798 = CARTESIAN_POINT ( 'NONE',  ( 161.4816992964961742, 250.9524876563463067, -12.92750327687364198 ) ) ;
#16799 = ADVANCED_FACE ( 'NONE', ( #48987 ), #24671, .T. ) ;
#16800 = CARTESIAN_POINT ( 'NONE',  ( 147.1603453755519695, 275.7578002805973370, -5.230822882238410187 ) ) ;
#16801 = CARTESIAN_POINT ( 'NONE',  ( 190.8153366230912411, 300.1451374358846920, 3.771947273125533684 ) ) ;
#16802 = CARTESIAN_POINT ( 'NONE',  ( 180.5734370714514228, 271.1176088554109356, 17.19503379674203103 ) ) ;
#16803 = CARTESIAN_POINT ( 'NONE',  ( 164.3493441216711517, 245.9855811210807417, 1.722120810491653664 ) ) ;
#16804 = CARTESIAN_POINT ( 'NONE',  ( 76.05941642030330740, 65.49204198467158733, 13.96074477642770084 ) ) ;
#16805 = CARTESIAN_POINT ( 'NONE',  ( 154.8782533782051871, 264.3899914918594050, -17.45241046926759765 ) ) ;
#16806 = CARTESIAN_POINT ( 'NONE',  ( -22.42236680055709641, 157.8615022471902591, 0.000000000000000000 ) ) ;
#16807 = CARTESIAN_POINT ( 'NONE',  ( 117.3868696429430258, 229.3923013555409796, 4.594050593750050204 ) ) ;
#16808 = ORIENTED_EDGE ( 'NONE', *, *, #88403, .T. ) ;
#16809 = CARTESIAN_POINT ( 'NONE',  ( 191.3610003135137276, 299.2000202002271294, -9.855749861282104618 ) ) ;
#16810 = CARTESIAN_POINT ( 'NONE',  ( 70.32594426133741194, 65.43690866019677799, 11.69452207246081876 ) ) ;
#16811 = CARTESIAN_POINT ( 'NONE',  ( 202.8151641853381477, 279.3608264160075692, -16.28741359973609448 ) ) ;
#16812 = CARTESIAN_POINT ( 'NONE',  ( 204.2133777088835700, 276.9390495533970693, 13.75768580338462144 ) ) ;
#16813 = CARTESIAN_POINT ( 'NONE',  ( 83.80447776121599190, 52.10292630681441040, -14.99896445683751622 ) ) ;
#16814 = CARTESIAN_POINT ( 'NONE',  ( 174.8285612161963058, 252.5975812908445732, 5.144082065870574816 ) ) ;
#16815 = ORIENTED_EDGE ( 'NONE', *, *, #57491, .F. ) ;
#16816 = CARTESIAN_POINT ( 'NONE',  ( 163.3939361803663246, 247.6403962173759226, -10.78041711314006790 ) ) ;
#16817 = CARTESIAN_POINT ( 'NONE',  ( 82.93853206040887471, 44.70350428498475281, -9.452842870200390379 ) ) ;
#16818 = CARTESIAN_POINT ( 'NONE',  ( 24.59328401069779346, 196.5530062829863311, -4.648177544792955347E-16 ) ) ;
#16819 = CARTESIAN_POINT ( 'NONE',  ( 206.2536424468873406, 272.9128265684719281, 8.671401193505188232 ) ) ;
#16820 = CARTESIAN_POINT ( 'NONE',  ( 136.3040252829181327, 243.3768266524160140, 9.188101187500096856 ) ) ;
#16821 = CARTESIAN_POINT ( 'NONE',  ( 198.5970767652345899, 286.6667681383942181, -17.17073100918929640 ) ) ;
#16822 = CARTESIAN_POINT ( 'NONE',  ( 185.3345560757713315, 297.6803563334680689, 4.160651365811766311 ) ) ;
#16823 = CARTESIAN_POINT ( 'NONE',  ( 187.4269513160483314, 281.3598214497520189, -17.37670249948783763 ) ) ;
#16824 = CARTESIAN_POINT ( 'NONE',  ( -19.65312891409030271, 93.06504152958497400, -25.00000000000000000 ) ) ;
#16825 = CARTESIAN_POINT ( 'NONE',  ( 55.49285624440017273, 202.8458772461660260, 9.188101187500095079 ) ) ;
#16826 = CARTESIAN_POINT ( 'NONE',  ( 78.02123370085931242, 59.86933949065961968, -16.42544237888153447 ) ) ;
#16827 = ORIENTED_EDGE ( 'NONE', *, *, #60630, .F. ) ;
#16828 = CARTESIAN_POINT ( 'NONE',  ( 72.21531847787744596, 67.13642658987301104, 11.23760059196915861 ) ) ;
#16829 = CARTESIAN_POINT ( 'NONE',  ( 181.8509774751104544, 266.9677320091309412, 16.09658033613713712 ) ) ;
#16830 = B_SPLINE_CURVE_WITH_KNOTS ( 'NONE', 3,
 ( #44546, #98287, #35960, #29373, #36958, #75995, #30361 ),
 .UNSPECIFIED., .F., .F.,
 ( 4, 3, 4 ),
 ( 0.000000000000000000, 0.001498044977020785264, 0.001890351849317388738 ),
 .UNSPECIFIED. ) ;
#16831 = CARTESIAN_POINT ( 'NONE',  ( 70.03535249260973217, 70.71478112856975429, -3.280756518793910281 ) ) ;
#16832 = PLANE ( 'NONE',  #67763 ) ;
#16833 = CARTESIAN_POINT ( 'NONE',  ( 151.3082152111609844, 278.3337183599618356, -1.667790407313227918 ) ) ;
#16834 = CARTESIAN_POINT ( 'NONE',  ( 105.0000000000000000, 10.00000000000003197, 14.21260523776213347 ) ) ;
#16835 = CARTESIAN_POINT ( 'NONE',  ( 178.8406662910292084, 261.3676314715743274, 12.21613212044301022 ) ) ;
#16836 = CARTESIAN_POINT ( 'NONE',  ( 114.7524487161675779, 250.3927522451419634, 2.944929066748280225E-16 ) ) ;
#16837 = CARTESIAN_POINT ( 'NONE',  ( 3.562051267137642085, 25.55466486950697558, -1.111400068045478839E-16 ) ) ;
#16838 = VERTEX_POINT ( 'NONE', #2396 ) ;
#16839 = CARTESIAN_POINT ( 'NONE',  ( 163.1014434023538513, 248.1470085697407058, 9.692260209037655727 ) ) ;
#16840 = DIRECTION ( 'NONE',  ( 0.3002896333693371722, 0.9538480676139722281, 0.000000000000000000 ) ) ;
#16841 = EDGE_CURVE ( 'NONE', #54426, #49659, #63566, .T. ) ;
#16842 = CARTESIAN_POINT ( 'NONE',  ( 24.91150772114469092, 179.0643266524160140, 9.188101187500095079 ) ) ;
#16843 = CARTESIAN_POINT ( 'NONE',  ( 17.73189607522619937, 18.43677371833801359, -10.00000000000000355 ) ) ;
#16844 = CARTESIAN_POINT ( 'NONE',  ( 188.7579712926501543, 290.5937008958214847, -14.99838659903155325 ) ) ;
#16845 = DIRECTION ( 'NONE',  ( 1.000000000000000000, 0.000000000000000000, 0.000000000000000000 ) ) ;
#16846 = CARTESIAN_POINT ( 'NONE',  ( 72.14138414250713538, 72.07495387501906237, 2.939176625790155928 ) ) ;
#16848 = CARTESIAN_POINT ( 'NONE',  ( 51.02741275436266477, 210.2677522451419350, -5.000000000000047962 ) ) ;
#16847 = CARTESIAN_POINT ( 'NONE',  ( 12.65163835348095489, 7.708529653044779550, 1.583844403245363130 ) ) ;
#16849 = EDGE_CURVE ( 'NONE', #95819, #95312, #17859, .T. ) ;
#16850 = CARTESIAN_POINT ( 'NONE',  ( 173.2055275001436314, 289.0856056677645824, 8.083435772122928853 ) ) ;
#16851 = CARTESIAN_POINT ( 'NONE',  ( 163.2029997909485814, 256.0468373663799753, -14.94059154133669587 ) ) ;
#16852 = CARTESIAN_POINT ( 'NONE',  ( 204.6149525604204769, 276.2435015074934199, -13.22810747389629960 ) ) ;
#16853 = CARTESIAN_POINT ( 'NONE',  ( 162.2496630651073701, 251.8436134512154183, -12.97535039530458967 ) ) ;
#16854 = EDGE_LOOP ( 'NONE', ( #33876, #12083, #6958, #73122 ) ) ;
#16855 = VECTOR ( 'NONE', #32280, 1000.000000000000114 ) ;
#16856 = CARTESIAN_POINT ( 'NONE',  ( 161.8567175149206321, 267.2024831904969346, 16.48631320651076848 ) ) ;
#16857 = CARTESIAN_POINT ( 'NONE',  ( 21.74492879244924382, 193.3615022471903160, 5.000000000000046185 ) ) ;
#16858 = DIRECTION ( 'NONE',  ( 0.8660254037844395958, 0.4999999999999985567, 0.000000000000000000 ) ) ;
#16859 = CARTESIAN_POINT ( 'NONE',  ( 202.2603678735342214, 280.3217618159037556, 16.49712126737133744 ) ) ;
#16860 = CARTESIAN_POINT ( 'NONE',  ( -6.590166341514275494, 160.8768266524160140, 9.188101187500098632 ) ) ;
#16861 = CARTESIAN_POINT ( 'NONE',  ( 27.35361640444819287, 37.83396525600391413, -2.839279412974133887 ) ) ;
#16864 = ADVANCED_FACE ( 'NONE', ( #87558 ), #71296, .T. ) ;
#16863 = CARTESIAN_POINT ( 'NONE',  ( 200.2141246490667754, 282.1197396120186909, 17.30140834831486529 ) ) ;
#16862 = CARTESIAN_POINT ( 'NONE',  ( 164.5093404746413910, 259.6730185065525802, -16.72720059574769991 ) ) ;
#16865 = CARTESIAN_POINT ( 'NONE',  ( 185.5400204171384075, 259.9029772015394428, 7.379271805359726599 ) ) ;
#16866 = CARTESIAN_POINT ( 'NONE',  ( 206.4537138826727301, 273.0586734743599209, 11.45643784582899016 ) ) ;
#16867 = AXIS2_PLACEMENT_3D ( 'NONE', #93693, #24256, #55133 ) ;
#16868 = CARTESIAN_POINT ( 'NONE',  ( 186.6238840102718086, 259.3006934494294455, -2.364174896264719994 ) ) ;
#16869 = CARTESIAN_POINT ( 'NONE',  ( 65.82177962144463379, 68.97126114446055567, 2.130094581049046365 ) ) ;
#16870 = VERTEX_POINT ( 'NONE', #40358 ) ;
#16871 = LINE ( 'NONE', #40156, #51977 ) ;
#16872 = CARTESIAN_POINT ( 'NONE',  ( 179.8194114752668042, 286.2860187198718904, 13.09292147992676902 ) ) ;
#16873 = CARTESIAN_POINT ( 'NONE',  ( 154.6671547551263757, 278.4911608342019349, -5.208367705655446045 ) ) ;
#16874 = CARTESIAN_POINT ( 'NONE',  ( 12.50787272796288896, 10.14754757982088051, -5.678558825948275768 ) ) ;
#16875 = CARTESIAN_POINT ( 'NONE',  ( 207.2585079244812221, 271.6647293043187688, 8.480643094032153328 ) ) ;
#16876 = CARTESIAN_POINT ( 'NONE',  ( 206.4484807199597753, 273.0677375780628608, -9.220527398138528952 ) ) ;
#16877 = EDGE_CURVE ( 'NONE', #88681, #33594, #1888, .T. ) ;
#16878 = DIRECTION ( 'NONE',  ( -0.000000000000000000, 0.000000000000000000, -1.000000000000000000 ) ) ;
#16879 = CARTESIAN_POINT ( 'NONE',  ( 80.61430232155159104, 228.8967562850347122, -4.648177544792955347E-16 ) ) ;
#16880 = CARTESIAN_POINT ( 'NONE',  ( 191.4732661803433018, 298.1837965232045349, 9.193897954715051668 ) ) ;
#16881 = CARTESIAN_POINT ( 'NONE',  ( 207.9743173328493526, 270.4249110404894054, -2.481515874287090639 ) ) ;
#16882 = CARTESIAN_POINT ( 'NONE',  ( 154.9455285025717615, 262.2734675583710100, 18.28470720339922551 ) ) ;
#16883 = VERTEX_POINT ( 'NONE', #33276 ) ;
#16884 = ORIENTED_EDGE ( 'NONE', *, *, #66791, .T. ) ;
#16885 = DIRECTION ( 'NONE',  ( -0.8660254037844359321, -0.5000000000000051070, -0.000000000000000000 ) ) ;
#16886 = CARTESIAN_POINT ( 'NONE',  ( 89.54518929453067244, 234.0530062829863027, -4.648177544792955347E-16 ) ) ;
#16887 = ORIENTED_EDGE ( 'NONE', *, *, #86343, .T. ) ;
#16888 = CARTESIAN_POINT ( 'NONE',  ( 188.8891845508813390, 297.3683201713357107, 7.792454418634450874 ) ) ;
#16889 = EDGE_LOOP ( 'NONE', ( #45028, #39770, #78188, #29137 ) ) ;
#16890 = DIRECTION ( 'NONE',  ( 0.4999999999999992784, -0.8660254037844390407, 0.000000000000000000 ) ) ;
#16891 = CARTESIAN_POINT ( 'NONE',  ( 79.01889296114715933, 59.41967273037257513, -16.52995258344894580 ) ) ;
#16892 = CARTESIAN_POINT ( 'NONE',  ( 11.80767242186427879, 30.53330575246453904, 10.00000000000000000 ) ) ;
#16893 = ORIENTED_EDGE ( 'NONE', *, *, #6915, .T. ) ;
#16894 = CARTESIAN_POINT ( 'NONE',  ( 200.4592688079413847, 283.4413569069752725, 18.39277739746426832 ) ) ;
#16895 = DIRECTION ( 'NONE',  ( -0.001635407438350354676, -0.9999986627203610867, 0.000000000000000000 ) ) ;
#16896 = CARTESIAN_POINT ( 'NONE',  ( 191.4484954869714954, 299.0484741143815199, 8.684991747358081327 ) ) ;
#16897 = CARTESIAN_POINT ( 'NONE',  ( 149.4284094220488157, 274.0275188989749040, -8.736341709343308892 ) ) ;
#16898 = ORIENTED_EDGE ( 'NONE', *, *, #80886, .F. ) ;
#16899 = EDGE_CURVE ( 'NONE', #65652, #62907, #86335, .T. ) ;
#16900 = EDGE_CURVE ( 'NONE', #31576, #64281, #48485, .T. ) ;
#16901 = CARTESIAN_POINT ( 'NONE',  ( 170.6773407966179263, 255.4795565429710678, -11.51496627275842144 ) ) ;
#16902 = VERTEX_POINT ( 'NONE', #79426 ) ;
#16903 = ORIENTED_EDGE ( 'NONE', *, *, #26150, .F. ) ;
#16904 = CARTESIAN_POINT ( 'NONE',  ( 73.05277295987646369, 59.90981557475946317, 15.36185477374104025 ) ) ;
#16905 = ORIENTED_EDGE ( 'NONE', *, *, #6844, .T. ) ;
#16906 = CARTESIAN_POINT ( 'NONE',  ( 149.4596969528118393, 273.7752065243203106, 10.43958276706939614 ) ) ;
#16907 = ORIENTED_EDGE ( 'NONE', *, *, #97400, .T. ) ;
#16908 = EDGE_CURVE ( 'NONE', #6038, #8322, #9992, .T. ) ;
#16909 = CARTESIAN_POINT ( 'NONE',  ( 81.89930626873778863, 42.21375885382296644, 7.647715624843494098 ) ) ;
#16910 = CARTESIAN_POINT ( 'NONE',  ( 168.8745654493266102, 272.6928345997080783, 16.05439322531100999 ) ) ;
#16911 = CARTESIAN_POINT ( 'NONE',  ( 164.4068639292406715, 270.3611440525622811, 17.36650109901806971 ) ) ;
#16912 = CARTESIAN_POINT ( 'NONE',  ( 194.5252985417586729, 293.7192948986070178, -14.54632727629426370 ) ) ;
#16913 = CARTESIAN_POINT ( 'NONE',  ( 82.59012279121988342, 53.49374897786832150, -15.73261944071848895 ) ) ;
#16914 = EDGE_CURVE ( 'NONE', #79192, #13224, #16581, .T. ) ;
#16915 = CARTESIAN_POINT ( 'NONE',  ( 197.7164576114591341, 288.1920452548512230, -17.18932158603989180 ) ) ;
#16917 = CARTESIAN_POINT ( 'NONE',  ( 166.8603047740130876, 247.0964243085869896, 1.925065518075911530 ) ) ;
#16916 = B_SPLINE_CURVE_WITH_KNOTS ( 'NONE', 3,
 ( #8036, #32318, #63219, #38407 ),
 .UNSPECIFIED., .F., .F.,
 ( 4, 4 ),
 ( 0.01205678105519798413, 0.01821341545976904938 ),
 .UNSPECIFIED. ) ;
#16918 = CARTESIAN_POINT ( 'NONE',  ( 22.66683848874176022, 18.80170272979926693, 7.433330006724137462 ) ) ;
#16919 = CARTESIAN_POINT ( 'NONE',  ( 164.7297297678022403, 245.3267338555121455, 3.020078936458732599 ) ) ;
#16921 = ORIENTED_EDGE ( 'NONE', *, *, #69116, .F. ) ;
#16920 = CARTESIAN_POINT ( 'NONE',  ( 197.8977219949227049, 287.8780861330898801, 17.48564646125164046 ) ) ;
#16922 = ADVANCED_FACE ( 'NONE', ( #20093 ), #50467, .F. ) ;
#16923 = CARTESIAN_POINT ( 'NONE',  ( 35.03822396736671152, 49.37458582131907292, 10.00000000000000000 ) ) ;
#16924 = EDGE_CURVE ( 'NONE', #80622, #74751, #70959, .T. ) ;
#16925 = CARTESIAN_POINT ( 'NONE',  ( 206.7680519836501958, 272.5142239127119979, -10.57935479673322021 ) ) ;
#16926 = CARTESIAN_POINT ( 'NONE',  ( 48.61286661847091040, 84.94359857078811160, -10.00000000000000000 ) ) ;
#16927 = VECTOR ( 'NONE', #23898, 1000.000000000000227 ) ;
#16928 = FACE_OUTER_BOUND ( 'NONE', #74031, .T. ) ;
#16929 = CARTESIAN_POINT ( 'NONE',  ( 190.9750074087093026, 262.0973604801322381, -0.7408433392359728975 ) ) ;
#16930 = EDGE_LOOP ( 'NONE', ( #83711, #76580, #66767, #78715 ) ) ;
#16931 = CARTESIAN_POINT ( 'NONE',  ( 3.076650163567010932, 38.97070005862290287, 59.99999999999999289 ) ) ;
#16932 = CARTESIAN_POINT ( 'NONE',  ( 74.76064909570828831, 66.79516745633125652, -13.17056974000816005 ) ) ;
#16933 = CARTESIAN_POINT ( 'NONE',  ( 207.6007741873543750, 271.0719067473055475, 7.587922723682903658 ) ) ;
#16934 = CARTESIAN_POINT ( 'NONE',  ( 13.28313890609088688, 185.1427522451419350, -10.00000000000009415 ) ) ;
#16935 = CARTESIAN_POINT ( 'NONE',  ( 86.66977078063996487, 220.8458772461660544, 9.188101187500095079 ) ) ;
#16936 = VECTOR ( 'NONE', #67498, 1000.000000000000114 ) ;
#16937 = CARTESIAN_POINT ( 'NONE',  ( 82.18541192110650684, 40.82295230248577411, -1.158419095661346487 ) ) ;
#16938 = CARTESIAN_POINT ( 'NONE',  ( 6.981765372403105907, 27.52903772873354882, -1.583844403245363575 ) ) ;
#16939 = CARTESIAN_POINT ( 'NONE',  ( 167.0011108565465747, 278.0668406281866396, -14.45516252385082900 ) ) ;
#16941 = CARTESIAN_POINT ( 'NONE',  ( 75.92188977558036811, 65.58667241883225074, 13.87414006683291134 ) ) ;
#16940 = CARTESIAN_POINT ( 'NONE',  ( 2.232293911657190488, 172.0958772461660544, -9.188101187500095079 ) ) ;
#16942 = CARTESIAN_POINT ( 'NONE',  ( 161.1238074876215478, 251.5723744529297505, 13.42537408252843179 ) ) ;
#16943 = ORIENTED_EDGE ( 'NONE', *, *, #78097, .F. ) ;
#16945 = VERTEX_POINT ( 'NONE', #66668 ) ;
#16944 = UNCERTAINTY_MEASURE_WITH_UNIT (LENGTH_MEASURE( 1.000000000000000082E-05 ), #67455, 'distance_accuracy_value', 'NONE');
#16946 = CARTESIAN_POINT ( 'NONE',  ( 198.1198657144259982, 265.9800056028663562, -2.879908836942639105 ) ) ;
#16947 = CARTESIAN_POINT ( 'NONE',  ( 68.08257952738715346, 69.66255777483917200, 2.615794919781196715 ) ) ;
#16948 = CARTESIAN_POINT ( 'NONE',  ( 33.84893051719189572, 201.8967562850347122, -4.648177544792955347E-16 ) ) ;
#16949 = CARTESIAN_POINT ( 'NONE',  ( 156.6543370668840680, 266.2741171134555316, 17.28817642186849213 ) ) ;
#16950 = CARTESIAN_POINT ( 'NONE',  ( 167.3110317288038686, 250.1317611871268696, 9.699734311170200129 ) ) ;
#16951 = CARTESIAN_POINT ( 'NONE',  ( 33.21950506899538880, 199.1744531367911293, 4.594050593750047540 ) ) ;
#16952 = CARTESIAN_POINT ( 'NONE',  ( 199.8327978920034411, 276.9379622803334087, 15.19750203934660249 ) ) ;
#16953 = ORIENTED_EDGE ( 'NONE', *, *, #20309, .T. ) ;
#16954 = FACE_OUTER_BOUND ( 'NONE', #11675, .T. ) ;
#16955 = CARTESIAN_POINT ( 'NONE',  ( 175.2786348600535860, 281.1565833761089266, -15.16109458501749607 ) ) ;
#16957 = EDGE_CURVE ( 'NONE', #7306, #39570, #6883, .T. ) ;
#16956 = VECTOR ( 'NONE', #22223, 1000.000000000000114 ) ;
#16958 = CARTESIAN_POINT ( 'NONE',  ( -13.03140383004354241, 163.2833772461660544, -9.188101187500095079 ) ) ;
#16959 = CARTESIAN_POINT ( 'NONE',  ( 80.62770670945103291, 57.26257946240811236, -16.23162490972527294 ) ) ;
#16960 = CARTESIAN_POINT ( 'NONE',  ( 154.9683083969241011, 262.2340116239618055, 18.33261662430134109 ) ) ;
#16961 = CARTESIAN_POINT ( 'NONE',  ( 198.7829547491859330, 286.3448180261817129, -18.59838968157616179 ) ) ;
#16962 = CYLINDRICAL_SURFACE ( 'NONE', #72682, 17.82106496071139645 ) ;
#16963 = CARTESIAN_POINT ( 'NONE',  ( 147.8308140999695866, 274.5965143850199865, -7.866624397492971710 ) ) ;
#16964 = EDGE_CURVE ( 'NONE', #61138, #62301, #30228, .T. ) ;
#16965 = CARTESIAN_POINT ( 'NONE',  ( 192.5271661211833703, 265.1515744257078495, 7.739560070318121987 ) ) ;
#16966 = CARTESIAN_POINT ( 'NONE',  ( 163.7010375032499212, 247.1084811230698506, 6.649922295230481950 ) ) ;
#16967 = CARTESIAN_POINT ( 'NONE',  ( -19.42194755839791753, 24.31068691715150010, -10.00000000000000000 ) ) ;
#16968 = CARTESIAN_POINT ( 'NONE',  ( 191.1687199697037443, 299.5330595250031820, -8.491751560014430211 ) ) ;
#16969 = CARTESIAN_POINT ( 'NONE',  ( 190.6084209867335915, 300.5035258309363826, -0.5505750481748228342 ) ) ;
#16970 = ORIENTED_EDGE ( 'NONE', *, *, #27535, .F. ) ;
#16971 = CARTESIAN_POINT ( 'NONE',  ( 152.5423653171682474, 268.4358682943698682, -15.78187745328793490 ) ) ;
#16972 = LINE ( 'NONE', #9387, #70836 ) ;
#16973 = CARTESIAN_POINT ( 'NONE',  ( 108.5372593219620683, 221.2202760586659167, -5.415160957724236172E-17 ) ) ;
#16974 = CARTESIAN_POINT ( 'NONE',  ( 12.04840505635704417, 25.14336893147754282, 7.433330006724141015 ) ) ;
#16976 = EDGE_CURVE ( 'NONE', #37468, #28879, #60795, .T. ) ;
#16975 = DIRECTION ( 'NONE',  ( -0.2033683215378938036, 0.3522442655536374700, -0.9135454576426059736 ) ) ;
#16978 = CARTESIAN_POINT ( 'NONE',  ( 191.5612668698545633, 276.9093416755657699, 16.88675210317316910 ) ) ;
#16977 = DIRECTION ( 'NONE',  ( 1.000000000000000000, 0.000000000000000000, 0.000000000000000000 ) ) ;
#16979 = CARTESIAN_POINT ( 'NONE',  ( 191.3465768251321890, 299.2250024149264505, -6.938973362607056217 ) ) ;
#16980 = B_SPLINE_CURVE_WITH_KNOTS ( 'NONE', 3,
 ( #75879, #6457, #66261, #58635 ),
 .UNSPECIFIED., .F., .F.,
 ( 4, 4 ),
 ( 0.01344258228325481003, 0.02205949149894677330 ),
 .UNSPECIFIED. ) ;
#16981 = CARTESIAN_POINT ( 'NONE',  ( 22.68382546022871438, 31.83478043621389020, -8.090169943749479842 ) ) ;
#16982 = CARTESIAN_POINT ( 'NONE',  ( 149.2923684163597784, 272.0650280510108701, -12.99082738998495756 ) ) ;
#16983 = CARTESIAN_POINT ( 'NONE',  ( 83.16056367749568778, 225.4865022471902876, 10.00000000000009415 ) ) ;
#16984 = CARTESIAN_POINT ( 'NONE',  ( 173.1636647817533685, 289.7167559925995874, -1.225364899902585902 ) ) ;
#16985 = DIRECTION ( 'NONE',  ( -0.7510153523339117010, 0.6602847420308685100, 0.000000000000000000 ) ) ;
#16986 = ORIENTED_EDGE ( 'NONE', *, *, #60227, .F. ) ;
#16987 = CARTESIAN_POINT ( 'NONE',  ( 130.9983832723993089, 257.9860189848785694, -2.679491924311252493 ) ) ;
#16988 = CARTESIAN_POINT ( 'NONE',  ( 175.8776426353156523, 278.6924052921702923, 15.46313303699034059 ) ) ;
#16989 = CARTESIAN_POINT ( 'NONE',  ( -13.11024591527734451, 4.999999999999999112, 48.00000000000000000 ) ) ;
#16991 = VERTEX_POINT ( 'NONE', #99083 ) ;
#16990 = ADVANCED_FACE ( 'NONE', ( #6374 ), #68156, .F. ) ;
#16992 = EDGE_CURVE ( 'NONE', #42801, #100197, #5626, .T. ) ;
#16993 = CARTESIAN_POINT ( 'NONE',  ( 86.01243404335103548, 46.72055381764010917, 10.47010224649849164 ) ) ;
#16994 = VECTOR ( 'NONE', #58615, 1000.000000000000114 ) ;
#16995 = FACE_OUTER_BOUND ( 'NONE', #48074, .T. ) ;
#16996 = CARTESIAN_POINT ( 'NONE',  ( 194.3094773688834778, 284.8302703302293253, 17.74979085435418469 ) ) ;
#16997 = CARTESIAN_POINT ( 'NONE',  ( 192.5254593562406171, 297.1831179748913314, 11.00703791256144015 ) ) ;
#16998 = ORIENTED_EDGE ( 'NONE', *, *, #50830, .F. ) ;
#16999 = CARTESIAN_POINT ( 'NONE',  ( 191.2585535523842850, 280.2024068932645378, 17.45594619081192889 ) ) ;
#17000 = B_SPLINE_SURFACE_WITH_KNOTS ( 'NONE', 3, 1, ( 
 ( #19848, #57324 ),
 ( #58319, #88800 ),
 ( #74557, #97846 ),
 ( #58805, #43616 ),
 ( #97356, #64943 ),
 ( #11748, #11261 ),
 ( #66916, #82179 ),
 ( #50226, #20848 ),
 ( #81670, #42124 ),
 ( #4633, #89294 ),
 ( #50716, #81181 ),
 ( #5133, #66428 ),
 ( #27922, #36015 ),
 ( #95888, #51739 ),
 ( #28415, #27445 ),
 ( #96371, #89769 ),
 ( #42611, #73542 ),
 ( #10746, #59295 ),
 ( #65921, #26449 ),
 ( #41622, #35019 ),
 ( #88296, #3168 ),
 ( #12243, #43102 ),
 ( #72564, #74045 ),
 ( #18852, #73055 ),
 ( #49733, #80686 ),
 ( #35528, #20340 ),
 ( #34530, #65430 ),
 ( #51212, #90276 ),
 ( #26937, #91255 ),
 ( #83158, #68412 ),
 ( #59810, #84654 ),
 ( #98343, #99339 ),
 ( #23303, #67415 ),
 ( #13248, #44105 ) ),
 .UNSPECIFIED., .T., .F., .F.,
 ( 4, 2, 2, 2, 2, 2, 2, 2, 2, 2, 2, 2, 2, 2, 2, 2, 4 ),
 ( 2, 2 ),
 ( 0.000000000000000000, 0.06250000000000000000, 0.1250000000000000000, 0.1875000000000000000, 0.2500000000000000000, 0.3125000000000000000, 0.3750000000000000000, 0.4375000000000000000, 0.5000000000000000000, 0.5625000000000000000, 0.6250000000000000000, 0.6875000000000000000, 0.7500000000000000000, 0.8125000000000000000, 0.8750000000000000000, 0.9375000000000000000, 1.000000000000000000 ),
 ( 0.000000000000000000, 1.000000000000000000 ),
 .UNSPECIFIED. ) ;
#17001 = CARTESIAN_POINT ( 'NONE',  ( 32.50825522076439000, 36.95586893147758190, 7.433330006724141015 ) ) ;
#17002 = CARTESIAN_POINT ( 'NONE',  ( 176.7804342879712465, 274.6069073446109883, -17.51127113154074522 ) ) ;
#17003 = EDGE_LOOP ( 'NONE', ( #92932, #10575, #50033, #51049 ) ) ;
#17004 = CARTESIAN_POINT ( 'NONE',  ( 167.6448875122848108, 280.9501575304901735, 11.66831761562362857 ) ) ;
#17005 = CARTESIAN_POINT ( 'NONE',  ( 147.9133274879049793, 274.4535970048112290, -9.359166267164972908 ) ) ;
#17006 = CARTESIAN_POINT ( 'NONE',  ( 80.20857538925844210, 44.21345027839176112, -11.30608575764589752 ) ) ;
#17007 = ORIENTED_EDGE ( 'NONE', *, *, #90170, .T. ) ;
#17008 = CARTESIAN_POINT ( 'NONE',  ( 86.15665200708443194, 46.94614013873178493, -10.61509939557873139 ) ) ;
#17009 = CARTESIAN_POINT ( 'NONE',  ( 44.95821123098110661, 116.5722627105190270, 10.00000000000000000 ) ) ;
#17010 = CARTESIAN_POINT ( 'NONE',  ( 71.37900974329706116, 202.0177522451417929, 5.000000000000051514 ) ) ;
#17011 = CARTESIAN_POINT ( 'NONE',  ( 86.31635269648819531, 44.43553455137352870, -7.074382444400770353 ) ) ;
#17012 = CARTESIAN_POINT ( 'NONE',  ( -30.18034446749236821, 25.12100238203590763, 10.00000000000000000 ) ) ;
#17013 = CARTESIAN_POINT ( 'NONE',  ( 40.57792791151964451, 35.37878583063844218, 9.188101187500006262 ) ) ;
#17014 = CARTESIAN_POINT ( 'NONE',  ( 155.5587153255869453, 261.2113968263770971, -18.30500480654006878 ) ) ;
#17015 = VERTEX_POINT ( 'NONE', #22059 ) ;
#17016 = ORIENTED_EDGE ( 'NONE', *, *, #4821, .F. ) ;
#17017 = B_SPLINE_CURVE_WITH_KNOTS ( 'NONE', 3,
 ( #58107, #50498, #1924, #25208, #40395, #25731, #94653, #18121, #95674, #49023, #79956, #10524, #41399, #2948, #18630, #20124 ),
 .UNSPECIFIED., .F., .F.,
 ( 4, 1, 2, 2, 2, 1, 2, 2, 4 ),
 ( 0.000000000000000000, 0.1249999999999992506, 0.1874999999999986122, 0.2499999999999979461, 0.4999999999999965028, 0.6249999999999962252, 0.6874999999999970024, 0.7499999999999976685, 1.000000000000000000 ),
 .UNSPECIFIED. ) ;
#17018 = CARTESIAN_POINT ( 'NONE',  ( 95.62772104926125394, 236.0177522451419350, 5.000000000000046185 ) ) ;
#17019 = ORIENTED_EDGE ( 'NONE', *, *, #21292, .F. ) ;
#17020 = CARTESIAN_POINT ( 'NONE',  ( 77.18032279635316684, 49.61715883235847002, -14.98457440409997332 ) ) ;
#17021 = ORIENTED_EDGE ( 'NONE', *, *, #64757, .T. ) ;
#17022 = CARTESIAN_POINT ( 'NONE',  ( 30.62489312496363425, 46.16797101519271962, -10.00000000000000000 ) ) ;
#17023 = CARTESIAN_POINT ( 'NONE',  ( 203.3349860717029571, 278.4604684979374838, -16.59553970625579566 ) ) ;
#17025 = VERTEX_POINT ( 'NONE', #29178 ) ;
#17024 =( BOUNDED_CURVE ( )  B_SPLINE_CURVE ( 2, ( #21376, #75581, #31948, #25764, #95192, #85728, #57127, #78075, #39039, #8661, #65727, #10554, #41429 ),
 .UNSPECIFIED., .F., .T. ) 
 B_SPLINE_CURVE_WITH_KNOTS ( ( 3, 2, 2, 2, 2, 2, 3 ),
 ( 0.9625000000000000222, 0.9649999999999999689, 0.9699999999999999734, 0.9749999999999999778, 0.9799999999999999822, 0.9849999999999999867, 0.9875000000000000444 ),
 .UNSPECIFIED. ) 
 CURVE ( )  GEOMETRIC_REPRESENTATION_ITEM ( )  RATIONAL_B_SPLINE_CURVE ( ( 0.9755282581475767101, 0.9755282581475772652, 1.000000000000000000, 0.9510565162951535312, 1.000000000000000000, 0.9510565162951535312, 1.000000000000000000, 0.9510565162951535312, 1.000000000000000000, 0.9510565162951535312, 1.000000000000000000, 0.9755282581475761550, 0.9755282581475767101 ) ) 
 REPRESENTATION_ITEM ( '' )  );
#17026 = ADVANCED_FACE ( 'NONE', ( #45833 ), #44357, .F. ) ;
#17027 = CARTESIAN_POINT ( 'NONE',  ( 205.9334673742153257, 273.9597668594684023, -10.28447216160094158 ) ) ;
#17028 = CARTESIAN_POINT ( 'NONE',  ( 190.2767435973494798, 301.0780079210716735, 3.520490206057748317 ) ) ;
#17029 = CARTESIAN_POINT ( 'NONE',  ( 156.6812872898450735, 261.2670451491295012, 0.000000000000000000 ) ) ;
#17030 = CARTESIAN_POINT ( 'NONE',  ( 82.36756280691109566, 40.91737819406999677, 1.008661990617413462 ) ) ;
#17031 = CARTESIAN_POINT ( 'NONE',  ( 167.6860649869540509, 249.0846947427896509, -5.222016127407463237 ) ) ;
#17032 = FACE_OUTER_BOUND ( 'NONE', #28394, .T. ) ;
#17033 = ADVANCED_FACE ( 'NONE', ( #5872 ), #51973, .T. ) ;
#17034 = CARTESIAN_POINT ( 'NONE',  ( 153.8583843864966241, 279.6722161493621570, 2.192119895967011622 ) ) ;
#17035 = EDGE_CURVE ( 'NONE', #10907, #93808, #91011, .T. ) ;
#17036 = CARTESIAN_POINT ( 'NONE',  ( 134.1932619090760568, 236.0327760586659736, 1.948934522072303157E-15 ) ) ;
#17037 = CARTESIAN_POINT ( 'NONE',  ( 186.6308142930050735, 262.8605285626102841, -9.271754035113762171 ) ) ;
#17038 = VERTEX_POINT ( 'NONE', #30156 ) ;
#17039 = VECTOR ( 'NONE', #94840, 1000.000000000000000 ) ;
#17040 = EDGE_CURVE ( 'NONE', #36797, #52552, #76756, .T. ) ;
#17042 = EDGE_LOOP ( 'NONE', ( #5584, #87496, #31677, #60742 ) ) ;
#17041 = DIRECTION ( 'NONE',  ( 0.000000000000000000, 0.000000000000000000, 1.000000000000000000 ) ) ;
#17043 = CARTESIAN_POINT ( 'NONE',  ( 200.0693866756322734, 273.7496136914496674, 13.78539325936003657 ) ) ;
#17044 = CARTESIAN_POINT ( 'NONE',  ( 180.7525632646832321, 256.2381716922662918, 1.265208511841812600 ) ) ;
#17045 = CARTESIAN_POINT ( 'NONE',  ( 174.0979558812879304, 290.0036607898268244, -4.751154830586174604 ) ) ;
#17046 = CARTESIAN_POINT ( 'NONE',  ( 192.0448397941376584, 298.0155754755651287, 11.82564086563478156 ) ) ;
#17047 = DIRECTION ( 'NONE',  ( -0.8660254037844387076, -0.4999999999999998890, -0.000000000000000000 ) ) ;
#17048 = CARTESIAN_POINT ( 'NONE',  ( 81.26123305391610074, 43.19691626584125999, 9.572390852610855205 ) ) ;
#17049 = CARTESIAN_POINT ( 'NONE',  ( 79.41556488834493166, 57.64893992652134358, 16.61893195969238946 ) ) ;
#17050 =( BOUNDED_CURVE ( )  B_SPLINE_CURVE ( 2, ( #4323, #98039, #29134, #43814, #90478, #75239, #36212, #35224, #89962 ),
 .UNSPECIFIED., .F., .T. ) 
 B_SPLINE_CURVE_WITH_KNOTS ( ( 3, 2, 2, 2, 3 ),
 ( 0.02016129032258064807, 0.02150537634408602322, 0.02419354838709677352, 0.02688172043010752729, 0.02822580645161290591 ),
 .UNSPECIFIED. ) 
 CURVE ( )  GEOMETRIC_REPRESENTATION_ITEM ( )  RATIONAL_B_SPLINE_CURVE ( ( 0.9330127018922192983, 0.9330127018922194093, 1.000000000000000000, 0.8660254037844387076, 1.000000000000000000, 0.8660254037844387076, 1.000000000000000000, 0.9330127018922191873, 0.9330127018922192983 ) ) 
 REPRESENTATION_ITEM ( '' )  );
#17051 = CARTESIAN_POINT ( 'NONE',  ( 173.2412943989675398, 277.7050541934257240, 16.79641741871846250 ) ) ;
#17052 = CARTESIAN_POINT ( 'NONE',  ( 177.2220074482157770, 256.0735339440234952, -7.327850677533820800 ) ) ;
#17053 = ORIENTED_EDGE ( 'NONE', *, *, #72853, .T. ) ;
#17054 = CARTESIAN_POINT ( 'NONE',  ( 194.4666154385731431, 293.8209370148700827, -14.56896502715340702 ) ) ;
#17055 = CARTESIAN_POINT ( 'NONE',  ( 166.9178459015252542, 248.1196852899930718, -6.726913786253128080 ) ) ;
#17056 = VERTEX_POINT ( 'NONE', #21574 ) ;
#17057 = DIRECTION ( 'NONE',  ( -1.000000000000000000, 0.000000000000000000, 0.000000000000000000 ) ) ;
#17058 = CARTESIAN_POINT ( 'NONE',  ( 158.0274747602609580, 277.2166826364630197, 10.25079899571118602 ) ) ;
#17059 = CARTESIAN_POINT ( 'NONE',  ( 151.9376213889835299, 267.4833155035536265, -16.92460756927863130 ) ) ;
#17060 = DIRECTION ( 'NONE',  ( -0.8660254037844377084, -0.5000000000000014433, -0.000000000000000000 ) ) ;
#17061 = CARTESIAN_POINT ( 'NONE',  ( 202.9216520459657147, 279.1763840310111391, 15.75371595331685803 ) ) ;
#17063 = CARTESIAN_POINT ( 'NONE',  ( 154.5109925159944169, 277.6691952191739574, -9.102046555125145488 ) ) ;
#17062 = CARTESIAN_POINT ( 'NONE',  ( 161.4315010361464431, 281.4375180470930218, -6.688515640316089694 ) ) ;
#17064 = CARTESIAN_POINT ( 'NONE',  ( 200.0792105639032172, 267.3392562440996585, 6.292352169839691811 ) ) ;
#17065 = ORIENTED_EDGE ( 'NONE', *, *, #40547, .T. ) ;
#17066 = CARTESIAN_POINT ( 'NONE',  ( 205.0054711740847608, 272.4066460739620084, -9.410916817109468369 ) ) ;
#17067 = B_SPLINE_CURVE_WITH_KNOTS ( 'NONE', 3,
 ( #87487, #26613, #26115, #65106, #25094, #56992, #55977, #64104, #49905, #18520, #18023, #19033, #48916, #10922 ),
 .UNSPECIFIED., .F., .F.,
 ( 4, 2, 2, 2, 2, 2, 4 ),
 ( 0.001295899257826045765, 0.001512579950660447722, 0.001729260643494849679, 0.001945941336329251635, 0.002162622029163653592, 0.002595983414832457505, 0.003029344800501261419 ),
 .UNSPECIFIED. ) ;
#17068 = CARTESIAN_POINT ( 'NONE',  ( 186.8071600733163393, 262.5868003515040527, -8.808218396323256982 ) ) ;
#17069 = CARTESIAN_POINT ( 'NONE',  ( -19.65312891409030271, 93.06504152958497400, 25.00000000000000000 ) ) ;
#17070 = CARTESIAN_POINT ( 'NONE',  ( 73.95673202641080479, 225.0530062829863311, -4.648177544792955347E-16 ) ) ;
#17071 = CARTESIAN_POINT ( 'NONE',  ( 200.0313018224816801, 276.5939864008022369, 15.71640468486303099 ) ) ;
#17072 = CIRCLE ( 'NONE', #62395, 45.19948692389424139 ) ;
#17073 = CARTESIAN_POINT ( 'NONE',  ( 153.2712411579340426, 265.1734183057532732, 16.26687330118495467 ) ) ;
#17074 = LINE ( 'NONE', #86543, #57597 ) ;
#17075 = CARTESIAN_POINT ( 'NONE',  ( 74.23458728405026363, 68.58752153053315226, 11.05172902932885748 ) ) ;
#17076 = CARTESIAN_POINT ( 'NONE',  ( 71.73760591565927314, 71.67260046175982779, -3.632057051425773953 ) ) ;
#17077 = CARTESIAN_POINT ( 'NONE',  ( -3.667330603741788320, 162.5643266524160140, 9.188101187500095079 ) ) ;
#17078 = CARTESIAN_POINT ( 'NONE',  ( 87.02133327910362937, 230.2369531367911009, -4.594050593750048428 ) ) ;
#17079 = CARTESIAN_POINT ( 'NONE',  ( 203.4696564630250464, 278.2272125378923988, -16.38980782817167636 ) ) ;
#17080 = CARTESIAN_POINT ( 'NONE',  ( 88.11938802471243548, 44.55983648551643483, -5.053413235213819021 ) ) ;
#17081 = DIRECTION ( 'NONE',  ( -0.8660254037844387076, -0.4999999999999998890, -0.000000000000000000 ) ) ;
#17082 = ADVANCED_FACE ( 'NONE', ( #44850 ), #61041, .T. ) ;
#17083 = CARTESIAN_POINT ( 'NONE',  ( 154.9903553346911735, 262.1958252075976361, -18.39016733948542637 ) ) ;
#17084 = CARTESIAN_POINT ( 'NONE',  ( 78.56874099464104688, 58.44545352437597785, 16.21180999836897385 ) ) ;
#17085 = CARTESIAN_POINT ( 'NONE',  ( 84.75937136884553524, 50.43455760676256006, -13.50133169173267156 ) ) ;
#17086 = CARTESIAN_POINT ( 'NONE',  ( 77.60916036496431047, 61.86143054388973184, 15.65520624218167889 ) ) ;
#17088 = CARTESIAN_POINT ( 'NONE',  ( 76.38456361472545098, 51.42163124864198664, 15.62351987089070526 ) ) ;
#17087 = CARTESIAN_POINT ( 'NONE',  ( 23.64814127513158937, 118.0650415295850451, 45.00000000000000711 ) ) ;
#17089 = CARTESIAN_POINT ( 'NONE',  ( 162.0191462209216979, 250.0216022768697144, 13.77935367201302341 ) ) ;
#17090 = CARTESIAN_POINT ( 'NONE',  ( -9.297732140679750401, 176.9860189848785410, -2.679491924311252493 ) ) ;
#17091 = CARTESIAN_POINT ( 'NONE',  ( 164.7508860646548783, 245.2900900744633930, -5.203382148009804808 ) ) ;
#17092 = CARTESIAN_POINT ( 'NONE',  ( 157.8763546842245376, 257.1971277035954699, 17.68444922773363004 ) ) ;
#17093 = CARTESIAN_POINT ( 'NONE',  ( 71.63103492117564031, 72.07843208848032646, 3.395715836721240777 ) ) ;
#17094 = CARTESIAN_POINT ( 'NONE',  ( 47.23881193640350062, 188.8923013555410080, 4.594050593750050204 ) ) ;
#17095 = CARTESIAN_POINT ( 'NONE',  ( 61.36533069198963375, 215.4244531367911293, -4.594050593750046652 ) ) ;
#17096 = DIRECTION ( 'NONE',  ( 0.000000000000000000, 0.000000000000000000, 1.000000000000000000 ) ) ;
#17098 = EDGE_CURVE ( 'NONE', #86003, #28497, #99804, .T. ) ;
#17097 = DIRECTION ( 'NONE',  ( -0.5295078238379060664, -0.5024823063053051042, -0.6834712842135700628 ) ) ;
#17099 = B_SPLINE_CURVE_WITH_KNOTS ( 'NONE', 3,
 ( #27891, #36479, #67383, #43067, #21301, #58286, #42090, #90744, #20811, #73507 ),
 .UNSPECIFIED., .F., .F.,
 ( 4, 2, 2, 2, 4 ),
 ( 0.000000000000000000, 0.0002622400424273466394, 0.0005244800848546932789, 0.0007867201272820399183, 0.001048960169709386558 ),
 .UNSPECIFIED. ) ;
#17100 = CARTESIAN_POINT ( 'NONE',  ( 13.87707171214468715, 8.416033932543234286, -1.583844403245364241 ) ) ;
#17102 = DIRECTION ( 'NONE',  ( -0.8660254037844387076, -0.4999999999999998890, -0.000000000000000000 ) ) ;
#17101 = CARTESIAN_POINT ( 'NONE',  ( 184.8670040873090841, 279.3961096007919878, 17.75634087450649190 ) ) ;
#17103 = CARTESIAN_POINT ( 'NONE',  ( 181.8129518053731033, 270.5384970965435514, -17.23398818032472946 ) ) ;
#17104 = AXIS2_PLACEMENT_3D ( 'NONE', #52671, #13696, #37963 ) ;
#17105 = CARTESIAN_POINT ( 'NONE',  ( 30.57771352727866443, 18.44966523072495335, -2.296566073217252530E-15 ) ) ;
#17106 = CARTESIAN_POINT ( 'NONE',  ( 150.7850480413316632, 269.4796311011364764, -14.43114374163211089 ) ) ;
#17107 = CARTESIAN_POINT ( 'NONE',  ( 148.9194629746633893, 272.7109192224475009, -12.27648025871169679 ) ) ;
#17108 = CARTESIAN_POINT ( 'NONE',  ( 16.80672687576512203, 25.10171378149917842, 9.188101187500008038 ) ) ;
#17109 = CARTESIAN_POINT ( 'NONE',  ( 69.24135662524314228, 198.5327760586659451, 1.948934522072302763E-15 ) ) ;
#17110 = CARTESIAN_POINT ( 'NONE',  ( 97.16130770534415717, 220.2365022471902023, 10.00000000000009948 ) ) ;
#17111 = CARTESIAN_POINT ( 'NONE',  ( 202.7754741559590173, 279.4295715634463022, -15.65855077192107636 ) ) ;
#17112 = CARTESIAN_POINT ( 'NONE',  ( 198.6587626159274294, 286.5599251108861267, 17.99840276545888784 ) ) ;
#17113 = DIRECTION ( 'NONE',  ( -0.4999999999999987788, 0.8660254037844392627, 0.000000000000000000 ) ) ;
#17114 = CARTESIAN_POINT ( 'NONE',  ( 201.6407369932504992, 281.3949939824937019, 16.25974739329136298 ) ) ;
#17115 = EDGE_CURVE ( 'NONE', #27140, #32226, #65792, .T. ) ;
#17116 = AXIS2_PLACEMENT_3D ( 'NONE', #69864, #17166, #77986 ) ;
#17117 = EDGE_CURVE ( 'NONE', #50533, #60486, #75289, .T. ) ;
#17118 = CARTESIAN_POINT ( 'NONE',  ( 34.97213163436671124, 51.32435524152969464, -10.00000000000000000 ) ) ;
#17119 = CARTESIAN_POINT ( 'NONE',  ( 87.55613534105700069, 44.89236293052572790, -6.575074172489557611 ) ) ;
#17120 = CARTESIAN_POINT ( 'NONE',  ( 117.4407359106297264, 248.6115022471903160, -5.000000000000047962 ) ) ;
#17121 = DIRECTION ( 'NONE',  ( -0.4972609476841356457, 0.8612812260087758798, 0.1045284632676436315 ) ) ;
#17122 = CARTESIAN_POINT ( 'NONE',  ( 207.4764081617721843, 271.2873150223495600, 6.359972247200924578 ) ) ;
#17123 = ORIENTED_EDGE ( 'NONE', *, *, #62303, .F. ) ;
#17124 = CARTESIAN_POINT ( 'NONE',  ( 77.71494937802162895, 49.45066113300357102, 15.33194528869553785 ) ) ;
#17125 = CARTESIAN_POINT ( 'NONE',  ( 184.8398010511286316, 271.1657223325220798, 16.51723966498060037 ) ) ;
#17126 = ORIENTED_EDGE ( 'NONE', *, *, #30617, .F. ) ;
#17127 = CARTESIAN_POINT ( 'NONE',  ( 159.2186641046529303, 254.8721795879351646, -15.96198087403305443 ) ) ;
#17128 = LINE ( 'NONE', #87106, #27186 ) ;
#17129 = DIRECTION ( 'NONE',  ( -0.03304531753666253152, -0.9994538543569188027, 0.000000000000000000 ) ) ;
#17130 = ORIENTED_EDGE ( 'NONE', *, *, #7896, .T. ) ;
#17131 = CARTESIAN_POINT ( 'NONE',  ( -19.65312891409030271, 93.06504152958497400, 40.00000000000000000 ) ) ;
#17132 = VERTEX_POINT ( 'NONE', #53933 ) ;
#17133 = CARTESIAN_POINT ( 'NONE',  ( 79.56052108471259032, 46.24302599146017911, -13.19616287432493706 ) ) ;
#17134 = CARTESIAN_POINT ( 'NONE',  ( 167.3947881066641514, 247.6242492910987778, 3.581681636340571018 ) ) ;
#17135 = CARTESIAN_POINT ( 'NONE',  ( 148.4951514626549738, 273.8415162155406506, 8.072631028758147309 ) ) ;
#17136 = ORIENTED_EDGE ( 'NONE', *, *, #24480, .F. ) ;
#17137 = CARTESIAN_POINT ( 'NONE',  ( 22.71735025659390317, 28.51421378149919406, -9.188101187500004485 ) ) ;
#17138 = AXIS2_PLACEMENT_3D ( 'NONE', #72811, #49469, #41870 ) ;
#17139 = CARTESIAN_POINT ( 'NONE',  ( 74.92223598134691542, 66.83043205548884202, -13.20899543911388108 ) ) ;
#17140 = CARTESIAN_POINT ( 'NONE',  ( 81.06846199619322135, 48.85856745326930906, -13.70439893166367362 ) ) ;
#17141 = VERTEX_POINT ( 'NONE', #37257 ) ;
#17142 = DIRECTION ( 'NONE',  ( 0.000000000000000000, 1.000000000000000000, 0.000000000000000000 ) ) ;
#17143 = FACE_OUTER_BOUND ( 'NONE', #46675, .T. ) ;
#17144 = AXIS2_PLACEMENT_3D ( 'NONE', #68538, #98472, #37628 ) ;
#17145 = VERTEX_POINT ( 'NONE', #6857 ) ;
#17146 = CARTESIAN_POINT ( 'NONE',  ( 183.2164173712471040, 295.8027025434371922, 1.003979349283407707 ) ) ;
#17147 = ADVANCED_FACE ( 'NONE', ( #92016 ), #52959, .T. ) ;
#17149 = LINE ( 'NONE', #57640, #86421 ) ;
#17148 = CARTESIAN_POINT ( 'NONE',  ( 67.65092628909327743, 65.77671196984043434, 10.59442795868019260 ) ) ;
#17150 = CARTESIAN_POINT ( 'NONE',  ( 81.54778536404420208, 55.93674090176426716, -16.03022157117148794 ) ) ;
#17151 = CARTESIAN_POINT ( 'NONE',  ( 193.8913555215501390, 294.8173164187117550, 15.40725395879721837 ) ) ;
#17152 = CARTESIAN_POINT ( 'NONE',  ( 185.4383826630807448, 292.6325493778165310, -10.71708923905308986 ) ) ;
#17153 = CARTESIAN_POINT ( 'NONE',  ( 157.7733463334721478, 257.3755434007023268, -16.94489513499352995 ) ) ;
#17154 = CARTESIAN_POINT ( 'NONE',  ( 135.2211464324225858, 255.0024278399161517, -9.188101187500093303 ) ) ;
#17155 = CARTESIAN_POINT ( 'NONE',  ( 73.74570213160561138, 62.19087806175586053, -15.23723686604174077 ) ) ;
#17156 = CARTESIAN_POINT ( 'NONE',  ( 79.59476633789469702, 59.27799801817308634, 16.56459525109985975 ) ) ;
#17157 = CARTESIAN_POINT ( 'NONE',  ( 88.48327179163739231, 212.7048013555409796, 4.594050593750051981 ) ) ;
#17158 = EDGE_LOOP ( 'NONE', ( #63515, #71640, #57523, #39147 ) ) ;
#17159 = CARTESIAN_POINT ( 'NONE',  ( 150.7530568467738590, 269.5350414755053521, 15.60317050893315916 ) ) ;
#17160 = CARTESIAN_POINT ( 'NONE',  ( 77.82180247422382990, 61.41261899432889493, -16.13690189282890941 ) ) ;
#17161 = ORIENTED_EDGE ( 'NONE', *, *, #1452, .F. ) ;
#17162 = CARTESIAN_POINT ( 'NONE',  ( 157.1602365732760802, 258.4374806559784474, -16.85676213245926292 ) ) ;
#17163 = VERTEX_POINT ( 'NONE', #53446 ) ;
#17164 = CARTESIAN_POINT ( 'NONE',  ( 80.01671443575703790, 44.39865788142935088, -11.57581203907570000 ) ) ;
#17165 = EDGE_CURVE ( 'NONE', #13291, #77081, #84397, .T. ) ;
#17166 = DIRECTION ( 'NONE',  ( -0.7713848165480218233, 0.6363689690731114679, 0.000000000000000000 ) ) ;
#17167 = CARTESIAN_POINT ( 'NONE',  ( 191.0481192767711036, 299.7419460525905492, -9.103377665618040737 ) ) ;
#17168 = CARTESIAN_POINT ( 'NONE',  ( 163.8402655714165519, 249.7793471524227868, 10.22989909625667693 ) ) ;
#17169 = CARTESIAN_POINT ( 'NONE',  ( 85.35902799246794359, 47.15769306684208573, -10.74235809367880456 ) ) ;
#17170 = CARTESIAN_POINT ( 'NONE',  ( 162.5429104506708597, 249.1144160197565043, 10.44355587256373674 ) ) ;
#17171 = CARTESIAN_POINT ( 'NONE',  ( 88.13136219740870558, 215.5643266524159571, -9.188101187500093303 ) ) ;
#17172 = ORIENTED_EDGE ( 'NONE', *, *, #57167, .F. ) ;
#17173 = ORIENTED_EDGE ( 'NONE', *, *, #45138, .F. ) ;
#17174 = CARTESIAN_POINT ( 'NONE',  ( 208.3863431123642727, 269.7112614563416173, -1.693909372230378851 ) ) ;
#17175 = VERTEX_POINT ( 'NONE', #13485 ) ;
#17176 = DIRECTION ( 'NONE',  ( -0.000000000000000000, -0.000000000000000000, -1.000000000000000000 ) ) ;
#17177 = VECTOR ( 'NONE', #27134, 1000.000000000000000 ) ;
#17178 = CARTESIAN_POINT ( 'NONE',  ( 161.5852327833977142, 283.9684635997116970, 0.5249851707666771672 ) ) ;
#17179 = CARTESIAN_POINT ( 'NONE',  ( 87.90883736606430432, 44.33697863951398688, 4.769790285073533198 ) ) ;
#17180 = VERTEX_POINT ( 'NONE', #69148 ) ;
#17182 = CARTESIAN_POINT ( 'NONE',  ( 84.04835165962728638, 43.69724715580328933, -7.079821572537318808 ) ) ;
#17181 = CIRCLE ( 'NONE', #12366, 0.1418229129681522482 ) ;
#17183 = CARTESIAN_POINT ( 'NONE',  ( 32.41152252715882298, 42.21091486745863364, 7.012934429366973338E-14 ) ) ;
#17184 = CARTESIAN_POINT ( 'NONE',  ( 206.0870578475358172, 273.6937403561189512, -10.07771901274806581 ) ) ;
#17185 = CARTESIAN_POINT ( 'NONE',  ( 155.7501102573973526, 262.3711424935290211, -17.08610291111812529 ) ) ;
#17186 = CARTESIAN_POINT ( 'NONE',  ( 174.5965431966999120, 283.7287010187061469, 13.61117779920129323 ) ) ;
#17187 = CARTESIAN_POINT ( 'NONE',  ( 198.9920886056412144, 285.3025922593915311, -17.15779807132265944 ) ) ;
#17188 = EDGE_CURVE ( 'NONE', #66481, #85402, #88961, .T. ) ;
#17189 = CARTESIAN_POINT ( 'NONE',  ( 141.4548986661878303, 259.1427522451419350, 10.00000000000009415 ) ) ;
#17190 = ORIENTED_EDGE ( 'NONE', *, *, #10513, .T. ) ;
#17191 = CARTESIAN_POINT ( 'NONE',  ( -1.637757109730603178, 179.8615022471903444, 5.000000000000046185 ) ) ;
#17192 = CARTESIAN_POINT ( 'NONE',  ( 200.2690241097007799, 283.7708703901988656, 16.96680019208369927 ) ) ;
#17193 = CARTESIAN_POINT ( 'NONE',  ( 85.39402269659207434, 44.11278400351730511, 6.509279094370365115 ) ) ;
#17194 = CARTESIAN_POINT ( 'NONE',  ( 186.6676767428766937, 265.3792542468744386, -11.85556035995023905 ) ) ;
#17195 = CARTESIAN_POINT ( 'NONE',  ( 78.20977235749720080, 61.70939135586247204, 16.12143617465002521 ) ) ;
#17196 = CARTESIAN_POINT ( 'NONE',  ( 174.9406376537963297, 290.1712607282375984, -6.365627776605657040 ) ) ;
#17197 = ADVANCED_FACE ( 'NONE', ( #9357, #16449 ), #47348, .F. ) ;
#17198 = CARTESIAN_POINT ( 'NONE',  ( 156.6677280378305284, 272.7060788182535020, 14.73662401990965876 ) ) ;
#17199 = VERTEX_POINT ( 'NONE', #31138 ) ;
#17200 = VECTOR ( 'NONE', #22885, 1000.000000000000000 ) ;
#17201 = CARTESIAN_POINT ( 'NONE',  ( 72.67881136679183385, 64.39378700367657871, -13.40573345294599328 ) ) ;
#17203 = CARTESIAN_POINT ( 'NONE',  ( 73.87064539096938631, 55.12372134487154796, 16.60095896530753379 ) ) ;
#17202 = CARTESIAN_POINT ( 'NONE',  ( 179.9792551569844363, 266.4521290304439276, -14.77927586968167617 ) ) ;
#17204 = CARTESIAN_POINT ( 'NONE',  ( 183.2562432415718092, 256.2013173691302086, 2.311692295278971798 ) ) ;
#17205 = CARTESIAN_POINT ( 'NONE',  ( 29.10770312285472627, 32.50829794293882458, -10.00000000000000355 ) ) ;
#17206 = CARTESIAN_POINT ( 'NONE',  ( 181.8559320684326224, 273.7276056269956257, 17.73031764801637067 ) ) ;
#17207 = CARTESIAN_POINT ( 'NONE',  ( 175.7622132985686392, 274.0430017844784629, -17.75579533532145504 ) ) ;
#17208 = CARTESIAN_POINT ( 'NONE',  ( -61.61048871844075592, 38.59675092633816007, -10.00000000000000000 ) ) ;
#17209 = CARTESIAN_POINT ( 'NONE',  ( 195.0382653549689280, 265.8412794934087628, -7.320742485009862577 ) ) ;
#17210 = CARTESIAN_POINT ( 'NONE',  ( -3.153561889951042474, 178.1744531367911577, 4.594050593750047540 ) ) ;
#17211 = CARTESIAN_POINT ( 'NONE',  ( 82.83348971583357923, 50.32886766858683103, 14.01852798243808529 ) ) ;
#17212 = ORIENTED_EDGE ( 'NONE', *, *, #22528, .F. ) ;
#17213 = CARTESIAN_POINT ( 'NONE',  ( 161.3981413584396876, 253.0972142504356270, -15.11937522241654719 ) ) ;
#17214 = CARTESIAN_POINT ( 'NONE',  ( 35.25707387162091067, 20.75978393459166327, -1.583844403245362020 ) ) ;
#17215 = CARTESIAN_POINT ( 'NONE',  ( 203.7676226056132691, 275.1754274059050545, -12.67277803424182281 ) ) ;
#17216 = CARTESIAN_POINT ( 'NONE',  ( 72.11276354278739120, 72.31486658476875107, -1.049745372677822530 ) ) ;
#17217 = CARTESIAN_POINT ( 'NONE',  ( 26.91401791951368949, 186.3458772461660544, 9.188101187500095079 ) ) ;
#17218 = CARTESIAN_POINT ( 'NONE',  ( 66.77824978924009258, 209.3615022471902591, -10.00000000000009592 ) ) ;
#17219 = CARTESIAN_POINT ( 'NONE',  ( 36.28012939083434674, 26.11029122506296929, -8.090169943749478065 ) ) ;
#17220 = CARTESIAN_POINT ( 'NONE',  ( 178.6803586118992939, 291.7013059717194210, 6.068282667768776228 ) ) ;
#17221 = CARTESIAN_POINT ( 'NONE',  ( 191.8329718516215223, 298.3825415164982928, -8.871589506312979267 ) ) ;
#17222 = CARTESIAN_POINT ( 'NONE',  ( 149.6891899025559383, 271.3777130753837241, 11.83206864037965289 ) ) ;
#17223 = CARTESIAN_POINT ( 'NONE',  ( 73.42854352997271405, 67.10243356698696005, 12.40008471655043820 ) ) ;
#17224 = CARTESIAN_POINT ( 'NONE',  ( 81.33751392502985311, 42.06992806637205717, 7.942293151799421302 ) ) ;
#17225 = FACE_OUTER_BOUND ( 'NONE', #25623, .T. ) ;
#17226 = CARTESIAN_POINT ( 'NONE',  ( 83.39698567699524290, 51.83659370627650986, 14.98600084375454067 ) ) ;
#17227 = EDGE_CURVE ( 'NONE', #49678, #50293, #42920, .T. ) ;
#17228 = EDGE_CURVE ( 'NONE', #54644, #46249, #29671, .T. ) ;
#17229 = CARTESIAN_POINT ( 'NONE',  ( 73.27344031762343946, 203.1115022471901739, -5.000000000000041744 ) ) ;
#17230 = CARTESIAN_POINT ( 'NONE',  ( 70.73742561589182287, 66.68555088280790244, -10.79243469196173599 ) ) ;
#17231 = CARTESIAN_POINT ( 'NONE',  ( 185.6221575045317138, 277.7868078161695280, -17.14424904577442277 ) ) ;
#17232 = CARTESIAN_POINT ( 'NONE',  ( 149.9899443387552083, 245.8567911112850481, 0.000000000000000000 ) ) ;
#17233 = ADVANCED_FACE ( 'NONE', ( #27573 ), #59339, .F. ) ;
#17234 = CARTESIAN_POINT ( 'NONE',  ( 38.06444208900335013, 180.5327760586659451, 1.948934522072303157E-15 ) ) ;
#17235 = CARTESIAN_POINT ( 'NONE',  ( 159.2876523829509665, 254.7526883847961017, 15.64395448151312351 ) ) ;
#17236 = EDGE_CURVE ( 'NONE', #62754, #77470, #47771, .T. ) ;
#17237 = CARTESIAN_POINT ( 'NONE',  ( 203.1584666061235396, 270.1366466773015986, -6.432727867013968925 ) ) ;
#17238 = FACE_OUTER_BOUND ( 'NONE', #23216, .T. ) ;
#17239 = DIRECTION ( 'NONE',  ( -0.8660254037844359321, -0.5000000000000051070, -0.000000000000000000 ) ) ;
#17240 = ORIENTED_EDGE ( 'NONE', *, *, #68513, .T. ) ;
#17241 = DIRECTION ( 'NONE',  ( -0.07193265315672570104, 0.9974094913373514615, 0.000000000000000000 ) ) ;
#17242 = CARTESIAN_POINT ( 'NONE',  ( -8.223158621222619757, 159.3927522451418213, 10.00000000000009948 ) ) ;
#17243 = CARTESIAN_POINT ( 'NONE',  ( -52.33464467766007289, 32.58262665401804270, 10.00000000000000000 ) ) ;
#17244 = B_SPLINE_CURVE_WITH_KNOTS ( 'NONE', 3,
 ( #20241, #35919, #82582, #5037, #27830, #44508, #45508, #28316, #98751, #12649, #51115, #14128, #45010, #90171, #99236, #44002, #75438, #83061, #60197, #66820, #13145, #75955, #97748, #14628, #67830, #6532, #58706, #37407, #20744, #90679, #43518, #51630, #74944, #5528, #89680, #29331, #76440, #36412, #21723, #74457, #67316, #68313, #98244, #28832, #52114, #21235, #52607, #13634, #29822, #60696 ),
 .UNSPECIFIED., .F., .F.,
 ( 4, 2, 2, 2, 2, 2, 2, 2, 2, 2, 2, 2, 2, 2, 2, 2, 2, 2, 2, 2, 2, 2, 2, 2, 4 ),
 ( 0.0003547852092621711076, 0.001373122238808988701, 0.001882290753582355376, 0.002009582882275727511, 0.002136875010969099646, 0.002264167139662471781, 0.002391459268355844350, 0.002646043525742580813, 0.002900627783129316843, 0.003409796297902792806, 0.004428133327449595112, 0.005446470356996396985, 0.005955638871769835217, 0.006210223129156513568, 0.006464807386543191051, 0.006528453450889841990, 0.006592099515236493797, 0.006655745579583143869, 0.006719391643929794808, 0.006973975901316441933, 0.007483144416089663326, 0.007737728673476274022, 0.007992312930862884718, 0.008246897188249495414, 0.008501481445636106110 ),
 .UNSPECIFIED. ) ;
#17245 = CARTESIAN_POINT ( 'NONE',  ( 201.6504829983214222, 272.7620465441235638, 12.67600476192259507 ) ) ;
#17246 = CARTESIAN_POINT ( 'NONE',  ( 25.14222138719033595, 29.91421378149919974, 9.188101187500008038 ) ) ;
#17247 = CARTESIAN_POINT ( 'NONE',  ( 202.9093905060991005, 279.1976216410395182, 16.97070083370504179 ) ) ;
#17248 = CARTESIAN_POINT ( 'NONE',  ( 196.9728329903666122, 289.4800408803428695, -17.53478045286815856 ) ) ;
#17249 = VECTOR ( 'NONE', #70280, 1000.000000000000000 ) ;
#17250 = CARTESIAN_POINT ( 'NONE',  ( 186.0548307059467277, 267.6833961656038241, -15.01235236491201164 ) ) ;
#17251 = VERTEX_POINT ( 'NONE', #67037 ) ;
#17252 = VECTOR ( 'NONE', #56012, 1000.000000000000114 ) ;
#17253 = CARTESIAN_POINT ( 'NONE',  ( 13.91516400911260298, 10.96004757982088584, -5.678558825948275768 ) ) ;
#17254 = CARTESIAN_POINT ( 'NONE',  ( 72.14092658844184314, 60.15097928497420554, -15.11828870562148097 ) ) ;
#17255 = CARTESIAN_POINT ( 'NONE',  ( 42.55121439978241682, 60.39930420098813357, -10.00000000000000000 ) ) ;
#17256 = B_SPLINE_CURVE_WITH_KNOTS ( 'NONE', 3,
 ( #9689, #47154, #41552, #71485 ),
 .UNSPECIFIED., .F., .F.,
 ( 4, 4 ),
 ( 0.8920974736355009593, 1.000000000000000000 ),
 .UNSPECIFIED. ) ;
#17257 = ORIENTED_EDGE ( 'NONE', *, *, #56694, .F. ) ;
#17258 = CARTESIAN_POINT ( 'NONE',  ( 183.6018926243820601, 279.6860137177432080, 17.64978500148036389 ) ) ;
#17259 = CARTESIAN_POINT ( 'NONE',  ( 178.7278109544135134, 282.3134984357692474, 15.46213385585119404 ) ) ;
#17260 = VECTOR ( 'NONE', #40711, 1000.000000000000000 ) ;
#17261 = CARTESIAN_POINT ( 'NONE',  ( 85.39213576672661077, 49.09213582878910387, 12.39711816105355169 ) ) ;
#17262 = CARTESIAN_POINT ( 'NONE',  ( 177.5672598793707948, 256.2453929386242066, -7.265003576077156744 ) ) ;
#17263 = CARTESIAN_POINT ( 'NONE',  ( 149.6676065383367416, 271.4150965588098074, 11.80358707172367261 ) ) ;
#17264 = ORIENTED_EDGE ( 'NONE', *, *, #52200, .F. ) ;
#17265 = ORIENTED_EDGE ( 'NONE', *, *, #17424, .T. ) ;
#17266 = B_SPLINE_CURVE_WITH_KNOTS ( 'NONE', 3,
 ( #80014, #977, #87149, #79521, #33371, #54653, #25268, #64274, #93716, #94212 ),
 .UNSPECIFIED., .F., .F.,
 ( 4, 2, 2, 2, 4 ),
 ( 0.000000000000000000, 0.2500000000000000000, 0.5000000000000000000, 0.7500000000000000000, 1.000000000000000000 ),
 .UNSPECIFIED. ) ;
#17268 = SURFACE_STYLE_USAGE ( .BOTH. , #61363 ) ;
#17267 = CARTESIAN_POINT ( 'NONE',  ( 189.5365842474118665, 274.1395708678550704, -15.66050912157280983 ) ) ;
#17269 = EDGE_LOOP ( 'NONE', ( #18273, #11209 ) ) ;
#17270 = CARTESIAN_POINT ( 'NONE',  ( 152.8328714238065515, 265.9326969577624027, -16.29536156676786263 ) ) ;
#17271 = CARTESIAN_POINT ( 'NONE',  ( 80.86586985908986946, 155.7185146834693512, 0.000000000000000000 ) ) ;
#17272 = CARTESIAN_POINT ( 'NONE',  ( 72.58983975722236437, 57.29650192470587911, -16.33847390063895944 ) ) ;
#17273 = CARTESIAN_POINT ( 'NONE',  ( 68.22375369157857961, 184.2153022007868515, 0.000000000000000000 ) ) ;
#17274 = CARTESIAN_POINT ( 'NONE',  ( 157.6668627405778409, 257.5599783937680058, -16.78811156090270629 ) ) ;
#17275 = CARTESIAN_POINT ( 'NONE',  ( 105.9391831106087096, 219.7202760586659167, -5.415160957724236172E-17 ) ) ;
#17276 = DIRECTION ( 'NONE',  ( -0.000000000000000000, 0.000000000000000000, -1.000000000000000000 ) ) ;
#17277 = VERTEX_POINT ( 'NONE', #91373 ) ;
#17278 = VECTOR ( 'NONE', #31755, 999.9999999999998863 ) ;
#17279 = CARTESIAN_POINT ( 'NONE',  ( 208.2555382576270233, 269.9378221106229034, 3.215405476967123199 ) ) ;
#17280 = ORIENTED_EDGE ( 'NONE', *, *, #25840, .F. ) ;
#17281 = CARTESIAN_POINT ( 'NONE',  ( 27.91350267930052809, 31.51421378149921182, -9.188101187500004485 ) ) ;
#17282 = CARTESIAN_POINT ( 'NONE',  ( 198.0858447170796524, 287.5522480202560018, 18.44384186289807559 ) ) ;
#17283 = CARTESIAN_POINT ( 'NONE',  ( 78.54833788481614931, 48.00718989679155158, -13.97922736711163871 ) ) ;
#17284 = CARTESIAN_POINT ( 'NONE',  ( 61.01376819352597636, 206.0333772461660544, 9.188101187500095079 ) ) ;
#17285 = CARTESIAN_POINT ( 'NONE',  ( 73.96424987833113107, 68.60250435897062005, 10.89670188853132160 ) ) ;
#17286 = CARTESIAN_POINT ( 'NONE',  ( 32.89180500207565672, 24.15404122711135670, 8.090169943749479842 ) ) ;
#17287 = CARTESIAN_POINT ( 'NONE',  ( 197.9988809731023025, 287.7028736432410483, 18.08661327024293897 ) ) ;
#17289 = VECTOR ( 'NONE', #69219, 1000.000000000000000 ) ;
#17288 = CARTESIAN_POINT ( 'NONE',  ( 176.6106934046284493, 273.2656583511206918, 17.19257000985071215 ) ) ;
#17290 = ORIENTED_EDGE ( 'NONE', *, *, #33756, .F. ) ;
#17291 = CARTESIAN_POINT ( 'NONE',  ( 79.44531977136954026, 56.84425820487384584, -16.19431182515960543 ) ) ;
#17292 = CARTESIAN_POINT ( 'NONE',  ( 85.51659574944204678, 43.18010505494499540, -3.869227498884009186 ) ) ;
#17293 = CARTESIAN_POINT ( 'NONE',  ( 177.3243750670959287, 288.8712866368100549, 11.28047403827316764 ) ) ;
#17294 = DIRECTION ( 'NONE',  ( 1.000000000000000000, 0.000000000000000000, 0.000000000000000000 ) ) ;
#17295 = VERTEX_POINT ( 'NONE', #5742 ) ;
#17296 = CARTESIAN_POINT ( 'NONE',  ( 101.2828866085936852, 240.8297689869268936, -2.679491924311252493 ) ) ;
#17297 = CARTESIAN_POINT ( 'NONE',  ( 68.99060303605790523, 69.57119366415392392, -4.889576104870550388 ) ) ;
#17298 = CARTESIAN_POINT ( 'NONE',  ( 207.3646600298985447, 271.4808684644054324, -5.284084612275558257 ) ) ;
#17299 = CARTESIAN_POINT ( 'NONE',  ( 146.8153075009282134, 276.3554234099810287, -4.113808735271278216 ) ) ;
#17300 = CARTESIAN_POINT ( 'NONE',  ( 149.6036070299368532, 271.5259469590175740, 11.63513718912356865 ) ) ;
#17301 = B_SPLINE_CURVE_WITH_KNOTS ( 'NONE', 3,
 ( #31386, #62270, #3028, #64805 ),
 .UNSPECIFIED., .F., .F.,
 ( 4, 4 ),
 ( 0.03832837999546955671, 0.04687175281637306901 ),
 .UNSPECIFIED. ) ;
#17302 = ADVANCED_FACE ( 'NONE', ( #91885 ), #6746, .T. ) ;
#17303 = CARTESIAN_POINT ( 'NONE',  ( 180.7592890006537800, 271.2502507736807047, 17.08356462066134540 ) ) ;
#17304 = CARTESIAN_POINT ( 'NONE',  ( 82.65630208547716506, 42.40614048910975242, -7.237031299700372955 ) ) ;
#17305 = CARTESIAN_POINT ( 'NONE',  ( 76.20785806305732990, 65.13882236753694599, 14.17010354976770081 ) ) ;
#17306 = CARTESIAN_POINT ( 'NONE',  ( 154.0654594722044521, 264.2254380362395523, -16.58972724529802889 ) ) ;
#17307 = CARTESIAN_POINT ( 'NONE',  ( -19.65312891409030271, 93.06504152958497400, 10.00000000000000888 ) ) ;
#17308 = CARTESIAN_POINT ( 'NONE',  ( 111.6762543149156386, 235.2833772461660544, -9.188101187500095079 ) ) ;
#17309 = ORIENTED_EDGE ( 'NONE', *, *, #18403, .T. ) ;
#17310 = CARTESIAN_POINT ( 'NONE',  ( 191.5324528500417216, 298.9030556958743432, -8.286652526617016790 ) ) ;
#17311 = CARTESIAN_POINT ( 'NONE',  ( 70.44136121614442914, 65.74669562498131370, 11.49719858076791112 ) ) ;
#17312 = CARTESIAN_POINT ( 'NONE',  ( 202.9881971861223917, 279.0611244672630278, -15.16231470264511927 ) ) ;
#17313 = CARTESIAN_POINT ( 'NONE',  ( 192.5198628683430684, 296.3988585064753352, 11.83524212884658411 ) ) ;
#17314 = CARTESIAN_POINT ( 'NONE',  ( 83.82065378329919270, 51.84410121092205515, -14.88618515114630370 ) ) ;
#17315 = CARTESIAN_POINT ( 'NONE',  ( 178.2401400375956939, 255.0819166014324821, 4.396970161736177829 ) ) ;
#17316 = ORIENTED_EDGE ( 'NONE', *, *, #55165, .T. ) ;
#17317 = CARTESIAN_POINT ( 'NONE',  ( 80.31827234370541646, 57.12191670730477000, -16.23302104177161098 ) ) ;
#17318 = CARTESIAN_POINT ( 'NONE',  ( 154.6982851380984130, 273.6571292083216349, -13.42362762759460892 ) ) ;
#17319 = CARTESIAN_POINT ( 'NONE',  ( 71.97624815057693581, 71.57072644777218784, 5.573434703584700500 ) ) ;
#17320 = CARTESIAN_POINT ( 'NONE',  ( 206.6961830126489303, 272.6387046219738295, -10.22526498917591375 ) ) ;
#17321 = CARTESIAN_POINT ( 'NONE',  ( 134.1932619090760568, 236.0327760586659736, 1.948934522072302763E-15 ) ) ;
#17322 = CARTESIAN_POINT ( 'NONE',  ( 198.4522155198218059, 286.9176751754968109, -17.57438352224490075 ) ) ;
#17323 = CARTESIAN_POINT ( 'NONE',  ( 190.2428527899854487, 298.9129196009670864, -8.201882143933323377 ) ) ;
#17324 = CARTESIAN_POINT ( 'NONE',  ( 188.0035612729766115, 279.2325960380115362, 17.82077010991123700 ) ) ;
#17325 = CARTESIAN_POINT ( 'NONE',  ( 47.96943409690536697, 192.3768266524160140, 9.188101187500098632 ) ) ;
#17326 = VECTOR ( 'NONE', #29054, 999.9999999999998863 ) ;
#17328 = CARTESIAN_POINT ( 'NONE',  ( 72.21962075016683968, 61.93018538591146438, -14.97888511395804301 ) ) ;
#17327 = VECTOR ( 'NONE', #74378, 1000.000000000000114 ) ;
#17329 = CARTESIAN_POINT ( 'NONE',  ( 189.6134825805156368, 259.7924916801782160, -1.707211797017506472 ) ) ;
#17330 = B_SPLINE_SURFACE_WITH_KNOTS ( 'NONE', 3, 1, ( 
 ( #48877, #86930 ),
 ( #85408, #39234 ),
 ( #25570, #79812 ),
 ( #71184, #24555 ),
 ( #9364, #32659 ),
 ( #1269, #56459 ),
 ( #55434, #40243 ),
 ( #63559, #756 ),
 ( #86424, #87450 ),
 ( #33161, #93499 ),
 ( #10376, #63061 ),
 ( #32154, #17983 ),
 ( #94498, #24059 ),
 ( #23541, #31640 ),
 ( #25056, #16456 ),
 ( #64066, #48370 ),
 ( #62540, #79318 ),
 ( #40743, #78275 ),
 ( #54953, #85932 ),
 ( #95010, #41246 ),
 ( #263, #46860 ),
 ( #92988, #47353 ),
 ( #8859, #39726 ),
 ( #96505, #27073 ),
 ( #66061, #41753 ),
 ( #65557, #34657 ),
 ( #4254, #57450 ),
 ( #28050, #33676 ),
 ( #50354, #19972 ),
 ( #72699, #82312 ),
 ( #97485, #97011 ) ),
 .UNSPECIFIED., .F., .F., .F.,
 ( 4, 3, 3, 3, 3, 3, 3, 3, 3, 3, 4 ),
 ( 2, 2 ),
 ( 0.000000000000000000, 0.1333490885032349860, 0.3007194338854367599, 0.4699862290245074292, 0.5844252810809225096, 0.6686540514502804511, 0.7354980260655492597, 0.8028463152565746830, 0.8633854507757233732, 0.9437142632667367970, 1.000000000000000000 ),
 ( 0.000000000000000000, 1.000000000000000000 ),
 .UNSPECIFIED. ) ;
#17331 = CARTESIAN_POINT ( 'NONE',  ( 69.26427230429020199, 70.44614424028236499, -2.306916011527871291 ) ) ;
#17332 = CARTESIAN_POINT ( 'NONE',  ( 171.1789833775259808, 259.9602249310370894, 14.90491122363313004 ) ) ;
#17333 = CARTESIAN_POINT ( 'NONE',  ( 151.8566147802715705, 278.2686478900306497, -1.635913686782525911 ) ) ;
#17334 = CARTESIAN_POINT ( 'NONE',  ( -19.65312891409030271, 93.06504152958497400, 177.5919119679930134 ) ) ;
#17335 = CARTESIAN_POINT ( 'NONE',  ( 155.6281496932864457, 261.0911329737299980, -18.07904265579665548 ) ) ;
#17336 = CARTESIAN_POINT ( 'NONE',  ( 17.70578863690133886, 169.4824982072973967, 3.021315404115420679E-15 ) ) ;
#17337 = VECTOR ( 'NONE', #86046, 1000.000000000000000 ) ;
#17338 = CARTESIAN_POINT ( 'NONE',  ( 119.0104069514411123, 249.5177522451419065, 5.000000000000046185 ) ) ;
#17339 = DIRECTION ( 'NONE',  ( -0.8660254037844379305, -0.5000000000000014433, -0.000000000000000000 ) ) ;
#17340 = EDGE_LOOP ( 'NONE', ( #35689, #46157, #62714, #6021 ) ) ;
#17341 = CARTESIAN_POINT ( 'NONE',  ( 147.6220714307702622, 274.9580672937808572, 8.392894244419288441 ) ) ;
#17342 = CARTESIAN_POINT ( 'NONE',  ( 87.56439764236804990, 44.61845377809836322, 4.962693721234261446 ) ) ;
#17343 = CARTESIAN_POINT ( 'NONE',  ( 20.90579313287664576, 189.0024278399160949, -9.188101187500093303 ) ) ;
#17344 = CARTESIAN_POINT ( 'NONE',  ( 12.21574338843640284, 25.79103043416548147, 8.090169943749478065 ) ) ;
#17345 = CIRCLE ( 'NONE', #10940, 70.00000000000001421 ) ;
#17346 = CARTESIAN_POINT ( 'NONE',  ( 80.11143256479013530, 210.3927522451418213, 10.00000000000009948 ) ) ;
#17347 = CARTESIAN_POINT ( 'NONE',  ( 146.9324727656309335, 276.1524872186338371, 3.813717745456558728 ) ) ;
#17348 = CARTESIAN_POINT ( 'NONE',  ( 72.28971570511666300, 72.05020073419474613, 3.372523219123622518 ) ) ;
#17350 = CARTESIAN_POINT ( 'NONE',  ( 60.12067949409930634, 205.5177522451418497, -10.00000000000009592 ) ) ;
#17349 = CARTESIAN_POINT ( 'NONE',  ( 152.8593402092683959, 275.2840601128194749, 10.96293945604634068 ) ) ;
#17351 = CARTESIAN_POINT ( 'NONE',  ( 4.135592144620554578, 24.16126292948893450, -6.180339887498951690 ) ) ;
#17352 = CARTESIAN_POINT ( 'NONE',  ( 163.2088130023161057, 256.0821108490627580, -14.95559493010926921 ) ) ;
#17353 = DIRECTION ( 'NONE',  ( 0.000000000000000000, 0.000000000000000000, -1.000000000000000000 ) ) ;
#17354 = CARTESIAN_POINT ( 'NONE',  ( 66.30020840643021529, 68.74685235891840307, -4.316186131942656878 ) ) ;
#17355 = VERTEX_POINT ( 'NONE', #36631 ) ;
#17356 = EDGE_CURVE ( 'NONE', #56036, #56410, #65909, .T. ) ;
#17357 = CARTESIAN_POINT ( 'NONE',  ( 19.94070920123167312, 188.9865022471903160, -10.00000000000009415 ) ) ;
#17358 = CARTESIAN_POINT ( 'NONE',  ( 32.27148724097330756, 200.9860189848785410, -2.679491924311252493 ) ) ;
#17359 = VECTOR ( 'NONE', #81336, 1000.000000000000000 ) ;
#17360 = CARTESIAN_POINT ( 'NONE',  ( 202.8211298556536804, 279.3504935719197988, 17.07914446815911447 ) ) ;
#17361 = CARTESIAN_POINT ( 'NONE',  ( -5.047471817081990331, 158.7048013555409796, 4.594050593750051981 ) ) ;
#17362 = CARTESIAN_POINT ( 'NONE',  ( 39.09967052555147404, 28.28920272979929962, -7.433330006724141015 ) ) ;
#17364 = CARTESIAN_POINT ( 'NONE',  ( 199.9134407114337364, 283.6250491837689651, 17.05367660732407842 ) ) ;
#17363 = CARTESIAN_POINT ( 'NONE',  ( 164.1994273494235301, 252.5555082259370181, 13.35012251226196867 ) ) ;
#17365 = ADVANCED_FACE ( 'NONE', ( #62930 ), #639, .T. ) ;
#17366 = CARTESIAN_POINT ( 'NONE',  ( 22.11123320312891849, 195.1199935810940929, 2.679491924311251605 ) ) ;
#17367 = CARTESIAN_POINT ( 'NONE',  ( 25.79477067763620468, 36.93396525600391556, 2.839279412974139660 ) ) ;
#17368 = B_SPLINE_CURVE_WITH_KNOTS ( 'NONE', 3,
 ( #45934, #53547, #61142, #53055 ),
 .UNSPECIFIED., .F., .F.,
 ( 4, 4 ),
 ( 2.602085213965210642E-18, 0.003217767275339507987 ),
 .UNSPECIFIED. ) ;
#17369 = CARTESIAN_POINT ( 'NONE',  ( 164.4261001824251878, 245.8526357240660900, 1.583002802772015549 ) ) ;
#17370 = CARTESIAN_POINT ( 'NONE',  ( 183.2458657411818308, 257.8356223092092705, -2.282625027615983182 ) ) ;
#17371 = CARTESIAN_POINT ( 'NONE',  ( 65.84382221999611318, 68.94682728932481552, 2.365708372102203860 ) ) ;
#17372 = ORIENTED_EDGE ( 'NONE', *, *, #18775, .F. ) ;
#17373 = CARTESIAN_POINT ( 'NONE',  ( 196.9098758191317700, 289.5890858996224324, -16.54412079817003800 ) ) ;
#17374 = CARTESIAN_POINT ( 'NONE',  ( 177.9925615710933755, 254.8251403409008731, -7.350624415798725053 ) ) ;
#17375 = CARTESIAN_POINT ( 'NONE',  ( 9.553764119070452310, 20.91421378149917132, 9.188101187500008038 ) ) ;
#17376 = CARTESIAN_POINT ( 'NONE',  ( 153.2873167144811646, 277.6669624900651456, -5.602515137802061673 ) ) ;
#17377 = CARTESIAN_POINT ( 'NONE',  ( 10.20631340951632104, 27.93396525600388713, 2.839279412974139660 ) ) ;
#17378 = CARTESIAN_POINT ( 'NONE',  ( 160.5729363862711523, 252.5265111888899696, 15.95386353709229965 ) ) ;
#17379 = CARTESIAN_POINT ( 'NONE',  ( -78.10577900106846982, 54.55156729251706338, 177.5919119679930134 ) ) ;
#17380 = EDGE_LOOP ( 'NONE', ( #7564, #23813, #29276, #53758 ) ) ;
#17381 = CARTESIAN_POINT ( 'NONE',  ( 192.4202172926039793, 297.3654025762033370, 10.98569444949570872 ) ) ;
#17382 = CARTESIAN_POINT ( 'NONE',  ( 207.3502731283117555, 271.5057873089173768, 6.280625384230454245 ) ) ;
#17383 = CARTESIAN_POINT ( 'NONE',  ( 190.9015239950540206, 298.2326252366660810, 9.554377282061516041 ) ) ;
#17384 = CARTESIAN_POINT ( 'NONE',  ( 87.89265348834460667, 45.03651295921147835, 6.473805411810640287 ) ) ;
#17385 = CARTESIAN_POINT ( 'NONE',  ( 193.9204722154232741, 294.7668848255750049, 15.43855698596013859 ) ) ;
#17386 = EDGE_LOOP ( 'NONE', ( #98495, #43804, #90688, #95184, #41189, #37176, #96293, #24532, #79479, #96522, #22625, #15144, #46163, #28980, #68972, #44801, #59095, #13705, #68474, #1063 ) ) ;
#17387 = ORIENTED_EDGE ( 'NONE', *, *, #90014, .F. ) ;
#17388 = DIRECTION ( 'NONE',  ( 0.06115825522547173321, -0.9981280818701455670, 0.000000000000000000 ) ) ;
#17389 = CARTESIAN_POINT ( 'NONE',  ( 86.47451081130098771, 47.36193104714216418, 10.30071581693739624 ) ) ;
#17390 = ORIENTED_EDGE ( 'NONE', *, *, #14602, .T. ) ;
#17391 = CARTESIAN_POINT ( 'NONE',  ( 77.39735829247300103, 55.57776196096627785, 16.14182346449976180 ) ) ;
#17392 = CARTESIAN_POINT ( 'NONE',  ( 188.5527807511783180, 297.9505215649899696, 7.797827009507764195 ) ) ;
#17393 = ORIENTED_EDGE ( 'NONE', *, *, #5131, .F. ) ;
#17394 = CARTESIAN_POINT ( 'NONE',  ( 78.12740563502775615, 61.81406844543894863, -15.72119867135329407 ) ) ;
#17395 = CARTESIAN_POINT ( 'NONE',  ( 79.28344036561787789, 59.07624401938414138, -16.22551900837544281 ) ) ;
#17396 = VECTOR ( 'NONE', #73758, 999.9999999999998863 ) ;
#17397 = CARTESIAN_POINT ( 'NONE',  ( 18.32728854387591255, 18.78052372038640172, -10.00000000000000355 ) ) ;
#17398 = ORIENTED_EDGE ( 'NONE', *, *, #44947, .T. ) ;
#17399 = CARTESIAN_POINT ( 'NONE',  ( 173.7019467158212933, 267.2044448140225086, 16.95278284378356659 ) ) ;
#17400 = CARTESIAN_POINT ( 'NONE',  ( 180.3089020998223475, 294.4768193211729681, -5.541584815692371713 ) ) ;
#17401 = CIRCLE ( 'NONE', #25508, 70.00000000000001421 ) ;
#17402 = CARTESIAN_POINT ( 'NONE',  ( 127.4956995296957416, 255.9637435831425023, 2.679491924311251605 ) ) ;
#17403 = CARTESIAN_POINT ( 'NONE',  ( 191.5766842709549280, 298.8264446275616137, 8.039910086100929831 ) ) ;
#17404 = CARTESIAN_POINT ( 'NONE',  ( 151.4143897794357088, 274.9824025847329949, -8.616620037206830673 ) ) ;
#17405 = EDGE_LOOP ( 'NONE', ( #86185, #64093, #21545, #78148 ) ) ;
#17406 = CARTESIAN_POINT ( 'NONE',  ( 170.7449765318682466, 255.6388512455198736, -11.59872511109924709 ) ) ;
#17407 = PLANE ( 'NONE',  #33685 ) ;
#17408 = VERTEX_POINT ( 'NONE', #16334 ) ;
#17409 = ORIENTED_EDGE ( 'NONE', *, *, #36134, .F. ) ;
#17410 = CARTESIAN_POINT ( 'NONE',  ( 72.70390389555041111, 58.44164253163238243, 15.66496257417437654 ) ) ;
#17411 = VERTEX_POINT ( 'NONE', #70528 ) ;
#17412 = CARTESIAN_POINT ( 'NONE',  ( 88.42017002704760387, 43.92753743058676008, 1.721442031696316599 ) ) ;
#17413 = VERTEX_POINT ( 'NONE', #86295 ) ;
#17414 = CARTESIAN_POINT ( 'NONE',  ( 83.30833261233810560, 49.39214575607078217, 13.32215296955395623 ) ) ;
#17415 = CARTESIAN_POINT ( 'NONE',  ( 167.3899042128373651, 272.0936304241042194, 16.05079403648893788 ) ) ;
#17416 = CARTESIAN_POINT ( 'NONE',  ( -31.49356256989596758, 94.88921800892812541, 45.19948692389422717 ) ) ;
#17417 = CARTESIAN_POINT ( 'NONE',  ( 147.8819534105757043, 274.5079385007862811, -9.338341377131436971 ) ) ;
#17418 = CARTESIAN_POINT ( 'NONE',  ( 82.47021907082940118, 53.30441442868471569, -15.33472904691312699 ) ) ;
#17419 = CARTESIAN_POINT ( 'NONE',  ( -37.33262083840143930, 163.6868197944959036, -37.49999999999995737 ) ) ;
#17420 = VECTOR ( 'NONE', #47539, 1000.000000000000114 ) ;
#17421 = ORIENTED_EDGE ( 'NONE', *, *, #70534, .F. ) ;
#17422 = CARTESIAN_POINT ( 'NONE',  ( 5.968649350820482979, 188.6868197944959320, -37.49999999999994316 ) ) ;
#17423 = CARTESIAN_POINT ( 'NONE',  ( 14.90450122504689823, 30.64646525600389637, -2.839279412974133887 ) ) ;
#17424 = EDGE_CURVE ( 'NONE', #27867, #82530, #25430, .T. ) ;
#17425 = CARTESIAN_POINT ( 'NONE',  ( 164.2801755739368446, 246.1053845600426087, 2.518777461081745717 ) ) ;
#17426 = CARTESIAN_POINT ( 'NONE',  ( 205.7576124508049418, 274.2643565215761328, 10.88614016733041545 ) ) ;
#17428 = ORIENTED_EDGE ( 'NONE', *, *, #4714, .F. ) ;
#17427 = CARTESIAN_POINT ( 'NONE',  ( 196.4628211408765139, 276.9783169463397030, -16.67918425853740771 ) ) ;
#17429 = AXIS2_PLACEMENT_3D ( 'NONE', #94706, #32868, #63774 ) ;
#17430 = ORIENTED_EDGE ( 'NONE', *, *, #98473, .F. ) ;
#17431 = CARTESIAN_POINT ( 'NONE',  ( 190.6843051365801784, 300.3720906279131100, 5.205712306949425106 ) ) ;
#17432 = DIRECTION ( 'NONE',  ( 0.000000000000000000, 0.000000000000000000, 1.000000000000000000 ) ) ;
#17433 = CARTESIAN_POINT ( 'NONE',  ( 206.7893622945242385, 272.4773133715531230, -10.52881283832460291 ) ) ;
#17434 = DIRECTION ( 'NONE',  ( 1.000000000000000000, 0.000000000000000000, 0.000000000000000000 ) ) ;
#17435 = EDGE_CURVE ( 'NONE', #5666, #82885, #2149, .T. ) ;
#17436 = CARTESIAN_POINT ( 'NONE',  ( 161.3193951073452581, 251.2336067582368742, 13.01220207292984377 ) ) ;
#17437 = CARTESIAN_POINT ( 'NONE',  ( 190.8369279865719932, 261.8867820640782043, -0.3648464445779296406 ) ) ;
#17438 = ORIENTED_EDGE ( 'NONE', *, *, #63482, .T. ) ;
#17439 = CARTESIAN_POINT ( 'NONE',  ( 167.2609760701786570, 252.9900861492237425, -12.15359341202019117 ) ) ;
#17440 = CARTESIAN_POINT ( 'NONE',  ( -19.65312891409030271, 93.06504152958497400, 177.5919119679930134 ) ) ;
#17441 = AXIS2_PLACEMENT_3D ( 'NONE', #52341, #83283, #13370 ) ;
#17442 = CARTESIAN_POINT ( 'NONE',  ( 75.05448840609841454, 66.98218832618681517, -13.15900604923073480 ) ) ;
#17444 = EDGE_CURVE ( 'NONE', #25006, #98353, #79180, .T. ) ;
#17443 = DIRECTION ( 'NONE',  ( 0.000000000000000000, 0.000000000000000000, 1.000000000000000000 ) ) ;
#17445 = CARTESIAN_POINT ( 'NONE',  ( 23.67544375150423619, 171.1427522451417644, 1.119607411625061291E-15 ) ) ;
#17446 = CARTESIAN_POINT ( 'NONE',  ( 95.22211873877631660, 213.5327760586659451, 1.948934522072302763E-15 ) ) ;
#17447 = CARTESIAN_POINT ( 'NONE',  ( 82.59121451996566066, 40.53000206385964788, -1.428901709462959468 ) ) ;
#17448 = CARTESIAN_POINT ( 'NONE',  ( 26.60956029314639082, 56.97371141178327747, 59.99999999999999289 ) ) ;
#17449 = CARTESIAN_POINT ( 'NONE',  ( 169.8363984463651377, 280.1429775057247298, -13.61031055851517557 ) ) ;
#17451 = CARTESIAN_POINT ( 'NONE',  ( 75.58531661750802755, 65.25623013732912625, 14.34312269817976571 ) ) ;
#17450 = CARTESIAN_POINT ( 'NONE',  ( 5.777845730223497789, 164.9548013555410080, -4.594050593750042211 ) ) ;
#17452 = CARTESIAN_POINT ( 'NONE',  ( 161.2799361541916028, 251.3019516699124836, 14.40628917569557110 ) ) ;
#17453 = ORIENTED_EDGE ( 'NONE', *, *, #78170, .T. ) ;
#17454 = ORIENTED_EDGE ( 'NONE', *, *, #41816, .T. ) ;
#17455 = CARTESIAN_POINT ( 'NONE',  ( 200.2433557449332682, 267.4156030511788344, -2.849737501924599403 ) ) ;
#17456 = DIRECTION ( 'NONE',  ( -0.8660254037844379305, -0.5000000000000014433, -0.000000000000000000 ) ) ;
#17457 = CARTESIAN_POINT ( 'NONE',  ( 22.94593010929795085, 36.18080186712593616, 3.090169943749475401 ) ) ;
#17458 = CARTESIAN_POINT ( 'NONE',  ( 40.86965645935567437, 187.7365022471901739, -10.00000000000009237 ) ) ;
#17459 = CARTESIAN_POINT ( 'NONE',  ( -57.88150100324660485, 35.92665207732902388, 10.00000000000000000 ) ) ;
#17460 = CARTESIAN_POINT ( 'NONE',  ( -13.11024591527734628, 15.00000000000000000, 32.50000000000000000 ) ) ;
#17461 = CARTESIAN_POINT ( 'NONE',  ( 28.53781555160951555, 187.2833772461660544, -9.188101187500095079 ) ) ;
#17462 = CARTESIAN_POINT ( 'NONE',  ( 81.77131458871032521, 208.0177522451417929, 5.000000000000051514 ) ) ;
#17463 = CIRCLE ( 'NONE', #99987, 15.50000000000000000 ) ;
#17464 = CYLINDRICAL_SURFACE ( 'NONE', #28555, 70.00000000000002842 ) ;
#17465 = VERTEX_POINT ( 'NONE', #40618 ) ;
#17466 = CARTESIAN_POINT ( 'NONE',  ( 83.13189617009490462, 45.21769814841992030, 9.926785792809118547 ) ) ;
#17467 = DIRECTION ( 'NONE',  ( 0.8660254037844303809, 0.5000000000000144329, 0.000000000000000000 ) ) ;
#17468 = VECTOR ( 'NONE', #55799, 1000.000000000000114 ) ;
#17469 = CARTESIAN_POINT ( 'NONE',  ( -4.722712290662820500, 158.8923013555410080, 4.594050593750050204 ) ) ;
#17470 = AXIS2_PLACEMENT_3D ( 'NONE', #45629, #52247, #97386 ) ;
#17471 = CARTESIAN_POINT ( 'NONE',  ( 68.69421868117841257, 64.67178190514665914, -12.16033057019549801 ) ) ;
#17472 = CARTESIAN_POINT ( 'NONE',  ( 207.1211793645798878, 271.9025893473983047, -6.294110402770905388 ) ) ;
#17473 = DIRECTION ( 'NONE',  ( -0.8660254037844378194, -0.5000000000000014433, -0.000000000000000000 ) ) ;
#17474 = CARTESIAN_POINT ( 'NONE',  ( 194.3708539535661259, 293.9868007723104029, -16.01585187499628304 ) ) ;
#17475 = EDGE_CURVE ( 'NONE', #39911, #41051, #63436, .T. ) ;
#17476 = DIRECTION ( 'NONE',  ( -0.4999999999999987788, 0.8660254037844392627, 0.000000000000000000 ) ) ;
#17477 = CARTESIAN_POINT ( 'NONE',  ( 164.2059258710715994, 246.2339888178522926, 7.329631442356459914 ) ) ;
#17478 = CARTESIAN_POINT ( 'NONE',  ( 191.0478321355427624, 299.7424433957868928, -9.006798842970001218 ) ) ;
#17479 = CARTESIAN_POINT ( 'NONE',  ( 148.0427192501136062, 274.2294838985851015, 9.385226820296049155 ) ) ;
#17480 = ORIENTED_EDGE ( 'NONE', *, *, #89306, .F. ) ;
#17481 = B_SPLINE_CURVE_WITH_KNOTS ( 'NONE', 3,
 ( #28356, #20782, #82622, #44041, #74981, #36451, #88234, #85093, #38440, #52643, #75991, #14164 ),
 .UNSPECIFIED., .F., .F.,
 ( 4, 2, 2, 2, 2, 4 ),
 ( 0.000000000000000000, 0.1860970332708319352, 0.2791455499062492351, 0.3721940665416665350, 0.5582910998124992474, 0.7443881330833320709 ),
 .UNSPECIFIED. ) ;
#17482 = CARTESIAN_POINT ( 'NONE',  ( 208.1757572214753793, 270.0760069187178374, 2.172546422564154867 ) ) ;
#17483 = CARTESIAN_POINT ( 'NONE',  ( 110.3772162092389948, 234.5333772461660828, 9.188101187500095079 ) ) ;
#17484 = CARTESIAN_POINT ( 'NONE',  ( 23.64951029700315743, 14.44966523072494624, -2.296566073217252530E-15 ) ) ;
#17485 = CARTESIAN_POINT ( 'NONE',  ( 75.27726335905293809, 66.87231400452490959, 13.31561030640130916 ) ) ;
#17486 = EDGE_CURVE ( 'NONE', #42311, #5196, #39608, .T. ) ;
#17487 = CARTESIAN_POINT ( 'NONE',  ( 78.33954679865345838, 57.47496213173443635, -16.60598043669875068 ) ) ;
#17488 = AXIS2_PLACEMENT_3D ( 'NONE', #69480, #583, #47668 ) ;
#17490 = CARTESIAN_POINT ( 'NONE',  ( 200.1133476818314705, 272.1141633677412415, 12.87458617912082914 ) ) ;
#17489 = CARTESIAN_POINT ( 'NONE',  ( 157.0957870390718369, 258.5491105237443321, 17.69218919045495397 ) ) ;
#17491 = CARTESIAN_POINT ( 'NONE',  ( 204.5028199768381398, 272.8749048982307954, -9.750091098900030673 ) ) ;
#17492 = B_SPLINE_CURVE_WITH_KNOTS ( 'NONE', 3,
 ( #99386, #55242, #15751, #30958 ),
 .UNSPECIFIED., .F., .F.,
 ( 4, 4 ),
 ( 0.008069797487559298571, 0.01626517688446255105 ),
 .UNSPECIFIED. ) ;
#17493 = CARTESIAN_POINT ( 'NONE',  ( -22.42236680055709641, 157.8615022471902591, 0.000000000000000000 ) ) ;
#17494 = CARTESIAN_POINT ( 'NONE',  ( 196.2293283710122012, 290.7678286567270902, -17.07152402978540096 ) ) ;
#17495 = CARTESIAN_POINT ( 'NONE',  ( 82.05544088639145173, 41.12520979201238447, -3.426473099821476964 ) ) ;
#17496 = CARTESIAN_POINT ( 'NONE',  ( 172.6105268277075311, 290.6563111985113892, -1.849890294009189251 ) ) ;
#17497 = FACE_OUTER_BOUND ( 'NONE', #67890, .T. ) ;
#17498 = VERTEX_POINT ( 'NONE', #143 ) ;
#17499 = CARTESIAN_POINT ( 'NONE',  ( -33.66737166714137430, 24.21715323669988607, 10.00000000000000000 ) ) ;
#17500 = CARTESIAN_POINT ( 'NONE',  ( 17.39660613652184296, 31.81751292744056059, -6.180339887498951690 ) ) ;
#17501 = CARTESIAN_POINT ( 'NONE',  ( 189.5599828453989346, 263.0657735508838186, -9.804501003715218488 ) ) ;
#17502 = ORIENTED_EDGE ( 'NONE', *, *, #26815, .F. ) ;
#17503 = CARTESIAN_POINT ( 'NONE',  ( 84.90716433703735788, 44.17344321180959099, 8.036067867235411555 ) ) ;
#17504 = DIRECTION ( 'NONE',  ( -0.000000000000000000, 0.000000000000000000, -1.000000000000000000 ) ) ;
#17505 = LINE ( 'NONE', #40784, #80908 ) ;
#17506 = CARTESIAN_POINT ( 'NONE',  ( 152.7314557461996571, 266.1083540640618708, 17.39314074348802208 ) ) ;
#17507 = VECTOR ( 'NONE', #77136, 1000.000000000000000 ) ;
#17508 = ORIENTED_EDGE ( 'NONE', *, *, #28836, .F. ) ;
#17509 = CARTESIAN_POINT ( 'NONE',  ( 163.2523617031003482, 269.8851863420952668, -17.32811968646028689 ) ) ;
#17510 = CARTESIAN_POINT ( 'NONE',  ( 39.71190250773520347, 34.87878583063844928, -9.188101187500006262 ) ) ;
#17511 = CARTESIAN_POINT ( 'NONE',  ( 195.3339445956660256, 290.3114242235789675, -16.63067108908084535 ) ) ;
#17512 = ORIENTED_EDGE ( 'NONE', *, *, #76595, .T. ) ;
#17513 = CARTESIAN_POINT ( 'NONE',  ( 163.7954642885384544, 279.4399783988836248, 12.25154076785413082 ) ) ;
#17514 = DIRECTION ( 'NONE',  ( -0.4805540241036398430, -0.8769651246872924855, 0.000000000000000000 ) ) ;
#17515 = CARTESIAN_POINT ( 'NONE',  ( 20.87890338866488804, 172.8615022471901739, 5.000000000000051514 ) ) ;
#17516 = ORIENTED_EDGE ( 'NONE', *, *, #88072, .T. ) ;
#17517 = CARTESIAN_POINT ( 'NONE',  ( 79.53039288183295241, 59.52037319582147035, 16.54552321433124007 ) ) ;
#17518 = CARTESIAN_POINT ( 'NONE',  ( 188.7491163893556347, 293.7278928144251040, 12.91049369769965516 ) ) ;
#17519 = CARTESIAN_POINT ( 'NONE',  ( 83.99043920266019825, 44.44647294453730524, -9.181167553117798974 ) ) ;
#17520 = CARTESIAN_POINT ( 'NONE',  ( 75.64058981421790406, 52.75146229252735708, -15.94971674686773611 ) ) ;
#17521 = CARTESIAN_POINT ( 'NONE',  ( 84.78071699792324978, 50.02262005461608396, -13.67739062443489750 ) ) ;
#17522 = CARTESIAN_POINT ( 'NONE',  ( 155.0304386007204016, 262.1263989543018056, -17.12961552904782181 ) ) ;
#17523 = ORIENTED_EDGE ( 'NONE', *, *, #63482, .F. ) ;
#17524 = VERTEX_POINT ( 'NONE', #1145 ) ;
#17525 = DIRECTION ( 'NONE',  ( -0.3535533905932676246, 0.6123724356957830350, -0.7071067811865604513 ) ) ;
#17526 = ORIENTED_EDGE ( 'NONE', *, *, #75938, .T. ) ;
#17527 = CARTESIAN_POINT ( 'NONE',  ( 77.14781257410808735, 49.36774166773431460, -15.41843211982917339 ) ) ;
#17528 = VERTEX_POINT ( 'NONE', #93882 ) ;
#17529 = CARTESIAN_POINT ( 'NONE',  ( 74.46907260258244321, 56.36757137110866722, 16.09080421635434632 ) ) ;
#17530 = CARTESIAN_POINT ( 'NONE',  ( 78.49844428082862180, 50.04128099798806772, 14.89165427517412077 ) ) ;
#17531 = ORIENTED_EDGE ( 'NONE', *, *, #20706, .T. ) ;
#17532 = ADVANCED_BREP_SHAPE_REPRESENTATION ( '', ( #77374, #68784 ), #36458 ) ;
#17533 = CARTESIAN_POINT ( 'NONE',  ( 206.7127649687076314, 272.6099838315917623, -10.35326570309970506 ) ) ;
#17534 = CARTESIAN_POINT ( 'NONE',  ( 190.5255224008060395, 300.6471103936386271, 2.040674304113719639 ) ) ;
#17535 = DIRECTION ( 'NONE',  ( -0.000000000000000000, -0.000000000000000000, -1.000000000000000000 ) ) ;
#17536 = CARTESIAN_POINT ( 'NONE',  ( 192.4172326059820648, 297.3705722050773943, -12.52563289807247848 ) ) ;
#17537 = VECTOR ( 'NONE', #29031, 999.9999999999998863 ) ;
#17538 = CARTESIAN_POINT ( 'NONE',  ( 201.1755594471486859, 282.2007051268825535, -18.15567516623250910 ) ) ;
#17539 = CARTESIAN_POINT ( 'NONE',  ( -19.65312891409030271, 93.06504152958497400, 177.5919119679930134 ) ) ;
#17541 = CARTESIAN_POINT ( 'NONE',  ( 157.8706589075648310, 280.9451892264036132, 2.094144116980718451 ) ) ;
#17540 = VECTOR ( 'NONE', #52128, 1000.000000000000000 ) ;
#17542 = CARTESIAN_POINT ( 'NONE',  ( 123.8274129399422918, 251.4869531367911577, 4.594050593750046652 ) ) ;
#17543 = CARTESIAN_POINT ( 'NONE',  ( 75.92249805096321325, 55.87144976864329493, 16.14995706910994500 ) ) ;
#17544 = CARTESIAN_POINT ( 'NONE',  ( 38.63056705113294953, 37.70171378149921537, -9.188101187500004485 ) ) ;
#17545 = AXIS2_PLACEMENT_3D ( 'NONE', #34973, #90230, #36971 ) ;
#17546 = VERTEX_POINT ( 'NONE', #85805 ) ;
#17547 = EDGE_CURVE ( 'NONE', #86867, #11833, #57467, .T. ) ;
#17548 = VECTOR ( 'NONE', #28512, 1000.000000000000000 ) ;
#17550 = ORIENTED_EDGE ( 'NONE', *, *, #781, .F. ) ;
#17549 = DIRECTION ( 'NONE',  ( -0.9646071681523453734, 0.2636911283094537373, 0.000000000000000000 ) ) ;
#17551 = CARTESIAN_POINT ( 'NONE',  ( 203.6078461682101590, 276.3159402255348027, 13.42158206181595048 ) ) ;
#17552 = CARTESIAN_POINT ( 'NONE',  ( 177.8946713442994678, 253.3491511510508190, 1.398846671321700486 ) ) ;
#17553 = EDGE_CURVE ( 'NONE', #18450, #48481, #55802, .T. ) ;
#17554 = CARTESIAN_POINT ( 'NONE',  ( 172.6012549852709412, 290.2025030293380610, -5.021894074213228087 ) ) ;
#17555 = CARTESIAN_POINT ( 'NONE',  ( 192.8302070313391141, 296.6552795181322608, 12.00067902349765880 ) ) ;
#17556 = CARTESIAN_POINT ( 'NONE',  ( 70.74512962697180285, 71.93581810439270896, 1.182017065394330935 ) ) ;
#17557 = DIRECTION ( 'NONE',  ( -0.3177184104407523302, 0.9481851146622169990, 0.000000000000000000 ) ) ;
#17558 = CARTESIAN_POINT ( 'NONE',  ( 176.7740879285838389, 288.5420746471101552, -9.314761950507488564 ) ) ;
#17559 = CARTESIAN_POINT ( 'NONE',  ( 193.4225248517565774, 292.8543354191958201, -14.39945119728164435 ) ) ;
#17560 = CARTESIAN_POINT ( 'NONE',  ( 177.2273226362962362, 256.0984073744629086, -7.379249422943265024 ) ) ;
#17561 = ORIENTED_EDGE ( 'NONE', *, *, #56103, .T. ) ;
#17562 = CARTESIAN_POINT ( 'NONE',  ( 148.0346525705264469, 274.2434557974783615, -9.381294579651672905 ) ) ;
#17563 = LINE ( 'NONE', #95114, #83610 ) ;
#17564 = EDGE_LOOP ( 'NONE', ( #6324, #601, #55047, #88397 ) ) ;
#17566 = EDGE_CURVE ( 'NONE', #61138, #5695, #31028, .T. ) ;
#17565 = CARTESIAN_POINT ( 'NONE',  ( 163.0656072001963537, 277.9852329471388543, 13.74753899820123415 ) ) ;
#17567 = CARTESIAN_POINT ( 'NONE',  ( 26.37028381016232004, 40.32183835407518302, -10.00000000000000000 ) ) ;
#17568 = CARTESIAN_POINT ( 'NONE',  ( 192.1435947104413913, 297.8445269430296776, -9.754524473716664090 ) ) ;
#17569 = CARTESIAN_POINT ( 'NONE',  ( 148.9230895364621574, 272.7046378331555161, 12.20434325797056019 ) ) ;
#17570 = CARTESIAN_POINT ( 'NONE',  ( 162.6626107288841467, 248.9070890562113902, 10.12509462564867313 ) ) ;
#17572 = CARTESIAN_POINT ( 'NONE',  ( 160.5520610138454458, 282.2019950894995759, 6.659617355605994327 ) ) ;
#17571 = CARTESIAN_POINT ( 'NONE',  ( 153.4735438756679002, 270.0204785379407326, 14.29634556544180235 ) ) ;
#17573 = CARTESIAN_POINT ( 'NONE',  ( 152.7729059155601021, 266.0365602647466972, -17.50667083025758686 ) ) ;
#17574 = ORIENTED_EDGE ( 'NONE', *, *, #56421, .T. ) ;
#17575 = CARTESIAN_POINT ( 'NONE',  ( 163.1033070407499110, 249.6811796723388852, -11.57508889205896274 ) ) ;
#17576 = PRODUCT_DEFINITION_SHAPE ( 'NONE', 'NONE',  #3701 ) ;
#17577 = CARTESIAN_POINT ( 'NONE',  ( 186.9555558246591431, 262.3224090832389379, -8.686013347077395252 ) ) ;
#17578 = DIRECTION ( 'NONE',  ( 0.5000000000000048850, -0.8660254037844358210, 0.000000000000000000 ) ) ;
#17579 = CARTESIAN_POINT ( 'NONE',  ( -22.42236680055709641, 157.8615022471902591, 0.000000000000000000 ) ) ;
#17580 = EDGE_CURVE ( 'NONE', #68024, #20256, #37022, .T. ) ;
#17581 = CARTESIAN_POINT ( 'NONE',  ( 184.6438136528588529, 297.2564992327004916, -4.482047658127568113 ) ) ;
#17582 = EDGE_CURVE ( 'NONE', #1108, #53329, #84083, .T. ) ;
#17583 = CARTESIAN_POINT ( 'NONE',  ( 201.1893450866852504, 280.1768276987904756, -16.82388990131531870 ) ) ;
#17584 = DIRECTION ( 'NONE',  ( 0.4829524219151267173, -0.8756465943326184886, 0.000000000000000000 ) ) ;
#17585 = CARTESIAN_POINT ( 'NONE',  ( -11.23620533500811725, 170.9865022471903444, -10.00000000000009592 ) ) ;
#17586 = CARTESIAN_POINT ( 'NONE',  ( 69.18172419252286431, 70.58912176915313808, -0.05407004869426973448 ) ) ;
#17587 = CARTESIAN_POINT ( 'NONE',  ( -6.265406815095104776, 161.0643266524159856, 9.188101187500095079 ) ) ;
#17588 = CARTESIAN_POINT ( 'NONE',  ( 88.48327179163739231, 212.7048013555409796, 4.594050593750051981 ) ) ;
#17589 = CARTESIAN_POINT ( 'NONE',  ( 26.05470188313195123, 197.3967562850347122, -4.648177544792955347E-16 ) ) ;
#17590 = CARTESIAN_POINT ( 'NONE',  ( 87.91732953454810229, 44.48954743135376333, -3.956250123475848923 ) ) ;
#17591 = CARTESIAN_POINT ( 'NONE',  ( 182.8190671368951428, 294.1949347170434521, -7.963347553794334566 ) ) ;
#17592 = CARTESIAN_POINT ( 'NONE',  ( -12.03006195514386434, 173.8615022471903160, 5.000000000000046185 ) ) ;
#17593 = CARTESIAN_POINT ( 'NONE',  ( 78.70150085959764397, 59.83202584994826623, 16.12694553795978081 ) ) ;
#17594 = CARTESIAN_POINT ( 'NONE',  ( 78.14496974547672892, 61.87975766354972507, 15.71822119279614149 ) ) ;
#17596 = CARTESIAN_POINT ( 'NONE',  ( 76.61485521235918839, 51.34506894449801706, 16.06955735627100879 ) ) ;
#17595 = CARTESIAN_POINT ( 'NONE',  ( 67.00187114335926708, 67.08813303282481399, 8.529924657355552498 ) ) ;
#17597 = CARTESIAN_POINT ( 'NONE',  ( 161.9469964850341626, 250.1465692851796518, 14.00188699914706092 ) ) ;
#17598 = EDGE_CURVE ( 'NONE', #97734, #29236, #1873, .T. ) ;
#17599 = CARTESIAN_POINT ( 'NONE',  ( 169.2574381869089564, 252.1335231699163160, -8.836137456772515719 ) ) ;
#17600 = CARTESIAN_POINT ( 'NONE',  ( 164.3378896953848596, 246.0054207693806063, -5.823270600575261469 ) ) ;
#17601 = DIRECTION ( 'NONE',  ( 0.5000000000000002220, -0.8660254037844387076, -0.000000000000000000 ) ) ;
#17602 = DIRECTION ( 'NONE',  ( -0.6123724356958113457, -0.3535533905932644605, -0.7071067811865376918 ) ) ;
#17603 = B_SPLINE_CURVE_WITH_KNOTS ( 'NONE', 3,
 ( #90978, #83366, #52922, #5830, #21538, #52421, #67624, #30123, #99049, #37710, #59511, #13932, #45317, #68618, #14436, #36223, #44811, #91461, #61005, #14913, #67125, #36720, #53416, #59005, #98049, #12963, #75748, #76252, #99541, #6331, #68121 ),
 .UNSPECIFIED., .F., .F.,
 ( 4, 3, 3, 3, 3, 3, 3, 3, 3, 3, 4 ),
 ( 0.000000000000000000, 3.357709145156238112E-05, 6.715417940116638184E-05, 0.0001007313198657320137, 0.0001343084960840525556, 0.0001678856156954656629, 0.0002014626747008688135, 0.0002350397637044835341, 0.0002686169264846348381, 0.0003021940916574198136, 0.0003125816342522854925 ),
 .UNSPECIFIED. ) ;
#17604 = CARTESIAN_POINT ( 'NONE',  ( 73.46598367719339251, 69.88918780369783690, 9.751349427452053575 ) ) ;
#17605 = EDGE_CURVE ( 'NONE', #80767, #91193, #57817, .T. ) ;
#17606 = CARTESIAN_POINT ( 'NONE',  ( 30.18841615574984516, 197.4244531367911293, -4.594050593750046652 ) ) ;
#17607 = CARTESIAN_POINT ( 'NONE',  ( 175.1616093908759240, 264.7739651183366618, -16.67648531822408486 ) ) ;
#17608 = VECTOR ( 'NONE', #94989, 1000.000000000000000 ) ;
#17609 = CARTESIAN_POINT ( 'NONE',  ( 64.39641960523518094, 217.1744531367911293, 4.594050593750047540 ) ) ;
#17610 = CARTESIAN_POINT ( 'NONE',  ( 164.5641499066685469, 246.8022252770303169, -5.664862832761055955 ) ) ;
#17611 = CARTESIAN_POINT ( 'NONE',  ( 88.33319108017924748, 44.17511578188309329, 0.3281601038862981268 ) ) ;
#17612 = AXIS2_PLACEMENT_3D ( 'NONE', #87460, #26085, #10387 ) ;
#17613 = EDGE_CURVE ( 'NONE', #92966, #56021, #61048, .T. ) ;
#17614 = CARTESIAN_POINT ( 'NONE',  ( 166.2779816807986322, 259.4367366842961360, 15.68628669229216932 ) ) ;
#17616 = CYLINDRICAL_SURFACE ( 'NONE', #15037, 17.82106496071139645 ) ;
#17615 = LINE ( 'NONE', #79952, #67872 ) ;
#17617 = VECTOR ( 'NONE', #39211, 1000.000000000000000 ) ;
#17618 = CARTESIAN_POINT ( 'NONE',  ( 176.5628964405708530, 270.0282015820967558, -17.29816915654511078 ) ) ;
#17619 = EDGE_CURVE ( 'NONE', #92966, #61965, #19991, .T. ) ;
#17620 = CARTESIAN_POINT ( 'NONE',  ( 24.77416059058194264, 29.70171378149920471, -9.188101187500004485 ) ) ;
#17621 = DIRECTION ( 'NONE',  ( -0.000000000000000000, -0.000000000000000000, -1.000000000000000000 ) ) ;
#17622 = CARTESIAN_POINT ( 'NONE',  ( 148.9322735291567597, 272.6887306911919495, -12.40988026045598858 ) ) ;
#17623 = ORIENTED_EDGE ( 'NONE', *, *, #78688, .T. ) ;
#17624 = CARTESIAN_POINT ( 'NONE',  ( 21.77916244986271366, 18.28920272979926764, -7.433330006724141015 ) ) ;
#17625 = CARTESIAN_POINT ( 'NONE',  ( 71.43287601098374751, 221.2369531367911293, -4.594050593750048428 ) ) ;
#17626 = LINE ( 'NONE', #11038, #41618 ) ;
#17627 = AXIS2_PLACEMENT_3D ( 'NONE', #51528, #28225, #92074 ) ;
#17628 = CARTESIAN_POINT ( 'NONE',  ( 172.6035724952978967, 290.6552710437545670, -0.3907579110097771369 ) ) ;
#17629 = CARTESIAN_POINT ( 'NONE',  ( 74.23220016013017641, 67.58394823275320107, 11.88963712537928963 ) ) ;
#17630 = CARTESIAN_POINT ( 'NONE',  ( 154.0650720908321034, 263.7984627973538068, 16.93260884073979966 ) ) ;
#17631 = EDGE_CURVE ( 'NONE', #54122, #49104, #18939, .T. ) ;
#17632 = ORIENTED_EDGE ( 'NONE', *, *, #17040, .F. ) ;
#17633 = CARTESIAN_POINT ( 'NONE',  ( 168.2820353728258738, 287.7095463320123940, -5.019694092131335772 ) ) ;
#17635 = CARTESIAN_POINT ( 'NONE',  ( 87.49549730082159726, 45.05290463331818529, -6.101382655908043517 ) ) ;
#17634 = CIRCLE ( 'NONE', #1442, 70.00000000000001421 ) ;
#17637 =( BOUNDED_CURVE ( )  B_SPLINE_CURVE ( 2, ( #44872, #90033, #97622, #59062, #29689, #52479, #6396, #74326, #36782 ),
 .UNSPECIFIED., .F., .T. ) 
 B_SPLINE_CURVE_WITH_KNOTS ( ( 3, 2, 2, 2, 3 ),
 ( 0.4556451612903225645, 0.4569892473118279397, 0.4596774193548386900, 0.4623655913978494403, 0.4637096774193548154 ),
 .UNSPECIFIED. ) 
 CURVE ( )  GEOMETRIC_REPRESENTATION_ITEM ( )  RATIONAL_B_SPLINE_CURVE ( ( 0.9330127018922194093, 0.9330127018922194093, 1.000000000000000000, 0.8660254037844387076, 1.000000000000000000, 0.8660254037844387076, 1.000000000000000000, 0.9330127018922194093, 0.9330127018922194093 ) ) 
 REPRESENTATION_ITEM ( '' )  );
#17636 = CARTESIAN_POINT ( 'NONE',  ( 126.4618338667177113, 230.4865022471901170, 1.119607411625061291E-15 ) ) ;
#17638 = CARTESIAN_POINT ( 'NONE',  ( 15.95338390109293059, 180.0177522451418497, -10.00000000000009592 ) ) ;
#17639 = CARTESIAN_POINT ( 'NONE',  ( 75.15133516359631471, 53.27350175670123633, 16.03037545075837755 ) ) ;
#17640 = ORIENTED_EDGE ( 'NONE', *, *, #1316, .F. ) ;
#17641 = CARTESIAN_POINT ( 'NONE',  ( 82.15897249015579007, 54.19038615186607188, 15.63353333787036092 ) ) ;
#17642 = ORIENTED_EDGE ( 'NONE', *, *, #5236, .F. ) ;
#17643 = CARTESIAN_POINT ( 'NONE',  ( 202.3425522658138505, 280.1794142728863903, 15.86053073629060961 ) ) ;
#17644 = CARTESIAN_POINT ( 'NONE',  ( -22.42236680055709641, 157.8615022471902591, 0.000000000000000000 ) ) ;
#17645 = CYLINDRICAL_SURFACE ( 'NONE', #59607, 17.82106496071139645 ) ;
#17646 = VERTEX_POINT ( 'NONE', #97844 ) ;
#17647 = CARTESIAN_POINT ( 'NONE',  ( 175.9795468396543185, 253.0532177342393254, -0.2546238855235851140 ) ) ;
#17648 = ORIENTED_EDGE ( 'NONE', *, *, #85806, .T. ) ;
#17649 = DIRECTION ( 'NONE',  ( 0.1172721027424030449, 0.9930998207221544138, 0.000000000000000000 ) ) ;
#17650 = CARTESIAN_POINT ( 'NONE',  ( 170.6815359018025333, 250.4067295894952281, 3.251190589082308513 ) ) ;
#17651 = CARTESIAN_POINT ( 'NONE',  ( 148.5271690325042186, 274.6709829484061061, 7.673052289842670071 ) ) ;
#17652 = VECTOR ( 'NONE', #32429, 1000.000000000000000 ) ;
#17653 = ORIENTED_EDGE ( 'NONE', *, *, #60759, .T. ) ;
#17654 = CARTESIAN_POINT ( 'NONE',  ( 30.88926192328758802, 20.76004757982090609, 5.678558825948272215 ) ) ;
#17655 = CARTESIAN_POINT ( 'NONE',  ( 79.98196094458992889, 44.41873343662761897, 11.61139898969204332 ) ) ;
#17656 = CARTESIAN_POINT ( 'NONE',  ( 74.91863663735624357, 66.38413888100485849, -13.07019282884168554 ) ) ;
#17657 = CARTESIAN_POINT ( 'NONE',  ( -70.92467617367975663, 45.40763453331954480, -10.00000000000000000 ) ) ;
#17658 = CARTESIAN_POINT ( 'NONE',  ( 167.9209307024295583, 276.8122465436554762, 15.57331525377104775 ) ) ;
#17659 = FACE_OUTER_BOUND ( 'NONE', #47957, .T. ) ;
#17660 = EDGE_LOOP ( 'NONE', ( #28896, #78326, #37607, #9563 ) ) ;
#17661 = ORIENTED_EDGE ( 'NONE', *, *, #30024, .F. ) ;
#17662 = CARTESIAN_POINT ( 'NONE',  ( 183.3830520126487329, 295.9076832148600147, 1.011780174870672511 ) ) ;
#17664 = CARTESIAN_POINT ( 'NONE',  ( 147.9500839974939197, 274.3899328626944225, -9.375093207164509224 ) ) ;
#17663 = CARTESIAN_POINT ( 'NONE',  ( 67.74658028437072232, 65.68527340592420671, 10.74595957982673333 ) ) ;
#17665 = FACE_OUTER_BOUND ( 'NONE', #48262, .T. ) ;
#17666 = CARTESIAN_POINT ( 'NONE',  ( 193.9204722154232741, 294.7668848255750049, 15.43855698596013859 ) ) ;
#17667 = CARTESIAN_POINT ( 'NONE',  ( 70.62151858337061583, 71.87035307724539734, -0.9651809227819526660 ) ) ;
#17668 = CARTESIAN_POINT ( 'NONE',  ( 205.4103625296683617, 274.8658110279089897, -13.38953657917851814 ) ) ;
#17669 = CARTESIAN_POINT ( 'NONE',  ( 208.0418200135015923, 270.3079929679526572, -4.942760474469149123 ) ) ;
#17670 = CARTESIAN_POINT ( 'NONE',  ( 206.4325537506903459, 270.6027761474677504, 2.448701755339154129 ) ) ;
#17671 = CARTESIAN_POINT ( 'NONE',  ( -30.95603806669010538, 23.98360954755322183, 10.00000000000000000 ) ) ;
#17672 = CARTESIAN_POINT ( 'NONE',  ( 77.06204113558260360, 224.4869531367911293, 4.594050593750046652 ) ) ;
#17673 = ORIENTED_EDGE ( 'NONE', *, *, #90442, .T. ) ;
#17674 = CARTESIAN_POINT ( 'NONE',  ( 151.4384131719918685, 268.3479694989391078, 14.98299707687648841 ) ) ;
#17675 = CARTESIAN_POINT ( 'NONE',  ( 78.04364300777291419, 61.42399649461658129, -16.16113552180852508 ) ) ;
#17676 = ORIENTED_EDGE ( 'NONE', *, *, #56017, .T. ) ;
#17677 = CARTESIAN_POINT ( 'NONE',  ( 195.4464213238641150, 292.1238634399910552, -17.06481037329052342 ) ) ;
#17678 = ORIENTED_EDGE ( 'NONE', *, *, #76938, .F. ) ;
#17679 = ORIENTED_EDGE ( 'NONE', *, *, #96554, .F. ) ;
#17680 = CARTESIAN_POINT ( 'NONE',  ( 80.04842081486408745, 44.52432947382052220, -11.67065558011785598 ) ) ;
#17681 = DIRECTION ( 'NONE',  ( 0.3037402332698194707, 0.8935232438716381731, 0.3306933373297694656 ) ) ;
#17682 = CARTESIAN_POINT ( 'NONE',  ( 191.5893301551938350, 298.8045413135534432, -8.323356515452589477 ) ) ;
#17683 = CARTESIAN_POINT ( 'NONE',  ( 84.28420018112215928, 42.01594207371087464, -1.269366431083392754 ) ) ;
#17684 = CARTESIAN_POINT ( 'NONE',  ( 80.77687203815185057, 48.27074620053196696, -13.47869067257540188 ) ) ;
#17685 = CARTESIAN_POINT ( 'NONE',  ( 208.0366075493969902, 270.3170212206142082, 1.570844709476715284 ) ) ;
#17686 = CARTESIAN_POINT ( 'NONE',  ( 99.63334886536203783, 219.1423013555409796, -4.594050593750043987 ) ) ;
#17687 = VERTEX_POINT ( 'NONE', #82679 ) ;
#17688 = ORIENTED_EDGE ( 'NONE', *, *, #43573, .F. ) ;
#17689 = CARTESIAN_POINT ( 'NONE',  ( 162.7459776558209228, 248.7626933030860812, -9.895605163646791880 ) ) ;
#17690 = ORIENTED_EDGE ( 'NONE', *, *, #21120, .F. ) ;
#17691 = EDGE_CURVE ( 'NONE', #28238, #87428, #2700, .T. ) ;
#17692 = VECTOR ( 'NONE', #93192, 1000.000000000000000 ) ;
#17693 = B_SPLINE_CURVE_WITH_KNOTS ( 'NONE', 3,
 ( #55801, #1142, #16826, #71552, #64437, #93878, #47714, #40114, #86794, #33028, #48749, #47226, #17328, #94867, #25428, #70525 ),
 .UNSPECIFIED., .F., .F.,
 ( 4, 1, 2, 2, 2, 1, 2, 2, 4 ),
 ( 0.000000000000000000, 0.1250000000000061340, 0.1875000000000072442, 0.2500000000000083822, 0.5000000000000089928, 0.6250000000000093259, 0.6875000000000095479, 0.7500000000000096589, 1.000000000000000000 ),
 .UNSPECIFIED. ) ;
#17694 = CARTESIAN_POINT ( 'NONE',  ( 75.63268008801898645, 65.14737934564519151, -14.41129995628931404 ) ) ;
#17695 = CARTESIAN_POINT ( 'NONE',  ( 69.36794925685066460, 69.30658466222585901, -6.105352991895093062 ) ) ;
#17696 = CARTESIAN_POINT ( 'NONE',  ( -16.08955603893133812, 171.5177522451419350, 5.000000000000046185 ) ) ;
#17697 = CARTESIAN_POINT ( 'NONE',  ( 88.03035862218379748, 44.39407565500617636, 4.731894665149350310 ) ) ;
#17698 = AXIS2_PLACEMENT_3D ( 'NONE', #83262, #13829, #35131 ) ;
#17699 = ORIENTED_EDGE ( 'NONE', *, *, #84758, .F. ) ;
#17700 = CARTESIAN_POINT ( 'NONE',  ( 204.4329329219251861, 276.5587687693421799, 13.28840463846547948 ) ) ;
#17701 = CARTESIAN_POINT ( 'NONE',  ( 80.52615818510180645, 45.35857030409034252, 11.48786613706528570 ) ) ;
#17702 = CARTESIAN_POINT ( 'NONE',  ( 159.8188415394622268, 253.8326417772889840, -15.43862849427313222 ) ) ;
#17703 = CARTESIAN_POINT ( 'NONE',  ( 81.05763270389509501, 43.67158023151814916, 9.470390458390101074 ) ) ;
#17705 = EDGE_CURVE ( 'NONE', #78457, #47416, #40608, .T. ) ;
#17704 = CARTESIAN_POINT ( 'NONE',  ( 71.62823836921063503, 58.95366258879743526, -15.87062632715016974 ) ) ;
#17706 = CARTESIAN_POINT ( 'NONE',  ( 72.62284165280777870, 70.75758632292105688, 7.142220272083244836 ) ) ;
#17707 = ADVANCED_FACE ( 'NONE', ( #52702, #67413, #37501, #68408, #99336, #14714, #76529, #69903, #85154, #516, #85675, #63309, #94251, #8617, #62803, #23802, #71427, #1018, #16212, #86670 ), #39484, .T. ) ;
#17708 = CARTESIAN_POINT ( 'NONE',  ( -22.42236680055709641, 157.8615022471902591, 0.000000000000000000 ) ) ;
#17709 = ORIENTED_EDGE ( 'NONE', *, *, #91274, .F. ) ;
#17710 = LINE ( 'NONE', #25295, #28391 ) ;
#17711 = VECTOR ( 'NONE', #93034, 1000.000000000000000 ) ;
#17712 = CARTESIAN_POINT ( 'NONE',  ( 161.6707029936031574, 250.6251236501384483, 14.45053103226186231 ) ) ;
#17713 = CARTESIAN_POINT ( 'NONE',  ( 84.25055062944881001, 42.67738571844763129, 4.568100458215928583 ) ) ;
#17714 = CARTESIAN_POINT ( 'NONE',  ( 170.4700060268252457, 251.4149474771376731, 7.010157526727356370 ) ) ;
#17715 = LINE ( 'NONE', #27310, #6236 ) ;
#17716 = CARTESIAN_POINT ( 'NONE',  ( 200.9741374040782489, 267.1036203943184546, 5.055124302673880798 ) ) ;
#17717 = CARTESIAN_POINT ( 'NONE',  ( -19.65312891409030271, 93.06504152958497400, 10.00000000000000888 ) ) ;
#17718 = VERTEX_POINT ( 'NONE', #31899 ) ;
#17719 = VECTOR ( 'NONE', #89921, 1000.000000000000000 ) ;
#17720 = B_SPLINE_CURVE_WITH_KNOTS ( 'NONE', 3,
 ( #85485, #22644, #29744, #45428, #46417, #31226, #84970, #14553, #92578, #24138, #61122, #77852 ),
 .UNSPECIFIED., .F., .F.,
 ( 4, 2, 2, 2, 2, 4 ),
 ( 0.000000000000000000, 0.0004691669264628405001, 0.0009383338529256810001, 0.001407500779388521717, 0.001642084242619940015, 0.001876667705851358314 ),
 .UNSPECIFIED. ) ;
#17721 = CARTESIAN_POINT ( 'NONE',  ( 164.2672861321391053, 246.1277097281173667, -2.417001679502223777 ) ) ;
#17722 = CARTESIAN_POINT ( 'NONE',  ( 74.25007963244678422, 55.44098039740443085, 16.12168607022720579 ) ) ;
#17723 = CARTESIAN_POINT ( 'NONE',  ( 199.2695128734261516, 281.5989303855700996, -16.59789331015314318 ) ) ;
#17724 = B_SPLINE_CURVE_WITH_KNOTS ( 'NONE', 3,
 ( #21587, #23050, #51986, #45846, #74812, #76298, #30678, #92027, #76768, #52470, #5883, #7362, #60553, #61558, #92505, #13985, #82924, #82447, #29680, #13011, #43870, #5392, #44371, #67175, #83417, #98099, #75302, #75802, #36770, #98610, #29192, #99094, #70663, #16464, #79323, #47846, #78785, #40250, #86937, #33170, #55443, #71190, #15446, #7880, #94009, #9371, #16955, #46346, #69661, #63565, #54439, #64072 ),
 .UNSPECIFIED., .F., .F.,
 ( 4, 2, 2, 2, 2, 2, 2, 2, 2, 2, 2, 2, 2, 2, 2, 2, 2, 2, 2, 2, 2, 2, 2, 2, 2, 4 ),
 ( 9.939757338935888544E-05, 0.001109022545050053358, 0.001361428787965241480, 0.001613835030880429603, 0.001740038152338023447, 0.001866241273795617509, 0.001992444395253211570, 0.002118647516710805197, 0.002371053759626150313, 0.002623460002541494994, 0.003128272488372348288, 0.004137897460034054876, 0.005147522431695762332, 0.005652334917526606953, 0.005904741160442065692, 0.006030944281899838430, 0.006157147403357612035, 0.006220248964086553915, 0.006283350524815494928, 0.006409553646273225165, 0.006661959889188582423, 0.006914366132103938814, 0.007166772375019295205, 0.007419178617934651596, 0.007671584860850008854, 0.008176397346680856076 ),
 .UNSPECIFIED. ) ;
#17725 = CARTESIAN_POINT ( 'NONE',  ( 34.88136640284594847, 21.10801979619931146, 3.090169943749476733 ) ) ;
#17726 = CARTESIAN_POINT ( 'NONE',  ( 192.1640094933931096, 297.8091675017319062, 12.36911124822534447 ) ) ;
#17727 = CARTESIAN_POINT ( 'NONE',  ( 170.9335546628262534, 274.1512530509741055, 16.08033032509779758 ) ) ;
#17728 = FACE_BOUND ( 'NONE', #39307, .T. ) ;
#17729 = CARTESIAN_POINT ( 'NONE',  ( 161.0344790431144304, 273.4108582822469771, -15.37894900309793655 ) ) ;
#17730 = CARTESIAN_POINT ( 'NONE',  ( 188.6052575583571524, 261.0271860406964493, 2.867474821217330661 ) ) ;
#17731 = CARTESIAN_POINT ( 'NONE',  ( 161.8668411317136986, 250.2854024296290447, -13.43522912998426655 ) ) ;
#17732 = EDGE_CURVE ( 'NONE', #76706, #60917, #40496, .T. ) ;
#17733 = CARTESIAN_POINT ( 'NONE',  ( 5.155129649429669669, 173.7833772461660828, -9.188101187500095079 ) ) ;
#17734 = CARTESIAN_POINT ( 'NONE',  ( 81.89275847971933331, 46.90471798235346057, 12.15198961269920730 ) ) ;
#17735 = ORIENTED_EDGE ( 'NONE', *, *, #56543, .F. ) ;
#17736 = CARTESIAN_POINT ( 'NONE',  ( 160.1510049008126089, 253.7907123372172862, -14.98674719755693729 ) ) ;
#17737 = ADVANCED_FACE ( 'NONE', ( #47105 ), #40466, .T. ) ;
#17738 = PLANE ( 'NONE',  #33800 ) ;
#17739 = CARTESIAN_POINT ( 'NONE',  ( 204.6350011963004647, 275.7068757420208271, -12.64342396695018245 ) ) ;
#17740 = CARTESIAN_POINT ( 'NONE',  ( 82.06978721653376851, 41.21810153943793864, 5.445615563582272500 ) ) ;
#17741 = CARTESIAN_POINT ( 'NONE',  ( 13.65283037618196893, 184.8149278399161233, 9.188101187500093303 ) ) ;
#17742 = CARTESIAN_POINT ( 'NONE',  ( 161.4726291907278721, 250.9681975403669867, 14.52346149734912117 ) ) ;
#17743 = CARTESIAN_POINT ( 'NONE',  ( 12.00096474099108690, 32.03863464977599307, 10.00000000000000000 ) ) ;
#17744 = CARTESIAN_POINT ( 'NONE',  ( 42.35759689194659927, 26.58380873178790793, 6.180339887498953466 ) ) ;
#17745 = CARTESIAN_POINT ( 'NONE',  ( 181.7908406276906703, 294.3191638571922226, 6.361577546909467529 ) ) ;
#17746 = CARTESIAN_POINT ( 'NONE',  ( 173.5944101645363844, 272.6791245995305530, -16.35745397706937609 ) ) ;
#17747 = CARTESIAN_POINT ( 'NONE',  ( 149.6461826035522904, 271.4522039023545972, 11.73164196682384386 ) ) ;
#17748 = CARTESIAN_POINT ( 'NONE',  ( 38.20673285489099413, 96.19101212341352891, 59.99999999999999289 ) ) ;
#17749 = CARTESIAN_POINT ( 'NONE',  ( 10.13172230794903683, 17.80066082961419838, 10.00000000000000533 ) ) ;
#17750 = EDGE_CURVE ( 'NONE', #40534, #5726, #30920, .T. ) ;
#17751 = CARTESIAN_POINT ( 'NONE',  ( 190.0398248856338057, 298.8169614316505545, -8.166243001185458539 ) ) ;
#17752 = CARTESIAN_POINT ( 'NONE',  ( 84.06109941699628507, 51.61974178474098096, 14.72645736870185473 ) ) ;
#17753 = CARTESIAN_POINT ( 'NONE',  ( 84.09875786492884231, 229.3615022471903160, 5.000000000000046185 ) ) ;
#17754 = CARTESIAN_POINT ( 'NONE',  ( 69.72700409348841788, 66.78052502340607077, -10.07945174565168678 ) ) ;
#17755 = CARTESIAN_POINT ( 'NONE',  ( 203.7311721596700238, 270.2501766899930544, 6.028001199396760157 ) ) ;
#17756 = CARTESIAN_POINT ( 'NONE',  ( 40.68897417663616523, 203.4869531367911293, 4.594050593750046652 ) ) ;
#17757 = CARTESIAN_POINT ( 'NONE',  ( 194.3094773688834778, 284.8302703302293253, 17.74979085435418469 ) ) ;
#17758 = ORIENTED_EDGE ( 'NONE', *, *, #50742, .F. ) ;
#17759 = CARTESIAN_POINT ( 'NONE',  ( -13.78482047291978141, 85.09546807867688756, 14.96147123686172620 ) ) ;
#17760 = CARTESIAN_POINT ( 'NONE',  ( 146.8358616138309571, 276.3198226421291679, 4.054088818585255716 ) ) ;
#17762 = CARTESIAN_POINT ( 'NONE',  ( 72.97386446981147401, 70.68132344495336383, 8.316175787459508584 ) ) ;
#17761 = AXIS2_PLACEMENT_3D ( 'NONE', #9449, #70741, #78864 ) ;
#17763 = EDGE_LOOP ( 'NONE', ( #89620, #20544, #452, #11423 ) ) ;
#17764 = CARTESIAN_POINT ( 'NONE',  ( 89.19923881209058436, 210.7592609112379876, 2.679491924311254714 ) ) ;
#17765 = CARTESIAN_POINT ( 'NONE',  ( -167.0327448629461742, 42.61639673982678289, -21.50000000000000000 ) ) ;
#17766 = DIRECTION ( 'NONE',  ( -0.8660254037844387076, -0.4999999999999998890, -0.000000000000000000 ) ) ;
#17767 = CARTESIAN_POINT ( 'NONE',  ( 206.6679807590241467, 270.3735744487264583, -1.305484171715150854 ) ) ;
#17768 = CARTESIAN_POINT ( 'NONE',  ( 20.47532000956703513, 32.79752408145593279, -5.678558825948271327 ) ) ;
#17769 = CARTESIAN_POINT ( 'NONE',  ( 202.6560281492536717, 279.6364581158209717, 17.15553667345918853 ) ) ;
#17770 = CARTESIAN_POINT ( 'NONE',  ( 149.7200635338602410, 271.3242383773507527, -12.12223662813266500 ) ) ;
#17771 = CARTESIAN_POINT ( 'NONE',  ( 157.4627203480516755, 258.4629190429250798, 16.86169483958236626 ) ) ;
#17772 = ORIENTED_EDGE ( 'NONE', *, *, #21270, .T. ) ;
#17773 = CARTESIAN_POINT ( 'NONE',  ( 8.259543914800127951, 22.95586893147753571, 7.433330006724141015 ) ) ;
#17774 = B_SPLINE_CURVE_WITH_KNOTS ( 'NONE', 3,
 ( #80751, #96939, #35587, #20908, #12303, #66972, #57883, #51795, #66482, #74103, #51270, #19427, #42667, #27505, #5189, #73600 ),
 .UNSPECIFIED., .F., .F.,
 ( 4, 2, 2, 2, 2, 2, 2, 4 ),
 ( 0.000000000000000000, 0.0003044019995352871002, 0.0006088039990705742003, 0.0009132059986058614631, 0.001217607998141148401, 0.001522009997676435555, 0.001826411997211722926, 0.002435215996282302873 ),
 .UNSPECIFIED. ) ;
#17775 = CARTESIAN_POINT ( 'NONE',  ( 76.93060788005539052, 58.57154978847167826, -16.09350835567875748 ) ) ;
#17776 = CARTESIAN_POINT ( 'NONE',  ( 71.84099513407564075, 72.54812194311107021, -1.276242074083207001 ) ) ;
#17777 = VERTEX_POINT ( 'NONE', #64313 ) ;
#17778 = CARTESIAN_POINT ( 'NONE',  ( 179.6077830788075005, 283.1794306977752171, 16.12751113146045867 ) ) ;
#17779 = CARTESIAN_POINT ( 'NONE',  ( 150.6431064791187850, 269.7254810985950257, 15.11064854015152470 ) ) ;
#17780 = CARTESIAN_POINT ( 'NONE',  ( 182.1439385020048860, 290.0253507885926183, 13.01467259685074573 ) ) ;
#17781 = CARTESIAN_POINT ( 'NONE',  ( 74.91675901630549106, 64.03713867913845093, -14.74143563292419934 ) ) ;
#17782 = EDGE_LOOP ( 'NONE', ( #11942, #89729, #3600, #93416 ) ) ;
#17783 = AXIS2_PLACEMENT_3D ( 'NONE', #100092, #6868, #52971 ) ;
#17784 = ORIENTED_EDGE ( 'NONE', *, *, #95834, .T. ) ;
#17786 = CARTESIAN_POINT ( 'NONE',  ( -19.65312891409030271, 93.06504152958497400, 177.5919119679930134 ) ) ;
#17785 = CARTESIAN_POINT ( 'NONE',  ( 189.6669961101834190, 274.2288721523702861, -15.66740572939721154 ) ) ;
#17787 = EDGE_LOOP ( 'NONE', ( #74842, #9152, #46683, #35102 ) ) ;
#17788 = CARTESIAN_POINT ( 'NONE',  ( 200.9521687275011175, 282.5876292032514243, -18.16013154125647944 ) ) ;
#17789 = DIRECTION ( 'NONE',  ( 0.000000000000000000, -0.000000000000000000, -1.000000000000000000 ) ) ;
#17790 = CARTESIAN_POINT ( 'NONE',  ( 72.63229333555629808, 57.14188050215015835, -16.36598023500532051 ) ) ;
#17791 = CARTESIAN_POINT ( 'NONE',  ( 76.95477351241487440, 63.69079797318030955, 15.35326628456841824 ) ) ;
#17792 = EDGE_CURVE ( 'NONE', #23912, #54506, #98602, .T. ) ;
#17793 = CARTESIAN_POINT ( 'NONE',  ( 157.8239779013331372, 257.2878469527003062, -17.92251383114021479 ) ) ;
#17794 = CARTESIAN_POINT ( 'NONE',  ( 101.7984123748231298, 220.3923013555410080, 4.594050593750050204 ) ) ;
#17795 = VECTOR ( 'NONE', #21141, 1000.000000000000000 ) ;
#17796 = CARTESIAN_POINT ( 'NONE',  ( 87.96987174722529801, 210.0494855054051584, -2.679491924311248496 ) ) ;
#17797 = VERTEX_POINT ( 'NONE', #82560 ) ;
#17798 = FACE_OUTER_BOUND ( 'NONE', #63296, .T. ) ;
#17799 = ORIENTED_EDGE ( 'NONE', *, *, #70034, .T. ) ;
#17800 = CARTESIAN_POINT ( 'NONE',  ( 25.85549604718420014, 26.87878583063842797, -9.188101187500006262 ) ) ;
#17801 = LINE ( 'NONE', #18302, #3475 ) ;
#17802 = CARTESIAN_POINT ( 'NONE',  ( 70.24096790410676761, 70.63068755123174469, -5.460583647663642459 ) ) ;
#17803 = CARTESIAN_POINT ( 'NONE',  ( 57.65757265809627796, 216.3464784336661637, 1.353441290958777525E-15 ) ) ;
#17804 = CARTESIAN_POINT ( 'NONE',  ( 73.77733668265750566, 68.41783923479601981, 10.96675506585084925 ) ) ;
#17805 = CARTESIAN_POINT ( 'NONE',  ( 191.5451565139252068, 298.8810523045859213, 7.782291334092181323 ) ) ;
#17806 = CARTESIAN_POINT ( 'NONE',  ( 198.1915864813676933, 287.3690979120270867, 17.02875488965938189 ) ) ;
#17807 = CARTESIAN_POINT ( 'NONE',  ( 174.6077656993458902, 272.0895251850873251, 16.48419557227402521 ) ) ;
#17808 = CARTESIAN_POINT ( 'NONE',  ( 87.83187315495058556, 45.09740525803776023, 6.666720864128775403 ) ) ;
#17809 = B_SPLINE_CURVE_WITH_KNOTS ( 'NONE', 3,
 ( #783, #53968, #45865, #37289, #14502, #77812, #68184, #23076, #15471, #69184 ),
 .UNSPECIFIED., .F., .F.,
 ( 4, 2, 2, 2, 4 ),
 ( 0.000000000000000000, 0.2500000000000000000, 0.5000000000000000000, 0.7500000000000000000, 1.000000000000000000 ),
 .UNSPECIFIED. ) ;
#17810 = VERTEX_POINT ( 'NONE', #44988 ) ;
#17811 = CARTESIAN_POINT ( 'NONE',  ( 80.74481995453727734, 56.30375985177428078, -16.12179401971438608 ) ) ;
#17812 = CARTESIAN_POINT ( 'NONE',  ( 178.0498610173981433, 288.8670518452568672, 10.97635994419254324 ) ) ;
#17813 = CARTESIAN_POINT ( 'NONE',  ( 30.80155721116056355, 46.36891074996812989, 10.00000000000000000 ) ) ;
#17814 = VERTEX_POINT ( 'NONE', #37386 ) ;
#17815 = CARTESIAN_POINT ( 'NONE',  ( 172.0900369064530082, 258.7028160241414412, -13.89453031103171909 ) ) ;
#17816 = CARTESIAN_POINT ( 'NONE',  ( 174.2114552513667434, 277.4090650679840451, -15.60050915102441849 ) ) ;
#17817 = CARTESIAN_POINT ( 'NONE',  ( 161.0974665087481981, 251.6179983666593216, -13.69252715295363210 ) ) ;
#17818 = CARTESIAN_POINT ( 'NONE',  ( 71.90223342829800401, 218.9865022471902876, -10.00000000000009592 ) ) ;
#17819 = ADVANCED_FACE ( 'NONE', ( #99214 ), #13124, .F. ) ;
#17820 = CARTESIAN_POINT ( 'NONE',  ( 149.6700657135140489, 271.4108371424580355, 12.58635654151485284 ) ) ;
#17821 = CARTESIAN_POINT ( 'NONE',  ( 44.18794977381974576, 118.5901545549086791, 10.00000000000000000 ) ) ;
#17822 = CARTESIAN_POINT ( 'NONE',  ( 206.4768661561222984, 273.0185725604343361, 11.39716120335626925 ) ) ;
#17823 = CARTESIAN_POINT ( 'NONE',  ( 75.80739212458533416, 65.61160923183801685, 13.82794609268849406 ) ) ;
#17824 = CARTESIAN_POINT ( 'NONE',  ( 164.1198370452240454, 253.9973699534765501, 14.40966736368955026 ) ) ;
#17825 = FACE_OUTER_BOUND ( 'NONE', #24765, .T. ) ;
#17826 = CARTESIAN_POINT ( 'NONE',  ( 102.3121810886138832, 236.0024278399160949, 9.188101187500095079 ) ) ;
#17827 = ORIENTED_EDGE ( 'NONE', *, *, #33051, .T. ) ;
#17828 = CARTESIAN_POINT ( 'NONE',  ( 191.4082244002820516, 299.1182256826033949, -8.271837126846561361 ) ) ;
#17829 = CARTESIAN_POINT ( 'NONE',  ( 83.10371324467729437, 41.41193507237026949, 1.792060051283224098 ) ) ;
#17830 = CARTESIAN_POINT ( 'NONE',  ( 203.3684377202211522, 278.4025285431072803, -16.56116267537666076 ) ) ;
#17831 = EDGE_CURVE ( 'NONE', #17546, #50031, #75931, .T. ) ;
#17832 = FACE_OUTER_BOUND ( 'NONE', #17950, .T. ) ;
#17833 = EDGE_CURVE ( 'NONE', #34456, #42933, #90080, .T. ) ;
#17834 = CARTESIAN_POINT ( 'NONE',  ( 83.74452895351211623, 51.49425885220755816, -14.36953079076762663 ) ) ;
#17835 = CARTESIAN_POINT ( 'NONE',  ( 174.8082613492344706, 252.7768654443898697, 5.092377277474876784 ) ) ;
#17836 = ORIENTED_EDGE ( 'NONE', *, *, #94713, .F. ) ;
#17837 = CARTESIAN_POINT ( 'NONE',  ( 80.51438793199335464, 57.80134815862462005, -16.24637616362180026 ) ) ;
#17838 = CARTESIAN_POINT ( 'NONE',  ( 71.90384105138682003, 72.23694104886283185, 0.5914362187818961170 ) ) ;
#17840 = CARTESIAN_POINT ( 'NONE',  ( 184.5707630536305714, 261.7313796936621770, 9.605701619106270073 ) ) ;
#17839 = CARTESIAN_POINT ( 'NONE',  ( 72.51358964696871112, 70.84733833069179809, 7.633428234268393453 ) ) ;
#17841 = CARTESIAN_POINT ( 'NONE',  ( 164.4575000359379828, 245.7982495824318505, -1.032884424947213997 ) ) ;
#17842 = CARTESIAN_POINT ( 'NONE',  ( 134.2197177853555843, 257.4869531367911577, 4.594050593750046652 ) ) ;
#17843 = CARTESIAN_POINT ( 'NONE',  ( 150.9584389135710865, 269.1793093008492406, -15.82751450793727699 ) ) ;
#17844 = AXIS2_PLACEMENT_3D ( 'NONE', #38235, #63057, #76286 ) ;
#17845 = CARTESIAN_POINT ( 'NONE',  ( 187.6000567067785596, 297.9053677150377553, 4.710378011297792433 ) ) ;
#17846 = DIRECTION ( 'NONE',  ( -0.7082622432767160525, -0.7059494278973771353, 0.000000000000000000 ) ) ;
#17847 = CARTESIAN_POINT ( 'NONE',  ( 57.82012596918833935, 210.3149278399160664, 9.188101187500093303 ) ) ;
#17848 = CARTESIAN_POINT ( 'NONE',  ( 85.63146384662782395, 48.39429698310328121, -12.21155806772682340 ) ) ;
#17849 = CARTESIAN_POINT ( 'NONE',  ( 171.0605077851577391, 249.7720551134824802, 4.373113433538289740 ) ) ;
#17850 = CARTESIAN_POINT ( 'NONE',  ( 68.04992555225376805, 69.88878367761962807, -0.7546937224205583217 ) ) ;
#17851 = CARTESIAN_POINT ( 'NONE',  ( 174.8228812346009420, 261.7023400441105991, 14.27858715412817681 ) ) ;
#17852 = LINE ( 'NONE', #33034, #56329 ) ;
#17853 = CARTESIAN_POINT ( 'NONE',  ( 6.117390533544194930, 29.33055864014943026, -10.00000000000000000 ) ) ;
#17854 = CARTESIAN_POINT ( 'NONE',  ( -23.73952538801239598, 24.43184193311134678, -10.00000000000000000 ) ) ;
#17855 = AXIS2_PLACEMENT_3D ( 'NONE', #64300, #94731, #95756 ) ;
#17856 = CARTESIAN_POINT ( 'NONE',  ( 193.2148890581035516, 289.1379580677868830, 16.18061100571382838 ) ) ;
#17857 = EDGE_CURVE ( 'NONE', #59587, #27141, #43493, .T. ) ;
#17858 = CARTESIAN_POINT ( 'NONE',  ( 123.2683651867145898, 248.6427522451419350, 10.00000000000009237 ) ) ;
#17859 = B_SPLINE_CURVE_WITH_KNOTS ( 'NONE', 3,
 ( #79924, #55555, #39845, #32271 ),
 .UNSPECIFIED., .F., .F.,
 ( 4, 4 ),
 ( 0.004970936986721591171, 0.01054214532650148139 ),
 .UNSPECIFIED. ) ;
#17860 = B_SPLINE_SURFACE_WITH_KNOTS ( 'NONE', 3, 1, ( 
 ( #296, #9915 ),
 ( #85447, #77819 ),
 ( #8401, #72221 ),
 ( #3324, #2826 ),
 ( #49398, #48908 ),
 ( #73706, #35188 ),
 ( #25607, #80856 ),
 ( #57994, #88975 ),
 ( #33715, #88464 ),
 ( #42280, #56983 ),
 ( #73214, #34690 ),
 ( #49898, #3809 ),
 ( #34205, #64607 ),
 ( #11428, #87968 ),
 ( #4288, #19530 ),
 ( #81834, #72734 ),
 ( #79843, #56494 ),
 ( #41788, #26108 ),
 ( #87481, #43277 ),
 ( #18016, #26606 ),
 ( #65591, #95562 ),
 ( #89451, #96048 ),
 ( #66096, #11916 ),
 ( #19025, #10913 ),
 ( #65095, #96539 ),
 ( #10409, #41279 ),
 ( #18512, #20007 ),
 ( #80345, #27110 ),
 ( #50886, #50390 ),
 ( #81342, #42772 ),
 ( #97044, #27612 ) ),
 .UNSPECIFIED., .F., .F., .F.,
 ( 4, 3, 3, 3, 3, 3, 3, 3, 3, 3, 4 ),
 ( 2, 2 ),
 ( 0.000000000000000000, 0.1333490885032332374, 0.3007194338854220494, 0.4699862290245090390, 0.5844252810809320575, 0.6686540514502788968, 0.7354980260655487045, 0.8028463152565534777, 0.8633854507757111607, 0.9437142632667073761, 1.000000000000000000 ),
 ( 0.000000000000000000, 1.000000000000000000 ),
 .UNSPECIFIED. ) ;
#17861 = CARTESIAN_POINT ( 'NONE',  ( 76.82765370740766286, 53.09445422599739572, -15.90143384433676665 ) ) ;
#17862 = VERTEX_POINT ( 'NONE', #84050 ) ;
#17863 = CARTESIAN_POINT ( 'NONE',  ( 190.6084209867335915, 300.5035258309363826, -0.5505750481748228342 ) ) ;
#17864 = CARTESIAN_POINT ( 'NONE',  ( 9.894862028763428796, 29.21091486745858745, -1.111400068045478839E-16 ) ) ;
#17865 = CARTESIAN_POINT ( 'NONE',  ( 50.26990084964904071, 190.6423013555410080, -4.594050593750043987 ) ) ;
#17866 = B_SPLINE_CURVE_WITH_KNOTS ( 'NONE', 3,
 ( #37996, #31902, #77009, #62806, #30915, #84655, #99834, #54696, #23807, #85680, #22317, #9120, #24321, #84171, #61802, #32419, #85158, #93252, #53699, #68909, #16217, #7112, #30418, #55196, #7615, #86180, #23304, #15200, #61308, #47109, #78029, #8621, #92270, #46604, #46096, #38503, #70414, #1537, #16714, #47607, #69418, #62295, #45601, #39992, #54193, #70931, #22818, #8127 ),
 .UNSPECIFIED., .F., .F.,
 ( 4, 2, 2, 2, 2, 2, 2, 2, 2, 2, 2, 2, 2, 2, 2, 2, 2, 2, 2, 2, 2, 2, 2, 4 ),
 ( 0.0006475970585499132631, 0.001633499019554147860, 0.001879974509805226648, 0.002126450000056305436, 0.002249687745181803630, 0.002372925490307301391, 0.002496163235432799152, 0.002619400980558297346, 0.002865876470809139778, 0.003112351961059982210, 0.003605302941561666641, 0.004591204902565082339, 0.005577106863568498905, 0.006070057844070207188, 0.006563008824571915471, 0.006686246569697319557, 0.006747865442260097060, 0.006809484314822874564, 0.006932722059948418294, 0.007055959805073961158, 0.007302435295325071171, 0.007548910785576180317, 0.008041861766078397741, 0.008534812746580616033 ),
 .UNSPECIFIED. ) ;
#17867 = CARTESIAN_POINT ( 'NONE',  ( 16.56575413784759121, 33.65659080271450421, -1.878358725466461243E-16 ) ) ;
#17868 = CARTESIAN_POINT ( 'NONE',  ( 191.2966886305924277, 269.6700499042153751, 14.73436473925947254 ) ) ;
#17869 = CARTESIAN_POINT ( 'NONE',  ( 73.90491717100159974, 220.1427522451418781, 10.00000000000009415 ) ) ;
#17870 = CARTESIAN_POINT ( 'NONE',  ( 190.9586609929293104, 299.8968923453624598, -4.970176667899034229 ) ) ;
#17871 = CARTESIAN_POINT ( 'NONE',  ( 72.27349450330626723, 72.00028387666623075, 3.519045224867114907 ) ) ;
#17873 = CARTESIAN_POINT ( 'NONE',  ( 60.98670489788378291, 196.0177522451417929, 5.000000000000051514 ) ) ;
#17872 = CARTESIAN_POINT ( 'NONE',  ( 198.1299909997756572, 277.6936685613563327, -16.45399728936175521 ) ) ;
#17874 = DIRECTION ( 'NONE',  ( -7.401486830834377265E-16, 7.401486830834377265E-16, -1.000000000000000000 ) ) ;
#17875 = CARTESIAN_POINT ( 'NONE',  ( 181.0163322597064735, 256.3998266669695454, 1.320919897633525686 ) ) ;
#17876 = CARTESIAN_POINT ( 'NONE',  ( 157.8043799545718286, 257.3217915922150496, -17.97575562758749257 ) ) ;
#17877 = LINE ( 'NONE', #80711, #27461 ) ;
#17878 = ORIENTED_EDGE ( 'NONE', *, *, #83156, .T. ) ;
#17879 = CARTESIAN_POINT ( 'NONE',  ( 51.11762373747155408, 186.9865022471901455, 1.119607411625061291E-15 ) ) ;
#17880 = CARTESIAN_POINT ( 'NONE',  ( 184.6791799238867213, 294.3958812847097875, 10.00409762499635846 ) ) ;
#17881 = CARTESIAN_POINT ( 'NONE',  ( 208.3132655666949233, 269.8378354783333180, 2.688523655043302707 ) ) ;
#17882 = CARTESIAN_POINT ( 'NONE',  ( 4.830370123010505168, 173.5958772461660828, -9.188101187500095079 ) ) ;
#17883 = CARTESIAN_POINT ( 'NONE',  ( 38.69009612255265296, 24.19860640527295104, 2.839279412974134775 ) ) ;
#17885 = CARTESIAN_POINT ( 'NONE',  ( 185.0827326577621932, 267.3863886128668241, -15.44458570467620007 ) ) ;
#17884 = CARTESIAN_POINT ( 'NONE',  ( 163.8743436044941006, 247.1942500250122237, 6.352646675549487476 ) ) ;
#17886 = CARTESIAN_POINT ( 'NONE',  ( 192.0963028965829551, 297.9264387674147656, 11.34530024772836754 ) ) ;
#17887 = CARTESIAN_POINT ( 'NONE',  ( 31.37640799630998956, 30.06628583063843507, -9.188101187500006262 ) ) ;
#17888 = CARTESIAN_POINT ( 'NONE',  ( 155.7565973091642491, 261.3698664144865802, -17.06302194855465970 ) ) ;
#17889 = CARTESIAN_POINT ( 'NONE',  ( 93.96857342517719758, -8.000000000000000000, 0.000000000000000000 ) ) ;
#17890 = CARTESIAN_POINT ( 'NONE',  ( 65.86133180236033979, 68.95061956165834260, 2.403325992957665580 ) ) ;
#17891 = VERTEX_POINT ( 'NONE', #74924 ) ;
#17892 = CARTESIAN_POINT ( 'NONE',  ( 37.17256469204939151, 37.16454794089045066, -10.00000000000000355 ) ) ;
#17893 = CARTESIAN_POINT ( 'NONE',  ( 150.3919553510150138, 271.7028101267143256, -12.69180684425547234 ) ) ;
#17894 =( NAMED_UNIT ( * ) PLANE_ANGLE_UNIT ( ) SI_UNIT ( $, .RADIAN. ) );
#17895 = EDGE_CURVE ( 'NONE', #61222, #49297, #66309, .T. ) ;
#17896 = CARTESIAN_POINT ( 'NONE',  ( 12.27453364332850505, 12.80170272979924739, 7.433330006724137462 ) ) ;
#17897 = CARTESIAN_POINT ( 'NONE',  ( 153.3438016572222296, 277.7235982778221342, -5.222468100669257041 ) ) ;
#17898 = CARTESIAN_POINT ( 'NONE',  ( 12.13982549814181411, 27.98502408145591502, -5.678558825948271327 ) ) ;
#17899 = CARTESIAN_POINT ( 'NONE',  ( 207.2372516306344608, 271.7015462852415908, 9.113068844475435526 ) ) ;
#17900 = CARTESIAN_POINT ( 'NONE',  ( 84.42663183290279960, 49.91580812419739743, -13.73522929182741059 ) ) ;
#17901 = CARTESIAN_POINT ( 'NONE',  ( 88.12055419386514643, 44.14876995426037354, -1.724036421897656934 ) ) ;
#17902 = ORIENTED_EDGE ( 'NONE', *, *, #45812, .F. ) ;
#17903 = CARTESIAN_POINT ( 'NONE',  ( 73.43762515466688967, 73.52662068827324049, 2.033788753608857291E-15 ) ) ;
#17904 = CARTESIAN_POINT ( 'NONE',  ( 207.4764081617721843, 271.2873150223495600, 6.359972247200924578 ) ) ;
#17905 = CARTESIAN_POINT ( 'NONE',  ( 191.6375357288227121, 298.3185633171067934, 8.736688151381864387 ) ) ;
#17906 = CARTESIAN_POINT ( 'NONE',  ( 87.18667961818120204, 45.38743208957181707, 7.099644388500629510 ) ) ;
#17907 = CARTESIAN_POINT ( 'NONE',  ( 194.3252252352508265, 294.0658320307167628, 14.07225870721148731 ) ) ;
#17908 = ORIENTED_EDGE ( 'NONE', *, *, #52945, .F. ) ;
#17909 = ORIENTED_EDGE ( 'NONE', *, *, #58316, .F. ) ;
#17910 = CARTESIAN_POINT ( 'NONE',  ( 159.2882649660388097, 278.2295398647215166, -9.800005944379622136 ) ) ;
#17911 = CARTESIAN_POINT ( 'NONE',  ( 85.85796257688252808, 47.46348540752531875, 10.78667950937928310 ) ) ;
#17912 = ORIENTED_EDGE ( 'NONE', *, *, #87657, .T. ) ;
#17913 = CARTESIAN_POINT ( 'NONE',  ( 77.99241281452712826, 58.97741566620933895, 16.11859265156807552 ) ) ;
#17914 = CARTESIAN_POINT ( 'NONE',  ( 188.9259862807830928, 297.2999610039981917, 7.833423077949829505 ) ) ;
#17915 = ORIENTED_EDGE ( 'NONE', *, *, #51314, .F. ) ;
#17916 = CARTESIAN_POINT ( 'NONE',  ( 27.81076257310190769, 39.55466486950702176, 7.012934429366973338E-14 ) ) ;
#17917 = CARTESIAN_POINT ( 'NONE',  ( 78.92023586790456591, 59.45316570216662910, -16.52216786098998824 ) ) ;
#17918 = CARTESIAN_POINT ( 'NONE',  ( 80.20807540180908290, 48.38748433693235285, -14.23851719010586336 ) ) ;
#17919 = CARTESIAN_POINT ( 'NONE',  ( 80.48839377771611225, 43.63089982895380103, 9.811837369924520047 ) ) ;
#17920 = ORIENTED_EDGE ( 'NONE', *, *, #85209, .T. ) ;
#17921 = CARTESIAN_POINT ( 'NONE',  ( 161.4844649541891499, 250.9476973967054789, 12.93553496455142415 ) ) ;
#17922 = CARTESIAN_POINT ( 'NONE',  ( 166.1882723046687715, 274.1880526520006356, -15.18604489847817440 ) ) ;
#17923 = DIRECTION ( 'NONE',  ( -0.8718556560469457040, -0.4897629171537489778, 0.000000000000000000 ) ) ;
#17924 = CARTESIAN_POINT ( 'NONE',  ( 30.46276441966746873, 39.36126292948897998, 6.180339887498949913 ) ) ;
#17925 = ORIENTED_EDGE ( 'NONE', *, *, #65535, .T. ) ;
#17926 = CYLINDRICAL_SURFACE ( 'NONE', #86027, 10.00000000000010658 ) ;
#17927 = CARTESIAN_POINT ( 'NONE',  ( 33.58045587329145576, 41.16126292948898424, -6.180339887498951690 ) ) ;
#17928 = EDGE_LOOP ( 'NONE', ( #43552, #53171, #76975, #69088 ) ) ;
#17929 = ORIENTED_EDGE ( 'NONE', *, *, #45726, .T. ) ;
#17930 = DIRECTION ( 'NONE',  ( 1.000000000000000000, -1.235257323912246174E-15, 0.000000000000000000 ) ) ;
#17931 = ORIENTED_EDGE ( 'NONE', *, *, #28146, .F. ) ;
#17932 = DIRECTION ( 'NONE',  ( 0.000000000000000000, 0.000000000000000000, 1.000000000000000000 ) ) ;
#17933 = AXIS2_PLACEMENT_3D ( 'NONE', #67594, #82850, #74235 ) ;
#17934 = ORIENTED_EDGE ( 'NONE', *, *, #90245, .F. ) ;
#17935 = B_SPLINE_CURVE_WITH_KNOTS ( 'NONE', 3,
 ( #92927, #53877, #22003, #75726, #8307, #52401 ),
 .UNSPECIFIED., .F., .F.,
 ( 4, 2, 4 ),
 ( 0.02140010735210632134, 0.02598537340429217871, 0.03057063945647803607 ),
 .UNSPECIFIED. ) ;
#17936 = CARTESIAN_POINT ( 'NONE',  ( 158.8610524726626352, 259.9521463235002443, 17.06794338822354007 ) ) ;
#17937 = CARTESIAN_POINT ( 'NONE',  ( 147.5402343333208819, 275.0998133045071086, 7.426466083746204205 ) ) ;
#17938 = CARTESIAN_POINT ( 'NONE',  ( 180.3607121444757695, 291.6144073518768209, -9.916234337600110749 ) ) ;
#17939 = CARTESIAN_POINT ( 'NONE',  ( 69.31776955885030134, 64.77206886784115625, 11.72538624431390630 ) ) ;
#17940 = CARTESIAN_POINT ( 'NONE',  ( 152.6945189806187955, 266.1723304187151484, 16.62409282110771613 ) ) ;
#17941 = CARTESIAN_POINT ( 'NONE',  ( 82.56662147140762897, 53.48431740468424778, -15.73383048919865423 ) ) ;
#17942 = CARTESIAN_POINT ( 'NONE',  ( 77.36600796148924530, 49.13692148722834929, -14.77749963168140113 ) ) ;
#17943 = ORIENTED_EDGE ( 'NONE', *, *, #46843, .T. ) ;
#17944 = PLANE ( 'NONE',  #38289 ) ;
#17945 = CARTESIAN_POINT ( 'NONE',  ( 21.37261828447143586, 20.84335787977763133, 9.188101187500006262 ) ) ;
#17946 = CARTESIAN_POINT ( 'NONE',  ( 205.8379285891498682, 274.1252448892948905, 10.44730901608240181 ) ) ;
#17947 = CARTESIAN_POINT ( 'NONE',  ( 190.8615153089693877, 298.2432307714133799, -9.563193282498932746 ) ) ;
#17949 = ORIENTED_EDGE ( 'NONE', *, *, #50941, .T. ) ;
#17948 = CARTESIAN_POINT ( 'NONE',  ( 159.2876523829509665, 254.7526883847961017, 15.64395448151312351 ) ) ;
#17950 = EDGE_LOOP ( 'NONE', ( #24492, #77620, #11504 ) ) ;
#17951 = CARTESIAN_POINT ( 'NONE',  ( 191.0347634949463895, 299.7650789452856657, 5.488533456550475087 ) ) ;
#17952 = CARTESIAN_POINT ( 'NONE',  ( 81.46828529536601593, 52.31631583627443405, -15.16276159314715066 ) ) ;
#17953 = CARTESIAN_POINT ( 'NONE',  ( 86.67826574493778935, 45.56729948127456709, 8.573571648110831944 ) ) ;
#17954 = FACE_OUTER_BOUND ( 'NONE', #5780, .T. ) ;
#17955 = B_SPLINE_CURVE_WITH_KNOTS ( 'NONE', 3,
 ( #58224, #81571, #73941, #96273, #43522, #41524, #74461, #5040, #66823, #3073, #4527, #35430, #11652, #97266, #27833, #64844, #95792, #26346, #57719, #11163, #42030, #3556, #34435, #26841, #23580, #298, #15480, #6024, #46897, #21238, #67833, #52610, #5532, #21726, #59717, #39274, #28835, #52117, #82585, #83568, #83064, #13638, #98754, #90682, #13149, #31185, #91161, #36920 ),
 .UNSPECIFIED., .F., .F.,
 ( 4, 2, 2, 2, 2, 2, 2, 2, 2, 2, 2, 2, 2, 2, 2, 2, 2, 2, 2, 2, 2, 2, 2, 4 ),
 ( 0.002832262493831907979, 0.003034780587620233231, 0.003237298681408558049, 0.003338557728302722193, 0.003439816775196886337, 0.003541075822091050047, 0.003642334868985214191, 0.003844852962773611868, 0.004047371056562009545, 0.004452407244138802296, 0.005262479619292319277, 0.006072551994445837126, 0.006882624369599354974, 0.007692696744752871955, 0.007793955791646984925, 0.007844585315093993705, 0.007895214838541001617, 0.007945844361988012999, 0.007996473885435020912, 0.008097732932329217148, 0.008300251026117758807, 0.008502769119906296996, 0.008907805307483380314, 0.009312841495060458427 ),
 .UNSPECIFIED. ) ;
#17956 = ADVANCED_FACE ( 'NONE', ( #36391 ), #5017, .T. ) ;
#17957 = CARTESIAN_POINT ( 'NONE',  ( 161.0952649348064938, 251.6218116045831437, 13.81854265722852482 ) ) ;
#17958 = EDGE_CURVE ( 'NONE', #36461, #36797, #55136, .T. ) ;
#17959 = CARTESIAN_POINT ( 'NONE',  ( 79.14312167556931854, 57.64441083166269664, 0.000000000000000000 ) ) ;
#17960 = ORIENTED_EDGE ( 'NONE', *, *, #54651, .T. ) ;
#17961 = FACE_OUTER_BOUND ( 'NONE', #96703, .T. ) ;
#17962 = CARTESIAN_POINT ( 'NONE',  ( 5.249714564834229158, 26.52903772873355237, -1.583844403245363575 ) ) ;
#17963 = CARTESIAN_POINT ( 'NONE',  ( 51.91943859288068097, 212.3297689869269220, -2.679491924311252493 ) ) ;
#17964 = EDGE_CURVE ( 'NONE', #61794, #89238, #10792, .T. ) ;
#17965 = CARTESIAN_POINT ( 'NONE',  ( 192.1902081399911708, 278.5511368846052846, 17.60910353013618490 ) ) ;
#17966 = ADVANCED_FACE ( 'NONE', ( #86066 ), #2499, .T. ) ;
#17967 = CARTESIAN_POINT ( 'NONE',  ( 26.27351996285754510, 172.6427522451417929, 1.119607411625061291E-15 ) ) ;
#17968 = CARTESIAN_POINT ( 'NONE',  ( 104.5047417616495125, 221.9548013555409511, -4.594050593750042211 ) ) ;
#17969 = FACE_OUTER_BOUND ( 'NONE', #65510, .T. ) ;
#17970 = DIRECTION ( 'NONE',  ( 0.4999999999999992784, -0.8660254037844390407, 0.000000000000000000 ) ) ;
#17971 = CARTESIAN_POINT ( 'NONE',  ( 170.0778888726681259, 280.3528892525189917, -13.69567824744189011 ) ) ;
#17972 = CARTESIAN_POINT ( 'NONE',  ( 16.87327557256410060, 189.7369531367911293, -4.594050593750048428 ) ) ;
#17973 = CARTESIAN_POINT ( 'NONE',  ( 200.3414094930810165, 283.6454952284590263, 16.87912319229835489 ) ) ;
#17974 = ORIENTED_EDGE ( 'NONE', *, *, #8614, .T. ) ;
#17976 = ORIENTED_EDGE ( 'NONE', *, *, #27551, .F. ) ;
#17975 = PRODUCT_DEFINITION_CONTEXT ( 'detailed design', #31646, 'design' ) ;
#17977 = CARTESIAN_POINT ( 'NONE',  ( 200.9301851018323930, 267.7613211563358391, -3.272224760724934622 ) ) ;
#17978 = CARTESIAN_POINT ( 'NONE',  ( 67.90496466116340457, 69.50686951990996931, 2.866334304769667884 ) ) ;
#17979 = CARTESIAN_POINT ( 'NONE',  ( 190.2629546459234859, 273.4080951500121159, -16.67925241984795903 ) ) ;
#17980 = DIRECTION ( 'NONE',  ( -0.8660254037844387076, -0.4999999999999998890, -0.000000000000000000 ) ) ;
#17981 = CARTESIAN_POINT ( 'NONE',  ( 207.7836085030675690, 270.7552284231231852, -5.468305433308493058 ) ) ;
#17982 = CARTESIAN_POINT ( 'NONE',  ( 184.4613657420405559, 285.4439036850075695, 15.12519662030571510 ) ) ;
#17983 = CARTESIAN_POINT ( 'NONE',  ( 74.46210375232622880, 68.11509597928741755, -11.59312039134510819 ) ) ;
#17984 = CARTESIAN_POINT ( 'NONE',  ( 42.04265951369687571, 185.8923013555410080, 4.594050593750050204 ) ) ;
#17985 = CARTESIAN_POINT ( 'NONE',  ( 83.50336539627915045, 219.0177522451418497, -10.00000000000009592 ) ) ;
#17986 = ORIENTED_EDGE ( 'NONE', *, *, #31199, .F. ) ;
#17987 = CARTESIAN_POINT ( 'NONE',  ( 84.48565599034226636, 48.85800685522642794, 12.55231365627821916 ) ) ;
#17988 = CARTESIAN_POINT ( 'NONE',  ( 178.9277264332957316, 259.3186642429575386, -10.30312369890718571 ) ) ;
#17989 = CARTESIAN_POINT ( 'NONE',  ( 0.9872088458345583684, 177.5024278399160949, 9.188101187500095079 ) ) ;
#17990 = DIRECTION ( 'NONE',  ( 0.000000000000000000, -1.000000000000000000, 1.090355031989287297E-16 ) ) ;
#17991 = CARTESIAN_POINT ( 'NONE',  ( 161.1750406344237661, 251.4836360396366501, -14.21198410781773802 ) ) ;
#17992 = DIRECTION ( 'NONE',  ( -0.8660254037844387076, -0.4999999999999998890, -0.000000000000000000 ) ) ;
#17993 = CARTESIAN_POINT ( 'NONE',  ( 192.9523350703175311, 296.4437475495926719, -13.35611922184540923 ) ) ;
#17994 = CARTESIAN_POINT ( 'NONE',  ( 193.2752197284765998, 263.9480352582601768, 7.898392093415175452 ) ) ;
#17995 = CARTESIAN_POINT ( 'NONE',  ( 171.5690451057043617, 279.9092378594070851, 15.19443294771788189 ) ) ;
#17996 = CARTESIAN_POINT ( 'NONE',  ( 147.1259762202154207, 275.8173294038533641, -0.6716460511724978710 ) ) ;
#17997 = CARTESIAN_POINT ( 'NONE',  ( 206.9676408587583296, 272.1685258403992975, 7.544050792475608169 ) ) ;
#17998 = ORIENTED_EDGE ( 'NONE', *, *, #21952, .F. ) ;
#17999 = AXIS2_PLACEMENT_3D ( 'NONE', #8281, #31559, #72093 ) ;
#18000 = CARTESIAN_POINT ( 'NONE',  ( 164.4963285489318991, 245.7309966251440301, -6.672251175510283794 ) ) ;
#18001 = CARTESIAN_POINT ( 'NONE',  ( -9.359816960141781550, 158.7365022471902023, 10.00000000000009592 ) ) ;
#18002 = CARTESIAN_POINT ( 'NONE',  ( -52.15214130626392830, 100.0173953888347569, -10.00000000000000000 ) ) ;
#18003 = CARTESIAN_POINT ( 'NONE',  ( 102.9345500736427113, 239.4244531367911293, -4.594050593750046652 ) ) ;
#18004 = CARTESIAN_POINT ( 'NONE',  ( 24.63222838094502265, 17.14754757982090894, -5.678558825948276656 ) ) ;
#18005 = CARTESIAN_POINT ( 'NONE',  ( 75.11766928578728653, 67.11905233721752495, 12.65062760071900705 ) ) ;
#18006 = CARTESIAN_POINT ( 'NONE',  ( 151.2671975087473015, 270.6445237267302559, 14.15418255155509542 ) ) ;
#18008 = PLANE ( 'NONE',  #78119 ) ;
#18007 = CARTESIAN_POINT ( 'NONE',  ( 195.8449251089225811, 291.4336346372613775, 16.14492769602857081 ) ) ;
#18009 = CARTESIAN_POINT ( 'NONE',  ( 204.6262888618301190, 272.9406470939589440, -9.753183039192979464 ) ) ;
#18010 = VERTEX_POINT ( 'NONE', #87064 ) ;
#18011 = CARTESIAN_POINT ( 'NONE',  ( 190.5804445141703241, 262.3181372627366841, -4.380721925984095932 ) ) ;
#18012 = CARTESIAN_POINT ( 'NONE',  ( 149.1486417047969155, 272.3139700178423368, -11.47583619705022606 ) ) ;
#18013 = ADVANCED_FACE ( 'NONE', ( #88061 ), #71314, .F. ) ;
#18014 = CARTESIAN_POINT ( 'NONE',  ( 190.5052505396941740, 300.1343187134208392, 3.427856936506675556 ) ) ;
#18015 = CARTESIAN_POINT ( 'NONE',  ( 176.0802790653596048, 291.8812439832981909, -1.090742048283624088 ) ) ;
#18016 = CARTESIAN_POINT ( 'NONE',  ( 81.52014092374062670, 55.46057516179622837, -16.31907950184206513 ) ) ;
#18017 = EDGE_LOOP ( 'NONE', ( #58025, #73842, #84091, #20892 ) ) ;
#18018 = CARTESIAN_POINT ( 'NONE',  ( 70.11864118459847361, 65.88152597758180207, -11.84054788745243414 ) ) ;
#18019 = CARTESIAN_POINT ( 'NONE',  ( 178.2382707639212356, 285.7843550335422833, 14.43266090959460435 ) ) ;
#18020 = CARTESIAN_POINT ( 'NONE',  ( 165.3873398078029595, 269.6810096676893522, -16.29630396821910310 ) ) ;
#18021 = CARTESIAN_POINT ( 'NONE',  ( 71.94719849994382344, 72.57089041204895352, 1.653882010069164021 ) ) ;
#18022 = CARTESIAN_POINT ( 'NONE',  ( 199.2993768369113354, 272.2699461441282551, 12.30839096982038505 ) ) ;
#18023 = CARTESIAN_POINT ( 'NONE',  ( 156.3272571654081275, 261.0848386047626377, 17.42342629828958067 ) ) ;
#18024 = CARTESIAN_POINT ( 'NONE',  ( 70.62781635888518394, 71.46971406967139728, 0.07536961296809761846 ) ) ;
#18025 = CARTESIAN_POINT ( 'NONE',  ( 148.4345653551533815, 274.8385398012493965, 7.278542558485217917 ) ) ;
#18026 = ORIENTED_EDGE ( 'NONE', *, *, #1004, .F. ) ;
#18027 = CARTESIAN_POINT ( 'NONE',  ( 190.8877596188617645, 280.8087401328753003, 16.64766537405279223 ) ) ;
#18028 = CARTESIAN_POINT ( 'NONE',  ( 41.62797693021462209, 26.96004757982093381, -5.678558825948276656 ) ) ;
#18029 = CARTESIAN_POINT ( 'NONE',  ( 195.3658642540283950, 290.3602234657191730, -16.70539931202024775 ) ) ;
#18030 = ORIENTED_EDGE ( 'NONE', *, *, #45339, .T. ) ;
#18031 = CARTESIAN_POINT ( 'NONE',  ( 167.7652100969719413, 280.9220867458556654, 12.66497483005768210 ) ) ;
#18032 = ADVANCED_FACE ( 'NONE', ( #87577 ), #50856, .F. ) ;
#18033 = CARTESIAN_POINT ( 'NONE',  ( 147.6095889327917803, 274.9796876144846465, -8.460961150142429332 ) ) ;
#18034 = CARTESIAN_POINT ( 'NONE',  ( 165.3053181839423473, 245.9328214431010338, -1.040564150934635057 ) ) ;
#18035 = ORIENTED_EDGE ( 'NONE', *, *, #46398, .T. ) ;
#18036 = CARTESIAN_POINT ( 'NONE',  ( 78.86410592861936664, 59.57720046317054852, 16.50785913320113352 ) ) ;
#18037 = FACE_OUTER_BOUND ( 'NONE', #87443, .T. ) ;
#18038 = CARTESIAN_POINT ( 'NONE',  ( 88.21629111658447187, 43.86250281267856366, -2.113840622537501268 ) ) ;
#18039 = CARTESIAN_POINT ( 'NONE',  ( 81.33978991279256832, 50.93462248752911137, -14.65978185948963386 ) ) ;
#18040 = CARTESIAN_POINT ( 'NONE',  ( 189.4949498660852214, 300.2643150046559413, 3.278686253974624432 ) ) ;
#18041 = CARTESIAN_POINT ( 'NONE',  ( 155.5322964227545413, 261.2571557083629159, -18.35853982030605280 ) ) ;
#18042 = EDGE_LOOP ( 'NONE', ( #93951, #30610, #89105, #89340 ) ) ;
#18043 = VERTEX_POINT ( 'NONE', #25189 ) ;
#18044 = CARTESIAN_POINT ( 'NONE',  ( 179.0484917649878298, 259.9789987921100192, 12.89662402083353854 ) ) ;
#18045 = ORIENTED_EDGE ( 'NONE', *, *, #86847, .T. ) ;
#18046 = CARTESIAN_POINT ( 'NONE',  ( 69.61542750552385428, 62.56132062511078828, -13.94275833699888700 ) ) ;
#18047 = ORIENTED_EDGE ( 'NONE', *, *, #88822, .T. ) ;
#18048 = CARTESIAN_POINT ( 'NONE',  ( 88.36883182482389998, 44.19992593570371042, 0.005427499793692280861 ) ) ;
#18049 = CARTESIAN_POINT ( 'NONE',  ( 78.93730744513115383, 51.88019286357000226, 15.41741368655081246 ) ) ;
#18050 = VERTEX_POINT ( 'NONE', #74191 ) ;
#18051 = CARTESIAN_POINT ( 'NONE',  ( 81.92045520014677606, 41.11899774358128923, 3.718728919965262225 ) ) ;
#18053 = CARTESIAN_POINT ( 'NONE',  ( 147.1889317863637530, 275.7082871646651370, -6.244700368100694732 ) ) ;
#18052 = B_SPLINE_CURVE_WITH_KNOTS ( 'NONE', 3,
 ( #48906, #72219, #33195, #3322 ),
 .UNSPECIFIED., .F., .F.,
 ( 4, 4 ),
 ( 0.02444194389405377615, 0.03368619770401917735 ),
 .UNSPECIFIED. ) ;
#18054 = CARTESIAN_POINT ( 'NONE',  ( 192.3030664838027519, 265.4539026115626257, 10.80274721496235735 ) ) ;
#18055 = FACE_OUTER_BOUND ( 'NONE', #26431, .T. ) ;
#18056 = CARTESIAN_POINT ( 'NONE',  ( 152.7375212135632125, 266.0978483664162582, -16.47968945089317572 ) ) ;
#18057 = CARTESIAN_POINT ( 'NONE',  ( 48.53010236944518851, 101.9116055364396090, -10.00000000000000000 ) ) ;
#18058 = CARTESIAN_POINT ( 'NONE',  ( 154.1353700909746181, 279.5493911791057826, 2.161561130678962606 ) ) ;
#18059 = CARTESIAN_POINT ( 'NONE',  ( 136.7913381204293728, 237.5327760586659736, 1.948934522072303157E-15 ) ) ;
#18060 = CARTESIAN_POINT ( 'NONE',  ( 42.32809528168264990, 126.1521775423068163, -10.00000000000000000 ) ) ;
#18061 = ORIENTED_EDGE ( 'NONE', *, *, #94144, .T. ) ;
#18063 = ORIENTED_EDGE ( 'NONE', *, *, #88355, .T. ) ;
#18062 = CARTESIAN_POINT ( 'NONE',  ( 25.72017957606892580, 26.80066082961422680, 10.00000000000000533 ) ) ;
#18064 = CARTESIAN_POINT ( 'NONE',  ( 203.5186246619243207, 276.4695941624181046, 13.73756916699280417 ) ) ;
#18065 = ADVANCED_FACE ( 'NONE', ( #35663 ), #9766, .F. ) ;
#18066 = CARTESIAN_POINT ( 'NONE',  ( 179.6182561431837428, 255.5231795168529345, 1.315866801863230240 ) ) ;
#18067 = CARTESIAN_POINT ( 'NONE',  ( 172.5766600205861607, 288.7097676792643028, -4.646140225306805149 ) ) ;
#18068 = DIRECTION ( 'NONE',  ( -2.816764622163176506E-16, -1.626259812849726205E-16, 1.000000000000000000 ) ) ;
#18069 = CARTESIAN_POINT ( 'NONE',  ( 157.3706863651409549, 280.2504512272545867, -7.019172882110545686 ) ) ;
#18070 = FACE_OUTER_BOUND ( 'NONE', #68635, .T. ) ;
#18071 = CARTESIAN_POINT ( 'NONE',  ( 78.14015596333129565, 47.79605781546002419, 14.53813849205122466 ) ) ;
#18072 = DIRECTION ( 'NONE',  ( 0.000000000000000000, -0.000000000000000000, 1.000000000000000000 ) ) ;
#18073 = AXIS2_PLACEMENT_3D ( 'NONE', #2328, #72746, #3339 ) ;
#18074 = CARTESIAN_POINT ( 'NONE',  ( 195.1239386621870437, 291.9024892941676512, 15.58172254008325019 ) ) ;
#18075 = VERTEX_POINT ( 'NONE', #6253 ) ;
#18076 = CARTESIAN_POINT ( 'NONE',  ( 195.3887114072277882, 286.2014090520565901, -17.68059800431107220 ) ) ;
#18077 = CARTESIAN_POINT ( 'NONE',  ( 152.7506372714153713, 273.5640845184121872, 11.93689953919982649 ) ) ;
#18078 = ORIENTED_EDGE ( 'NONE', *, *, #32798, .T. ) ;
#18079 = CARTESIAN_POINT ( 'NONE',  ( -19.65312891409030271, 93.06504152958497400, 59.99999999999999289 ) ) ;
#18080 = EDGE_CURVE ( 'NONE', #17465, #42705, #52846, .T. ) ;
#18081 = CARTESIAN_POINT ( 'NONE',  ( 204.2869422847054182, 269.1846276741756014, -2.932770657268202630 ) ) ;
#18082 = CARTESIAN_POINT ( 'NONE',  ( 191.4039669030298967, 299.1255998841573387, -10.25374536856971019 ) ) ;
#18083 = CARTESIAN_POINT ( 'NONE',  ( 79.14312167556931854, 57.64441083166269664, 0.000000000000000000 ) ) ;
#18084 = CARTESIAN_POINT ( 'NONE',  ( 202.8787628851569593, 279.2506702366259788, 17.01435431865322556 ) ) ;
#18086 = CARTESIAN_POINT ( 'NONE',  ( 151.4858105020860251, 274.9918459198586902, -8.658055901311536573 ) ) ;
#18085 = CARTESIAN_POINT ( 'NONE',  ( 164.5423507617603320, 283.6868644380134583, -6.754471756332288024 ) ) ;
#18087 = CARTESIAN_POINT ( 'NONE',  ( -22.42236680055709641, 157.8615022471902591, 0.000000000000000000 ) ) ;
#18088 = ORIENTED_EDGE ( 'NONE', *, *, #70149, .F. ) ;
#18089 = CARTESIAN_POINT ( 'NONE',  ( 71.09431784387571440, 62.57662900256345750, -13.84435817819633385 ) ) ;
#18090 = CARTESIAN_POINT ( 'NONE',  ( -19.65312891409030271, 93.06504152958497400, 177.5919119679930134 ) ) ;
#18091 = CARTESIAN_POINT ( 'NONE',  ( 15.10771242554802463, 167.9824982072973967, -5.229199737892075682E-14 ) ) ;
#18092 = CARTESIAN_POINT ( 'NONE',  ( 192.1859061758433143, 297.7712413352111298, 11.15082371775444336 ) ) ;
#18093 = CARTESIAN_POINT ( 'NONE',  ( 80.72890526444484749, 43.21432171413569989, -9.149766045926375213 ) ) ;
#18094 = CARTESIAN_POINT ( 'NONE',  ( 69.09200187819043038, 70.53478952123415979, 0.07191778000971091322 ) ) ;
#18095 = CARTESIAN_POINT ( 'NONE',  ( -3.938137090306929711, 168.5333772461660828, 9.188101187500095079 ) ) ;
#18096 = CARTESIAN_POINT ( 'NONE',  ( 87.93867815554295930, 44.50532786965745657, -3.967150898595685593 ) ) ;
#18097 = DIRECTION ( 'NONE',  ( -0.000000000000000000, -0.000000000000000000, -1.000000000000000000 ) ) ;
#18098 = LINE ( 'NONE', #97136, #12433 ) ;
#18099 = CARTESIAN_POINT ( 'NONE',  ( 78.68575686975825079, 59.63804999145194330, 16.14434349017544434 ) ) ;
#18100 = LINE ( 'NONE', #41379, #46965 ) ;
#18101 = CARTESIAN_POINT ( 'NONE',  ( 163.3065739647292673, 284.2937766533170247, 6.003775226036714763 ) ) ;
#18103 = CARTESIAN_POINT ( 'NONE',  ( 163.1096928939807924, 248.1327200311062882, -9.690381021358412283 ) ) ;
#18102 = CARTESIAN_POINT ( 'NONE',  ( 44.35815684012577265, 67.96982248125696913, -10.00000000000000000 ) ) ;
#18104 = CARTESIAN_POINT ( 'NONE',  ( 207.7730309186906084, 270.7735493366856190, 6.335709893618091115 ) ) ;
#18105 = CARTESIAN_POINT ( 'NONE',  ( -56.14442822474984496, 33.32908021129815523, -10.00000000000000000 ) ) ;
#18106 = CARTESIAN_POINT ( 'NONE',  ( 168.3557124657904467, 273.6222795104500278, 17.14480014634877136 ) ) ;
#18107 = CARTESIAN_POINT ( 'NONE',  ( 78.15040261416261558, 55.05491506378064059, -16.09679860028264287 ) ) ;
#18108 = LINE ( 'NONE', #97142, #18909 ) ;
#18109 = CARTESIAN_POINT ( 'NONE',  ( 66.63175369249636049, 68.36105297849150020, -4.334338317156124276 ) ) ;
#18110 = CARTESIAN_POINT ( 'NONE',  ( 48.37494963522306080, 207.9244531367911293, -4.594050593750046652 ) ) ;
#18111 = DIRECTION ( 'NONE',  ( 0.000000000000000000, 0.000000000000000000, -1.000000000000000000 ) ) ;
#18112 = CARTESIAN_POINT ( 'NONE',  ( 76.25066296318219372, 205.6423013555409796, -4.594050593750043987 ) ) ;
#18113 = CARTESIAN_POINT ( 'NONE',  ( 207.7836085030675690, 270.7552284231231852, -5.468305433308493058 ) ) ;
#18114 = PLANE ( 'NONE',  #13620 ) ;
#18115 = DIRECTION ( 'NONE',  ( 0.000000000000000000, 0.000000000000000000, 1.000000000000000000 ) ) ;
#18117 = CARTESIAN_POINT ( 'NONE',  ( 152.1020077497548755, 267.1985899746260316, 15.41056800135520710 ) ) ;
#18116 = DIRECTION ( 'NONE',  ( 0.2837547813814357833, 0.9281390619545413223, -0.2409172175609659572 ) ) ;
#18118 = DIRECTION ( 'NONE',  ( -0.000000000000000000, 0.000000000000000000, -1.000000000000000000 ) ) ;
#18119 = EDGE_CURVE ( 'NONE', #90508, #90974, #73298, .T. ) ;
#18120 = CARTESIAN_POINT ( 'NONE',  ( 31.19238438139944947, 38.98502408145593989, -5.678558825948271327 ) ) ;
#18121 = CARTESIAN_POINT ( 'NONE',  ( 81.89326088175978668, 48.07889234901487896, 13.52455100267233234 ) ) ;
#18122 = CARTESIAN_POINT ( 'NONE',  ( 84.58903325794560146, 46.78888499796955358, -10.74999075493416356 ) ) ;
#18123 = EDGE_LOOP ( 'NONE', ( #74128, #30834, #99, #77737 ) ) ;
#18124 = CARTESIAN_POINT ( 'NONE',  ( 21.69737781089059681, 21.03085787977762777, 9.188101187500006262 ) ) ;
#18125 = CARTESIAN_POINT ( 'NONE',  ( 78.09096694622414248, 206.7048013555409796, 4.594050593750051981 ) ) ;
#18126 = CARTESIAN_POINT ( 'NONE',  ( 32.07315653955450330, 47.77038272570916888, 10.00000000000000000 ) ) ;
#18127 = DIRECTION ( 'NONE',  ( -0.000000000000000000, -1.000000000000000000, -0.000000000000000000 ) ) ;
#18128 = CARTESIAN_POINT ( 'NONE',  ( -30.04356256989558815, 94.88921800892795488, 12.63376007436073323 ) ) ;
#18129 = CARTESIAN_POINT ( 'NONE',  ( 154.1134794093426592, 263.7146188622353407, 17.41994999336771244 ) ) ;
#18130 = EDGE_CURVE ( 'NONE', #48457, #82532, #76182, .T. ) ;
#18131 = CARTESIAN_POINT ( 'NONE',  ( 5.968649350820472321, 188.6868197944958752, 22.50000000000001421 ) ) ;
#18132 = CARTESIAN_POINT ( 'NONE',  ( 191.0557287345794180, 287.0893601664016614, 16.13915540770992152 ) ) ;
#18133 = CARTESIAN_POINT ( 'NONE',  ( 136.0806360202347491, 237.8262482093457493, 3.021315404115420679E-15 ) ) ;
#18134 = CARTESIAN_POINT ( 'NONE',  ( 87.58584962094528237, 45.11644481794071737, -6.124215339656664980 ) ) ;
#18135 = CARTESIAN_POINT ( 'NONE',  ( 129.0599100780710558, 231.9865022471901455, 1.119607411625061291E-15 ) ) ;
#18136 = DIRECTION ( 'NONE',  ( 0.000000000000000000, 0.000000000000000000, -1.000000000000000000 ) ) ;
#18137 = CARTESIAN_POINT ( 'NONE',  ( 74.72358351985596414, 53.61584409156186126, 16.08411429754375277 ) ) ;
#18138 = ORIENTED_EDGE ( 'NONE', *, *, #22512, .T. ) ;
#18139 = CARTESIAN_POINT ( 'NONE',  ( 82.07917488340794421, 54.03863367488002467, 15.60468158849540998 ) ) ;
#18140 = ORIENTED_EDGE ( 'NONE', *, *, #3900, .T. ) ;
#18141 = CARTESIAN_POINT ( 'NONE',  ( 163.1014434023538513, 248.1470085697407058, 9.692260209037655727 ) ) ;
#18142 = PLANE ( 'NONE',  #14222 ) ;
#18143 = EDGE_CURVE ( 'NONE', #57886, #33116, #32177, .T. ) ;
#18144 = CARTESIAN_POINT ( 'NONE',  ( 149.8050492866161392, 271.5723974896224604, -11.69608657949948061 ) ) ;
#18145 = EDGE_LOOP ( 'NONE', ( #20571, #24275, #26289, #2210 ) ) ;
#18146 = DIRECTION ( 'NONE',  ( -1.000000000000000000, 0.000000000000000000, 0.000000000000000000 ) ) ;
#18147 = VERTEX_POINT ( 'NONE', #70541 ) ;
#18148 = CARTESIAN_POINT ( 'NONE',  ( 72.05417303993513656, 71.64307123591491688, 5.506498905688411050 ) ) ;
#18149 = CARTESIAN_POINT ( 'NONE',  ( 147.8505793332463725, 274.5622799967613332, -9.317516487097901035 ) ) ;
#18150 = CARTESIAN_POINT ( 'NONE',  ( 148.5802502259396647, 273.7349012789782137, 8.359561399005384530 ) ) ;
#18151 = VERTEX_POINT ( 'NONE', #41126 ) ;
#18152 = CARTESIAN_POINT ( 'NONE',  ( 31.98863997849372254, 36.65586893147758474, -7.433330006724137462 ) ) ;
#18153 = CARTESIAN_POINT ( 'NONE',  ( 79.83020946089156666, 44.72169397376073618, 11.27752533527092282 ) ) ;
#18154 = CARTESIAN_POINT ( 'NONE',  ( 84.83002093244189723, 50.29676582423640241, -13.82165720535206788 ) ) ;
#18155 = CARTESIAN_POINT ( 'NONE',  ( 5.783292089056025098, 27.85010085989870277, 10.00000000000000000 ) ) ;
#18156 = CARTESIAN_POINT ( 'NONE',  ( 168.0771236874269334, 276.6984061524693175, 15.22277158092185978 ) ) ;
#18157 = ADVANCED_FACE ( 'NONE', ( #23938 ), #32552, .T. ) ;
#18158 = DIRECTION ( 'NONE',  ( 0.4737039832092511671, 0.8806841296921895657, 0.000000000000000000 ) ) ;
#18159 = ORIENTED_EDGE ( 'NONE', *, *, #31086, .T. ) ;
#18160 = ORIENTED_EDGE ( 'NONE', *, *, #23514, .F. ) ;
#18161 = CARTESIAN_POINT ( 'NONE',  ( 183.0745236532343370, 295.8212215650241887, 0.6855209140772098309 ) ) ;
#18163 = CARTESIAN_POINT ( 'NONE',  ( 147.9133274879049793, 274.4535970048112290, -9.359166267164972908 ) ) ;
#18162 = CARTESIAN_POINT ( 'NONE',  ( 164.0741338217690668, 246.4622593432776796, 7.359073626423302983 ) ) ;
#18164 = CARTESIAN_POINT ( 'NONE',  ( 207.9743173328493526, 270.4249110404894054, -2.481515874287090639 ) ) ;
#18165 = CARTESIAN_POINT ( 'NONE',  ( 194.1011995340913074, 294.4538559273262877, 13.93949783759920713 ) ) ;
#18166 = CARTESIAN_POINT ( 'NONE',  ( 185.2119534494709967, 292.8366621963887724, -11.93359106299072359 ) ) ;
#18167 = CARTESIAN_POINT ( 'NONE',  ( 157.6500260163024620, 257.5891404556457474, -18.23450497588216379 ) ) ;
#18168 = CARTESIAN_POINT ( 'NONE',  ( 207.3563322976324912, 271.4952925198022058, -4.480576336268985216 ) ) ;
#18169 = CARTESIAN_POINT ( 'NONE',  ( 166.3373473137807252, 265.5045842688243738, 16.55012934221398169 ) ) ;
#18170 = FACE_OUTER_BOUND ( 'NONE', #54256, .T. ) ;
#18171 = CARTESIAN_POINT ( 'NONE',  ( 90.40467888234286420, 216.8768266524159856, -9.188101187500091527 ) ) ;
#18172 = ORIENTED_EDGE ( 'NONE', *, *, #44241, .F. ) ;
#18173 = CARTESIAN_POINT ( 'NONE',  ( 150.1167764007130643, 271.3850789835987030, 12.27179235466227603 ) ) ;
#18174 = CARTESIAN_POINT ( 'NONE',  ( 80.86586985908986946, 155.7185146834693512, 0.000000000000000000 ) ) ;
#18175 = ORIENTED_EDGE ( 'NONE', *, *, #9958, .T. ) ;
#18176 = AXIS2_PLACEMENT_3D ( 'NONE', #42892, #4942, #81464 ) ;
#18177 = CARTESIAN_POINT ( 'NONE',  ( 168.2073321238995049, 267.1113765662216792, -17.52088750715768484 ) ) ;
#18178 = ORIENTED_EDGE ( 'NONE', *, *, #32022, .T. ) ;
#18179 = VERTEX_POINT ( 'NONE', #94386 ) ;
#18180 = EDGE_CURVE ( 'NONE', #58645, #5821, #10251, .T. ) ;
#18181 = CARTESIAN_POINT ( 'NONE',  ( 12.69602586335324190, 7.734156793818200981, -2.889640176918245968E-15 ) ) ;
#18182 = ADVANCED_FACE ( 'NONE', ( #47731 ), #1158, .T. ) ;
#18183 = CARTESIAN_POINT ( 'NONE',  ( 84.00308638938395234, 207.7592609112379876, 2.679491924311254714 ) ) ;
#18185 = B_SPLINE_SURFACE_WITH_KNOTS ( 'NONE', 3, 1, ( 
 ( #43318, #82876 ),
 ( #50923, #21056 ),
 ( #74264, #81873 ),
 ( #51935, #34729 ),
 ( #73742, #36716 ),
 ( #58034, #59002 ),
 ( #98552, #82390 ),
 ( #29141, #35733 ),
 ( #66630, #60010 ),
 ( #20549, #90975 ),
 ( #51427, #21535 ),
 ( #43821, #52417 ),
 ( #65628, #27149 ),
 ( #4333, #13875 ),
 ( #12907, #59958 ),
 ( #37654, #43265 ),
 ( #50875, #74210 ),
 ( #90930, #43766 ),
 ( #21480, #5773 ),
 ( #81824, #19996 ),
 ( #58948, #60453 ),
 ( #83814, #74710 ),
 ( #75689, #58468 ),
 ( #28572, #4800 ),
 ( #21971, #14381 ),
 ( #52368, #36662 ),
 ( #35681, #36166 ),
 ( #76199, #51371 ),
 ( #90433, #59452 ),
 ( #21005, #83313 ),
 ( #13395, #44756 ),
 ( #51886, #66583 ),
 ( #6775, #82827 ),
 ( #82339, #67569 ) ),
 .UNSPECIFIED., .T., .F., .F.,
 ( 4, 2, 2, 2, 2, 2, 2, 2, 2, 2, 2, 2, 2, 2, 2, 2, 4 ),
 ( 2, 2 ),
 ( 0.000000000000000000, 0.06250000000000000000, 0.1250000000000000000, 0.1875000000000000000, 0.2500000000000000000, 0.3125000000000000000, 0.3750000000000000000, 0.4375000000000000000, 0.5000000000000000000, 0.5625000000000000000, 0.6250000000000000000, 0.6875000000000000000, 0.7500000000000000000, 0.8125000000000000000, 0.8750000000000000000, 0.9375000000000000000, 1.000000000000000000 ),
 ( 0.000000000000000000, 1.000000000000000000 ),
 .UNSPECIFIED. ) ;
#18184 = CARTESIAN_POINT ( 'NONE',  ( 191.0702043019150835, 299.7036936669546776, -8.800021049343948576 ) ) ;
#18186 = CARTESIAN_POINT ( 'NONE',  ( 27.21537010445218741, 39.21091486745862653, 7.012934429366973338E-14 ) ) ;
#18187 = CARTESIAN_POINT ( 'NONE',  ( 47.84007798744510609, 106.1754093786579318, -10.00000000000000000 ) ) ;
#18188 = CARTESIAN_POINT ( 'NONE',  ( 162.4993287900620942, 249.1899016702093661, 10.54298717179175071 ) ) ;
#18189 = CARTESIAN_POINT ( 'NONE',  ( 102.2314250767153538, 220.6423013555409796, -4.594050593750043987 ) ) ;
#18190 = ORIENTED_EDGE ( 'NONE', *, *, #64591, .T. ) ;
#18191 = EDGE_CURVE ( 'NONE', #98201, #61436, #31536, .T. ) ;
#18192 = ORIENTED_EDGE ( 'NONE', *, *, #95990, .F. ) ;
#18193 = CARTESIAN_POINT ( 'NONE',  ( 118.5773942495489166, 239.2677522451418497, 10.00000000000009592 ) ) ;
#18194 = CARTESIAN_POINT ( 'NONE',  ( 162.7070706717508699, 248.8300821762643693, -9.986337079333621247 ) ) ;
#18195 = ORIENTED_EDGE ( 'NONE', *, *, #26405, .T. ) ;
#18196 = EDGE_CURVE ( 'NONE', #5695, #15552, #63943, .T. ) ;
#18197 = CARTESIAN_POINT ( 'NONE',  ( 76.05882932919557504, 64.70680307606549775, -14.35248828871676174 ) ) ;
#18198 = FACE_OUTER_BOUND ( 'NONE', #58373, .T. ) ;
#18199 = LINE ( 'NONE', #46193, #15574 ) ;
#18200 = CARTESIAN_POINT ( 'NONE',  ( 48.32408078245681793, 82.80331927372955647, 10.00000000000000000 ) ) ;
#18201 = CARTESIAN_POINT ( 'NONE',  ( 88.22177397292790602, 44.42207723138842113, 4.484962078095955818 ) ) ;
#18202 = ORIENTED_EDGE ( 'NONE', *, *, #31534, .F. ) ;
#18203 = CARTESIAN_POINT ( 'NONE',  ( 204.6163864379986705, 276.2410179586759682, 14.66911174422491726 ) ) ;
#18204 = EDGE_CURVE ( 'NONE', #65871, #22415, #91431, .T. ) ;
#18205 = CARTESIAN_POINT ( 'NONE',  ( 160.6175188173358492, 275.6489243641970575, 12.85245945024576564 ) ) ;
#18206 = CARTESIAN_POINT ( 'NONE',  ( 82.18503486167877270, 40.60955881824741454, -3.312051805122440129 ) ) ;
#18207 = EDGE_CURVE ( 'NONE', #23003, #65011, #30936, .T. ) ;
#18208 = CARTESIAN_POINT ( 'NONE',  ( 188.8357241328549492, 269.5691870241041102, 14.73685245099255958 ) ) ;
#18209 = CARTESIAN_POINT ( 'NONE',  ( 183.3702726886198491, 288.7829620135148048, 14.41901549737766253 ) ) ;
#18210 = CARTESIAN_POINT ( 'NONE',  ( -32.04500338604974985, 25.44370296803430520, -10.00000000000000000 ) ) ;
#18211 = CARTESIAN_POINT ( 'NONE',  ( 147.6497331045811734, 249.4111022060903622, 10.00000000000009770 ) ) ;
#18212 = ORIENTED_EDGE ( 'NONE', *, *, #57306, .F. ) ;
#18213 = CARTESIAN_POINT ( 'NONE',  ( 149.0580910181880654, 274.3322375007426217, 9.004245725843048831 ) ) ;
#18214 = CARTESIAN_POINT ( 'NONE',  ( 161.4469036912142599, 251.0127554125742222, 12.93933463576739307 ) ) ;
#18215 = CARTESIAN_POINT ( 'NONE',  ( 84.94422939829060226, 43.49408491451843162, 5.705947650134866933 ) ) ;
#18216 = CARTESIAN_POINT ( 'NONE',  ( 167.9211111253673323, 249.4040118433879627, 8.061254949035708606 ) ) ;
#18217 = CARTESIAN_POINT ( 'NONE',  ( 77.92147852599414648, 62.01641577372943459, 15.66086047352921540 ) ) ;
#18218 = CARTESIAN_POINT ( 'NONE',  ( 176.7048560268192716, 290.6280913003972728, -6.170303688665058850 ) ) ;
#18219 = CARTESIAN_POINT ( 'NONE',  ( 162.9935763125246240, 248.3338398497890580, -10.29128364753544034 ) ) ;
#18220 = ORIENTED_EDGE ( 'NONE', *, *, #12183, .F. ) ;
#18221 = CARTESIAN_POINT ( 'NONE',  ( 164.9779129355220562, 244.8968679994381148, -1.771286574179712803 ) ) ;
#18223 = CARTESIAN_POINT ( 'NONE',  ( 184.6099029562445253, 266.0940484426244552, 13.19535090614431816 ) ) ;
#18222 = CARTESIAN_POINT ( 'NONE',  ( 179.1221870662444928, 265.9242797405647138, -14.83509186512012867 ) ) ;
#18224 = DIRECTION ( 'NONE',  ( 0.9041295198386993803, -0.4272584830711297910, 0.000000000000000000 ) ) ;
#18225 = CARTESIAN_POINT ( 'NONE',  ( 30.46276441966746518, 39.36126292948897998, 6.180339887498949913 ) ) ;
#18226 = CARTESIAN_POINT ( 'NONE',  ( 192.2943420783192323, 297.5834248427583475, 12.53393473147773562 ) ) ;
#18227 = PLANE ( 'NONE',  #59428 ) ;
#18228 = CARTESIAN_POINT ( 'NONE',  ( 71.85869513609316073, 58.67586711399008692, -15.48493562761569287 ) ) ;
#18229 = CARTESIAN_POINT ( 'NONE',  ( 82.87443698061515818, 43.21958489367609957, -7.413545511274116429 ) ) ;
#18230 = CARTESIAN_POINT ( 'NONE',  ( 28.58622839714300667, 60.96364432824390178, 59.99999999999999289 ) ) ;
#18231 =( BOUNDED_CURVE ( )  B_SPLINE_CURVE ( 2, ( #659, #84798, #45742, #84307, #22949, #76192, #69051, #85305, #70046 ),
 .UNSPECIFIED., .F., .T. ) 
 B_SPLINE_CURVE_WITH_KNOTS ( ( 3, 2, 2, 2, 3 ),
 ( 0.3911290322580645018, 0.3924731182795698770, 0.3951612903225806273, 0.3978494623655913776, 0.3991935483870967527 ),
 .UNSPECIFIED. ) 
 CURVE ( )  GEOMETRIC_REPRESENTATION_ITEM ( )  RATIONAL_B_SPLINE_CURVE ( ( 0.9330127018922194093, 0.9330127018922194093, 1.000000000000000000, 0.8660254037844387076, 1.000000000000000000, 0.8660254037844387076, 1.000000000000000000, 0.9330127018922194093, 0.9330127018922194093 ) ) 
 REPRESENTATION_ITEM ( '' )  );
#18232 = CARTESIAN_POINT ( 'NONE',  ( 10.86574497745707646, 167.8923013555410080, 4.594050593750050204 ) ) ;
#18233 = B_SPLINE_CURVE_WITH_KNOTS ( 'NONE', 3,
 ( #13991, #66687, #36780, #74819, #83425, #52477, #52979, #22581, #6877, #67182, #45372, #4907, #98617, #13507, #67688, #44377, #76305, #61065, #30177, #59568 ),
 .UNSPECIFIED., .F., .F.,
 ( 4, 2, 2, 2, 2, 2, 2, 2, 2, 4 ),
 ( 0.003620162585681084913, 0.003755372724757697310, 0.003890582863834310141, 0.004025793002910922971, 0.004161003141987535368, 0.004431423420140844296, 0.004701843698294154092, 0.005242684254600804040, 0.005783524810907454856, 0.007946887036134204704 ),
 .UNSPECIFIED. ) ;
#18234 = CARTESIAN_POINT ( 'NONE',  ( 82.77577997019196232, 50.05166863141886324, 13.88734606986174924 ) ) ;
#18235 = VERTEX_POINT ( 'NONE', #79675 ) ;
#18236 = CARTESIAN_POINT ( 'NONE',  ( 86.80989918712758424, 45.87808919071956382, 8.896275332294523608 ) ) ;
#18237 = PLANE ( 'NONE',  #77460 ) ;
#18238 = CARTESIAN_POINT ( 'NONE',  ( 202.9461111005703913, 274.5853058359568308, -12.78354684315880618 ) ) ;
#18239 = CARTESIAN_POINT ( 'NONE',  ( -50.66096862766640641, 31.69950886434491721, 10.00000000000000000 ) ) ;
#18240 = CARTESIAN_POINT ( 'NONE',  ( 34.35668405510998724, 181.4548013555409796, -4.594050593750042211 ) ) ;
#18241 = AXIS2_PLACEMENT_3D ( 'NONE', #6264, #98982, #83304 ) ;
#18242 = AXIS2_PLACEMENT_3D ( 'NONE', #67945, #98865, #61323 ) ;
#18243 = CARTESIAN_POINT ( 'NONE',  ( 200.4403816905005158, 283.4740703539914648, 16.81798557643505987 ) ) ;
#18244 = CARTESIAN_POINT ( 'NONE',  ( 22.01921768174555893, 36.21091486745860522, -1.111400068045478839E-16 ) ) ;
#18245 = CARTESIAN_POINT ( 'NONE',  ( 41.80280824456575317, 23.94473085651394939, 1.475505719884397138E-15 ) ) ;
#18246 = CARTESIAN_POINT ( 'NONE',  ( 181.3918697797460311, 294.4956595908585086, 6.501009157982572617 ) ) ;
#18247 = FACE_OUTER_BOUND ( 'NONE', #12844, .T. ) ;
#18248 = DIRECTION ( 'NONE',  ( -0.4851478631379979034, 0.8403007481384877631, 0.2419218955996582654 ) ) ;
#18249 = CARTESIAN_POINT ( 'NONE',  ( 165.8975677354378035, 271.5909624305264174, 17.28637137770206067 ) ) ;
#18250 = CARTESIAN_POINT ( 'NONE',  ( 87.16825469001011584, 46.28910860497907009, -8.521112165214120182 ) ) ;
#18251 = AXIS2_PLACEMENT_3D ( 'NONE', #75093, #53262, #5672 ) ;
#18252 = CARTESIAN_POINT ( 'NONE',  ( 83.43050110256683638, 51.89332412091457059, 15.00139857044201896 ) ) ;
#18253 = CARTESIAN_POINT ( 'NONE',  ( 95.28491933047791917, 212.4865022471901455, 1.119607411625061291E-15 ) ) ;
#18254 = CARTESIAN_POINT ( 'NONE',  ( 164.6319316456770139, 246.1186112673341597, 1.146231737620790891 ) ) ;
#18255 = CARTESIAN_POINT ( 'NONE',  ( 183.3350989353408806, 260.3215222104232680, -10.84733429619501699 ) ) ;
#18256 = CARTESIAN_POINT ( 'NONE',  ( 39.14627965220388006, 205.6589784336661637, -6.496448406907675876E-16 ) ) ;
#18257 = DIRECTION ( 'NONE',  ( 0.4999999999999992784, -0.8660254037844390407, 0.000000000000000000 ) ) ;
#18258 = ORIENTED_EDGE ( 'NONE', *, *, #8184, .F. ) ;
#18259 = CARTESIAN_POINT ( 'NONE',  ( -17.94336299062649687, 80.50122156528269102, 14.21411446845087845 ) ) ;
#18260 = CARTESIAN_POINT ( 'NONE',  ( 147.5813496936708020, 275.0285994114094592, 4.516581957185684004 ) ) ;
#18261 = EDGE_CURVE ( 'NONE', #48830, #17141, #80171, .T. ) ;
#18262 = CARTESIAN_POINT ( 'NONE',  ( 67.25222559693544611, 66.46721440497699973, -8.699209683962450868 ) ) ;
#18263 = VERTEX_POINT ( 'NONE', #87802 ) ;
#18265 = CARTESIAN_POINT ( 'NONE',  ( 168.7715202826167911, 285.3210262249357356, 7.552708256878819526 ) ) ;
#18264 = AXIS2_PLACEMENT_3D ( 'NONE', #86394, #93475, #24027 ) ;
#18266 = CARTESIAN_POINT ( 'NONE',  ( 168.0576292222695542, 281.8341897004820567, -11.13511954253887914 ) ) ;
#18267 = DIRECTION ( 'NONE',  ( 0.4999999999999998890, -0.8660254037844385966, 0.000000000000000000 ) ) ;
#18268 = CARTESIAN_POINT ( 'NONE',  ( 86.83108767939293671, 232.4860189848785410, -2.679491924311252493 ) ) ;
#18269 = CARTESIAN_POINT ( 'NONE',  ( 22.71735025659390317, 28.51421378149919406, -9.188101187500004485 ) ) ;
#18270 = CARTESIAN_POINT ( 'NONE',  ( 163.2835940097493790, 247.8315144631017404, 11.08416305054517359 ) ) ;
#18271 = CARTESIAN_POINT ( 'NONE',  ( 149.3141802193904368, 272.0272488999566463, -11.40332369054239336 ) ) ;
#18272 = CARTESIAN_POINT ( 'NONE',  ( 171.3930954440937739, 255.6893612109813034, 11.28323771083614524 ) ) ;
#18273 = ORIENTED_EDGE ( 'NONE', *, *, #65194, .T. ) ;
#18274 = CARTESIAN_POINT ( 'NONE',  ( 10.08301516415377641, 26.79752408145591147, -5.678558825948271327 ) ) ;
#18275 = CARTESIAN_POINT ( 'NONE',  ( 90.04477061917849312, 44.76220097505219542, 0.000000000000000000 ) ) ;
#18276 = CARTESIAN_POINT ( 'NONE',  ( 171.8875188505430458, 252.3843871569532098, 8.791676787938541793 ) ) ;
#18277 = LINE ( 'NONE', #49172, #39174 ) ;
#18278 = ADVANCED_FACE ( 'NONE', ( #49237 ), #57811, .F. ) ;
#18279 = ORIENTED_EDGE ( 'NONE', *, *, #69198, .F. ) ;
#18280 = CARTESIAN_POINT ( 'NONE',  ( 179.1455725186695815, 282.4470739261427639, 15.26283603612785988 ) ) ;
#18281 = CARTESIAN_POINT ( 'NONE',  ( 85.51452730306243666, 49.05009231135860404, 12.30971062534492866 ) ) ;
#18282 = EDGE_CURVE ( 'NONE', #99384, #50939, #27437, .T. ) ;
#18283 = DIRECTION ( 'NONE',  ( -0.9616534368410322164, 0.2742675106749447034, 0.000000000000000000 ) ) ;
#18284 = CARTESIAN_POINT ( 'NONE',  ( 69.36019124367645361, 65.42472516583706010, -11.87354268267799995 ) ) ;
#18285 = VERTEX_POINT ( 'NONE', #58312 ) ;
#18286 = VERTEX_POINT ( 'NONE', #19836 ) ;
#18288 = FACE_OUTER_BOUND ( 'NONE', #87604, .T. ) ;
#18287 = CARTESIAN_POINT ( 'NONE',  ( 188.5138031843794124, 273.5367886141518738, -15.67519387171974543 ) ) ;
#18289 = CARTESIAN_POINT ( 'NONE',  ( 149.3629284598386278, 271.9428144707212027, -12.99253781774931049 ) ) ;
#18290 = VERTEX_POINT ( 'NONE', #50708 ) ;
#18291 = CARTESIAN_POINT ( 'NONE',  ( 41.88317952681261858, 32.38052372038644933, 10.00000000000000533 ) ) ;
#18292 = CARTESIAN_POINT ( 'NONE',  ( 191.6399467885100876, 261.9049270161082177, -5.586019516979663813 ) ) ;
#18293 = CARTESIAN_POINT ( 'NONE',  ( 70.57990371369005800, 71.55749465124115716, -3.025387803121589059 ) ) ;
#18294 = CARTESIAN_POINT ( 'NONE',  ( 78.23407395591094371, 61.03864688087466561, -15.91017056289256715 ) ) ;
#18295 = DIRECTION ( 'NONE',  ( 0.8660254037844379305, 0.5000000000000014433, 0.000000000000000000 ) ) ;
#18296 = CARTESIAN_POINT ( 'NONE',  ( 116.7102005222951817, 232.0643266524159856, -9.188101187500093303 ) ) ;
#18297 = CARTESIAN_POINT ( 'NONE',  ( 80.83312040127709963, 224.1427522451419065, -10.00000000000009592 ) ) ;
#18298 = EDGE_LOOP ( 'NONE', ( #13816, #71034, #56541, #23016 ) ) ;
#18299 = CARTESIAN_POINT ( 'NONE',  ( 163.8398374448017591, 246.8680725722146008, -5.948785025486735378 ) ) ;
#18300 = ORIENTED_EDGE ( 'NONE', *, *, #5026, .F. ) ;
#18301 = CARTESIAN_POINT ( 'NONE',  ( 36.24780089259745353, 32.87878583063844218, -9.188101187500006262 ) ) ;
#18302 = CARTESIAN_POINT ( 'NONE',  ( 75.15191903148871688, 52.97183600646508239, -16.48001256418180915 ) ) ;
#18303 = CARTESIAN_POINT ( 'NONE',  ( 204.8009505137602844, 275.5216285192182113, -12.34812582524854285 ) ) ;
#18304 = CARTESIAN_POINT ( 'NONE',  ( 62.47501251452969484, 213.0024278399160949, -9.188101187500093303 ) ) ;
#18305 = CARTESIAN_POINT ( 'NONE',  ( 74.39896838111268096, 68.39356553035000275, 11.30479640254015195 ) ) ;
#18306 = FACE_OUTER_BOUND ( 'NONE', #92820, .T. ) ;
#18307 = CARTESIAN_POINT ( 'NONE',  ( 183.9509481277042937, 296.4026742571778641, 5.972361342789342942 ) ) ;
#18308 = CARTESIAN_POINT ( 'NONE',  ( 173.2210010745182842, 271.2950951356299925, 16.42349981143101090 ) ) ;
#18309 = VERTEX_POINT ( 'NONE', #81661 ) ;
#18310 = EDGE_CURVE ( 'NONE', #88281, #18732, #76670, .T. ) ;
#18311 = CARTESIAN_POINT ( 'NONE',  ( 74.31767992295678482, 58.65107630571846187, -15.81261070485675369 ) ) ;
#18312 = CARTESIAN_POINT ( 'NONE',  ( 169.3571508527084291, 283.0956279022483955, 12.63651818596384935 ) ) ;
#18313 = ORIENTED_EDGE ( 'NONE', *, *, #93191, .T. ) ;
#18314 = CARTESIAN_POINT ( 'NONE',  ( 172.2467550100553808, 258.4300157609564508, -14.58559033337875377 ) ) ;
#18315 = CARTESIAN_POINT ( 'NONE',  ( 174.2667842284330675, 277.2948997594879756, -15.61071884909420682 ) ) ;
#18316 = CARTESIAN_POINT ( 'NONE',  ( 161.5083988044524119, 250.9062427520286178, -14.53522982831775856 ) ) ;
#18317 = CARTESIAN_POINT ( 'NONE',  ( 206.5157691485259761, 270.5309844673936368, 2.116125166999188068 ) ) ;
#18318 = EDGE_CURVE ( 'NONE', #30892, #80971, #66420, .T. ) ;
#18319 = EDGE_CURVE ( 'NONE', #30468, #20065, #68233, .T. ) ;
#18320 = CARTESIAN_POINT ( 'NONE',  ( 148.9719199701866899, 272.6200610409887872, 12.59512981512031438 ) ) ;
#18321 = AXIS2_PLACEMENT_3D ( 'NONE', #18090, #87045, #77896 ) ;
#18322 = CARTESIAN_POINT ( 'NONE',  ( 32.13723363786251497, 199.3615022471903160, 5.000000000000046185 ) ) ;
#18323 = CARTESIAN_POINT ( 'NONE',  ( 86.62177255451531721, 43.12972632285899266, -3.134764161692230822 ) ) ;
#18324 = CARTESIAN_POINT ( 'NONE',  ( 47.46694519036043403, 73.19305994210745325, -10.00000000000000000 ) ) ;
#18325 = CARTESIAN_POINT ( 'NONE',  ( 164.4513687979423082, 254.3942805075391504, 14.15307082335797695 ) ) ;
#18326 = CARTESIAN_POINT ( 'NONE',  ( 208.2777459429579210, 269.8993572713111462, 3.129643751043610589 ) ) ;
#18327 = EDGE_CURVE ( 'NONE', #17163, #80346, #97345, .T. ) ;
#18328 = CARTESIAN_POINT ( 'NONE',  ( 121.1210835531159091, 249.9244531367911293, -4.594050593750046652 ) ) ;
#18329 = ORIENTED_EDGE ( 'NONE', *, *, #30590, .T. ) ;
#18330 = CARTESIAN_POINT ( 'NONE',  ( 87.63170318219837895, 44.36446170533411504, -4.079950490519347106 ) ) ;
#18331 = CARTESIAN_POINT ( 'NONE',  ( 84.62393343236645649, 42.70031028179986521, 3.917025725994074836 ) ) ;
#18332 = AXIS2_PLACEMENT_3D ( 'NONE', #68929, #14249, #23327 ) ;
#18333 = ADVANCED_FACE ( 'NONE', ( #8609 ), #78019, .T. ) ;
#18334 = CARTESIAN_POINT ( 'NONE',  ( 171.0677017869332417, 283.0637397488268334, -13.46002028830316988 ) ) ;
#18335 = CARTESIAN_POINT ( 'NONE',  ( 163.7729086741176161, 246.9839966035275438, 6.099406794390714204 ) ) ;
#18336 = CARTESIAN_POINT ( 'NONE',  ( 73.93202095776594263, 57.04871283604670396, 16.01142866964926270 ) ) ;
#18337 = CARTESIAN_POINT ( 'NONE',  ( 174.8587845204546056, 252.5724801960949151, 5.155470236899263092 ) ) ;
#18338 = VERTEX_POINT ( 'NONE', #46588 ) ;
#18339 = CARTESIAN_POINT ( 'NONE',  ( 80.58432042439230258, 57.19069178250910568, -16.22979220026185487 ) ) ;
#18340 = CARTESIAN_POINT ( 'NONE',  ( 158.4705108345335987, 275.1496518313210231, -12.42170905744487364 ) ) ;
#18341 = CARTESIAN_POINT ( 'NONE',  ( 183.6436237883546880, 261.3127158997198762, 9.534748110082331252 ) ) ;
#18342 = CARTESIAN_POINT ( 'NONE',  ( 34.13991738056614622, 190.5177522451418497, -10.00000000000009592 ) ) ;
#18343 = CARTESIAN_POINT ( 'NONE',  ( 141.9874905431360332, 240.5327760586659451, 1.948934522072302763E-15 ) ) ;
#18344 = CARTESIAN_POINT ( 'NONE',  ( 188.5502890729128183, 299.8136175509387726, -3.629854520258569028 ) ) ;
#18345 = CIRCLE ( 'NONE', #57146, 14.21260523776213347 ) ;
#18346 = DIRECTION ( 'NONE',  ( 0.4999999999999998890, -0.8660254037844385966, 0.000000000000000000 ) ) ;
#18347 = CARTESIAN_POINT ( 'NONE',  ( 67.58366560447741733, 68.29344612013603921, 5.947104913347712518 ) ) ;
#18348 = CARTESIAN_POINT ( 'NONE',  ( 67.02199298016300588, 203.3768266524159856, -9.188101187500091527 ) ) ;
#18349 = CARTESIAN_POINT ( 'NONE',  ( 170.7729407420521284, 250.5257104363971621, 3.420218544161329532 ) ) ;
#18350 = CYLINDRICAL_SURFACE ( 'NONE', #32162, 70.00000000000002842 ) ;
#18351 = CARTESIAN_POINT ( 'NONE',  ( 155.4174679471833826, 279.7120021735884166, -1.458095568104960549 ) ) ;
#18352 = CARTESIAN_POINT ( 'NONE',  ( 172.5808743809259909, 287.8688692445808215, -8.370650701620615308 ) ) ;
#18353 = CARTESIAN_POINT ( 'NONE',  ( 155.1865148098964937, 261.8560670301561686, -16.99758927948949605 ) ) ;
#18354 = CARTESIAN_POINT ( 'NONE',  ( -19.65312891409030271, 93.06504152958497400, 59.99999999999999289 ) ) ;
#18355 = CARTESIAN_POINT ( 'NONE',  ( 125.0004159942834860, 249.6427522451419065, -10.00000000000009415 ) ) ;
#18356 = CARTESIAN_POINT ( 'NONE',  ( 75.89861163282604650, 53.37371604803925607, -16.00187665499177925 ) ) ;
#18357 = ORIENTED_EDGE ( 'NONE', *, *, #8336, .F. ) ;
#18358 = ADVANCED_FACE ( 'NONE', ( #92260 ), #41293, .T. ) ;
#18359 = CARTESIAN_POINT ( 'NONE',  ( 148.2267527339363369, 273.9107285543102535, 7.913369084260907016 ) ) ;
#18360 = CARTESIAN_POINT ( 'NONE',  ( -15.41332078621576329, 174.1589784336661921, -6.496448406907676862E-16 ) ) ;
#18361 = CARTESIAN_POINT ( 'NONE',  ( 37.90188877791127453, 186.5643266524160424, 9.188101187500095079 ) ) ;
#18362 = CARTESIAN_POINT ( 'NONE',  ( 26.21435097644586776, 14.94473085651392630, 1.475505719884397138E-15 ) ) ;
#18363 = CARTESIAN_POINT ( 'NONE',  ( 85.94639921072385391, 48.27664717140825701, 11.96740676232643352 ) ) ;
#18364 = CARTESIAN_POINT ( 'NONE',  ( 65.84416302801280096, 69.14091760660781461, 0.2185777033355933430 ) ) ;
#18365 = CARTESIAN_POINT ( 'NONE',  ( 190.1542208370626099, 290.9744051383607371, -14.40790947658664400 ) ) ;
#18366 = CARTESIAN_POINT ( 'NONE',  ( 190.6218339396177441, 300.4802939150614520, -4.178005820806754755 ) ) ;
#18367 = CARTESIAN_POINT ( 'NONE',  ( 72.17372541499028671, 72.08331884783481769, 2.982055604231361290 ) ) ;
#18369 = CARTESIAN_POINT ( 'NONE',  ( 56.22356517706933943, 203.2677522451418781, 10.00000000000009592 ) ) ;
#18368 = CARTESIAN_POINT ( 'NONE',  ( 7.263013161461002731, 16.14441083166258295, 10.00000000000000533 ) ) ;
#18370 = CARTESIAN_POINT ( 'NONE',  ( -17.42236680055705023, 149.2012482093457777, 0.000000000000000000 ) ) ;
#18371 = CARTESIAN_POINT ( 'NONE',  ( 163.1660858168057473, 256.0097020245835893, -14.93562900060027765 ) ) ;
#18372 = CARTESIAN_POINT ( 'NONE',  ( -0.8439004895948557516, 176.9865022471903160, -10.00000000000009592 ) ) ;
#18373 = DIRECTION ( 'NONE',  ( -0.3613624741150709974, -0.7937185950816926239, 0.4893137583626469000 ) ) ;
#18374 = CARTESIAN_POINT ( 'NONE',  ( 179.2814824751584695, 294.6666816158376605, 1.075539458643513191 ) ) ;
#18375 = CARTESIAN_POINT ( 'NONE',  ( 30.47735161394232151, 201.7365022471903444, 2.944929066748280225E-16 ) ) ;
#18376 = CARTESIAN_POINT ( 'NONE',  ( 185.1158323825266052, 294.3144650231332662, 9.807602087358677778 ) ) ;
#18377 = CARTESIAN_POINT ( 'NONE',  ( 202.8787628851569593, 279.2506702366259788, 17.01435431865322556 ) ) ;
#18378 = CARTESIAN_POINT ( 'NONE',  ( 0.1751364819041374699, 183.1589784336661637, -6.496448406907675876E-16 ) ) ;
#18379 = CARTESIAN_POINT ( 'NONE',  ( 36.57256041901661803, 33.06628583063844928, -9.188101187500006262 ) ) ;
#18380 = FACE_OUTER_BOUND ( 'NONE', #96719, .T. ) ;
#18381 = CARTESIAN_POINT ( 'NONE',  ( 152.6992418905140028, 266.1641500988167763, 17.27767170937316621 ) ) ;
#18382 = CARTESIAN_POINT ( 'NONE',  ( 32.72297390791170812, 40.93396525600392977, 2.839279412974139660 ) ) ;
#18383 = CARTESIAN_POINT ( 'NONE',  ( 206.3106310032756596, 273.3065002911688453, 10.17860425536756175 ) ) ;
#18384 = EDGE_CURVE ( 'NONE', #20413, #31364, #17715, .T. ) ;
#18385 = CARTESIAN_POINT ( 'NONE',  ( 186.3729170633118599, 259.2531417649982473, -2.352328541926433925 ) ) ;
#18386 = CARTESIAN_POINT ( 'NONE',  ( 80.81105205787801538, 42.98178676852656821, -9.627323360252351137 ) ) ;
#18387 = PLANE ( 'NONE',  #23432 ) ;
#18388 = CARTESIAN_POINT ( 'NONE',  ( 176.9834359889674715, 260.3444538793796141, -13.76265079422755377 ) ) ;
#18389 = CARTESIAN_POINT ( 'NONE',  ( 4.512196379633642174, 24.64646525600387861, -2.839279412974133887 ) ) ;
#18390 = LINE ( 'NONE', #48285, #93665 ) ;
#18391 = CARTESIAN_POINT ( 'NONE',  ( 15.78795072819010770, 21.06628583063840665, -9.188101187500006262 ) ) ;
#18392 = CARTESIAN_POINT ( 'NONE',  ( 74.64464720694877542, 207.2365022471902023, -10.00000000000009237 ) ) ;
#18393 = AXIS2_PLACEMENT_3D ( 'NONE', #67711, #60087, #91050 ) ;
#18394 = CARTESIAN_POINT ( 'NONE',  ( 153.2412541709487357, 277.6964940543419971, -5.155127835892409749 ) ) ;
#18395 = CARTESIAN_POINT ( 'NONE',  ( 84.68046352546232924, 50.54697168049320055, -14.01127729920333742 ) ) ;
#18396 = CARTESIAN_POINT ( 'NONE',  ( 159.8188415394622268, 253.8326417772889840, -15.43862849427313222 ) ) ;
#18397 = CYLINDRICAL_SURFACE ( 'NONE', #60873, 10.00000000000010658 ) ;
#18398 = ADVANCED_FACE ( 'NONE', ( #63803 ), #94715, .T. ) ;
#18399 = ORIENTED_EDGE ( 'NONE', *, *, #73975, .T. ) ;
#18400 = CARTESIAN_POINT ( 'NONE',  ( -22.42236680055709641, 157.8615022471902591, 0.000000000000000000 ) ) ;
#18401 = CARTESIAN_POINT ( 'NONE',  ( 207.6727254509676186, 270.9472835030587703, 7.315149605389819953 ) ) ;
#18402 = CARTESIAN_POINT ( 'NONE',  ( 66.05014806366969538, 68.57571539968135710, 4.401547170603885561 ) ) ;
#18403 = EDGE_CURVE ( 'NONE', #44538, #28481, #42970, .T. ) ;
#18404 = CARTESIAN_POINT ( 'NONE',  ( 87.34055741008818075, 44.89555582937398981, 6.825810004488436888 ) ) ;
#18405 = VECTOR ( 'NONE', #29368, 1000.000000000000000 ) ;
#18406 = CARTESIAN_POINT ( 'NONE',  ( 193.7999837595647250, 294.9755769528473479, 15.24609078262870199 ) ) ;
#18407 = ORIENTED_EDGE ( 'NONE', *, *, #41038, .F. ) ;
#18408 = VERTEX_POINT ( 'NONE', #35395 ) ;
#18409 = LINE ( 'NONE', #24490, #48653 ) ;
#18410 = AXIS2_PLACEMENT_3D ( 'NONE', #79069, #40006, #86192 ) ;
#18411 = CARTESIAN_POINT ( 'NONE',  ( 86.25117823697901542, 47.20812847272011226, 10.82755581481952056 ) ) ;
#18412 = ORIENTED_EDGE ( 'NONE', *, *, #86727, .F. ) ;
#18413 = CARTESIAN_POINT ( 'NONE',  ( 78.15957118868782061, 60.17571743070642043, 16.00619919759238741 ) ) ;
#18414 = CARTESIAN_POINT ( 'NONE',  ( 155.4612256362409255, 261.7625261697407950, -16.98072832849991443 ) ) ;
#18415 = VERTEX_POINT ( 'NONE', #83535 ) ;
#18416 = CARTESIAN_POINT ( 'NONE',  ( 78.36990314024963311, 61.17320995784978521, -15.89858940129926523 ) ) ;
#18417 = CARTESIAN_POINT ( 'NONE',  ( -69.94229046795800286, 43.99946344738946635, -10.00000000000000000 ) ) ;
#18418 = VECTOR ( 'NONE', #45737, 1000.000000000000000 ) ;
#18419 = CARTESIAN_POINT ( 'NONE',  ( 80.50336155508412617, 43.50879043608720309, 9.659109878193110177 ) ) ;
#18420 = VERTEX_POINT ( 'NONE', #74919 ) ;
#18421 = CARTESIAN_POINT ( 'NONE',  ( 173.7157974438445081, 267.2565184175704758, 16.75892562235658900 ) ) ;
#18422 = CARTESIAN_POINT ( 'NONE',  ( 169.5377272533189625, 276.4473244127411249, -15.81453032960868832 ) ) ;
#18423 = CARTESIAN_POINT ( 'NONE',  ( 74.22445535223697277, 61.98362111549793241, 14.93260878751794074 ) ) ;
#18424 = B_SPLINE_SURFACE_WITH_KNOTS ( 'NONE', 3, 1, ( 
 ( #25529, #56417 ),
 ( #61997, #8328 ),
 ( #85370, #15916 ),
 ( #24017, #54915 ),
 ( #71145, #85894 ),
 ( #16418, #47313 ),
 ( #78239, #8820 ),
 ( #16915, #78737 ),
 ( #64530, #35111 ),
 ( #3740, #66021 ),
 ( #18441, #12843 ),
 ( #18945, #73629 ),
 ( #50314, #89382 ),
 ( #73144, #57916 ),
 ( #43196, #58888 ),
 ( #3253, #34135 ),
 ( #10834, #2747 ),
 ( #51298, #66516 ),
 ( #88896, #12332 ),
 ( #19935, #20432 ),
 ( #27538, #27032 ),
 ( #33637, #41712 ),
 ( #74140, #95488 ),
 ( #89857, #96971 ),
 ( #88391, #42698 ),
 ( #11355, #58407 ),
 ( #34617, #72658 ),
 ( #95974, #50808 ),
 ( #80781, #26040 ),
 ( #4215, #42209 ),
 ( #4733, #49823 ),
 ( #81758, #43704 ),
 ( #57410, #65517 ),
 ( #97441, #28012 ) ),
 .UNSPECIFIED., .T., .F., .F.,
 ( 4, 2, 2, 2, 2, 2, 2, 2, 2, 2, 2, 2, 2, 2, 2, 2, 4 ),
 ( 2, 2 ),
 ( 0.000000000000000000, 0.06250000000000000000, 0.1250000000000000000, 0.1875000000000000000, 0.2500000000000000000, 0.3125000000000000000, 0.3750000000000000000, 0.4375000000000000000, 0.5000000000000000000, 0.5625000000000000000, 0.6250000000000000000, 0.6875000000000000000, 0.7500000000000000000, 0.8125000000000000000, 0.8750000000000000000, 0.9375000000000000000, 1.000000000000000000 ),
 ( 0.000000000000000000, 1.000000000000000000 ),
 .UNSPECIFIED. ) ;
#18425 = EDGE_LOOP ( 'NONE', ( #80775, #67987, #23268, #215 ) ) ;
#18426 = CARTESIAN_POINT ( 'NONE',  ( 171.1865699020292766, 254.5746376615227291, -11.62694971751192519 ) ) ;
#18427 = CARTESIAN_POINT ( 'NONE',  ( 202.7599932440484451, 279.4563852894229967, 15.58249343055423353 ) ) ;
#18428 = ORIENTED_EDGE ( 'NONE', *, *, #89685, .F. ) ;
#18429 = ORIENTED_EDGE ( 'NONE', *, *, #57491, .T. ) ;
#18430 = CARTESIAN_POINT ( 'NONE',  ( 160.0914855916899171, 268.6372815687846014, -16.51133705495732684 ) ) ;
#18431 = ORIENTED_EDGE ( 'NONE', *, *, #28789, .F. ) ;
#18432 = CARTESIAN_POINT ( 'NONE',  ( 179.7646977617114601, 254.2800489533466077, -2.868012902750119331 ) ) ;
#18433 = ORIENTED_EDGE ( 'NONE', *, *, #97697, .T. ) ;
#18434 = EDGE_CURVE ( 'NONE', #20280, #92014, #93626, .T. ) ;
#18435 = CARTESIAN_POINT ( 'NONE',  ( 81.87359138893998534, 41.32955797152819599, 5.976920566253460798 ) ) ;
#18436 = CARTESIAN_POINT ( 'NONE',  ( 147.9292452580141912, 274.4260266182387227, 6.430851193091030815 ) ) ;
#18437 = CARTESIAN_POINT ( 'NONE',  ( 180.0253394064914119, 291.5621715643180778, -10.00052010529626934 ) ) ;
#18438 = CARTESIAN_POINT ( 'NONE',  ( 69.54656231429063951, 65.32963776451991578, 11.37142180160457094 ) ) ;
#18439 = CARTESIAN_POINT ( 'NONE',  ( 192.0712386031329686, 297.9698513971258649, 12.12276320360788873 ) ) ;
#18440 = DIRECTION ( 'NONE',  ( 0.09547062131715944311, -0.9954322480537364237, 0.000000000000000000 ) ) ;
#18441 = CARTESIAN_POINT ( 'NONE',  ( 197.5503536138679976, 288.4797458180196372, -16.78011540949930946 ) ) ;
#18442 = ORIENTED_EDGE ( 'NONE', *, *, #40958, .T. ) ;
#18443 = CARTESIAN_POINT ( 'NONE',  ( 2.064617007569730767, 27.83817977871671800, -10.00000000000000000 ) ) ;
#18444 = CARTESIAN_POINT ( 'NONE',  ( 24.50893013558248157, 16.01110640527292261, 2.839279412974134775 ) ) ;
#18445 = CARTESIAN_POINT ( 'NONE',  ( 205.8610808625997208, 274.0851439753691920, 10.38803237360972531 ) ) ;
#18447 = CARTESIAN_POINT ( 'NONE',  ( 164.3939401533646958, 245.9083385283718712, 2.844462461176849200 ) ) ;
#18446 = CARTESIAN_POINT ( 'NONE',  ( 77.56105267982387375, 49.72783448593992262, -15.46007777837396979 ) ) ;
#18449 = ORIENTED_EDGE ( 'NONE', *, *, #98607, .T. ) ;
#18448 = CARTESIAN_POINT ( 'NONE',  ( -6.542761065016642341, 25.57183462804972507, -10.00000000000000000 ) ) ;
#18450 = VERTEX_POINT ( 'NONE', #12620 ) ;
#18451 = CARTESIAN_POINT ( 'NONE',  ( 187.5612807588072428, 277.0616058210526944, 17.40194786215237244 ) ) ;
#18452 = DIRECTION ( 'NONE',  ( -1.000000000000000000, 0.000000000000000000, 0.000000000000000000 ) ) ;
#18453 = EDGE_CURVE ( 'NONE', #99040, #10180, #51083, .T. ) ;
#18454 = CARTESIAN_POINT ( 'NONE',  ( 164.3523996349191805, 247.8276598175897902, 8.684433193650701099 ) ) ;
#18455 = CARTESIAN_POINT ( 'NONE',  ( 79.11275361919636850, 46.11146926017930525, 13.27945046512232707 ) ) ;
#18456 = CARTESIAN_POINT ( 'NONE',  ( 160.5437591895810954, 252.5770475759798046, -16.01484307027506304 ) ) ;
#18457 = CARTESIAN_POINT ( 'NONE',  ( 71.71614068478815796, 59.03149745595231934, 15.86337787674895594 ) ) ;
#18458 = ORIENTED_EDGE ( 'NONE', *, *, #91483, .T. ) ;
#18459 = CYLINDRICAL_SURFACE ( 'NONE', #76903, 10.00000000000001066 ) ;
#18460 = CARTESIAN_POINT ( 'NONE',  ( 60.73642589098854216, 194.3262482093457777, 3.021315404115420679E-15 ) ) ;
#18461 = CARTESIAN_POINT ( 'NONE',  ( 206.9676408587583296, 272.1685258403992975, 7.544050792475608169 ) ) ;
#18462 = CARTESIAN_POINT ( 'NONE',  ( 27.21171415029068186, 176.5177522451417929, 5.000000000000051514 ) ) ;
#18463 = CARTESIAN_POINT ( 'NONE',  ( 95.76303752037657091, 226.0958772461660260, -9.188101187500095079 ) ) ;
#18464 = CARTESIAN_POINT ( 'NONE',  ( 180.7944058683433752, 294.0821055505414279, -2.743935788258776487 ) ) ;
#18465 = CARTESIAN_POINT ( 'NONE',  ( 85.29362735876655677, 48.41412782346650800, 12.38048700662147716 ) ) ;
#18466 = CARTESIAN_POINT ( 'NONE',  ( 207.9312334543074599, 270.4995345071110933, 1.552289074598145469 ) ) ;
#18467 = ADVANCED_FACE ( 'NONE', ( #29307 ), #5501, .T. ) ;
#18468 = CARTESIAN_POINT ( 'NONE',  ( 26.91401791951368949, 186.3458772461660544, 9.188101187500095079 ) ) ;
#18469 = CYLINDRICAL_SURFACE ( 'NONE', #99670, 10.00000000000010658 ) ;
#18470 = ORIENTED_EDGE ( 'NONE', *, *, #42284, .T. ) ;
#18471 = EDGE_LOOP ( 'NONE', ( #85514, #25127, #41454, #49928 ) ) ;
#18472 = CARTESIAN_POINT ( 'NONE',  ( 185.1499092832424651, 259.9585293422515520, -5.749318524461872748 ) ) ;
#18473 = CARTESIAN_POINT ( 'NONE',  ( 88.27284635163252347, 44.14049577968297200, 0.4518384918358809288 ) ) ;
#18474 = CARTESIAN_POINT ( 'NONE',  ( 84.24943540987109714, 43.94360214673953635, 7.356120964585859845 ) ) ;
#18475 = CARTESIAN_POINT ( 'NONE',  ( 192.9818866559145931, 263.7816602304387175, -4.162437127754325061 ) ) ;
#18476 = VECTOR ( 'NONE', #12959, 1000.000000000000000 ) ;
#18477 = CARTESIAN_POINT ( 'NONE',  ( 161.1747502674735415, 251.4841389699472529, -13.25152330924089839 ) ) ;
#18478 = CARTESIAN_POINT ( 'NONE',  ( 81.30975366074838462, 56.24313983998633404, -16.44754541364716971 ) ) ;
#18479 = CARTESIAN_POINT ( 'NONE',  ( 28.46864935082048831, 149.7156766241961350, -21.50000000000001421 ) ) ;
#18480 = CARTESIAN_POINT ( 'NONE',  ( 49.83688814775681664, 190.3923013555410080, 4.594050593750050204 ) ) ;
#18481 = CARTESIAN_POINT ( 'NONE',  ( 80.90528918492583443, 217.5177522451418497, -10.00000000000009592 ) ) ;
#18482 = ORIENTED_EDGE ( 'NONE', *, *, #42572, .T. ) ;
#18483 = EDGE_CURVE ( 'NONE', #18408, #81112, #32114, .T. ) ;
#18484 = CARTESIAN_POINT ( 'NONE',  ( 83.03935637480527987, 45.02721014752604844, 9.768256401072576978 ) ) ;
#18485 = VECTOR ( 'NONE', #73726, 999.9999999999998863 ) ;
#18486 = CARTESIAN_POINT ( 'NONE',  ( 157.7632566947985708, 282.3764601569879460, -1.694678876849560645 ) ) ;
#18487 = CARTESIAN_POINT ( 'NONE',  ( 0.4734401320438119676, 161.8923013555410080, 4.594050593750050204 ) ) ;
#18488 = CARTESIAN_POINT ( 'NONE',  ( 68.57734787275012422, 64.58769200091258256, -12.17370147371886624 ) ) ;
#18489 = CARTESIAN_POINT ( 'NONE',  ( 151.1699610800269511, 268.8129421616204695, -14.28929860221299286 ) ) ;
#18490 = CARTESIAN_POINT ( 'NONE',  ( 186.1126677289907434, 283.4250391647574929, 17.12934966007601645 ) ) ;
#18491 = CARTESIAN_POINT ( 'NONE',  ( 147.3379027498079381, 275.4502618871274535, -3.695260257281167249 ) ) ;
#18492 = CARTESIAN_POINT ( 'NONE',  ( 68.54821950050275348, 68.31194209259709282, -8.033256955384258546 ) ) ;
#18493 = CARTESIAN_POINT ( 'NONE',  ( 204.6427704787179493, 276.1953194596412118, 13.28850621060895953 ) ) ;
#18494 = CARTESIAN_POINT ( 'NONE',  ( 146.5157004908022031, 276.8743579738231233, -0.1877253132609108255 ) ) ;
#18495 = CARTESIAN_POINT ( 'NONE',  ( 164.3138894970802824, 246.0469903322357368, -2.642126690130961020 ) ) ;
#18496 = ORIENTED_EDGE ( 'NONE', *, *, #50746, .F. ) ;
#18497 = B_SPLINE_CURVE_WITH_KNOTS ( 'NONE', 3,
 ( #40499, #95273, #57698, #71431, #88178, #11138, #33936, #18724, #50113, #80057 ),
 .UNSPECIFIED., .F., .F.,
 ( 4, 2, 2, 2, 4 ),
 ( 0.000000000000000000, 0.2500000000000000000, 0.5000000000000000000, 0.7500000000000000000, 1.000000000000000000 ),
 .UNSPECIFIED. ) ;
#18498 = CARTESIAN_POINT ( 'NONE',  ( -6.040052912301486110, 173.9865022471903160, -10.00000000000009415 ) ) ;
#18499 = CARTESIAN_POINT ( 'NONE',  ( 181.1462475035585271, 268.2071771633989670, 15.44497821374024049 ) ) ;
#18500 = CARTESIAN_POINT ( 'NONE',  ( 112.2171730965159071, 247.8464784336661353, 1.353441290958777327E-15 ) ) ;
#18501 = CARTESIAN_POINT ( 'NONE',  ( 13.12254358208367400, 30.68290643055187061, 3.479690158560446702E-15 ) ) ;
#18502 = PLANE ( 'NONE',  #88090 ) ;
#18503 = CYLINDRICAL_SURFACE ( 'NONE', #71102, 17.82106496071139645 ) ;
#18505 = CARTESIAN_POINT ( 'NONE',  ( 185.5122157014849336, 288.1045496927467866, 15.02337816592467057 ) ) ;
#18504 = CARTESIAN_POINT ( 'NONE',  ( 157.0935036675524827, 258.5530654392286465, 17.32636058289560665 ) ) ;
#18506 = DIRECTION ( 'NONE',  ( -0.009162850352631533510, 0.9999580202055560196, 0.000000000000000000 ) ) ;
#18507 = ORIENTED_EDGE ( 'NONE', *, *, #10713, .T. ) ;
#18508 = CARTESIAN_POINT ( 'NONE',  ( 193.1827667186879864, 263.4048335427814322, -5.307581698297376249 ) ) ;
#18509 = CARTESIAN_POINT ( 'NONE',  ( 196.8435556370661459, 289.7039558245273838, -16.43899056939217118 ) ) ;
#18510 = CARTESIAN_POINT ( 'NONE',  ( 189.8641800978502658, 300.0801047183622359, 4.769842506271963600 ) ) ;
#18511 = CARTESIAN_POINT ( 'NONE',  ( 176.2543089179515619, 292.5905172262055203, -1.124657176953766102 ) ) ;
#18512 = CARTESIAN_POINT ( 'NONE',  ( 81.32801083308449108, 55.42016325551186640, -16.33050219934855463 ) ) ;
#18513 = EDGE_LOOP ( 'NONE', ( #50881, #88884, #79159, #61985 ) ) ;
#18514 = PLANE ( 'NONE',  #10137 ) ;
#18515 = CARTESIAN_POINT ( 'NONE',  ( 175.1327937842674771, 279.3162497976952636, 15.76955821438891903 ) ) ;
#18516 = CARTESIAN_POINT ( 'NONE',  ( -6.542761065016642341, 25.57183462804972862, -10.00000000000000000 ) ) ;
#18517 = EDGE_CURVE ( 'NONE', #23627, #46799, #73912, .T. ) ;
#18518 = B_SPLINE_CURVE_WITH_KNOTS ( 'NONE', 3,
 ( #9409, #8904, #1317, #40284 ),
 .UNSPECIFIED., .F., .F.,
 ( 4, 4 ),
 ( 0.009203791814746210831, 0.01435997971314354436 ),
 .UNSPECIFIED. ) ;
#18519 = CARTESIAN_POINT ( 'NONE',  ( 79.75097749241258782, 52.41140398045773452, 15.43538078857268836 ) ) ;
#18520 = CARTESIAN_POINT ( 'NONE',  ( 156.2139277615245589, 261.1003705204080916, 17.33299519700502245 ) ) ;
#18521 = EDGE_CURVE ( 'NONE', #31869, #36246, #72575, .T. ) ;
#18522 = CARTESIAN_POINT ( 'NONE',  ( 68.68909986782581711, 64.16576715805911135, -12.55144644517788777 ) ) ;
#18523 = CARTESIAN_POINT ( 'NONE',  ( 153.3703256797887775, 265.0017988796566897, 16.44314709207578318 ) ) ;
#18524 = EDGE_LOOP ( 'NONE', ( #92919, #46439, #31998, #7565 ) ) ;
#18525 = CARTESIAN_POINT ( 'NONE',  ( 164.4854433269806577, 246.2060377238486808, -1.879056492287135116 ) ) ;
#18526 = EDGE_CURVE ( 'NONE', #9601, #77760, #96109, .T. ) ;
#18527 = CARTESIAN_POINT ( 'NONE',  ( 12.12248498587032586, 9.127558733836243832, -6.180339887498949025 ) ) ;
#18528 = CARTESIAN_POINT ( 'NONE',  ( 175.0209189270691184, 273.4799616097778880, -16.39738812790832867 ) ) ;
#18529 = ORIENTED_EDGE ( 'NONE', *, *, #83832, .T. ) ;
#18530 = CARTESIAN_POINT ( 'NONE',  ( 78.08661669030729513, 61.77574478846858597, 16.09152831843414333 ) ) ;
#18531 = EDGE_CURVE ( 'NONE', #23843, #61231, #89176, .T. ) ;
#18532 = CARTESIAN_POINT ( 'NONE',  ( 148.3629184514745987, 273.6748826132846375, -8.219814532462343948 ) ) ;
#18533 = CARTESIAN_POINT ( 'NONE',  ( -22.42236680055709641, 157.8615022471902591, 0.000000000000000000 ) ) ;
#18534 = ORIENTED_EDGE ( 'NONE', *, *, #34080, .F. ) ;
#18535 = DIRECTION ( 'NONE',  ( -0.6778389383370750920, -0.7352104281592222179, 0.000000000000000000 ) ) ;
#18536 = CARTESIAN_POINT ( 'NONE',  ( 2.487887237287232711, 134.7156766241960497, 21.50000000000007461 ) ) ;
#18537 = CARTESIAN_POINT ( 'NONE',  ( 151.1926529451685326, 268.7736386982768408, 14.30343427984827365 ) ) ;
#18538 = CARTESIAN_POINT ( 'NONE',  ( 78.44491574804551703, 51.88413252454667912, -15.48821912003990242 ) ) ;
#18539 = CARTESIAN_POINT ( 'NONE',  ( 189.8233477357014465, 300.2304324313545294, 3.241907359326032356 ) ) ;
#18540 = CARTESIAN_POINT ( 'NONE',  ( 203.5555343017997529, 278.0784677578903370, -15.71723084798551362 ) ) ;
#18541 = EDGE_LOOP ( 'NONE', ( #73972, #16001, #12949, #9944 ) ) ;
#18543 = ORIENTED_EDGE ( 'NONE', *, *, #54380, .F. ) ;
#18542 =( BOUNDED_CURVE ( )  B_SPLINE_CURVE ( 2, ( #24381, #47662, #40561, #46670, #32968, #55253, #16770 ),
 .UNSPECIFIED., .F., .T. ) 
 B_SPLINE_CURVE_WITH_KNOTS ( ( 3, 2, 2, 3 ),
 ( 0.000000000000000000, 0.005000000000000000104, 0.01000000000000000021, 0.01250000000000000243 ),
 .UNSPECIFIED. ) 
 CURVE ( )  GEOMETRIC_REPRESENTATION_ITEM ( )  RATIONAL_B_SPLINE_CURVE ( ( 1.000000000000000000, 0.9510565162951535312, 1.000000000000000000, 0.9510565162951535312, 1.000000000000000000, 0.9755282581475768211, 0.9755282581475768211 ) ) 
 REPRESENTATION_ITEM ( '' )  );
#18544 = DIRECTION ( 'NONE',  ( 0.4999999999999998890, -0.8660254037844385966, 0.000000000000000000 ) ) ;
#18545 = ORIENTED_EDGE ( 'NONE', *, *, #82701, .F. ) ;
#18546 = CARTESIAN_POINT ( 'NONE',  ( 193.2749530133065150, 294.1419888553381838, 14.05938658124414431 ) ) ;
#18547 = CIRCLE ( 'NONE', #10440, 70.00000000000001421 ) ;
#18548 = ORIENTED_EDGE ( 'NONE', *, *, #63474, .F. ) ;
#18549 = DIRECTION ( 'NONE',  ( 0.3666034970181715757, -0.9303772761487930643, 0.000000000000000000 ) ) ;
#18550 = DIRECTION ( 'NONE',  ( 0.000000000000000000, 0.000000000000000000, 1.000000000000000000 ) ) ;
#18551 = VERTEX_POINT ( 'NONE', #81538 ) ;
#18552 = CARTESIAN_POINT ( 'NONE',  ( 185.5632263566141944, 282.0228027493975560, -16.47564400571021181 ) ) ;
#18553 = B_SPLINE_CURVE_WITH_KNOTS ( 'NONE', 3,
 ( #14625, #96902, #27474, #50739 ),
 .UNSPECIFIED., .F., .F.,
 ( 4, 4 ),
 ( 0.02891663082521821887, 0.03807346097812620150 ),
 .UNSPECIFIED. ) ;
#18554 = CARTESIAN_POINT ( 'NONE',  ( 81.94191999987826591, 41.06410402935708248, 3.451294334475704773 ) ) ;
#18555 = CARTESIAN_POINT ( 'NONE',  ( 80.78918961562681034, 43.20779693872438543, -9.098606657379765039 ) ) ;
#18556 = CARTESIAN_POINT ( 'NONE',  ( 197.3327212804159103, 267.5970440452412049, 9.861675131224707513 ) ) ;
#18557 = CARTESIAN_POINT ( 'NONE',  ( 193.2100161762185735, 295.9974307820218087, -12.46499585622781758 ) ) ;
#18558 = CARTESIAN_POINT ( 'NONE',  ( 201.3505934466285510, 281.8975373467312693, -16.83770227898004279 ) ) ;
#18559 = DIRECTION ( 'NONE',  ( -0.5000000000000013323, 0.8660254037844379305, 0.000000000000000000 ) ) ;
#18560 = DIRECTION ( 'NONE',  ( -1.982541115402060426E-16, 3.433861939970638790E-16, -1.000000000000000000 ) ) ;
#18561 = CARTESIAN_POINT ( 'NONE',  ( 131.6216415740022398, 255.9869531367911009, 4.594050593750046652 ) ) ;
#18562 = ORIENTED_EDGE ( 'NONE', *, *, #9633, .T. ) ;
#18563 = CARTESIAN_POINT ( 'NONE',  ( 70.89704694694920306, 61.12483521587895297, -14.46529911291810855 ) ) ;
#18564 = CARTESIAN_POINT ( 'NONE',  ( 2.780145572064765425, 23.64646525600387506, -2.839279412974133887 ) ) ;
#18565 = VERTEX_POINT ( 'NONE', #66304 ) ;
#18567 = ORIENTED_EDGE ( 'NONE', *, *, #76295, .T. ) ;
#18566 = DIRECTION ( 'NONE',  ( 0.8660254037844377084, 0.5000000000000016653, 0.000000000000000000 ) ) ;
#18568 = CARTESIAN_POINT ( 'NONE',  ( -16.56403295706242318, 104.9882471913986990, 12.26538863783448186 ) ) ;
#18569 = CARTESIAN_POINT ( 'NONE',  ( 202.5511585997265911, 279.8180975037686835, 17.12781264818056925 ) ) ;
#18570 = DIRECTION ( 'NONE',  ( -0.000000000000000000, -0.000000000000000000, -1.000000000000000000 ) ) ;
#18571 = CARTESIAN_POINT ( 'NONE',  ( 2.487887237287232711, 134.7156766241960497, -22.49999999999983302 ) ) ;
#18572 = CARTESIAN_POINT ( 'NONE',  ( 153.4850820818235491, 276.9265329172790757, 7.161006446225682609 ) ) ;
#18573 = DIRECTION ( 'NONE',  ( 0.000000000000000000, 0.000000000000000000, 1.000000000000000000 ) ) ;
#18574 = LINE ( 'NONE', #67014, #93316 ) ;
#18576 = CARTESIAN_POINT ( 'NONE',  ( 170.9494504878256294, 280.9963802879100285, 14.66202574695598138 ) ) ;
#18575 = B_SPLINE_CURVE_WITH_KNOTS ( 'NONE', 3,
 ( #34371, #49566, #5470, #42449, #81028, #97691, #74887 ),
 .UNSPECIFIED., .F., .F.,
 ( 4, 3, 4 ),
 ( 0.000000000000000000, 0.001498044977024529231, 0.003064388198862243000 ),
 .UNSPECIFIED. ) ;
#18577 = CARTESIAN_POINT ( 'NONE',  ( 76.43353238120225512, 51.64775962558189804, -16.15746030387889576 ) ) ;
#18578 = DIRECTION ( 'NONE',  ( 0.5000000000000003331, -0.8660254037844383745, 0.000000000000000000 ) ) ;
#18579 = ORIENTED_EDGE ( 'NONE', *, *, #93323, .T. ) ;
#18580 = CARTESIAN_POINT ( 'NONE',  ( -19.65312891409030271, 93.06504152958497400, -10.00000000000000888 ) ) ;
#18581 = ORIENTED_EDGE ( 'NONE', *, *, #57106, .T. ) ;
#18582 = CARTESIAN_POINT ( 'NONE',  ( 162.6380106777187962, 276.9062633384314722, 12.86980460176377150 ) ) ;
#18583 = B_SPLINE_CURVE_WITH_KNOTS ( 'NONE', 3,
 ( #6478, #81645, #26912, #57792, #49701, #12216, #50203, #3144, #81154, #11722, #42584, #29770 ),
 .UNSPECIFIED., .F., .F.,
 ( 4, 2, 2, 2, 2, 4 ),
 ( 0.001861292369029458101, 0.001963120261722284526, 0.002064948154415110516, 0.002268603939800654078, 0.002675915510571577269, 0.003490538652113424952 ),
 .UNSPECIFIED. ) ;
#18584 = CARTESIAN_POINT ( 'NONE',  ( 201.0217745861505705, 267.6100443300385336, -2.437338837632460287 ) ) ;
#18585 = CARTESIAN_POINT ( 'NONE',  ( 191.6373630319821473, 298.7213459305223182, -9.457989462015230941 ) ) ;
#18586 = CARTESIAN_POINT ( 'NONE',  ( 149.6071296322179194, 271.5198456328920997, 12.75640156477042453 ) ) ;
#18587 = EDGE_CURVE ( 'NONE', #20674, #98683, #88813, .T. ) ;
#18588 = CARTESIAN_POINT ( 'NONE',  ( 202.3894997978090373, 280.0980987621804275, 16.95659012541789323 ) ) ;
#18590 = CARTESIAN_POINT ( 'NONE',  ( 87.83461099834376284, 44.15040118474664865, 2.754765003853551164 ) ) ;
#18589 = CARTESIAN_POINT ( 'NONE',  ( 21.71530570849275321, 51.45382605859413161, 59.99999999999999289 ) ) ;
#18591 = CYLINDRICAL_SURFACE ( 'NONE', #64076, 17.82106496071139645 ) ;
#18592 = ORIENTED_EDGE ( 'NONE', *, *, #73643, .T. ) ;
#18593 = CARTESIAN_POINT ( 'NONE',  ( 71.16465123163835926, 62.56096922933172522, -13.87416499188189967 ) ) ;
#18594 = CARTESIAN_POINT ( 'NONE',  ( 190.2932943857919099, 273.3550103105087601, -16.39709156336667206 ) ) ;
#18595 = LINE ( 'NONE', #26188, #72685 ) ;
#18596 = CARTESIAN_POINT ( 'NONE',  ( 195.3624787578944222, 290.3824063481519602, -16.76522224015156226 ) ) ;
#18597 = CARTESIAN_POINT ( 'NONE',  ( 80.62296282160744454, 43.30841819719253039, -9.338142585044177935 ) ) ;
#18598 = CYLINDRICAL_SURFACE ( 'NONE', #85560, 17.82106496071139645 ) ;
#18599 = CARTESIAN_POINT ( 'NONE',  ( 202.2603678735342214, 280.3217618159037556, 16.49712126737133744 ) ) ;
#18600 = CARTESIAN_POINT ( 'NONE',  ( -13.03140383004354241, 163.2833772461660544, -9.188101187500095079 ) ) ;
#18601 = CARTESIAN_POINT ( 'NONE',  ( 101.5001087246834857, 241.6589784336661637, -6.496448406907675876E-16 ) ) ;
#18602 = CARTESIAN_POINT ( 'NONE',  ( 155.1398527401465230, 261.9368881057492899, -17.02245700497956449 ) ) ;
#18603 = CARTESIAN_POINT ( 'NONE',  ( 88.01665444240776992, 44.57641488075346814, -4.048309816952348150 ) ) ;
#18604 = CARTESIAN_POINT ( 'NONE',  ( 164.9009427471078766, 270.4319544559331234, -17.40525121274953335 ) ) ;
#18605 = ADVANCED_FACE ( 'NONE', ( #84532 ), #60665, .F. ) ;
#18606 = DIRECTION ( 'NONE',  ( 0.000000000000000000, 0.000000000000000000, 1.000000000000000000 ) ) ;
#18607 = CARTESIAN_POINT ( 'NONE',  ( 195.9879163382961735, 284.2697365227047044, 17.81990856217999664 ) ) ;
#18608 = CARTESIAN_POINT ( 'NONE',  ( 163.7707745167360258, 284.3866919517458314, 5.949292284668742603 ) ) ;
#18610 = DIRECTION ( 'NONE',  ( -0.000000000000000000, -0.000000000000000000, 1.000000000000000000 ) ) ;
#18609 = CYLINDRICAL_SURFACE ( 'NONE', #37048, 10.00000000000010658 ) ;
#18611 = CARTESIAN_POINT ( 'NONE',  ( 207.3943894158706485, 271.4293756574240888, 4.935128030509036812 ) ) ;
#18612 = DIRECTION ( 'NONE',  ( 0.3715724127386967335, -0.6435822975543782354, -0.6691306063588567943 ) ) ;
#18613 = CARTESIAN_POINT ( 'NONE',  ( 7.429509195272512301, 163.5494855054051868, -2.679491924311248496 ) ) ;
#18614 = CARTESIAN_POINT ( 'NONE',  ( 80.66989203997422919, 54.07632877718189945, -15.76682839205882303 ) ) ;
#18615 = CARTESIAN_POINT ( 'NONE',  ( 166.1440757875318468, 253.4574300428235176, -13.57559907896235707 ) ) ;
#18616 = AXIS2_PLACEMENT_3D ( 'NONE', #71152, #41211, #72150 ) ;
#18617 = CARTESIAN_POINT ( 'NONE',  ( 73.28147120125912295, 69.89235501152899133, 9.618937042358501444 ) ) ;
#18618 = B_SPLINE_CURVE_WITH_KNOTS ( 'NONE', 3,
 ( #32038, #10264, #655, #71074 ),
 .UNSPECIFIED., .F., .F.,
 ( 4, 4 ),
 ( 0.01369033625325341563, 0.02232895555845127236 ),
 .UNSPECIFIED. ) ;
#18619 = CARTESIAN_POINT ( 'NONE',  ( 46.20988612576196175, 206.6744531367911009, 4.594050593750047540 ) ) ;
#18620 = DIRECTION ( 'NONE',  ( 0.4999999999999998890, -0.8660254037844385966, 0.000000000000000000 ) ) ;
#18621 = CARTESIAN_POINT ( 'NONE',  ( 85.53328598605538957, 214.0643266524159856, -9.188101187500093303 ) ) ;
#18622 = CARTESIAN_POINT ( 'NONE',  ( 207.4541616930702617, 271.3258470364304458, -6.834942797545373594 ) ) ;
#18624 = CARTESIAN_POINT ( 'NONE',  ( 80.58959146898024528, 51.98427572625367787, -15.62881256032639143 ) ) ;
#18623 = VECTOR ( 'NONE', #73097, 999.9999999999998863 ) ;
#18625 = CARTESIAN_POINT ( 'NONE',  ( 163.2099281326308073, 258.2947298600615227, 16.26832179941359158 ) ) ;
#18627 = FACE_OUTER_BOUND ( 'NONE', #86251, .T. ) ;
#18626 = DIRECTION ( 'NONE',  ( -0.9563064286990887730, 0.2923662333936572488, 0.000000000000000000 ) ) ;
#18628 = CARTESIAN_POINT ( 'NONE',  ( 176.7395174816466579, 270.1897220922618317, -16.92019873687963738 ) ) ;
#18629 = CARTESIAN_POINT ( 'NONE',  ( 29.80674373534435162, 38.18502408145592852, 5.678558825948276656 ) ) ;
#18630 = CARTESIAN_POINT ( 'NONE',  ( 82.91284324307122233, 52.55272390429983176, 15.38138080693978260 ) ) ;
#18631 = CARTESIAN_POINT ( 'NONE',  ( -1.439292958244568821, 176.6427522451419065, 10.00000000000009415 ) ) ;
#18632 = VERTEX_POINT ( 'NONE', #38878 ) ;
#18633 = CARTESIAN_POINT ( 'NONE',  ( 76.00665944866153723, 220.8149278399160664, 9.188101187500093303 ) ) ;
#18634 = CARTESIAN_POINT ( 'NONE',  ( -2.512112762712737091, 143.3759306620403891, -30.52142883766493853 ) ) ;
#18635 = CARTESIAN_POINT ( 'NONE',  ( 198.9721957120447655, 281.0613474150461570, 17.36564602955951386 ) ) ;
#18636 = LINE ( 'NONE', #40895, #42528 ) ;
#18637 = CARTESIAN_POINT ( 'NONE',  ( 153.6273456746711759, 264.5566271899593858, 16.53755489349362051 ) ) ;
#18638 = ORIENTED_EDGE ( 'NONE', *, *, #68695, .F. ) ;
#18639 = DIRECTION ( 'NONE',  ( -0.09547062131716983757, 0.9954322480537355355, 0.000000000000000000 ) ) ;
#18640 = CARTESIAN_POINT ( 'NONE',  ( 189.9423737135788031, 286.7344497837455037, 16.91658226365147755 ) ) ;
#18641 = CARTESIAN_POINT ( 'NONE',  ( 72.60378163331358792, 71.48865662481082950, 5.602150642661395175 ) ) ;
#18642 = CARTESIAN_POINT ( 'NONE',  ( 129.9981042655041392, 235.8615022471901739, 5.000000000000051514 ) ) ;
#18643 = CARTESIAN_POINT ( 'NONE',  ( 157.8239779013331372, 257.2878469527003062, -17.92251383114021479 ) ) ;
#18644 = CARTESIAN_POINT ( 'NONE',  ( 23.71749583336532297, 25.64441083166261492, -10.00000000000000533 ) ) ;
#18645 = ORIENTED_EDGE ( 'NONE', *, *, #70020, .F. ) ;
#18646 = CARTESIAN_POINT ( 'NONE',  ( 168.9664584017443190, 248.6242280028398000, -1.894951047014129752 ) ) ;
#18647 = EDGE_LOOP ( 'NONE', ( #1262, #41630, #45607, #27258 ) ) ;
#18648 = CARTESIAN_POINT ( 'NONE',  ( 202.7599932440484451, 279.4563852894229967, 15.58249343055423353 ) ) ;
#18649 = CARTESIAN_POINT ( 'NONE',  ( 207.1609884636329184, 269.8336379652346295, -0.06011041530970540059 ) ) ;
#18650 = CARTESIAN_POINT ( 'NONE',  ( 149.8778024318413316, 271.4674628212321750, -11.84461879799805750 ) ) ;
#18651 = ADVANCED_FACE ( 'NONE', ( #23176 ), #32383, .F. ) ;
#18652 = ORIENTED_EDGE ( 'NONE', *, *, #28093, .F. ) ;
#18653 = CARTESIAN_POINT ( 'NONE',  ( 173.8149039564748648, 250.7382744391995004, 0.4725378802161041558 ) ) ;
#18654 = ORIENTED_EDGE ( 'NONE', *, *, #20721, .T. ) ;
#18655 = CARTESIAN_POINT ( 'NONE',  ( 72.14394712234364704, 71.70061920742823247, 5.492383471420779095 ) ) ;
#18656 = CARTESIAN_POINT ( 'NONE',  ( 167.5081569794162135, 288.0162707042766783, 1.593351152410132698 ) ) ;
#18657 = CARTESIAN_POINT ( 'NONE',  ( 193.9195169834368073, 280.6179910428906510, -17.69857902634443292 ) ) ;
#18658 = CARTESIAN_POINT ( 'NONE',  ( 192.1486163249491312, 296.6222505933895377, -11.73513860937963571 ) ) ;
#18659 = ORIENTED_EDGE ( 'NONE', *, *, #45660, .T. ) ;
#18660 = VECTOR ( 'NONE', #44808, 1000.000000000000114 ) ;
#18661 = CARTESIAN_POINT ( 'NONE',  ( 34.18979426048111492, 28.24335787977765477, -9.188101187500008038 ) ) ;
#18662 = CARTESIAN_POINT ( 'NONE',  ( 79.85636374066935161, 49.16479052345632539, -14.19701399251250606 ) ) ;
#18663 = CARTESIAN_POINT ( 'NONE',  ( 1.813001633210440611, 27.74720351945397923, -10.00000000000000000 ) ) ;
#18664 = DIRECTION ( 'NONE',  ( -2.816764622163176999E-16, -1.626259812849725466E-16, 1.000000000000000000 ) ) ;
#18665 = ORIENTED_EDGE ( 'NONE', *, *, #41239, .T. ) ;
#18666 = ORIENTED_EDGE ( 'NONE', *, *, #18971, .T. ) ;
#18667 = CARTESIAN_POINT ( 'NONE',  ( 198.2831132362969413, 286.4402291352642465, 17.17725333493805095 ) ) ;
#18669 = CARTESIAN_POINT ( 'NONE',  ( 148.3025927079438304, 273.7793698660844939, -8.046026357031887954 ) ) ;
#18668 = CARTESIAN_POINT ( 'NONE',  ( 163.7729086741176161, 246.9839966035275438, 6.099406794390714204 ) ) ;
#18670 = CARTESIAN_POINT ( 'NONE',  ( 186.8123841630082040, 258.3999256946553942, 3.104652050626591553 ) ) ;
#18671 = FACE_OUTER_BOUND ( 'NONE', #74142, .T. ) ;
#18672 = CARTESIAN_POINT ( 'NONE',  ( 205.2121761402296443, 275.2090799237855094, -14.05269615702442465 ) ) ;
#18673 = CARTESIAN_POINT ( 'NONE',  ( 207.8174097099488620, 270.6966830154477748, -3.591979512285951692 ) ) ;
#18674 = CARTESIAN_POINT ( 'NONE',  ( 166.0516328627014104, 265.6217384291983876, 16.61431992032753868 ) ) ;
#18675 = PLANE ( 'NONE',  #19239 ) ;
#18676 = CARTESIAN_POINT ( 'NONE',  ( 98.90203251333015544, 240.1589784336661637, -6.496448406907675876E-16 ) ) ;
#18677 = VERTEX_POINT ( 'NONE', #72822 ) ;
#18678 = CARTESIAN_POINT ( 'NONE',  ( 150.1524654112955659, 271.3963926634256723, 12.33079788649884456 ) ) ;
#18679 = CARTESIAN_POINT ( 'NONE',  ( 164.5817713503295181, 277.0414339631335565, -13.52591915174977366 ) ) ;
#18680 = VERTEX_POINT ( 'NONE', #3415 ) ;
#18681 = EDGE_LOOP ( 'NONE', ( #16268, #90010, #5450, #96790 ) ) ;
#18682 = CARTESIAN_POINT ( 'NONE',  ( 80.27473767918105807, 44.94266210147404195, -11.24373657056636411 ) ) ;
#18683 = CARTESIAN_POINT ( 'NONE',  ( 28.65277809448527080, 198.8967562850347122, -4.648177544792955347E-16 ) ) ;
#18684 = CARTESIAN_POINT ( 'NONE',  ( 84.89659611704327347, 42.30984424720800519, -0.5111085200278608909 ) ) ;
#18685 = CARTESIAN_POINT ( 'NONE',  ( 206.1405152101578437, 273.6011494880188479, -9.618815605734603480 ) ) ;
#18686 = CARTESIAN_POINT ( 'NONE',  ( 206.8073682671177664, 270.4461261121818438, -4.970999383176901709 ) ) ;
#18687 = CARTESIAN_POINT ( 'NONE',  ( 98.52366704282199805, 221.5643266524159856, -9.188101187500093303 ) ) ;
#18688 = ORIENTED_EDGE ( 'NONE', *, *, #26842, .T. ) ;
#18689 = VECTOR ( 'NONE', #41316, 1000.000000000000000 ) ;
#18690 = ORIENTED_EDGE ( 'NONE', *, *, #57557, .T. ) ;
#18691 = PLANE ( 'NONE',  #2601 ) ;
#18692 = EDGE_LOOP ( 'NONE', ( #83355, #20493, #55172, #21889 ) ) ;
#18693 = AXIS2_PLACEMENT_3D ( 'NONE', #93533, #23574, #16490 ) ;
#18694 = CARTESIAN_POINT ( 'NONE',  ( 75.97482311634344398, 65.22733265193998875, -14.46914695647701343 ) ) ;
#18695 = CARTESIAN_POINT ( 'NONE',  ( 154.1034206470755805, 265.3711135606169478, 16.96274506973287544 ) ) ;
#18696 = EDGE_CURVE ( 'NONE', #99795, #71782, #23542, .T. ) ;
#18697 = CARTESIAN_POINT ( 'NONE',  ( 72.57805760592546562, 69.29498314558189520, -9.228818816694399629 ) ) ;
#18699 = CARTESIAN_POINT ( 'NONE',  ( 87.69076027921141758, 45.30224151825790813, -7.205911438339954955 ) ) ;
#18698 = CARTESIAN_POINT ( 'NONE',  ( 129.0235653626489238, 254.4869531367911577, 4.594050593750046652 ) ) ;
#18700 = DIRECTION ( 'NONE',  ( -0.03487823687206607903, 0.06041087834084090530, 0.9975640502598237536 ) ) ;
#18701 = DIRECTION ( 'NONE',  ( -0.9628097264997621529, 0.2701803667135219689, 0.000000000000000000 ) ) ;
#18702 = ORIENTED_EDGE ( 'NONE', *, *, #82884, .F. ) ;
#18703 = CARTESIAN_POINT ( 'NONE',  ( 156.8296764551412537, 259.0100275755436883, 18.25869368615038013 ) ) ;
#18704 = CARTESIAN_POINT ( 'NONE',  ( 80.84499876707492660, 46.13620846899319616, 11.98265363283131890 ) ) ;
#18705 = CARTESIAN_POINT ( 'NONE',  ( 82.17821026166568288, 40.61471803336392128, -3.350310559445664360 ) ) ;
#18706 = CARTESIAN_POINT ( 'NONE',  ( 188.8869121454080755, 269.5302090799899020, 14.83494772155178332 ) ) ;
#18707 = CARTESIAN_POINT ( 'NONE',  ( 188.7930588916510999, 290.9633865388665299, 14.97457979531618832 ) ) ;
#18708 = DIRECTION ( 'NONE',  ( -6.123233995736783292E-17, 1.060575238724905929E-16, 1.000000000000000000 ) ) ;
#18709 = EDGE_CURVE ( 'NONE', #18235, #88859, #71307, .T. ) ;
#18710 = CYLINDRICAL_SURFACE ( 'NONE', #74492, 70.00000000000002842 ) ;
#18711 = CARTESIAN_POINT ( 'NONE',  ( 203.0105432934428507, 277.9143972074624571, -15.01251885043221002 ) ) ;
#18712 = CARTESIAN_POINT ( 'NONE',  ( 161.6673510627899191, 250.6309293646106653, 13.01175935005004192 ) ) ;
#18713 = CARTESIAN_POINT ( 'NONE',  ( 86.03120134746475856, 45.16028859492116254, 7.773040122391054574 ) ) ;
#18714 = CARTESIAN_POINT ( 'NONE',  ( 17.67616779290014861, 25.90829794293880184, 10.00000000000000355 ) ) ;
#18715 = CARTESIAN_POINT ( 'NONE',  ( 83.13520543127567919, 52.15262426605144697, 14.79738518802720115 ) ) ;
#18716 = CARTESIAN_POINT ( 'NONE',  ( 175.7882114856885210, 291.4026636951798537, -6.622811550496607857 ) ) ;
#18717 = ADVANCED_FACE ( 'NONE', ( #86549 ), #71555, .T. ) ;
#18718 = DIRECTION ( 'NONE',  ( 0.000000000000000000, 0.000000000000000000, 1.000000000000000000 ) ) ;
#18719 = CARTESIAN_POINT ( 'NONE',  ( 27.21537010445218741, 39.21091486745862653, 7.012934429366973338E-14 ) ) ;
#18720 = CARTESIAN_POINT ( 'NONE',  ( 73.74022686020369122, 64.09745181038972817, -13.92561685800006011 ) ) ;
#18721 = CARTESIAN_POINT ( 'NONE',  ( 74.23720666048474470, 55.39997257812912324, 16.12237831225943907 ) ) ;
#18722 = LINE ( 'NONE', #58684, #12617 ) ;
#18723 = CARTESIAN_POINT ( 'NONE',  ( 38.60757266705294910, 27.45404122711136452, -8.090169943749478065 ) ) ;
#18724 = CARTESIAN_POINT ( 'NONE',  ( 78.48263164489894450, 47.83473025059171135, 13.91046930105468959 ) ) ;
#18725 = CARTESIAN_POINT ( 'NONE',  ( 203.2732885619977026, 278.5673317194472247, -16.64305493556850024 ) ) ;
#18726 = CARTESIAN_POINT ( 'NONE',  ( 180.4323844735881437, 272.9924779018138565, 16.99013570338881252 ) ) ;
#18727 = CARTESIAN_POINT ( 'NONE',  ( 87.37773417632490691, 43.73256146576093073, 3.884381177787582740 ) ) ;
#18728 = AXIS2_PLACEMENT_3D ( 'NONE', #22173, #22680, #53559 ) ;
#18729 = CARTESIAN_POINT ( 'NONE',  ( 205.9915890110450505, 273.4897725707952532, -9.552466559589154471 ) ) ;
#18730 = CARTESIAN_POINT ( 'NONE',  ( 16.57566611395445477, 186.5024278399161233, 9.188101187500095079 ) ) ;
#18731 = LINE ( 'NONE', #70937, #33912 ) ;
#18732 = VERTEX_POINT ( 'NONE', #19618 ) ;
#18733 = CARTESIAN_POINT ( 'NONE',  ( 87.11349487006071968, 46.19076519147613169, 8.411924245371462661 ) ) ;
#18734 = CARTESIAN_POINT ( 'NONE',  ( 206.1585898378126274, 271.5698433145930721, 8.212139725584252758 ) ) ;
#18735 = CARTESIAN_POINT ( 'NONE',  ( 208.2555382576270233, 269.9378221106229034, 3.215405476967123199 ) ) ;
#18736 = CARTESIAN_POINT ( 'NONE',  ( 81.85284180441837520, 41.66615176753711580, 5.418929497052564770 ) ) ;
#18737 = CARTESIAN_POINT ( 'NONE',  ( 32.46173284068399312, 198.7369531367911293, -4.594050593750048428 ) ) ;
#18738 = CARTESIAN_POINT ( 'NONE',  ( 40.48539884740146277, 126.3902902409112556, -10.00000000000000000 ) ) ;
#18739 = CARTESIAN_POINT ( 'NONE',  ( 190.1813752874636805, 301.2431906792259042, -4.710625539811892359 ) ) ;
#18740 = CARTESIAN_POINT ( 'NONE',  ( 35.44051388448051654, 36.16454794089042935, -10.00000000000000355 ) ) ;
#18741 = CARTESIAN_POINT ( 'NONE',  ( 181.7166236227738239, 294.4692410469801302, 6.427997548790919780 ) ) ;
#18742 = DIRECTION ( 'NONE',  ( -0.6855440362341557181, 0.7280311630581363103, 0.000000000000000000 ) ) ;
#18744 = CARTESIAN_POINT ( 'NONE',  ( 148.9739782091477309, 272.6164960665341823, 12.45483701539941457 ) ) ;
#18743 = VECTOR ( 'NONE', #72174, 1000.000000000000227 ) ;
#18745 = CARTESIAN_POINT ( 'NONE',  ( 179.6158688349506463, 278.5679919970204423, -16.38266072639121518 ) ) ;
#18746 = CARTESIAN_POINT ( 'NONE',  ( 15.52034749996898633, 9.364779650996391425, 1.583844403245360466 ) ) ;
#18747 = ADVANCED_FACE ( 'NONE', ( #50476 ), #42858, .T. ) ;
#18748 = EDGE_CURVE ( 'NONE', #36466, #81234, #73793, .T. ) ;
#18749 = CARTESIAN_POINT ( 'NONE',  ( 86.84557476849437307, 45.86349151742059860, -8.191698938791937223 ) ) ;
#18750 = CARTESIAN_POINT ( 'NONE',  ( 83.85749844460281111, 51.92724282576335781, 14.91256361652489915 ) ) ;
#18751 = AXIS2_PLACEMENT_3D ( 'NONE', #81060, #98600, #29182 ) ;
#18752 = CARTESIAN_POINT ( 'NONE',  ( 94.05805000844996755, 215.1115022471902023, -5.000000000000041744 ) ) ;
#18753 = CYLINDRICAL_SURFACE ( 'NONE', #74948, 16.60714546451156792 ) ;
#18754 = CARTESIAN_POINT ( 'NONE',  ( 161.9062657679373842, 267.9766905929743643, -17.48695504021573655 ) ) ;
#18755 = CARTESIAN_POINT ( 'NONE',  ( 46.91405240998433612, 188.7048013555409796, 4.594050593750051981 ) ) ;
#18756 = ORIENTED_EDGE ( 'NONE', *, *, #21223, .T. ) ;
#18757 = DIRECTION ( 'NONE',  ( 0.5000000000000001110, -0.8660254037844384856, -0.000000000000000000 ) ) ;
#18758 = CARTESIAN_POINT ( 'NONE',  ( 150.7133245577828689, 269.6038598187387834, -14.58664962216439598 ) ) ;
#18759 = CARTESIAN_POINT ( 'NONE',  ( 181.9559929377375056, 291.6402902057536721, -11.43735378946719372 ) ) ;
#18760 = EDGE_CURVE ( 'NONE', #33613, #82781, #82783, .T. ) ;
#18761 = VERTEX_POINT ( 'NONE', #51477 ) ;
#18762 = CARTESIAN_POINT ( 'NONE',  ( 170.9671437369523517, 287.2122471754595949, 8.607527358884711433 ) ) ;
#18763 = CARTESIAN_POINT ( 'NONE',  ( 207.4826643481121664, 271.2764789897469768, 7.783310782367018454 ) ) ;
#18764 = B_SPLINE_CURVE_WITH_KNOTS ( 'NONE', 3,
 ( #84526, #38870, #45959, #60660 ),
 .UNSPECIFIED., .F., .F.,
 ( 4, 4 ),
 ( 0.008512387967132429428, 0.01362662226579259422 ),
 .UNSPECIFIED. ) ;
#18765 = CARTESIAN_POINT ( 'NONE',  ( 167.0271109968743417, 287.8086958075197686, 0.5416428030073258126 ) ) ;
#18766 = CARTESIAN_POINT ( 'NONE',  ( 20.10065364775352847, 33.64646525600390703, -2.839279412974133887 ) ) ;
#18767 = CARTESIAN_POINT ( 'NONE',  ( 189.7194741408086429, 264.5021160184427913, 10.84982732454233911 ) ) ;
#18768 = CARTESIAN_POINT ( 'NONE',  ( 86.43474555478655930, 47.06867616905372387, -10.03419037324795049 ) ) ;
#18769 = CARTESIAN_POINT ( 'NONE',  ( 204.4345574087956550, 276.5559550755466489, 14.49589339982634861 ) ) ;
#18770 = ORIENTED_EDGE ( 'NONE', *, *, #3999, .T. ) ;
#18771 = CARTESIAN_POINT ( 'NONE',  ( 20.84336723938811176, 14.96004757982089828, -5.678558825948275768 ) ) ;
#18772 = EDGE_CURVE ( 'NONE', #13470, #83200, #75639, .T. ) ;
#18773 = CARTESIAN_POINT ( 'NONE',  ( 172.2368248080031492, 252.4453057155697877, 8.861972572817373717 ) ) ;
#18774 = DIRECTION ( 'NONE',  ( 0.09248003802711829424, -0.9957145386939485476, 0.000000000000000000 ) ) ;
#18775 = EDGE_CURVE ( 'NONE', #47896, #88729, #58018, .T. ) ;
#18776 = EDGE_LOOP ( 'NONE', ( #89628, #69350, #95942 ) ) ;
#18777 = CARTESIAN_POINT ( 'NONE',  ( 179.2225705765399084, 282.9028557827877535, 16.02728324287294370 ) ) ;
#18778 = CARTESIAN_POINT ( 'NONE',  ( 191.5544531425776427, 298.8649500714207647, 8.366689293739112188 ) ) ;
#18779 = CARTESIAN_POINT ( 'NONE',  ( 45.56181175559624563, 118.5014625327306135, -10.00000000000000000 ) ) ;
#18780 = DIRECTION ( 'NONE',  ( 0.4999999999999998890, -0.8660254037844385966, 0.000000000000000000 ) ) ;
#18781 = ORIENTED_EDGE ( 'NONE', *, *, #77601, .F. ) ;
#18782 = ORIENTED_EDGE ( 'NONE', *, *, #45353, .F. ) ;
#18784 = CARTESIAN_POINT ( 'NONE',  ( -22.42236680055709641, 157.8615022471902591, 0.000000000000000000 ) ) ;
#18783 = CARTESIAN_POINT ( 'NONE',  ( 207.5462191418491500, 271.1663988579299485, -5.239401497773396699 ) ) ;
#18785 = CARTESIAN_POINT ( 'NONE',  ( 149.2765980486851731, 272.0923431290771646, -11.40617906909507973 ) ) ;
#18786 = ORIENTED_EDGE ( 'NONE', *, *, #80555, .T. ) ;
#18787 = CARTESIAN_POINT ( 'NONE',  ( 66.17343954913513926, 68.52301864461628611, -2.711686016849376379 ) ) ;
#18788 = CARTESIAN_POINT ( 'NONE',  ( 198.2819808855875863, 287.2125302111982705, 18.53535247371401695 ) ) ;
#18789 = CARTESIAN_POINT ( 'NONE',  ( 72.94747645884849874, 57.63385081541922972, -16.31741162060431805 ) ) ;
#18790 = CARTESIAN_POINT ( 'NONE',  ( 78.12678986096226197, 61.01961664896378323, -15.90133184208619710 ) ) ;
#18791 = CARTESIAN_POINT ( 'NONE',  ( 157.2104826425669728, 258.3504519110855995, -16.92635148710569482 ) ) ;
#18792 = CARTESIAN_POINT ( 'NONE',  ( 118.1714448432989144, 239.0333772461660544, 9.188101187500095079 ) ) ;
#18793 = CARTESIAN_POINT ( 'NONE',  ( -19.65312891409030271, 93.06504152958497400, 10.00000000000000888 ) ) ;
#18794 = VECTOR ( 'NONE', #68755, 1000.000000000000000 ) ;
#18795 = CARTESIAN_POINT ( 'NONE',  ( 164.1821508476733698, 246.2751683663292397, -7.347745041495428175 ) ) ;
#18796 = ORIENTED_EDGE ( 'NONE', *, *, #50025, .T. ) ;
#18797 = CARTESIAN_POINT ( 'NONE',  ( 36.63328578856461348, 23.01110640527294748, 2.839279412974134775 ) ) ;
#18798 = FACE_BOUND ( 'NONE', #35585, .T. ) ;
#18799 = CARTESIAN_POINT ( 'NONE',  ( 68.00890493122102498, 70.09522272019684408, -2.916841246453294456 ) ) ;
#18800 = CARTESIAN_POINT ( 'NONE',  ( 63.96340690334295687, 216.9244531367911293, -4.594050593750046652 ) ) ;
#18801 = CARTESIAN_POINT ( 'NONE',  ( 73.76584831522593788, 68.38082682530667000, 11.49424229391077290 ) ) ;
#18802 = CARTESIAN_POINT ( 'NONE',  ( 150.8359915840788688, 269.3913942967808453, 15.73449616766854575 ) ) ;
#18803 = CARTESIAN_POINT ( 'NONE',  ( 150.8613910702043768, 269.3474010963252567, 15.19517615056406612 ) ) ;
#18804 = AXIS2_PLACEMENT_3D ( 'NONE', #58676, #19721, #58193 ) ;
#18805 = DIRECTION ( 'NONE',  ( -0.5000000000000002220, 0.8660254037844384856, 0.000000000000000000 ) ) ;
#18806 = EDGE_LOOP ( 'NONE', ( #4302, #93503, #69008, #60102 ) ) ;
#18807 = CARTESIAN_POINT ( 'NONE',  ( 74.70131395912255812, 58.53265795774088076, -15.87551583097357799 ) ) ;
#18808 = CARTESIAN_POINT ( 'NONE',  ( 191.2649737798357705, 297.3663430354321235, 11.06343876070684296 ) ) ;
#18809 = EDGE_LOOP ( 'NONE', ( #10926, #45886, #28773, #6898 ) ) ;
#18810 = CARTESIAN_POINT ( 'NONE',  ( 172.2332593386741735, 258.4530275332109568, -14.26710149980596576 ) ) ;
#18811 = CARTESIAN_POINT ( 'NONE',  ( 67.35737046155603025, 69.12142928160184852, -3.136879690473392213 ) ) ;
#18812 = FACE_OUTER_BOUND ( 'NONE', #48323, .T. ) ;
#18813 = CARTESIAN_POINT ( 'NONE',  ( -19.65312891409030271, 93.06504152958497400, -10.00000000000000888 ) ) ;
#18814 = CARTESIAN_POINT ( 'NONE',  ( 148.9517569034208009, 272.6549844970639924, 12.50737104496728236 ) ) ;
#18815 = CARTESIAN_POINT ( 'NONE',  ( 180.7461886851734789, 271.3453486839773063, 16.63588864205645379 ) ) ;
#18816 = ADVANCED_FACE ( 'NONE', ( #90533 ), #21103, .T. ) ;
#18817 = DIRECTION ( 'NONE',  ( 0.2551196190400365493, 0.9669094993746139011, 0.000000000000000000 ) ) ;
#18818 = CARTESIAN_POINT ( 'NONE',  ( -19.74273382965125379, 93.17497195189844206, 59.99999999999999289 ) ) ;
#18819 = CARTESIAN_POINT ( 'NONE',  ( 164.2695167311736668, 253.9159192467835169, 14.61855453912878211 ) ) ;
#18820 = ORIENTED_EDGE ( 'NONE', *, *, #42814, .T. ) ;
#18821 = CARTESIAN_POINT ( 'NONE',  ( 164.3890147726454813, 245.9168695380243435, -6.010262808998044548 ) ) ;
#18822 = CARTESIAN_POINT ( 'NONE',  ( 117.9006383567337792, 245.0024278399160949, 9.188101187500095079 ) ) ;
#18823 = EDGE_LOOP ( 'NONE', ( #1308, #71280, #11089, #25274 ) ) ;
#18824 = VECTOR ( 'NONE', #58652, 999.9999999999998863 ) ;
#18825 = CARTESIAN_POINT ( 'NONE',  ( 82.88002151971222986, 44.20230398355771229, -8.882486828932147915 ) ) ;
#18826 = DIRECTION ( 'NONE',  ( -0.2473641778533917646, -0.9689225787001330970, 0.000000000000000000 ) ) ;
#18827 = APPLICATION_CONTEXT ( 'automotive_design' ) ;
#18828 = EDGE_CURVE ( 'NONE', #90614, #4734, #52467, .T. ) ;
#18829 = CARTESIAN_POINT ( 'NONE',  ( 155.5066938333533528, 261.3015006940112244, -18.40036130547566273 ) ) ;
#18830 = CIRCLE ( 'NONE', #52707, 0.1418229129681522482 ) ;
#18831 = CARTESIAN_POINT ( 'NONE',  ( 204.9103773355753617, 275.7318107871104189, 13.62808820451859937 ) ) ;
#18832 = CARTESIAN_POINT ( 'NONE',  ( 82.35975313173908319, 41.41624149291902057, 5.521678208619409389 ) ) ;
#18833 = CARTESIAN_POINT ( 'NONE',  ( 178.0467360553784033, 255.3817929127459934, 4.775061655386900306 ) ) ;
#18834 = ORIENTED_EDGE ( 'NONE', *, *, #66450, .F. ) ;
#18835 = CARTESIAN_POINT ( 'NONE',  ( 80.48346613340457623, 57.68579040447578166, -16.59506630531065241 ) ) ;
#18836 =( BOUNDED_CURVE ( )  B_SPLINE_CURVE ( 2, ( #31736, #47448, #78377, #8958, #63656, #15538, #9469, #25150, #40339, #63154, #46438, #84503, #70249 ),
 .UNSPECIFIED., .F., .T. ) 
 B_SPLINE_CURVE_WITH_KNOTS ( ( 3, 2, 2, 2, 2, 2, 3 ),
 ( 0.7125000000000000222, 0.7149999999999999689, 0.7199999999999999734, 0.7249999999999999778, 0.7299999999999999822, 0.7349999999999999867, 0.7375000000000000444 ),
 .UNSPECIFIED. ) 
 CURVE ( )  GEOMETRIC_REPRESENTATION_ITEM ( )  RATIONAL_B_SPLINE_CURVE ( ( 0.9755282581475767101, 0.9755282581475772652, 1.000000000000000000, 0.9510565162951535312, 1.000000000000000000, 0.9510565162951535312, 1.000000000000000000, 0.9510565162951535312, 1.000000000000000000, 0.9510565162951535312, 1.000000000000000000, 0.9755282581475761550, 0.9755282581475767101 ) ) 
 REPRESENTATION_ITEM ( '' )  );
#18837 = CARTESIAN_POINT ( 'NONE',  ( 158.5141842721128285, 275.0039168403922645, -12.51588967219915816 ) ) ;
#18839 = DIRECTION ( 'NONE',  ( -0.8660254037844377084, -0.5000000000000014433, -0.000000000000000000 ) ) ;
#18838 = FACE_OUTER_BOUND ( 'NONE', #79974, .T. ) ;
#18840 = CARTESIAN_POINT ( 'NONE',  ( 164.4306612431381325, 245.8447357351751066, -2.314684942147286595 ) ) ;
#18841 = CARTESIAN_POINT ( 'NONE',  ( 142.5284093247362591, 253.0958772461660544, -9.188101187500095079 ) ) ;
#18842 = ADVANCED_FACE ( 'NONE', ( #34775 ), #30167, .T. ) ;
#18843 = CARTESIAN_POINT ( 'NONE',  ( 189.0276693039769498, 300.1137990693615620, -3.525949465148791262 ) ) ;
#18844 = LINE ( 'NONE', #19838, #7703 ) ;
#18845 = CARTESIAN_POINT ( 'NONE',  ( 150.5438776023515004, 278.3016033182416322, -9.804454847755098641E-05 ) ) ;
#18846 = CARTESIAN_POINT ( 'NONE',  ( 72.21814540286966633, 206.3768266524159856, -9.188101187500091527 ) ) ;
#18847 = CARTESIAN_POINT ( 'NONE',  ( 157.8429099974857195, 257.2550556002704525, -17.85752049034686095 ) ) ;
#18848 = CARTESIAN_POINT ( 'NONE',  ( 174.6639587582037620, 252.0453782210719282, 3.541528378334539262 ) ) ;
#18849 = EDGE_CURVE ( 'NONE', #65623, #88359, #32544, .T. ) ;
#18850 = CARTESIAN_POINT ( 'NONE',  ( 22.75701074986381656, 14.10801979619928659, 3.090169943749476733 ) ) ;
#18851 = ADVANCED_FACE ( 'NONE', ( #7359 ), #53456, .T. ) ;
#18852 = CARTESIAN_POINT ( 'NONE',  ( 190.6661865267473104, 300.4034729807058852, 4.523489664447863490 ) ) ;
#18853 = CARTESIAN_POINT ( 'NONE',  ( 155.3925584512507498, 279.7696002511819415, -1.290171526702664995 ) ) ;
#18854 = CARTESIAN_POINT ( 'NONE',  ( 172.5626239099614168, 287.5492475841473379, -8.221891676024617013 ) ) ;
#18855 = CARTESIAN_POINT ( 'NONE',  ( 203.0026270830780675, 279.0361311525880978, -16.61345826058821373 ) ) ;
#18856 = CARTESIAN_POINT ( 'NONE',  ( 193.5438442197551296, 288.5803156727525902, 16.04593160988459033 ) ) ;
#18857 = CARTESIAN_POINT ( 'NONE',  ( 126.8046355855010603, 254.0177522451418781, 5.000000000000046185 ) ) ;
#18858 = CARTESIAN_POINT ( 'NONE',  ( 84.60735463175657856, 50.53152741511170376, -13.60229262012000184 ) ) ;
#18859 = ORIENTED_EDGE ( 'NONE', *, *, #39874, .F. ) ;
#18860 = CARTESIAN_POINT ( 'NONE',  ( 157.8092552871339365, 257.3133472685137235, 17.04082256169242626 ) ) ;
#18861 = CARTESIAN_POINT ( 'NONE',  ( 158.8266160086023149, 257.5512268093053194, -17.29683829744028856 ) ) ;
#18862 = CARTESIAN_POINT ( 'NONE',  ( -5.724140937729832679, 161.3768266524159856, -9.188101187500093303 ) ) ;
#18863 = VECTOR ( 'NONE', #20204, 1000.000000000000000 ) ;
#18864 = CARTESIAN_POINT ( 'NONE',  ( 45.07374842694240868, 187.6423013555410080, -4.594050593750043987 ) ) ;
#18865 = CARTESIAN_POINT ( 'NONE',  ( 175.3888197414261185, 256.6087255675022902, -10.77910597738013898 ) ) ;
#18866 = CARTESIAN_POINT ( 'NONE',  ( 22.92804849793282784, 21.43677371833801715, -10.00000000000000355 ) ) ;
#18867 = CARTESIAN_POINT ( 'NONE',  ( -72.30469571560091424, 48.86078274006646183, -10.00000000000000000 ) ) ;
#18868 = CARTESIAN_POINT ( 'NONE',  ( 157.8429099974857195, 257.2550556002704525, -17.85752049034686095 ) ) ;
#18869 = CARTESIAN_POINT ( 'NONE',  ( 192.0603001030472683, 293.3461588932823929, -14.68827779892621344 ) ) ;
#18870 = CARTESIAN_POINT ( 'NONE',  ( 190.6954410837624607, 300.3528026016029457, -5.728531842148099962 ) ) ;
#18871 = CARTESIAN_POINT ( 'NONE',  ( 74.13238489426800015, 55.63346398866154630, -16.58957000666680059 ) ) ;
#18872 = EDGE_CURVE ( 'NONE', #59884, #49538, #7765, .T. ) ;
#18874 = CARTESIAN_POINT ( 'NONE',  ( 47.20246722098136871, 211.3927522451419350, 2.944929066748280225E-16 ) ) ;
#18873 = CARTESIAN_POINT ( 'NONE',  ( 67.04888272437477781, 219.5177522451419065, 5.000000000000046185 ) ) ;
#18875 = CARTESIAN_POINT ( 'NONE',  ( 181.3255421082058376, 255.3544676688379127, 2.128643196724650632 ) ) ;
#18876 = CARTESIAN_POINT ( 'NONE',  ( 205.2391015854675516, 275.1624436846170738, -14.01434138479280911 ) ) ;
#18877 = DIRECTION ( 'NONE',  ( 0.000000000000000000, 0.000000000000000000, 1.000000000000000000 ) ) ;
#18878 = CONICAL_SURFACE ( 'NONE', #99792, 3.299999999999978950, 1.029744258676652313 ) ;
#18879 = EDGE_CURVE ( 'NONE', #16411, #8947, #87321, .T. ) ;
#18880 = CARTESIAN_POINT ( 'NONE',  ( 161.7323330629232316, 267.3777249680341015, 16.49771666234070366 ) ) ;
#18881 = CARTESIAN_POINT ( 'NONE',  ( 53.71569994882487009, 188.4865022471901455, 1.119607411625061291E-15 ) ) ;
#18882 = CARTESIAN_POINT ( 'NONE',  ( 183.4669127592752034, 292.6857018627941898, 9.408060097649215692 ) ) ;
#18883 = DIRECTION ( 'NONE',  ( 1.000000000000000000, 0.000000000000000000, 0.000000000000000000 ) ) ;
#18884 = CARTESIAN_POINT ( 'NONE',  ( -2.963858511049441979, 169.0958772461660544, -9.188101187500095079 ) ) ;
#18885 = CARTESIAN_POINT ( 'NONE',  ( 40.83172133312034191, 29.28920272979929962, -7.433330006724141015 ) ) ;
#18886 = CARTESIAN_POINT ( 'NONE',  ( -13.86269525828469895, 104.2312461070084879, 10.61543114587583148 ) ) ;
#18887 = CARTESIAN_POINT ( 'NONE',  ( 30.74798454907712042, 181.8927522451418497, 10.00000000000009948 ) ) ;
#18888 = CARTESIAN_POINT ( 'NONE',  ( 36.24660459446916150, 29.43085787977765833, -9.188101187500008038 ) ) ;
#18889 = CARTESIAN_POINT ( 'NONE',  ( 165.0020474182383339, 244.8550658491588479, 1.825383354618924425 ) ) ;
#18890 = CARTESIAN_POINT ( 'NONE',  ( 182.6449127974795203, 278.5736680211113594, 16.63823239613948601 ) ) ;
#18891 = ADVANCED_FACE ( 'NONE', ( #60550 ), #10248, .F. ) ;
#18892 = DIRECTION ( 'NONE',  ( -0.8660254037844387076, -0.4999999999999998890, -0.000000000000000000 ) ) ;
#18893 = LINE ( 'NONE', #9799, #18623 ) ;
#18894 = CARTESIAN_POINT ( 'NONE',  ( 176.5378754974050821, 260.2610757822269534, -13.57310438010597586 ) ) ;
#18895 = DIRECTION ( 'NONE',  ( 0.000000000000000000, 0.000000000000000000, 1.000000000000000000 ) ) ;
#18896 = CARTESIAN_POINT ( 'NONE',  ( 9.248262631489305718, 13.84335787977760823, 9.188101187500006262 ) ) ;
#18897 = CARTESIAN_POINT ( 'NONE',  ( 153.2955602623325149, 277.6818314479798460, -5.275435393451455290 ) ) ;
#18898 = CARTESIAN_POINT ( 'NONE',  ( 14.38185574516869458, 23.70171378149918340, -9.188101187500004485 ) ) ;
#18899 = CARTESIAN_POINT ( 'NONE',  ( 158.3828892404620490, 259.0189987438004096, 16.74082065088548177 ) ) ;
#18900 = EDGE_CURVE ( 'NONE', #54972, #16763, #12632, .T. ) ;
#18901 = CARTESIAN_POINT ( 'NONE',  ( 193.7999837595647250, 294.9755769528473479, 15.24609078262870199 ) ) ;
#18902 = VECTOR ( 'NONE', #70627, 1000.000000000000114 ) ;
#18903 = FACE_OUTER_BOUND ( 'NONE', #1497, .T. ) ;
#18904 = EDGE_CURVE ( 'NONE', #7425, #52455, #74047, .T. ) ;
#18905 = CARTESIAN_POINT ( 'NONE',  ( 206.1405152101578437, 273.6011494880188479, -9.618815605734603480 ) ) ;
#18906 = ORIENTED_EDGE ( 'NONE', *, *, #6026, .T. ) ;
#18907 = LINE ( 'NONE', #80744, #63509 ) ;
#18908 = CARTESIAN_POINT ( 'NONE',  ( 164.7243055739305078, 245.3361288348881999, -1.445094907380085170 ) ) ;
#18910 = B_SPLINE_CURVE_WITH_KNOTS ( 'NONE', 3,
 ( #75822, #38274, #21609, #5900, #100115, #30700, #52489, #84927, #37291, #37781, #76317, #60575, #291, #91531, #99615, #30193, #61079, #15473, #67703, #52992, #14003, #98630, #6409, #16488, #40768, #33192, #17491, #71212, #87475, #18009, #70177, #39267, #85442, #48397 ),
 .UNSPECIFIED., .F., .F.,
 ( 4, 2, 2, 2, 2, 2, 2, 2, 2, 2, 2, 2, 2, 2, 2, 2, 4 ),
 ( 0.003332772792290249371, 0.003484938153222827580, 0.003637103514155405788, 0.003713186194621726551, 0.003789268875088047314, 0.003941434236020691442, 0.004245764957886018730, 0.004550095679751345150, 0.005158757123481937275, 0.005767418567212528532, 0.006984741454673737068, 0.007593402898404376031, 0.007897733620269692043, 0.008049898981202348314, 0.008125981661668640887, 0.008164023001901790644, 0.008202064342134938665 ),
 .UNSPECIFIED. ) ;
#18909 = VECTOR ( 'NONE', #10012, 1000.000000000000000 ) ;
#18911 = CARTESIAN_POINT ( 'NONE',  ( 66.51592627583551121, 68.71315881233805101, 4.796467218963683443 ) ) ;
#18912 = CARTESIAN_POINT ( 'NONE',  ( 87.70668618551661666, 45.11329565042247935, 6.837976445409220894 ) ) ;
#18913 = ORIENTED_EDGE ( 'NONE', *, *, #70133, .T. ) ;
#18914 = VERTEX_POINT ( 'NONE', #95401 ) ;
#18916 = CARTESIAN_POINT ( 'NONE',  ( 63.51261232558832859, 214.1427522451419350, 10.00000000000009415 ) ) ;
#18915 = CARTESIAN_POINT ( 'NONE',  ( 159.6998082543438500, 278.4571990200508935, -9.779246870798463220 ) ) ;
#18917 = CARTESIAN_POINT ( 'NONE',  ( 86.47115166784590201, 47.25330420953332577, 10.74459335058070941 ) ) ;
#18918 = ORIENTED_EDGE ( 'NONE', *, *, #39476, .F. ) ;
#18919 = CARTESIAN_POINT ( 'NONE',  ( 76.75404550250510738, 52.66510328405545494, 15.83505843469623287 ) ) ;
#18920 = CARTESIAN_POINT ( 'NONE',  ( 199.0746189151364831, 265.2438329385483939, 1.559867394473611002 ) ) ;
#18921 = ORIENTED_EDGE ( 'NONE', *, *, #95869, .F. ) ;
#18922 = CARTESIAN_POINT ( 'NONE',  ( 68.96058394729804775, 64.32740065508541250, -11.90885421820057921 ) ) ;
#18923 = CARTESIAN_POINT ( 'NONE',  ( 77.66333127137711756, 50.58589379260305918, -15.22707563559156263 ) ) ;
#18924 = B_SPLINE_CURVE_WITH_KNOTS ( 'NONE', 3,
 ( #98568, #62004, #92955, #60022, #23508, #86893, #8825, #24023, #40715, #24524, #33129, #54921, #62502, #47319, #94466, #33645, #85899, #16424 ),
 .UNSPECIFIED., .F., .F.,
 ( 4, 2, 2, 2, 2, 2, 2, 2, 4 ),
 ( 6.399695615700000250E-17, 0.0002914903321845351307, 0.0005829806643690061850, 0.0008744709965534773477, 0.001165961328737948402, 0.001457451660922419456, 0.001748941993106890727, 0.002040432325291361999, 0.002331922657475833053 ),
 .UNSPECIFIED. ) ;
#18925 = CARTESIAN_POINT ( 'NONE',  ( 80.72327543658212790, 43.19257391986853634, 9.937540063720549099 ) ) ;
#18926 = ORIENTED_EDGE ( 'NONE', *, *, #20845, .F. ) ;
#18927 = CARTESIAN_POINT ( 'NONE',  ( 174.8111530639320108, 267.9940263390942619, 16.29984105809692707 ) ) ;
#18928 = CARTESIAN_POINT ( 'NONE',  ( 166.1857273590558179, 273.8697761094379644, -16.44210238554618897 ) ) ;
#18929 = DIRECTION ( 'NONE',  ( 0.000000000000000000, 0.000000000000000000, 1.000000000000000000 ) ) ;
#18930 = EDGE_LOOP ( 'NONE', ( #38992, #72664 ) ) ;
#18931 = DIRECTION ( 'NONE',  ( 0.4999999999999992784, -0.8660254037844390407, 0.000000000000000000 ) ) ;
#18932 = CARTESIAN_POINT ( 'NONE',  ( 163.1332433029523372, 248.0919295262283981, 11.24052392390482957 ) ) ;
#18933 = ORIENTED_EDGE ( 'NONE', *, *, #36758, .T. ) ;
#18934 = CARTESIAN_POINT ( 'NONE',  ( 34.81516168915607068, 51.10768172523390973, -10.00000000000000000 ) ) ;
#18935 = ORIENTED_EDGE ( 'NONE', *, *, #85133, .F. ) ;
#18936 = CARTESIAN_POINT ( 'NONE',  ( 157.5954339963122663, 268.8483900235063402, 15.63267351098963154 ) ) ;
#18937 = ORIENTED_EDGE ( 'NONE', *, *, #85972, .T. ) ;
#18938 = DIRECTION ( 'NONE',  ( -0.4996954135095461047, 0.8654978445076770832, -0.03489949670251103753 ) ) ;
#18939 = B_SPLINE_CURVE_WITH_KNOTS ( 'NONE', 3,
 ( #79682, #10244, #60786, #75532, #20844, #75042, #76045, #43614, #98339, #90775, #90273, #30415, #45598, #91751, #20337, #28932, #99829, #52206, #60292, #51737, #5129, #22314, #29421, #51210, #59806, #21326, #82175, #83154, #37012, #13721, #12751, #13244, #28413, #89767, #29916, #44597, #6626, #98842, #59292, #74553, #36012, #53217, #66914, #6116, #67921, #91251, #21815, #84168, #37992, #7109 ),
 .UNSPECIFIED., .F., .F.,
 ( 4, 2, 2, 2, 2, 2, 2, 2, 2, 2, 2, 2, 2, 2, 2, 2, 2, 2, 2, 2, 2, 2, 2, 2, 4 ),
 ( 0.001915670005683367365, 0.002365191695059523820, 0.002589952539747623732, 0.002814713384435723210, 0.002927093806779732400, 0.003039474229123741589, 0.003151854651467750346, 0.003264235073811759969, 0.003488995918499739751, 0.003713756763187719100, 0.004163278452563567641, 0.004612800141939415316, 0.005511843520691112400, 0.006410886899442808616, 0.006860408588818692720, 0.007309930278194576823, 0.007422310700538548717, 0.007478500911710535097, 0.007534691122882520610, 0.007647071545226449135, 0.007759451967570377660, 0.008208973656945820277, 0.008658495346321262026, 0.008883256191009034075, 0.009108017035696806124 ),
 .UNSPECIFIED. ) ;
#18940 = CARTESIAN_POINT ( 'NONE',  ( 147.3627346024176461, 275.4072518567613201, 7.337996838423670454 ) ) ;
#18941 = DIRECTION ( 'NONE',  ( 0.4999999999999992784, -0.8660254037844390407, 0.000000000000000000 ) ) ;
#18942 = CARTESIAN_POINT ( 'NONE',  ( 69.87185781331436374, 66.10011063722555491, 10.85240889336124859 ) ) ;
#18943 = CARTESIAN_POINT ( 'NONE',  ( 193.6023084030469761, 294.8553025941217243, 13.33578009685492560 ) ) ;
#18944 = CARTESIAN_POINT ( 'NONE',  ( 178.5465195133704981, 291.5681621643464041, 6.587540641832299038 ) ) ;
#18945 = CARTESIAN_POINT ( 'NONE',  ( 197.4356762619225663, 288.6783728180664070, -16.68343683487013962 ) ) ;
#18946 = ORIENTED_EDGE ( 'NONE', *, *, #43385, .T. ) ;
#18947 = LINE ( 'NONE', #49826, #33470 ) ;
#18948 = CARTESIAN_POINT ( 'NONE',  ( 29.70508255828911004, 19.01110640527293327, 2.839279412974134775 ) ) ;
#18949 = AXIS2_PLACEMENT_3D ( 'NONE', #1621, #32507, #33506 ) ;
#18950 = CARTESIAN_POINT ( 'NONE',  ( 165.0020474182383339, 244.8550658491588479, 1.825383354618924425 ) ) ;
#18952 = ORIENTED_EDGE ( 'NONE', *, *, #5997, .T. ) ;
#18951 = CARTESIAN_POINT ( 'NONE',  ( 198.6742831389107096, 286.5330427765190393, 17.60232614297041565 ) ) ;
#18953 = AXIS2_PLACEMENT_3D ( 'NONE', #40053, #33480, #3114 ) ;
#18954 = ORIENTED_EDGE ( 'NONE', *, *, #72190, .F. ) ;
#18955 = CARTESIAN_POINT ( 'NONE',  ( 190.8281514355135187, 300.1229415296796788, 6.778607853984104814 ) ) ;
#18956 = CARTESIAN_POINT ( 'NONE',  ( 171.5651214720799373, 259.5975988575258953, -15.07810809630464099 ) ) ;
#18957 = CARTESIAN_POINT ( 'NONE',  ( 163.9564365344733687, 247.8982689250301235, 8.517658320392268223 ) ) ;
#18958 = PLANE ( 'NONE',  #36023 ) ;
#18959 = B_SPLINE_CURVE_WITH_KNOTS ( 'NONE', 3,
 ( #54165, #69390, #67901, #98821 ),
 .UNSPECIFIED., .F., .F.,
 ( 4, 4 ),
 ( 0.000000000000000000, 0.005725910648720425322 ),
 .UNSPECIFIED. ) ;
#18960 = CARTESIAN_POINT ( 'NONE',  ( 47.74604483422196921, 186.8262482093457777, 3.021315404115420679E-15 ) ) ;
#18961 = CARTESIAN_POINT ( 'NONE',  ( 148.7072594763547215, 273.0784664630622274, -9.449416077291342475 ) ) ;
#18962 = VERTEX_POINT ( 'NONE', #97358 ) ;
#18963 = LINE ( 'NONE', #3756, #81807 ) ;
#18964 = CIRCLE ( 'NONE', #75557, 70.00000000000001421 ) ;
#18965 = LINE ( 'NONE', #73165, #88930 ) ;
#18966 = CARTESIAN_POINT ( 'NONE',  ( 47.13029843733273339, 198.0177522451418781, -10.00000000000009592 ) ) ;
#18967 = B_SPLINE_CURVE_WITH_KNOTS ( 'NONE', 3,
 ( #38922, #8049, #86104, #63737 ),
 .UNSPECIFIED., .F., .F.,
 ( 4, 4 ),
 ( 0.9262915356181703475, 1.000000000000000000 ),
 .UNSPECIFIED. ) ;
#18968 = CARTESIAN_POINT ( 'NONE',  ( 196.4287751515431921, 269.1031666285815618, -12.09581130873691279 ) ) ;
#18969 = CARTESIAN_POINT ( 'NONE',  ( 34.06774859691741142, 197.1427522451419350, -10.00000000000009415 ) ) ;
#18970 = CARTESIAN_POINT ( 'NONE',  ( 102.6097905472235539, 239.2369531367911009, -4.594050593750048428 ) ) ;
#18971 = EDGE_CURVE ( 'NONE', #9320, #94434, #27924, .T. ) ;
#18972 = CARTESIAN_POINT ( 'NONE',  ( 181.3921258689275646, 294.4728088502279775, -2.647902565978816014 ) ) ;
#18973 = B_SPLINE_CURVE_WITH_KNOTS ( 'NONE', 3,
 ( #52690, #83651, #14210, #76992, #46583, #38986, #15, #45588, #76514, #46081, #6614, #37979, #84157, #76036, #30900, #7098, #60775, #7599, #30400, #37487, #68397, #31392, #86165, #38486, #61788, #16201, #39471, #91739, #503, #47093, #68890, #69400, #99323, #14703, #29902, #92734, #92256, #99817, #84640, #61292, #8112, #22805, #53683, #22302, #53202, #78014, #8605, #15180 ),
 .UNSPECIFIED., .F., .F.,
 ( 4, 2, 2, 2, 2, 2, 2, 2, 2, 2, 2, 2, 2, 2, 2, 2, 2, 2, 2, 2, 2, 2, 2, 4 ),
 ( 0.0006084983335041455922, 0.001036156343644727140, 0.001249985348714947007, 0.001356899851249977144, 0.001463814353785007280, 0.001677643358855142146, 0.001891472363925276795, 0.002319130374065546743, 0.003174446394346166437, 0.004029762414626786998, 0.004885078434907406258, 0.005312736445047754053, 0.005526565450117964379, 0.005633479952653145870, 0.005686937203920737482, 0.005740394455188327361, 0.005793851706455918973, 0.005847308957723510586, 0.005954223460258693812, 0.006168052465329072406, 0.006595710475469845208, 0.007023368485610619744, 0.007237197490680984460, 0.007451026495751349177 ),
 .UNSPECIFIED. ) ;
#18974 = CARTESIAN_POINT ( 'NONE',  ( 22.16837966976980567, 14.92755873383626053, 6.180339887498953466 ) ) ;
#18975 = CARTESIAN_POINT ( 'NONE',  ( 162.4419666585835387, 249.2892557963607203, 10.75794555938079711 ) ) ;
#18976 = CARTESIAN_POINT ( 'NONE',  ( 14.70821206310299978, 188.4869531367911293, 4.594050593750046652 ) ) ;
#18977 = CARTESIAN_POINT ( 'NONE',  ( 161.6707029936031574, 250.6251236501384483, 14.45053103226186231 ) ) ;
#18978 = ORIENTED_EDGE ( 'NONE', *, *, #66938, .F. ) ;
#18979 = CIRCLE ( 'NONE', #31876, 12.50000000000000000 ) ;
#18980 = VERTEX_POINT ( 'NONE', #33546 ) ;
#18981 = CARTESIAN_POINT ( 'NONE',  ( 185.1894006957831778, 259.9970902747327841, -5.780845478426857476 ) ) ;
#18982 = ADVANCED_FACE ( 'NONE', ( #79687 ), #13725, .T. ) ;
#18983 = CARTESIAN_POINT ( 'NONE',  ( 67.54335693373008098, 69.17532794797624263, 3.376759353522594154 ) ) ;
#18984 = EDGE_CURVE ( 'NONE', #1813, #57272, #93110, .T. ) ;
#18985 = CARTESIAN_POINT ( 'NONE',  ( 190.2510882691990730, 301.1224442529128851, -5.480893437181090455 ) ) ;
#18986 = CARTESIAN_POINT ( 'NONE',  ( 192.9730208252800594, 263.8306068669091360, -4.263488463504454096 ) ) ;
#18987 = CARTESIAN_POINT ( 'NONE',  ( 161.6923300915171922, 250.5876644177310482, -14.43081872899884566 ) ) ;
#18988 = CARTESIAN_POINT ( 'NONE',  ( 185.8754509513723576, 286.6007344811247890, 15.75805532497020423 ) ) ;
#18989 = CARTESIAN_POINT ( 'NONE',  ( 99.88567928453475986, 235.1427522451419065, 10.00000000000009415 ) ) ;
#18990 = CARTESIAN_POINT ( 'NONE',  ( 49.32242524243604720, 199.2833772461660828, -9.188101187500095079 ) ) ;
#18991 = CARTESIAN_POINT ( 'NONE',  ( 79.10106959370823176, 223.1427522451419065, 10.00000000000009237 ) ) ;
#18992 = ORIENTED_EDGE ( 'NONE', *, *, #25243, .F. ) ;
#18993 = CARTESIAN_POINT ( 'NONE',  ( 84.65781438197950592, 49.52625469906533340, 12.95988928232620374 ) ) ;
#18994 = CARTESIAN_POINT ( 'NONE',  ( 158.0503757190722354, 282.4476557944344108, -1.686668573986806585 ) ) ;
#18995 = CARTESIAN_POINT ( 'NONE',  ( -3.667330603741788320, 162.5643266524160140, 9.188101187500095079 ) ) ;
#18996 = B_SPLINE_CURVE_WITH_KNOTS ( 'NONE', 3,
 ( #54341, #70561, #99990, #60957, #61459, #91916, #23958, #99490, #85839, #38663, #69566, #9275, #173, #31057, #92898, #8275, #47260, #78181, #84806, #8770, #76674, #22471, #14862, #53365, #84315, #45749, #92409, #39639, #15346, #32052, #62964, #77692, #78686, #7261, #38144, #85313, #15859, #93914, #22957, #39140, #46766, #668, #86325, #16862, #53846, #46242 ),
 .UNSPECIFIED., .F., .F.,
 ( 4, 2, 2, 2, 2, 2, 2, 2, 2, 2, 2, 2, 2, 2, 2, 2, 2, 2, 2, 2, 2, 2, 4 ),
 ( 0.002366943055100816529, 0.002788261558867141145, 0.002998920810750290225, 0.003104250436691864332, 0.003209580062633438872, 0.003314909688575013412, 0.003420239314516587952, 0.003630898566399730527, 0.004052217070165960167, 0.004894854077698489701, 0.005737491085231020971, 0.006580128092763551373, 0.007001446596529816574, 0.007422765100296080040, 0.007528094726237586493, 0.007580759539208290279, 0.007633424352178995800, 0.007686089165149699587, 0.007738753978120403373, 0.007844083604061628801, 0.008265402107826599898, 0.008686720611591570995, 0.009108039115356540358 ),
 .UNSPECIFIED. ) ;
#18997 = CARTESIAN_POINT ( 'NONE',  ( 68.82519319127361257, 64.71339118656145217, -12.18766638205895347 ) ) ;
#18998 = CARTESIAN_POINT ( 'NONE',  ( 199.0773057068961123, 285.8349872121713702, -17.17316764978006560 ) ) ;
#18999 = CARTESIAN_POINT ( 'NONE',  ( 79.90666100684894957, 48.61584110152371352, 14.44201039220772564 ) ) ;
#19000 = CARTESIAN_POINT ( 'NONE',  ( 192.8607783413999073, 296.6023284558532396, -11.80574095728561446 ) ) ;
#19001 = DIRECTION ( 'NONE',  ( 0.000000000000000000, -1.000000000000000000, 0.000000000000000000 ) ) ;
#19002 = CARTESIAN_POINT ( 'NONE',  ( 164.1224127655298730, 246.3786377597482158, 7.356982420601481998 ) ) ;
#19003 = CARTESIAN_POINT ( 'NONE',  ( 191.6823192895500370, 298.6434794082964572, -8.424208857102787107 ) ) ;
#19004 = CARTESIAN_POINT ( 'NONE',  ( 164.4440639631384045, 245.8215215431751233, -2.910115319305802029 ) ) ;
#19005 = ORIENTED_EDGE ( 'NONE', *, *, #68461, .T. ) ;
#19007 = EDGE_CURVE ( 'NONE', #64907, #86118, #43618, .T. ) ;
#19006 = B_SPLINE_CURVE_WITH_KNOTS ( 'NONE', 3,
 ( #29740, #62613, #22641, #60614 ),
 .UNSPECIFIED., .F., .F.,
 ( 4, 4 ),
 ( 2.422837424025932118E-15, 0.002968769119667788274 ),
 .UNSPECIFIED. ) ;
#19008 = CARTESIAN_POINT ( 'NONE',  ( 208.0692320075777957, 270.2605140014760536, 2.043861372130216569 ) ) ;
#19009 = CARTESIAN_POINT ( 'NONE',  ( -1.637757109730603178, 179.8615022471903444, 5.000000000000046185 ) ) ;
#19010 = CARTESIAN_POINT ( 'NONE',  ( 83.19757352214881507, 43.20952170335151266, 8.047085336822298984 ) ) ;
#19011 = CARTESIAN_POINT ( 'NONE',  ( 125.2075541532825014, 255.3464784336661353, 1.353441290958777327E-15 ) ) ;
#19012 = CARTESIAN_POINT ( 'NONE',  ( 17.84595736030643920, 25.70171378149918340, -9.188101187500004485 ) ) ;
#19013 = CARTESIAN_POINT ( 'NONE',  ( 77.76098460965452830, 59.25386675525071922, -16.47652547104713250 ) ) ;
#19014 = CARTESIAN_POINT ( 'NONE',  ( 37.53185021205516847, 199.1427522451419065, 10.00000000000009415 ) ) ;
#19016 = CARTESIAN_POINT ( 'NONE',  ( 185.7458139929641732, 288.0803647735083928, 14.78940038638959997 ) ) ;
#19015 = CARTESIAN_POINT ( 'NONE',  ( 81.95854183835243134, 41.81427719307645674, -5.625612379983921052 ) ) ;
#19017 = EDGE_CURVE ( 'NONE', #76847, #17199, #59812, .T. ) ;
#19018 = CARTESIAN_POINT ( 'NONE',  ( 18.77112655976752009, 19.03677371833801502, 10.00000000000000533 ) ) ;
#19019 = EDGE_LOOP ( 'NONE', ( #44398, #59248, #74250, #59499 ) ) ;
#19020 = CARTESIAN_POINT ( 'NONE',  ( 193.9979983253333842, 262.2552985615510579, -0.8131695963413709816 ) ) ;
#19021 = CARTESIAN_POINT ( 'NONE',  ( 149.3801359649374092, 271.9130101976182914, -11.41245530317637424 ) ) ;
#19022 = VECTOR ( 'NONE', #30182, 999.9999999999998863 ) ;
#19023 = DIRECTION ( 'NONE',  ( -0.3077152132536331575, -0.9514785060800222682, 0.000000000000000000 ) ) ;
#19024 = CARTESIAN_POINT ( 'NONE',  ( 173.2640678248423569, 289.7688146612205742, -1.079593490584200177 ) ) ;
#19025 = CARTESIAN_POINT ( 'NONE',  ( 81.42054145595460568, 55.42004525696071937, -16.32184955832448381 ) ) ;
#19026 = ORIENTED_EDGE ( 'NONE', *, *, #54057, .T. ) ;
#19027 = CARTESIAN_POINT ( 'NONE',  ( 76.08964319905662421, 64.37085305084526965, -14.90483801509815542 ) ) ;
#19028 = CARTESIAN_POINT ( 'NONE',  ( 168.9077028164640240, 271.8916309642168585, -16.88789700254694992 ) ) ;
#19029 = EDGE_CURVE ( 'NONE', #87101, #32335, #67925, .T. ) ;
#19030 = B_SPLINE_SURFACE_WITH_KNOTS ( 'NONE', 3, 1, ( 
 ( #56007, #31709 ),
 ( #17023, #25647 ),
 ( #1846, #26143 ),
 ( #47425, #39800 ),
 ( #95083, #94569 ),
 ( #56529, #48438 ),
 ( #62614, #25126 ),
 ( #2864, #33754 ),
 ( #73740, #59000 ),
 ( #49934, #98044 ),
 ( #11463, #42319 ),
 ( #42807, #65133 ),
 ( #10953, #82388 ),
 ( #65626, #66628 ),
 ( #5337, #26640 ),
 ( #66131, #4850 ),
 ( #72771, #89015 ),
 ( #88002, #19060 ),
 ( #80383, #96583 ),
 ( #80895, #73248 ),
 ( #12448, #3842 ),
 ( #81382, #3364 ),
 ( #35229, #50921 ),
 ( #88498, #12957 ),
 ( #49430, #27147 ),
 ( #34727, #41824 ),
 ( #51425, #43316 ),
 ( #58032, #19566 ),
 ( #28622, #50425 ),
 ( #4331, #43819 ),
 ( #74757, #36218 ),
 ( #97559, #81871 ),
 ( #97080, #11949 ),
 ( #67120, #27650 ) ),
 .UNSPECIFIED., .T., .F., .F.,
 ( 4, 2, 2, 2, 2, 2, 2, 2, 2, 2, 2, 2, 2, 2, 2, 2, 4 ),
 ( 2, 2 ),
 ( 0.000000000000000000, 0.06250000000000000000, 0.1250000000000000000, 0.1875000000000000000, 0.2500000000000000000, 0.3125000000000000000, 0.3750000000000000000, 0.4375000000000000000, 0.5000000000000000000, 0.5625000000000000000, 0.6250000000000000000, 0.6875000000000000000, 0.7500000000000000000, 0.8125000000000000000, 0.8750000000000000000, 0.9375000000000000000, 1.000000000000000000 ),
 ( 0.000000000000000000, 1.000000000000000000 ),
 .UNSPECIFIED. ) ;
#19031 = CARTESIAN_POINT ( 'NONE',  ( 77.53799973678586355, 49.68283126470399225, 14.93564267158908443 ) ) ;
#19032 = CARTESIAN_POINT ( 'NONE',  ( 196.5114978539924095, 270.9775588704130769, 12.02747001956845985 ) ) ;
#19033 = CARTESIAN_POINT ( 'NONE',  ( 156.5453005749562294, 261.0928181209063155, 17.61606195476766956 ) ) ;
#19034 = DIRECTION ( 'NONE',  ( 0.000000000000000000, -0.6788029332000657945, 0.7343204871709537729 ) ) ;
#19035 = CARTESIAN_POINT ( 'NONE',  ( 192.7693357657653053, 296.7607116428271183, 12.22606306887835714 ) ) ;
#19036 =( GEOMETRIC_REPRESENTATION_CONTEXT ( 3 ) GLOBAL_UNCERTAINTY_ASSIGNED_CONTEXT ( ( #8850 ) ) GLOBAL_UNIT_ASSIGNED_CONTEXT ( ( #27316, #62931, #40116 ) ) REPRESENTATION_CONTEXT ( 'NONE', 'WORKASPACE' ) );
#19037 = ORIENTED_EDGE ( 'NONE', *, *, #67320, .F. ) ;
#19038 = CARTESIAN_POINT ( 'NONE',  ( 194.5559179531667553, 283.0183282092541504, 17.56514686992159469 ) ) ;
#19039 = CARTESIAN_POINT ( 'NONE',  ( 9.015913755055775525, 20.90829794293878763, 10.00000000000000355 ) ) ;
#19040 = CARTESIAN_POINT ( 'NONE',  ( 173.7983950520408882, 272.6079108873909149, -16.38292534526199518 ) ) ;
#19041 = ORIENTED_EDGE ( 'NONE', *, *, #38510, .F. ) ;
#19042 = CARTESIAN_POINT ( 'NONE',  ( 163.8626652770474266, 279.3816800765269477, 12.16740215884250631 ) ) ;
#19043 = CARTESIAN_POINT ( 'NONE',  ( 194.6782745185928434, 293.4543327343926080, -14.56555309295305634 ) ) ;
#19044 = CARTESIAN_POINT ( 'NONE',  ( 159.5606259118165724, 264.0648208006689401, -17.79391822139266566 ) ) ;
#19045 = ORIENTED_EDGE ( 'NONE', *, *, #12881, .F. ) ;
#19046 = CARTESIAN_POINT ( 'NONE',  ( 79.19335676987149952, 59.81345803429233143, 16.50342877771833017 ) ) ;
#19047 = CARTESIAN_POINT ( 'NONE',  ( 185.3238942230333919, 291.2129889426717568, 12.00891028115657555 ) ) ;
#19048 = CARTESIAN_POINT ( 'NONE',  ( 93.96857342517719758, -8.000000000000000000, 0.000000000000000000 ) ) ;
#19049 = ORIENTED_EDGE ( 'NONE', *, *, #91374, .F. ) ;
#19050 = CARTESIAN_POINT ( 'NONE',  ( 77.51795247811750755, 52.17589778563348801, -15.67370978287279470 ) ) ;
#19051 = AXIS2_PLACEMENT_3D ( 'NONE', #1473, #78991, #9576 ) ;
#19052 = CARTESIAN_POINT ( 'NONE',  ( 185.0431258460432957, 259.9412888983961238, -5.848330788044057371 ) ) ;
#19053 = ORIENTED_EDGE ( 'NONE', *, *, #80391, .T. ) ;
#19054 = ORIENTED_EDGE ( 'NONE', *, *, #51709, .T. ) ;
#19055 = CARTESIAN_POINT ( 'NONE',  ( 178.4748507201557004, 260.9579597201419006, 12.09575687999501881 ) ) ;
#19056 = ORIENTED_EDGE ( 'NONE', *, *, #7187, .T. ) ;
#19057 = CARTESIAN_POINT ( 'NONE',  ( 77.23008513726504987, 49.48297111420801286, 14.92774319911447733 ) ) ;
#19058 = ORIENTED_EDGE ( 'NONE', *, *, #98274, .T. ) ;
#19059 = CARTESIAN_POINT ( 'NONE',  ( 74.81619755463081844, 57.89461443497145154, 15.97444856423281934 ) ) ;
#19060 = CARTESIAN_POINT ( 'NONE',  ( 154.9792334219179679, 262.2150889255981951, -17.21325849938693153 ) ) ;
#19061 = ORIENTED_EDGE ( 'NONE', *, *, #42251, .T. ) ;
#19062 = CIRCLE ( 'NONE', #43319, 0.1418229129680845801 ) ;
#19063 = CARTESIAN_POINT ( 'NONE',  ( 82.31202062023011479, 40.66771258265164590, 3.246634729999704483 ) ) ;
#19064 = CARTESIAN_POINT ( 'NONE',  ( 189.9926605375425481, 301.5700542142271843, 2.240758812287489743 ) ) ;
#19065 = CARTESIAN_POINT ( 'NONE',  ( 161.6007233961445309, 277.4982682042578404, -13.28202216465472674 ) ) ;
#19066 = CARTESIAN_POINT ( 'NONE',  ( 147.5749551500760788, 275.0396750858066639, -4.254929048021584670 ) ) ;
#19068 = ADVANCED_FACE ( 'NONE', ( #28417 ), #59297, .F. ) ;
#19067 = CARTESIAN_POINT ( 'NONE',  ( 153.4613150239306094, 264.8442007126561748, -16.86932470306368259 ) ) ;
#19069 = DIRECTION ( 'NONE',  ( -0.8868092729070087277, -0.4621356007560363244, 0.000000000000000000 ) ) ;
#19070 = CARTESIAN_POINT ( 'NONE',  ( 71.38870771651419034, 68.37070112333339011, -9.453314934521086954 ) ) ;
#19071 = CARTESIAN_POINT ( 'NONE',  ( 141.9874905431360332, 240.5327760586659451, 1.948934522072303157E-15 ) ) ;
#19072 = ORIENTED_EDGE ( 'NONE', *, *, #26316, .T. ) ;
#19073 = CARTESIAN_POINT ( 'NONE',  ( 70.55696984825441120, 61.37392526597871267, -14.80549934020668701 ) ) ;
#19074 = CARTESIAN_POINT ( 'NONE',  ( 10.54248283575963008, 11.80170272979924206, 7.433330006724137462 ) ) ;
#19075 = ORIENTED_EDGE ( 'NONE', *, *, #23167, .T. ) ;
#19077 = ORIENTED_EDGE ( 'NONE', *, *, #64872, .T. ) ;
#19076 = CARTESIAN_POINT ( 'NONE',  ( 203.8368721788344544, 271.7098658965333584, 9.656807015386196014 ) ) ;
#19078 = CARTESIAN_POINT ( 'NONE',  ( -5.238238056892285499, 179.3297689869269504, -2.679491924311240503 ) ) ;
#19079 = CARTESIAN_POINT ( 'NONE',  ( 78.17464201438049543, 47.84695061245597003, -14.00636085769150974 ) ) ;
#19080 = CARTESIAN_POINT ( 'NONE',  ( 170.9867886428140196, 287.8958644575130279, -5.368964696424015415 ) ) ;
#19081 = CARTESIAN_POINT ( 'NONE',  ( 152.8260228566844603, 277.7352812325914329, 6.769763962897619614 ) ) ;
#19082 = CARTESIAN_POINT ( 'NONE',  ( 78.50967049263377362, 51.05820285709072692, -15.70993305931173545 ) ) ;
#19083 = CARTESIAN_POINT ( 'NONE',  ( 178.6026051973306323, 254.4708812555809345, 5.813106864979912913 ) ) ;
#19084 = CARTESIAN_POINT ( 'NONE',  ( 87.51937303406259616, 45.11776172068187662, 6.154781583138794865 ) ) ;
#19085 = CARTESIAN_POINT ( 'NONE',  ( 88.13797031347935729, 44.16014372656159281, -1.732870377860791677 ) ) ;
#19086 = ORIENTED_EDGE ( 'NONE', *, *, #26286, .T. ) ;
#19087 = CARTESIAN_POINT ( 'NONE',  ( 185.0052077488253417, 273.1271762488819377, -16.58638918698247977 ) ) ;
#19088 = CARTESIAN_POINT ( 'NONE',  ( 66.10733050139633349, 69.29219150952910411, 0.2566142034190574961 ) ) ;
#19089 = ORIENTED_EDGE ( 'NONE', *, *, #73337, .F. ) ;
#19090 = AXIS2_PLACEMENT_3D ( 'NONE', #92523, #14973, #77807 ) ;
#19091 = CARTESIAN_POINT ( 'NONE',  ( 164.0768433133964095, 278.1026867120588122, 13.25608502235604647 ) ) ;
#19092 = DIRECTION ( 'NONE',  ( -0.000000000000000000, -0.000000000000000000, -1.000000000000000000 ) ) ;
#19093 = CARTESIAN_POINT ( 'NONE',  ( 164.1339789967515514, 246.3586044596203521, -8.192084292517387567 ) ) ;
#19094 = CARTESIAN_POINT ( 'NONE',  ( 149.2561433752359505, 272.1277716627430436, 12.99353668144589946 ) ) ;
#19095 = AXIS2_PLACEMENT_3D ( 'NONE', #28776, #82022, #3981 ) ;
#19096 = CARTESIAN_POINT ( 'NONE',  ( 202.2712651538608668, 280.3028871727136675, 16.13191389836473988 ) ) ;
#19098 = FACE_OUTER_BOUND ( 'NONE', #73377, .T. ) ;
#19097 = CARTESIAN_POINT ( 'NONE',  ( 161.4345289443906779, 281.4097987515496015, -6.805021284559834349 ) ) ;
#19099 = DIRECTION ( 'NONE',  ( -0.8660254037844387076, -0.4999999999999998890, -0.000000000000000000 ) ) ;
#19100 = ORIENTED_EDGE ( 'NONE', *, *, #46651, .F. ) ;
#19101 = VECTOR ( 'NONE', #86593, 1000.000000000000114 ) ;
#19102 = CARTESIAN_POINT ( 'NONE',  ( 74.62258251110877438, 61.63511669430710782, -15.13440849647893494 ) ) ;
#19103 = CARTESIAN_POINT ( 'NONE',  ( 79.94597790610303889, 58.10291136569557580, 16.26832645005858424 ) ) ;
#19104 = EDGE_CURVE ( 'NONE', #20250, #75378, #56204, .T. ) ;
#19105 = CARTESIAN_POINT ( 'NONE',  ( -59.65739779450132829, 37.15562860896454112, -10.00000000000000000 ) ) ;
#19106 = CARTESIAN_POINT ( 'NONE',  ( 153.4289928607825573, 264.9001843414388873, 17.27358709529985958 ) ) ;
#19107 = EDGE_CURVE ( 'NONE', #12543, #82272, #29425, .T. ) ;
#19108 = AXIS2_PLACEMENT_3D ( 'NONE', #6513, #29803, #36394 ) ;
#19109 = CARTESIAN_POINT ( 'NONE',  ( 80.87154830239147429, 43.64994579682081621, -9.570501097346140185 ) ) ;
#19110 = CARTESIAN_POINT ( 'NONE',  ( 192.4240881988952196, 286.9807864659827032, 17.27280571159278466 ) ) ;
#19111 = CARTESIAN_POINT ( 'NONE',  ( -14.45063460946529155, 102.6502293776574390, 44.23345500514351869 ) ) ;
#19112 = CARTESIAN_POINT ( 'NONE',  ( 10.35128207213630169, 176.7833772461660544, -9.188101187500095079 ) ) ;
#19113 = CARTESIAN_POINT ( 'NONE',  ( 106.1553423657898492, 232.0958772461660260, -9.188101187500095079 ) ) ;
#19114 = CARTESIAN_POINT ( 'NONE',  ( 203.3205561747472814, 278.4854618126124706, -15.14439614831292147 ) ) ;
#19115 = CARTESIAN_POINT ( 'NONE',  ( 88.00064672366042373, 44.55878435733892928, -4.022439529268951652 ) ) ;
#19116 = CARTESIAN_POINT ( 'NONE',  ( 186.6044737300459246, 296.1965008795603467, -7.321969523639923594 ) ) ;
#19117 = CARTESIAN_POINT ( 'NONE',  ( 81.04961468568201610, 43.68546784643918812, -9.492462169003031747 ) ) ;
#19118 = VECTOR ( 'NONE', #23978, 1000.000000000000000 ) ;
#19119 = CARTESIAN_POINT ( 'NONE',  ( 82.44310520575160695, 54.28011738120410001, -15.96781897959229113 ) ) ;
#19120 = CARTESIAN_POINT ( 'NONE',  ( 172.4746793654577743, 290.6488618360747864, 2.762989037780315904 ) ) ;
#19121 = CARTESIAN_POINT ( 'NONE',  ( -110.0000000000000142, 15.00000000000000000, 9.212605237762145904 ) ) ;
#19122 = CARTESIAN_POINT ( 'NONE',  ( 148.1829914015846157, 273.9865254053503349, -9.304102644963160529 ) ) ;
#19123 = CARTESIAN_POINT ( 'NONE',  ( 181.6983192186336566, 291.5179062160608510, 9.337665102737071621 ) ) ;
#19124 = CARTESIAN_POINT ( 'NONE',  ( 178.0782606409264304, 276.0678601331425739, -17.70468353419743579 ) ) ;
#19125 = CARTESIAN_POINT ( 'NONE',  ( 205.5005536374337112, 274.7095954468686045, -13.54891840104049194 ) ) ;
#19126 = CARTESIAN_POINT ( 'NONE',  ( -0.9341114727036623488, 180.2677522451419350, -5.000000000000047962 ) ) ;
#19127 = CARTESIAN_POINT ( 'NONE',  ( 74.33436806272575836, 56.35182720436719706, -16.09600543955971830 ) ) ;
#19128 = DIRECTION ( 'NONE',  ( -0.4999999999999987232, 0.8660254037844394848, 0.000000000000000000 ) ) ;
#19129 = EDGE_CURVE ( 'NONE', #31218, #65623, #68910, .T. ) ;
#19130 = B_SPLINE_CURVE_WITH_KNOTS ( 'NONE', 3,
 ( #59461, #14390, #66592, #59967 ),
 .UNSPECIFIED., .F., .F.,
 ( 4, 4 ),
 ( 0.01142038051278651892, 0.01737621679390735294 ),
 .UNSPECIFIED. ) ;
#19131 = CARTESIAN_POINT ( 'NONE',  ( 175.6683667130938034, 265.4573993361621547, -15.76779689782518368 ) ) ;
#19132 = CARTESIAN_POINT ( 'NONE',  ( 82.58295308470839302, 227.6744531367911293, 4.594050593750047540 ) ) ;
#19133 = CARTESIAN_POINT ( 'NONE',  ( 161.8668411317136986, 250.2854024296290447, -13.43522912998426655 ) ) ;
#19134 = CARTESIAN_POINT ( 'NONE',  ( 72.81050907550364570, 57.13790140118627647, 15.89804358815998953 ) ) ;
#19135 = PLANE ( 'NONE',  #98371 ) ;
#19137 = CARTESIAN_POINT ( 'NONE',  ( 151.7315266105576939, 267.8402821309618957, 15.96020185843874373 ) ) ;
#19136 = CARTESIAN_POINT ( 'NONE',  ( 42.16454434324482747, 125.9067112960471349, -10.00000000000000000 ) ) ;
#19138 = FACE_OUTER_BOUND ( 'NONE', #81135, .T. ) ;
#19139 = CARTESIAN_POINT ( 'NONE',  ( 176.7306370342185460, 270.1477411634788268, -17.15222723775526603 ) ) ;
#19140 = CARTESIAN_POINT ( 'NONE',  ( 36.41017387241338099, 23.94754757982092030, 5.678558825948272215 ) ) ;
#19141 = DIRECTION ( 'NONE',  ( -0.9292718480896806632, -0.3693965786901518555, 0.000000000000000000 ) ) ;
#19142 = CARTESIAN_POINT ( 'NONE',  ( 75.26996855991060897, 59.55077116385917435, 16.22776523571817364 ) ) ;
#19143 = ORIENTED_EDGE ( 'NONE', *, *, #62394, .T. ) ;
#19144 = CARTESIAN_POINT ( 'NONE',  ( 20.65814732634927609, 20.43085787977763346, -9.188101187500008038 ) ) ;
#19145 = CARTESIAN_POINT ( 'NONE',  ( 77.41429782557628414, 209.3768266524159571, -9.188101187500093303 ) ) ;
#19146 = DIRECTION ( 'NONE',  ( -0.8660254037844387076, -0.4999999999999998890, -0.000000000000000000 ) ) ;
#19147 = CARTESIAN_POINT ( 'NONE',  ( -30.24407882362163846, 94.12867598954146331, 12.26304263616266077 ) ) ;
#19148 = CARTESIAN_POINT ( 'NONE',  ( 191.4405189358380426, 288.5485936597882528, -15.93201744756964722 ) ) ;
#19149 =( BOUNDED_CURVE ( )  B_SPLINE_CURVE ( 2, ( #3997, #73660, #40730, #95515, #48865, #86911, #80293, #87923, #26561 ),
 .UNSPECIFIED., .F., .T. ) 
 B_SPLINE_CURVE_WITH_KNOTS ( ( 3, 2, 2, 2, 3 ),
 ( 0.6653225806451612545, 0.6666666666666666297, 0.6693548387096773800, 0.6720430107526881303, 0.6733870967741935054 ),
 .UNSPECIFIED. ) 
 CURVE ( )  GEOMETRIC_REPRESENTATION_ITEM ( )  RATIONAL_B_SPLINE_CURVE ( ( 0.9330127018922194093, 0.9330127018922194093, 1.000000000000000000, 0.8660254037844387076, 1.000000000000000000, 0.8660254037844387076, 1.000000000000000000, 0.9330127018922194093, 0.9330127018922194093 ) ) 
 REPRESENTATION_ITEM ( '' )  );
#19150 = CARTESIAN_POINT ( 'NONE',  ( 86.35455787144825024, 47.24910468700996091, 10.80869237663237570 ) ) ;
#19151 = LINE ( 'NONE', #17118, #7276 ) ;
#19152 = DIRECTION ( 'NONE',  ( -0.8653701635463872943, 0.5011331959107268030, 0.000000000000000000 ) ) ;
#19153 = CARTESIAN_POINT ( 'NONE',  ( 122.1317068477954422, 247.9865022471903160, 10.00000000000009237 ) ) ;
#19154 = CARTESIAN_POINT ( 'NONE',  ( 13.51768745649706993, 188.6115022471903160, -5.000000000000047962 ) ) ;
#19155 = CARTESIAN_POINT ( 'NONE',  ( 75.07675898528307812, 53.26063823009506848, 16.03352913183455186 ) ) ;
#19156 = ORIENTED_EDGE ( 'NONE', *, *, #15079, .F. ) ;
#19157 = AXIS2_PLACEMENT_3D ( 'NONE', #90802, #9666, #62319 ) ;
#19158 = CARTESIAN_POINT ( 'NONE',  ( 165.5769259146263437, 246.9434120422340868, -1.858383500763620910 ) ) ;
#19159 = ORIENTED_EDGE ( 'NONE', *, *, #37993, .T. ) ;
#19160 = CARTESIAN_POINT ( 'NONE',  ( 162.9466247808429102, 248.4151622881552441, 11.25765811906727443 ) ) ;
#19161 = LINE ( 'NONE', #9555, #51387 ) ;
#19162 = CARTESIAN_POINT ( 'NONE',  ( 73.62962662361488242, 68.62763621100698685, -10.64167080051653613 ) ) ;
#19163 = ORIENTED_EDGE ( 'NONE', *, *, #77798, .T. ) ;
#19164 = CARTESIAN_POINT ( 'NONE',  ( 77.00910850481051284, 63.69207575539577704, -14.97815254220547487 ) ) ;
#19165 = ORIENTED_EDGE ( 'NONE', *, *, #41229, .T. ) ;
#19166 = VECTOR ( 'NONE', #19513, 1000.000000000000000 ) ;
#19167 = CARTESIAN_POINT ( 'NONE',  ( 189.0455566057698604, 290.5252480108450186, 14.38176501911003236 ) ) ;
#19168 = CARTESIAN_POINT ( 'NONE',  ( 170.1131776778324820, 289.4493487920391317, 2.171624877603286485 ) ) ;
#19169 = CARTESIAN_POINT ( 'NONE',  ( 194.0402169394646137, 280.7468621445926829, -17.21104619501045363 ) ) ;
#19170 = CARTESIAN_POINT ( 'NONE',  ( 191.8781672928813293, 296.7077321713139213, -11.78931491291747768 ) ) ;
#19172 = EDGE_CURVE ( 'NONE', #78746, #57975, #44107, .T. ) ;
#19171 = CIRCLE ( 'NONE', #46594, 0.1418229129680828593 ) ;
#19173 = CARTESIAN_POINT ( 'NONE',  ( 111.8115707860309556, 225.3615022471902023, 5.000000000000051514 ) ) ;
#19174 = VECTOR ( 'NONE', #57040, 1000.000000000000114 ) ;
#19175 = CARTESIAN_POINT ( 'NONE',  ( 36.52324494929276710, 26.80170272979929180, 7.433330006724137462 ) ) ;
#19176 = CARTESIAN_POINT ( 'NONE',  ( 79.61341344889541460, 58.26341340635389798, -16.23793971862889407 ) ) ;
#19177 = CARTESIAN_POINT ( 'NONE',  ( 164.2085977011741988, 275.1762843307250819, 14.84329694928079491 ) ) ;
#19178 = CARTESIAN_POINT ( 'NONE',  ( 186.0348036264326481, 259.0250182415348945, 6.435743254585703177 ) ) ;
#19179 = VERTEX_POINT ( 'NONE', #76050 ) ;
#19180 = VERTEX_POINT ( 'NONE', #68414 ) ;
#19181 = CARTESIAN_POINT ( 'NONE',  ( 185.2974406820879096, 297.2943441938441538, 1.030251969549985880 ) ) ;
#19182 = VECTOR ( 'NONE', #30493, 1000.000000000000114 ) ;
#19184 = CARTESIAN_POINT ( 'NONE',  ( 194.3541845315608612, 294.0156730581561533, -14.67567721756631016 ) ) ;
#19183 = CARTESIAN_POINT ( 'NONE',  ( 204.2556901454867955, 276.8657622634082713, 13.61111001399713949 ) ) ;
#19185 = CARTESIAN_POINT ( 'NONE',  ( 85.76278670188220588, 48.57154102325930012, -11.82477194771139928 ) ) ;
#19186 = CARTESIAN_POINT ( 'NONE',  ( -22.42236680055709641, 157.8615022471902591, 0.000000000000000000 ) ) ;
#19187 = DIRECTION ( 'NONE',  ( 0.8495546651763555834, 0.5275005885087621360, 0.000000000000000000 ) ) ;
#19188 = CARTESIAN_POINT ( 'NONE',  ( 157.6921299354026189, 257.5162143285667753, -18.18720974599499840 ) ) ;
#19189 = CARTESIAN_POINT ( 'NONE',  ( 208.0925911829191932, 270.2200547229618337, -3.965170738876734546 ) ) ;
#19190 = CARTESIAN_POINT ( 'NONE',  ( 191.8986733338516331, 296.2687432111309249, 12.49828825629462337 ) ) ;
#19191 = AXIS2_PLACEMENT_3D ( 'NONE', #93966, #71650, #39688 ) ;
#19192 = CARTESIAN_POINT ( 'NONE',  ( 181.4842875826702482, 256.0790464748339446, 5.242542569475632241 ) ) ;
#19193 = CARTESIAN_POINT ( 'NONE',  ( 100.9591899430832029, 229.0958772461660260, -9.188101187500095079 ) ) ;
#19194 = VERTEX_POINT ( 'NONE', #5622 ) ;
#19195 = FACE_OUTER_BOUND ( 'NONE', #9294, .T. ) ;
#19196 = CARTESIAN_POINT ( 'NONE',  ( 118.5773942495489592, 229.2677522451417929, -5.000000000000041744 ) ) ;
#19197 = EDGE_LOOP ( 'NONE', ( #29621, #27145, #92956, #16808 ) ) ;
#19198 = B_SPLINE_CURVE_WITH_KNOTS ( 'NONE', 3,
 ( #59192, #90168, #36914, #29329, #83562, #20741, #38906, #45505, #93658, #60694, #53604, #61703, #47018, #92655, #30321, #99734 ),
 .UNSPECIFIED., .F., .F.,
 ( 4, 2, 2, 2, 2, 2, 2, 4 ),
 ( 0.000000000000000000, 0.0003786681000626416311, 0.0007573362001252832622, 0.001136004300187924785, 0.001514672400250566524, 0.001893340500313208264, 0.002272008600375849570, 0.003029344800501268357 ),
 .UNSPECIFIED. ) ;
#19199 = VERTEX_POINT ( 'NONE', #29921 ) ;
#19200 = CARTESIAN_POINT ( 'NONE',  ( 86.97241420434123427, 45.90339759676925979, -8.144416502837579230 ) ) ;
#19201 = CARTESIAN_POINT ( 'NONE',  ( 176.8376293082206701, 292.8516012225593386, -2.786154410470390363 ) ) ;
#19202 = CARTESIAN_POINT ( 'NONE',  ( 85.01702307733869191, 42.37204648715616173, -0.3572300862006242972 ) ) ;
#19203 = CARTESIAN_POINT ( 'NONE',  ( 159.9997000813754084, 253.5193855937126841, -16.28798248637880519 ) ) ;
#19204 = CARTESIAN_POINT ( 'NONE',  ( -52.66218383418999593, 96.92811335557053098, -10.00000000000000000 ) ) ;
#19205 = CARTESIAN_POINT ( 'NONE',  ( 96.60225995211651195, 217.3923013555410080, 4.594050593750050204 ) ) ;
#19206 = ORIENTED_EDGE ( 'NONE', *, *, #85123, .F. ) ;
#19207 = VECTOR ( 'NONE', #10052, 1000.000000000000000 ) ;
#19208 = ORIENTED_EDGE ( 'NONE', *, *, #97598, .F. ) ;
#19209 = CARTESIAN_POINT ( 'NONE',  ( 48.95103868752454446, 97.61288834769685252, -10.00000000000000000 ) ) ;
#19210 = ORIENTED_EDGE ( 'NONE', *, *, #33379, .T. ) ;
#19211 = CARTESIAN_POINT ( 'NONE',  ( 192.4325953160755773, 264.9157042485226725, -7.801807992731872865 ) ) ;
#19212 = CARTESIAN_POINT ( 'NONE',  ( 18.71383987920374992, 181.6115022471902591, 10.00000000000009592 ) ) ;
#19213 = AXIS2_PLACEMENT_3D ( 'NONE', #5013, #44480, #21210 ) ;
#19214 = CARTESIAN_POINT ( 'NONE',  ( 72.50310743999735053, 69.30443315113288349, -9.159185671101845116 ) ) ;
#19216 = CARTESIAN_POINT ( 'NONE',  ( 69.56331254061269931, 63.09499020812631187, -13.61442372004802159 ) ) ;
#19215 = CARTESIAN_POINT ( 'NONE',  ( 136.8177939967088435, 258.9869531367911009, 4.594050593750046652 ) ) ;
#19217 = CARTESIAN_POINT ( 'NONE',  ( -52.70992191624042533, 89.63437584143055403, -10.00000000000000000 ) ) ;
#19218 = CARTESIAN_POINT ( 'NONE',  ( 166.8083734521890449, 257.5796782931630560, -15.79284703031436798 ) ) ;
#19219 = ORIENTED_EDGE ( 'NONE', *, *, #75468, .F. ) ;
#19220 = CARTESIAN_POINT ( 'NONE',  ( 156.7854950622006527, 259.0865519928661911, 18.17819951099994213 ) ) ;
#19221 = CARTESIAN_POINT ( 'NONE',  ( 160.5517938760779089, 275.6377758284635888, 12.83436562505768741 ) ) ;
#19222 = CARTESIAN_POINT ( 'NONE',  ( 81.95468535755843220, 40.99502387196763920, -3.139656615793550820 ) ) ;
#19223 = CARTESIAN_POINT ( 'NONE',  ( 189.7737856813211579, 269.7866060870444471, 15.20194579022378889 ) ) ;
#19224 = LINE ( 'NONE', #44470, #57668 ) ;
#19225 = EDGE_CURVE ( 'NONE', #10682, #87650, #67417, .T. ) ;
#19226 = LINE ( 'NONE', #88160, #36845 ) ;
#19227 = FACE_OUTER_BOUND ( 'NONE', #9613, .T. ) ;
#19228 = EDGE_CURVE ( 'NONE', #1361, #33352, #7616, .T. ) ;
#19229 = LINE ( 'NONE', #73412, #26889 ) ;
#19230 = CARTESIAN_POINT ( 'NONE',  ( 153.6596595523362794, 266.9882342533689439, 16.60685250298524807 ) ) ;
#19231 = CARTESIAN_POINT ( 'NONE',  ( 206.7596416265183734, 271.4678399409689291, 6.202658291405857227 ) ) ;
#19232 = EDGE_CURVE ( 'NONE', #87618, #96856, #63056, .T. ) ;
#19233 = CARTESIAN_POINT ( 'NONE',  ( 206.8775514429320026, 272.3245652858344670, -9.838455694836268250 ) ) ;
#19234 = CARTESIAN_POINT ( 'NONE',  ( 78.05395834205243943, 61.78695400133908322, 16.08488452160743520 ) ) ;
#19235 = CARTESIAN_POINT ( 'NONE',  ( 162.8223739550644211, 248.6303710312858186, -11.16939803179192658 ) ) ;
#19236 = DIRECTION ( 'NONE',  ( -1.000000000000000000, 0.000000000000000000, 0.000000000000000000 ) ) ;
#19237 = EDGE_CURVE ( 'NONE', #11090, #68611, #69419, .T. ) ;
#19238 = CARTESIAN_POINT ( 'NONE',  ( 27.37348498259797935, 38.73705186507756082, -3.090169943749475845 ) ) ;
#19239 = AXIS2_PLACEMENT_3D ( 'NONE', #86622, #72388, #1479 ) ;
#19240 = VECTOR ( 'NONE', #80991, 1000.000000000000000 ) ;
#19241 = CARTESIAN_POINT ( 'NONE',  ( 70.36206151952180221, 64.89165491571560551, -12.13793269121529939 ) ) ;
#19244 = CARTESIAN_POINT ( 'NONE',  ( 74.28989463527457815, 55.24825063735668351, 16.60343178153034316 ) ) ;
#19243 = B_SPLINE_CURVE_WITH_KNOTS ( 'NONE', 3,
 ( #25909, #87764, #3605, #42081, #18303, #63387, #49201, #72518, #82133, #50670, #66871, #4081 ),
 .UNSPECIFIED., .F., .F.,
 ( 4, 2, 2, 2, 2, 4 ),
 ( 0.001172129118361127592, 0.001404330768412652593, 0.001636532418464177593, 0.002100935718567244724, 0.002565339018670311638, 0.003029742318773378552 ),
 .UNSPECIFIED. ) ;
#19242 = CARTESIAN_POINT ( 'NONE',  ( 177.5616848261300902, 264.8410986875884419, -15.15881583357887585 ) ) ;
#19245 = B_SPLINE_CURVE_WITH_KNOTS ( 'NONE', 3,
 ( #64049, #72170, #3276, #65051 ),
 .UNSPECIFIED., .F., .F.,
 ( 4, 4 ),
 ( 0.01672295409251149667, 0.02560742481406136015 ),
 .UNSPECIFIED. ) ;
#19246 = CARTESIAN_POINT ( 'NONE',  ( 5.625422033609194017, 26.18080186712590773, 3.090169943749475401 ) ) ;
#19247 = CARTESIAN_POINT ( 'NONE',  ( 32.19481522723634725, 40.36126292948897287, 6.180339887498949913 ) ) ;
#19248 = CARTESIAN_POINT ( 'NONE',  ( 92.68684311912451790, 230.9865022471902876, -10.00000000000009592 ) ) ;
#19249 = CARTESIAN_POINT ( 'NONE',  ( 155.4810912439522212, 261.3458456796594760, -18.44218279064527266 ) ) ;
#19250 = CARTESIAN_POINT ( 'NONE',  ( 71.61951074668084516, 58.89861525787757301, -15.38682514613026697 ) ) ;
#19251 = CARTESIAN_POINT ( 'NONE',  ( 87.73226871325611853, 43.96903184879543858, -2.008524143530736161 ) ) ;
#19252 = CARTESIAN_POINT ( 'NONE',  ( 6.183361268541195166, 180.5024278399160949, 9.188101187500095079 ) ) ;
#19253 = CARTESIAN_POINT ( 'NONE',  ( 8.569540968619184795, 75.51505761670109962, -10.00000000000000000 ) ) ;
#19254 = ORIENTED_EDGE ( 'NONE', *, *, #9448, .T. ) ;
#19255 = CARTESIAN_POINT ( 'NONE',  ( 87.01088915102032217, 46.46540990613273436, 8.894669589848916758 ) ) ;
#19256 = CARTESIAN_POINT ( 'NONE',  ( 15.67984500357415278, 27.79103043416548502, 8.090169943749478065 ) ) ;
#19257 = CARTESIAN_POINT ( 'NONE',  ( 81.64626603452745712, 41.61031147741153546, 5.575064572453345413 ) ) ;
#19258 = CARTESIAN_POINT ( 'NONE',  ( 32.38097682878547090, 183.3768266524160140, 9.188101187500096856 ) ) ;
#19259 = VECTOR ( 'NONE', #56208, 1000.000000000000000 ) ;
#19260 = CARTESIAN_POINT ( 'NONE',  ( 161.4726291907278721, 250.9681975403669867, 14.52346149734912117 ) ) ;
#19261 = CARTESIAN_POINT ( 'NONE',  ( 147.4368675721658519, 275.2788497866417288, 5.050119523016719292 ) ) ;
#19262 = CARTESIAN_POINT ( 'NONE',  ( 30.74868702942336895, 36.49103043416551628, -8.090169943749479842 ) ) ;
#19263 = CARTESIAN_POINT ( 'NONE',  ( 178.6323251955368505, 291.6746863476311660, 6.062186576083094636 ) ) ;
#19264 = CARTESIAN_POINT ( 'NONE',  ( 177.9425575674935374, 293.7981536106174758, 2.760600958814514616 ) ) ;
#19265 = CARTESIAN_POINT ( 'NONE',  ( 179.0121081408051396, 278.3636465084506426, -16.96624558982258080 ) ) ;
#19266 = CARTESIAN_POINT ( 'NONE',  ( 69.08701910782110645, 67.88901153317110015, -8.224971608199886930 ) ) ;
#19267 = B_SPLINE_SURFACE_WITH_KNOTS ( 'NONE', 3, 1, ( 
 ( #7412, #45412 ),
 ( #6436, #45894 ),
 ( #37805, #5929 ),
 ( #60105, #21634 ),
 ( #99639, #14030 ),
 ( #37314, #99139 ),
 ( #61105, #92078 ),
 ( #47409, #320 ),
 ( #24117, #61606 ),
 ( #9935, #46401 ),
 ( #92559, #63117 ),
 ( #70715, #94554 ),
 ( #1832, #84956 ),
 ( #15499, #55008 ),
 ( #1330, #69213 ),
 ( #62600, #77838 ),
 ( #7932, #78839 ),
 ( #25110, #32212 ),
 ( #69712, #94060 ),
 ( #85986, #100141 ),
 ( #30727, #38806 ),
 ( #32714, #23104 ),
 ( #63614, #53995 ),
 ( #16514, #55989 ),
 ( #814, #24613 ),
 ( #77325, #31209 ),
 ( #16017, #55495 ),
 ( #79372, #86481 ),
 ( #78335, #86986 ),
 ( #17008, #62096 ),
 ( #93043, #23599 ) ),
 .UNSPECIFIED., .F., .F., .F.,
 ( 4, 3, 3, 3, 3, 3, 3, 3, 3, 3, 4 ),
 ( 2, 2 ),
 ( 0.000000000000000000, 0.1333490885032353190, 0.3007194338854385363, 0.4699862290245196972, 0.5844252810809350551, 0.6686540514502717913, 0.7354980260655500368, 0.8028463152565585847, 0.8633854507757243724, 0.9437142632667462339, 1.000000000000000000 ),
 ( 0.000000000000000000, 1.000000000000000000 ),
 .UNSPECIFIED. ) ;
#19268 = CARTESIAN_POINT ( 'NONE',  ( 84.23301146803963491, 230.9860189848785410, -2.679491924311252493 ) ) ;
#19269 = CARTESIAN_POINT ( 'NONE',  ( 83.38047668388445288, 51.78471284047384415, 14.96842148903410319 ) ) ;
#19270 = PLANE ( 'NONE',  #41360 ) ;
#19271 = CARTESIAN_POINT ( 'NONE',  ( 88.42888488385111145, 211.8615022471902023, 5.000000000000051514 ) ) ;
#19272 = CARTESIAN_POINT ( 'NONE',  ( 75.15470013510049796, 53.07573778316540825, 16.49092276959341064 ) ) ;
#19273 = CARTESIAN_POINT ( 'NONE',  ( 181.4204268205617154, 259.5203828285251006, -11.17471347674236348 ) ) ;
#19274 = CARTESIAN_POINT ( 'NONE',  ( 38.76756708593069334, 199.3149278399161233, -9.188101187500095079 ) ) ;
#19275 = ORIENTED_EDGE ( 'NONE', *, *, #74132, .F. ) ;
#19276 = CARTESIAN_POINT ( 'NONE',  ( -17.81655838990255702, 80.92514050927856317, 14.32002587595537690 ) ) ;
#19277 = CARTESIAN_POINT ( 'NONE',  ( 198.7829547491859330, 286.3448180261817129, -18.59838968157616179 ) ) ;
#19278 = CARTESIAN_POINT ( 'NONE',  ( 41.10966550219798421, 207.8207943907112565, -18.47570218321542868 ) ) ;
#19279 = ORIENTED_EDGE ( 'NONE', *, *, #68824, .T. ) ;
#19280 = CARTESIAN_POINT ( 'NONE',  ( 171.2251843287659483, 286.5252364908957929, 7.482153322356102088 ) ) ;
#19281 = CARTESIAN_POINT ( 'NONE',  ( 207.6007741873543750, 271.0719067473055475, 7.587922723682903658 ) ) ;
#19282 = CARTESIAN_POINT ( 'NONE',  ( 1.813001633210440611, 27.74720351945397923, 10.00000000000000000 ) ) ;
#19283 = CARTESIAN_POINT ( 'NONE',  ( 24.98947064339976265, 26.37878583063841731, 9.188101187500006262 ) ) ;
#19284 = CARTESIAN_POINT ( 'NONE',  ( 189.0887393702818997, 265.5389857731253187, 10.68645298647155784 ) ) ;
#19285 = CARTESIAN_POINT ( 'NONE',  ( 196.4808189786114951, 290.3322341467384717, -17.84817245450773271 ) ) ;
#19286 = EDGE_CURVE ( 'NONE', #80986, #13784, #45261, .T. ) ;
#19287 = CARTESIAN_POINT ( 'NONE',  ( 175.1555329544323172, 257.3877955703446787, 11.56198837495037068 ) ) ;
#19288 = ORIENTED_EDGE ( 'NONE', *, *, #3295, .F. ) ;
#19289 = CARTESIAN_POINT ( 'NONE',  ( 19.20273687360401027, 16.80170272979925628, 7.433330006724137462 ) ) ;
#19290 = CARTESIAN_POINT ( 'NONE',  ( 68.45344762042827824, 64.57392882346940155, 12.12708197196866600 ) ) ;
#19291 = CARTESIAN_POINT ( 'NONE',  ( 171.6221518209352439, 252.5826950423761161, 8.616696649246458506 ) ) ;
#19292 = CARTESIAN_POINT ( 'NONE',  ( 14.02286894203806433, 172.2365022471902307, 10.00000000000009948 ) ) ;
#19293 = EDGE_LOOP ( 'NONE', ( #22638, #27043, #93492, #67858 ) ) ;
#19294 = CARTESIAN_POINT ( 'NONE',  ( 72.45938080685448313, 71.20901404950713243, -6.080114014991351290 ) ) ;
#19295 = CARTESIAN_POINT ( 'NONE',  ( 191.4484954869714954, 299.0484741143815199, 8.684991747358081327 ) ) ;
#19296 = DIRECTION ( 'NONE',  ( -0.8660254037844377084, -0.5000000000000014433, -0.000000000000000000 ) ) ;
#19297 = CARTESIAN_POINT ( 'NONE',  ( 166.7686158928260909, 246.5184119549025752, 0.4773397470127070386 ) ) ;
#19298 = EDGE_CURVE ( 'NONE', #26627, #22737, #19418, .T. ) ;
#19299 = ORIENTED_EDGE ( 'NONE', *, *, #69056, .T. ) ;
#19300 = ORIENTED_EDGE ( 'NONE', *, *, #81415, .T. ) ;
#19302 = LINE ( 'NONE', #50169, #20072 ) ;
#19301 = CARTESIAN_POINT ( 'NONE',  ( 161.8935665241663457, 250.2391126920490194, -13.69501063978231770 ) ) ;
#19303 = CARTESIAN_POINT ( 'NONE',  ( 196.4808189786114951, 290.3322341467384717, -17.84817245450773271 ) ) ;
#19304 = VERTEX_POINT ( 'NONE', #46605 ) ;
#19305 = CARTESIAN_POINT ( 'NONE',  ( 65.84722295223909327, 68.92719200281077008, -2.492171992192153240 ) ) ;
#19306 = CIRCLE ( 'NONE', #75919, 7.500000000000000000 ) ;
#19307 = CARTESIAN_POINT ( 'NONE',  ( 197.8809552785519656, 287.9071269377202498, 17.61728046362068412 ) ) ;
#19308 = CARTESIAN_POINT ( 'NONE',  ( 69.56017153759040639, 71.20905094733247154, -1.738453268357221582 ) ) ;
#19309 = CARTESIAN_POINT ( 'NONE',  ( 78.10947740687990404, 61.47724562959768946, -16.15800848020992930 ) ) ;
#19310 = EDGE_CURVE ( 'NONE', #42311, #2950, #1023, .T. ) ;
#19311 = CARTESIAN_POINT ( 'NONE',  ( 205.3943609285979051, 274.8935266139653777, -13.14270440534009943 ) ) ;
#19312 = CARTESIAN_POINT ( 'NONE',  ( 112.2171730965159071, 247.8464784336661353, 1.353441290958777525E-15 ) ) ;
#19313 = AXIS2_PLACEMENT_3D ( 'NONE', #56588, #40870, #95654 ) ;
#19314 = CARTESIAN_POINT ( 'NONE',  ( 34.21208616421488102, 183.8927522451417929, -10.00000000000009237 ) ) ;
#19315 = ORIENTED_EDGE ( 'NONE', *, *, #61391, .F. ) ;
#19316 = VECTOR ( 'NONE', #96987, 1000.000000000000000 ) ;
#19317 = CARTESIAN_POINT ( 'NONE',  ( 208.1757572214753793, 270.0760069187178374, 2.172546422564154867 ) ) ;
#19318 = VERTEX_POINT ( 'NONE', #31409 ) ;
#19319 = CARTESIAN_POINT ( 'NONE',  ( 32.94608582406294772, 39.99752408145594984, 5.678558825948277544 ) ) ;
#19320 = CARTESIAN_POINT ( 'NONE',  ( 159.9671766634011192, 253.5757178060795809, 16.49140845334465411 ) ) ;
#19321 = CARTESIAN_POINT ( 'NONE',  ( -110.0000000000000142, 0.000000000000000000, -9.212605237762117483 ) ) ;
#19322 = CARTESIAN_POINT ( 'NONE',  ( 72.16419236301562989, 200.2202760586659736, -5.415160957724236172E-17 ) ) ;
#19323 = ORIENTED_EDGE ( 'NONE', *, *, #781, .T. ) ;
#19324 = FACE_OUTER_BOUND ( 'NONE', #53272, .T. ) ;
#19325 = CARTESIAN_POINT ( 'NONE',  ( 150.8167050463783312, 269.4247995599803289, 14.38040671671637938 ) ) ;
#19326 = CARTESIAN_POINT ( 'NONE',  ( 168.9285091408607684, 266.8905904589466900, 17.77692745299157195 ) ) ;
#19327 = CARTESIAN_POINT ( 'NONE',  ( 172.6353124949622213, 276.9286716572659657, 15.75460722331730246 ) ) ;
#19328 = ORIENTED_EDGE ( 'NONE', *, *, #40844, .T. ) ;
#19329 = VECTOR ( 'NONE', #13311, 1000.000000000000000 ) ;
#19330 = FACE_OUTER_BOUND ( 'NONE', #71415, .T. ) ;
#19331 = DIRECTION ( 'NONE',  ( -0.7511915808658203852, -0.6600842437418951159, 0.000000000000000000 ) ) ;
#19332 = CARTESIAN_POINT ( 'NONE',  ( 203.5080190724872011, 278.1607665491929993, -15.47044080916498743 ) ) ;
#19333 = ORIENTED_EDGE ( 'NONE', *, *, #9088, .F. ) ;
#19334 = DIRECTION ( 'NONE',  ( -0.8660254037844379305, -0.5000000000000014433, -0.000000000000000000 ) ) ;
#19335 = CARTESIAN_POINT ( 'NONE',  ( 68.40658122464360247, 69.43545487971397279, -4.271840473564598284 ) ) ;
#19336 = CARTESIAN_POINT ( 'NONE',  ( 79.14312167556931854, 57.64441083166269664, 0.000000000000000000 ) ) ;
#19337 = CARTESIAN_POINT ( 'NONE',  ( 80.74781574657599492, 57.21644485803225422, 16.56566952311892749 ) ) ;
#19338 = CARTESIAN_POINT ( 'NONE',  ( 177.0481772032109120, 269.7367243736813975, 17.49060471085816815 ) ) ;
#19339 = AXIS2_PLACEMENT_3D ( 'NONE', #24960, #7262, #99991 ) ;
#19340 = PLANE ( 'NONE',  #48267 ) ;
#19341 = CARTESIAN_POINT ( 'NONE',  ( 86.18027666378026197, 49.75620593066997799, 22.50000000000002842 ) ) ;
#19342 = CARTESIAN_POINT ( 'NONE',  ( 153.8374836801523315, 264.9808921322257902, -16.57868851438277957 ) ) ;
#19343 = ORIENTED_EDGE ( 'NONE', *, *, #14894, .F. ) ;
#19344 = CARTESIAN_POINT ( 'NONE',  ( 10.02758540662582654, 165.0494855054052437, -2.679491924311248496 ) ) ;
#19345 = CARTESIAN_POINT ( 'NONE',  ( 126.2364799639240260, 237.5643266524160140, 9.188101187500095079 ) ) ;
#19346 = VERTEX_POINT ( 'NONE', #46097 ) ;
#19347 = CARTESIAN_POINT ( 'NONE',  ( 82.09644834878162101, 44.24571031629783846, -9.484918253198090454 ) ) ;
#19348 = DIRECTION ( 'NONE',  ( 1.000000000000000000, 0.000000000000000000, 0.000000000000000000 ) ) ;
#19349 = EDGE_CURVE ( 'NONE', #44888, #90330, #38504, .T. ) ;
#19350 = CARTESIAN_POINT ( 'NONE',  ( 163.2708734627827312, 285.5880326804372089, 1.431608037597408289 ) ) ;
#19351 = FACE_BOUND ( 'NONE', #10827, .T. ) ;
#19352 = CARTESIAN_POINT ( 'NONE',  ( 74.21441779998785648, 58.33243994155952805, 15.86737782346030201 ) ) ;
#19353 = CARTESIAN_POINT ( 'NONE',  ( 178.6690291948835068, 254.3411016048053170, 4.509037496016676805 ) ) ;
#19354 = ORIENTED_EDGE ( 'NONE', *, *, #97840, .T. ) ;
#19355 = CARTESIAN_POINT ( 'NONE',  ( 80.65711718680429954, 57.43377920104063605, -16.23697608741668574 ) ) ;
#19356 = CARTESIAN_POINT ( 'NONE',  ( -19.72534873751503781, 92.94298401958562295, 59.99999999999999289 ) ) ;
#19357 = DIRECTION ( 'NONE',  ( 0.000000000000000000, 0.000000000000000000, 1.000000000000000000 ) ) ;
#19358 = EDGE_CURVE ( 'NONE', #83021, #6447, #16738, .T. ) ;
#19359 = DIRECTION ( 'NONE',  ( -0.6681572590663519273, 0.7440200784635719877, 0.000000000000000000 ) ) ;
#19360 = ADVANCED_FACE ( 'NONE', ( #16715 ), #9643, .T. ) ;
#19361 = PLANE ( 'NONE',  #90270 ) ;
#19362 = CARTESIAN_POINT ( 'NONE',  ( 67.26344415152594536, 67.87376856832382543, 6.424593239651369636 ) ) ;
#19363 = EDGE_CURVE ( 'NONE', #87907, #29268, #40406, .T. ) ;
#19364 = CARTESIAN_POINT ( 'NONE',  ( 157.1850763439666139, 258.3944569110938687, -16.98181238659443437 ) ) ;
#19365 = CARTESIAN_POINT ( 'NONE',  ( 174.5802574196832779, 252.1115117894923117, 3.521029629026526386 ) ) ;
#19366 = CARTESIAN_POINT ( 'NONE',  ( 21.19816502305182837, 13.20801979619928268, -3.090169943749474069 ) ) ;
#19367 = FACE_OUTER_BOUND ( 'NONE', #26874, .T. ) ;
#19368 = DIRECTION ( 'NONE',  ( 0.000000000000000000, 0.000000000000000000, 1.000000000000000000 ) ) ;
#19369 = CARTESIAN_POINT ( 'NONE',  ( 169.3955309194774372, 285.1200513657703937, -8.058459443620145990 ) ) ;
#19370 = FACE_OUTER_BOUND ( 'NONE', #19739, .T. ) ;
#19371 = CARTESIAN_POINT ( 'NONE',  ( 157.5112492719526642, 271.0101375079576655, -14.70005484135263529 ) ) ;
#19372 = CARTESIAN_POINT ( 'NONE',  ( 134.5988642195610225, 258.5177522451419350, 5.000000000000046185 ) ) ;
#19373 = CARTESIAN_POINT ( 'NONE',  ( 77.80060431799728349, 52.79663923430527461, -15.76147068082156899 ) ) ;
#19374 = ORIENTED_EDGE ( 'NONE', *, *, #67059, .F. ) ;
#19375 = AXIS2_PLACEMENT_3D ( 'NONE', #35685, #82342, #12910 ) ;
#19376 = CARTESIAN_POINT ( 'NONE',  ( 157.4177733328310467, 257.9914139036126812, 18.29188238796808363 ) ) ;
#19377 = CARTESIAN_POINT ( 'NONE',  ( 190.5726849661229210, 300.5654224342945326, -0.2192718484028965964 ) ) ;
#19378 = CARTESIAN_POINT ( 'NONE',  ( -7.645548028435306342, 157.2048013555409796, 4.594050593750051981 ) ) ;
#19379 = CARTESIAN_POINT ( 'NONE',  ( 39.47103917862304456, 205.8464784336661637, 1.353441290958777327E-15 ) ) ;
#19380 = AXIS2_PLACEMENT_3D ( 'NONE', #15951, #39721, #77776 ) ;
#19381 = CARTESIAN_POINT ( 'NONE',  ( 83.23303302330263875, 41.40721320258948879, 4.067920842383329294 ) ) ;
#19382 = CARTESIAN_POINT ( 'NONE',  ( 25.38349897777161246, 16.78380873178787169, -6.180339887498949025 ) ) ;
#19383 = CARTESIAN_POINT ( 'NONE',  ( 68.10039974585599509, 65.18542567973287305, -10.72853162865224519 ) ) ;
#19384 = CARTESIAN_POINT ( 'NONE',  ( 157.2777284163744582, 258.2339788142568864, -16.82360006463426316 ) ) ;
#19385 = CARTESIAN_POINT ( 'NONE',  ( 189.0965068574246573, 290.5071001834722892, -14.60706148674475280 ) ) ;
#19386 = CARTESIAN_POINT ( 'NONE',  ( 146.8058449195592061, 276.3718130816831149, 4.181814292810413392 ) ) ;
#19387 = CARTESIAN_POINT ( 'NONE',  ( 73.74433816791051299, 55.34249187257252345, -16.59213747446436571 ) ) ;
#19389 = CARTESIAN_POINT ( 'NONE',  ( 77.51335635343681929, 208.8927522451417929, 10.00000000000009592 ) ) ;
#19388 = CARTESIAN_POINT ( 'NONE',  ( 167.6973146981588911, 256.6379102646401975, 13.70945070367496754 ) ) ;
#19390 = CARTESIAN_POINT ( 'NONE',  ( 76.24678322307947553, 56.72522291046242060, 16.60682109591483169 ) ) ;
#19391 = CARTESIAN_POINT ( 'NONE',  ( 33.69734285410222441, 21.58380873178789372, 6.180339887498953466 ) ) ;
#19392 = DIRECTION ( 'NONE',  ( -0.000000000000000000, -0.000000000000000000, -1.000000000000000000 ) ) ;
#19393 = VECTOR ( 'NONE', #85460, 1000.000000000000000 ) ;
#19394 = CARTESIAN_POINT ( 'NONE',  ( 49.45774171355136417, 189.3615022471902023, 5.000000000000051514 ) ) ;
#19395 = CARTESIAN_POINT ( 'NONE',  ( 181.9890126569457891, 291.7084811444626666, 9.326053301564767750 ) ) ;
#19396 = CARTESIAN_POINT ( 'NONE',  ( 163.1691520398773321, 248.0297337694385931, 11.21816141384514331 ) ) ;
#19397 = CARTESIAN_POINT ( 'NONE',  ( 12.08367997547019002, 165.5327760586659451, 1.948934522072303157E-15 ) ) ;
#19398 = CARTESIAN_POINT ( 'NONE',  ( 32.83301474718356161, 37.14336893147758900, 7.433330006724141015 ) ) ;
#19399 = DIRECTION ( 'NONE',  ( 0.4999999999999998890, -0.8660254037844385966, 0.000000000000000000 ) ) ;
#19400 = CARTESIAN_POINT ( 'NONE',  ( 192.1396999271463812, 297.8512729055811974, 12.32430960859512403 ) ) ;
#19401 = CARTESIAN_POINT ( 'NONE',  ( 33.82173346387272517, 28.03085787977764909, 9.188101187500006262 ) ) ;
#19402 = CARTESIAN_POINT ( 'NONE',  ( 156.2909461963670310, 261.2938674384161004, -17.49506900824429323 ) ) ;
#19403 = CARTESIAN_POINT ( 'NONE',  ( 179.3884211033321492, 277.5219014342368951, 16.65719480442988498 ) ) ;
#19404 = LINE ( 'NONE', #48789, #36811 ) ;
#19405 = DIRECTION ( 'NONE',  ( -0.1889875038809575303, -0.9819794923402652698, 0.000000000000000000 ) ) ;
#19406 = DIRECTION ( 'NONE',  ( 0.000000000000000000, 0.000000000000000000, 1.000000000000000000 ) ) ;
#19407 = CARTESIAN_POINT ( 'NONE',  ( 5.233272902960924178, 23.99752408145590010, 5.678558825948277544 ) ) ;
#19408 = CARTESIAN_POINT ( 'NONE',  ( 124.2787281577965075, 235.8927522451418213, 10.00000000000009948 ) ) ;
#19409 = CARTESIAN_POINT ( 'NONE',  ( 18.38602693954342371, 22.56628583063840310, 9.188101187500006262 ) ) ;
#19410 = VECTOR ( 'NONE', #13046, 1000.000000000000000 ) ;
#19411 = CARTESIAN_POINT ( 'NONE',  ( 159.3316980867583368, 259.1362291154864010, 16.70884618213627348 ) ) ;
#19412 = EDGE_CURVE ( 'NONE', #17718, #10180, #76032, .T. ) ;
#19413 = CARTESIAN_POINT ( 'NONE',  ( 154.8556227199321427, 262.4291889417971788, 17.77326384500479861 ) ) ;
#19414 = VERTEX_POINT ( 'NONE', #70932 ) ;
#19415 = CARTESIAN_POINT ( 'NONE',  ( 23.12210336471560623, 25.30066082961422325, -10.00000000000000533 ) ) ;
#19416 = CARTESIAN_POINT ( 'NONE',  ( 206.4640281786353171, 273.0408085897082060, -10.81921452789957883 ) ) ;
#19417 = EDGE_CURVE ( 'NONE', #68127, #63730, #93253, .T. ) ;
#19418 = CIRCLE ( 'NONE', #80913, 70.00000000000001421 ) ;
#19420 = ORIENTED_EDGE ( 'NONE', *, *, #93934, .T. ) ;
#19419 = B_SPLINE_CURVE_WITH_KNOTS ( 'NONE', 3,
 ( #78558, #8146, #78053, #32444, #8642, #85703, #18254, #49150, #25859, #9664, #86200, #95303 ),
 .UNSPECIFIED., .F., .F.,
 ( 4, 2, 2, 2, 2, 4 ),
 ( 0.001153997166473859142, 0.001388415620727351078, 0.001622834074980843014, 0.002091670983487826235, 0.002560507891994809240, 0.003029344800501792244 ),
 .UNSPECIFIED. ) ;
#19421 = CARTESIAN_POINT ( 'NONE',  ( 152.5758826934612955, 268.0217239346885094, 15.77428039732272858 ) ) ;
#19422 = CARTESIAN_POINT ( 'NONE',  ( 207.1122325394003951, 271.9180857031755636, 7.794245785756032774 ) ) ;
#19423 = CARTESIAN_POINT ( 'NONE',  ( 66.54990378112017879, 68.24084232656181825, 4.554841679438449198 ) ) ;
#19424 = CARTESIAN_POINT ( 'NONE',  ( 87.52489256634972037, 45.06004022996452107, 6.936227203615883852 ) ) ;
#19425 = ORIENTED_EDGE ( 'NONE', *, *, #13674, .T. ) ;
#19426 = EDGE_LOOP ( 'NONE', ( #31467, #52292, #78455, #10945 ) ) ;
#19428 = CARTESIAN_POINT ( 'NONE',  ( 204.7986527064648214, 275.9253235211867263, 14.74587861556245905 ) ) ;
#19427 = CARTESIAN_POINT ( 'NONE',  ( 164.1356542478074516, 246.7701760825098916, -4.987495687701697378 ) ) ;
#19429 = CARTESIAN_POINT ( 'NONE',  ( 192.5254593562406171, 297.1831179748913314, 11.00703791256144015 ) ) ;
#19430 = VERTEX_POINT ( 'NONE', #63315 ) ;
#19431 = CARTESIAN_POINT ( 'NONE',  ( 77.69300220237600740, 57.14232284133041873, 16.18446285159314257 ) ) ;
#19432 = CARTESIAN_POINT ( 'NONE',  ( 174.9783775354441104, 262.5161152102281221, 14.35741776163894734 ) ) ;
#19434 = EDGE_CURVE ( 'NONE', #52564, #97421, #53356, .T. ) ;
#19433 = EDGE_LOOP ( 'NONE', ( #45664, #943, #35326, #12163 ) ) ;
#19435 = DIRECTION ( 'NONE',  ( 0.4999999999999998890, -0.8660254037844385966, 0.000000000000000000 ) ) ;
#19436 = CARTESIAN_POINT ( 'NONE',  ( 81.34849765221251516, 49.51565197037416510, -13.99490981827331559 ) ) ;
#19437 = CARTESIAN_POINT ( 'NONE',  ( 81.01539833309765015, 43.04435665648513520, 9.559117910057512546 ) ) ;
#19438 = ORIENTED_EDGE ( 'NONE', *, *, #58095, .F. ) ;
#19439 = CARTESIAN_POINT ( 'NONE',  ( 46.99867368304095550, 76.19044720721625197, 10.00000000000000000 ) ) ;
#19440 = CARTESIAN_POINT ( 'NONE',  ( 169.4433785151117036, 276.3082714494867105, -15.64270847926871966 ) ) ;
#19441 = CARTESIAN_POINT ( 'NONE',  ( 73.35536025913421554, 58.29657773774909657, 15.76285285645408152 ) ) ;
#19442 = ORIENTED_EDGE ( 'NONE', *, *, #68029, .F. ) ;
#19443 = CARTESIAN_POINT ( 'NONE',  ( 175.2041007476701111, 277.6819973178614305, -15.66111034898646359 ) ) ;
#19444 = VERTEX_POINT ( 'NONE', #71434 ) ;
#19445 = EDGE_CURVE ( 'NONE', #37697, #11680, #66971, .T. ) ;
#19446 = CARTESIAN_POINT ( 'NONE',  ( 156.9458340580773665, 266.2207217376895869, -16.53175181285456219 ) ) ;
#19447 = VERTEX_POINT ( 'NONE', #48113 ) ;
#19448 = CARTESIAN_POINT ( 'NONE',  ( -64.74139798177010618, 41.16849083240310847, 10.00000000000000000 ) ) ;
#19449 = ORIENTED_EDGE ( 'NONE', *, *, #2779, .F. ) ;
#19450 =( BOUNDED_CURVE ( )  B_SPLINE_CURVE ( 2, ( #54549, #85533, #74033, #27911, #20331, #51202, #1392, #24180, #46977 ),
 .UNSPECIFIED., .F., .T. ) 
 B_SPLINE_CURVE_WITH_KNOTS ( ( 3, 2, 2, 2, 3 ),
 ( 0.8427419354838709964, 0.8440860215053763715, 0.8467741935483871218, 0.8494623655913978721, 0.8508064516129032473 ),
 .UNSPECIFIED. ) 
 CURVE ( )  GEOMETRIC_REPRESENTATION_ITEM ( )  RATIONAL_B_SPLINE_CURVE ( ( 0.9330127018922194093, 0.9330127018922194093, 1.000000000000000000, 0.8660254037844387076, 1.000000000000000000, 0.8660254037844387076, 1.000000000000000000, 0.9330127018922194093, 0.9330127018922194093 ) ) 
 REPRESENTATION_ITEM ( '' )  );
#19451 = CARTESIAN_POINT ( 'NONE',  ( 87.80086816424551444, 43.95683443436809767, 1.316077942333925277 ) ) ;
#19452 = CARTESIAN_POINT ( 'NONE',  ( 193.5623078039747895, 295.3872437836667473, 14.88922347750675712 ) ) ;
#19453 = CARTESIAN_POINT ( 'NONE',  ( 83.00815485991435594, 53.30142267139500234, 15.60062745561815589 ) ) ;
#19454 = PLANE ( 'NONE',  #57608 ) ;
#19455 = DIRECTION ( 'NONE',  ( -0.04056776950002415755, 0.9991767892008865948, 0.000000000000000000 ) ) ;
#19457 = CARTESIAN_POINT ( 'NONE',  ( 178.4143452015725870, 291.8002240674260861, 6.990295570472018660 ) ) ;
#19456 = VECTOR ( 'NONE', #2361, 1000.000000000000000 ) ;
#19458 = CARTESIAN_POINT ( 'NONE',  ( 191.1000148935602567, 299.6520602076213891, -9.462302242170249400 ) ) ;
#19459 = ORIENTED_EDGE ( 'NONE', *, *, #89556, .F. ) ;
#19460 = CARTESIAN_POINT ( 'NONE',  ( 67.66477494612622934, 65.93994996590180335, 10.43000742999573838 ) ) ;
#19461 = CARTESIAN_POINT ( 'NONE',  ( 26.56877070717806788, 23.84335787977763843, 9.188101187500006262 ) ) ;
#19463 = LINE ( 'NONE', #37106, #51522 ) ;
#19462 = CARTESIAN_POINT ( 'NONE',  ( 149.2923684163597784, 272.0650280510108701, -12.99082738998495756 ) ) ;
#19465 = VERTEX_POINT ( 'NONE', #22819 ) ;
#19464 = CARTESIAN_POINT ( 'NONE',  ( 198.3523905153085423, 287.0905771551796306, 18.52598547438866206 ) ) ;
#19466 = ORIENTED_EDGE ( 'NONE', *, *, #69535, .F. ) ;
#19467 = CARTESIAN_POINT ( 'NONE',  ( 146.6807985088175030, 276.5883998183917925, -3.564129467591749201 ) ) ;
#19468 = EDGE_CURVE ( 'NONE', #57311, #45676, #32909, .T. ) ;
#19469 = CARTESIAN_POINT ( 'NONE',  ( 171.5055362605466485, 259.4143056590929746, -13.88236582212129377 ) ) ;
#19470 = DIRECTION ( 'NONE',  ( 0.4999999999999998890, -0.8660254037844385966, 0.000000000000000000 ) ) ;
#19471 = DIRECTION ( 'NONE',  ( 0.000000000000000000, 0.000000000000000000, 1.000000000000000000 ) ) ;
#19472 = CARTESIAN_POINT ( 'NONE',  ( 199.1649783209272471, 285.6831337902369228, -18.56878453077520774 ) ) ;
#19473 = CARTESIAN_POINT ( 'NONE',  ( 190.2679671178493095, 301.0932092294775089, 0.1305210825167657518 ) ) ;
#19474 = AXIS2_PLACEMENT_3D ( 'NONE', #69901, #23800, #70407 ) ;
#19475 = EDGE_LOOP ( 'NONE', ( #85063, #75899, #15887, #69758 ) ) ;
#19477 = EDGE_CURVE ( 'NONE', #12886, #63646, #73922, .T. ) ;
#19476 = CARTESIAN_POINT ( 'NONE',  ( 167.3627897228288077, 252.8219202345026702, -12.34552495514862613 ) ) ;
#19478 = CARTESIAN_POINT ( 'NONE',  ( 132.0729567918564555, 240.3927522451418213, 10.00000000000009948 ) ) ;
#19479 = CARTESIAN_POINT ( 'NONE',  ( 165.0437781805843258, 244.7827860485373606, -2.050141714668513693 ) ) ;
#19480 = CARTESIAN_POINT ( 'NONE',  ( 36.81016237556818993, 185.3927522451417929, -10.00000000000009059 ) ) ;
#19481 = CARTESIAN_POINT ( 'NONE',  ( 103.7194723697636221, 236.8149278399160949, -9.188101187500095079 ) ) ;
#19482 = CARTESIAN_POINT ( 'NONE',  ( 183.6574624063936483, 296.2739094579258676, -2.715018486543457676 ) ) ;
#19483 = EDGE_CURVE ( 'NONE', #44296, #82635, #21082, .T. ) ;
#19484 = DIRECTION ( 'NONE',  ( 0.000000000000000000, 0.000000000000000000, 1.000000000000000000 ) ) ;
#19485 = CARTESIAN_POINT ( 'NONE',  ( 84.79698219828915740, 50.36941373931320243, 13.45059404220081234 ) ) ;
#19486 = CARTESIAN_POINT ( 'NONE',  ( 162.4263297320084121, 249.3163397476629086, 11.18012070315788087 ) ) ;
#19487 = CARTESIAN_POINT ( 'NONE',  ( 24.58674819472551931, 178.8768266524160140, 9.188101187500098632 ) ) ;
#19488 = CARTESIAN_POINT ( 'NONE',  ( 65.36586985908992631, 182.5653022007868458, 0.000000000000000000 ) ) ;
#19489 = VERTEX_POINT ( 'NONE', #49611 ) ;
#19490 = ORIENTED_EDGE ( 'NONE', *, *, #54384, .F. ) ;
#19492 = ADVANCED_FACE ( 'NONE', ( #4015 ), #34415, .T. ) ;
#19491 = CARTESIAN_POINT ( 'NONE',  ( 73.77070425341645432, 68.39923094797843817, 11.48015304846415141 ) ) ;
#19493 = CARTESIAN_POINT ( 'NONE',  ( 147.4771206202524354, 275.6046823160672830, -0.001107820683494442279 ) ) ;
#19494 = EDGE_CURVE ( 'NONE', #20041, #9204, #92318, .T. ) ;
#19495 = CARTESIAN_POINT ( 'NONE',  ( 70.25964755056540412, 71.21311948813186632, -0.4467044605720515982 ) ) ;
#19496 = CARTESIAN_POINT ( 'NONE',  ( 147.2494378675467033, 275.6034875578896504, 3.639370109197119341 ) ) ;
#19497 = CARTESIAN_POINT ( 'NONE',  ( 192.9905603666904881, 263.7646147800884933, -4.130271572274535785 ) ) ;
#19498 = PLANE ( 'NONE',  #94851 ) ;
#19499 = CARTESIAN_POINT ( 'NONE',  ( 185.8711499578670043, 286.5456327281862627, 15.65987533235325202 ) ) ;
#19500 = DIRECTION ( 'NONE',  ( 0.8660254037844382635, 0.5000000000000005551, 0.000000000000000000 ) ) ;
#19501 = CARTESIAN_POINT ( 'NONE',  ( 43.61180991440864574, 205.1744531367911293, 4.594050593750047540 ) ) ;
#19502 = CARTESIAN_POINT ( 'NONE',  ( 93.82350145804376496, 211.6427522451417644, 1.119607411625061291E-15 ) ) ;
#19503 = CARTESIAN_POINT ( 'NONE',  ( 79.28866853763615552, 59.92453731934287475, -16.49803216704722786 ) ) ;
#19504 = CARTESIAN_POINT ( 'NONE',  ( 179.0002306397571488, 259.3607547712236965, -10.30360065349030307 ) ) ;
#19505 = CARTESIAN_POINT ( 'NONE',  ( -2.476892769303202790, 175.5024278399161233, -9.188101187500093303 ) ) ;
#19506 = CARTESIAN_POINT ( 'NONE',  ( 68.76972388951917026, 64.18474346107819883, -11.93496927694269871 ) ) ;
#19507 = CARTESIAN_POINT ( 'NONE',  ( 198.4522155198218059, 286.9176751754968109, -17.57438352224490075 ) ) ;
#19508 = CYLINDRICAL_SURFACE ( 'NONE', #3119, 17.82106496071139645 ) ;
#19509 = CARTESIAN_POINT ( 'NONE',  ( 192.4172326059820648, 297.3705722050773943, -12.52563289807247848 ) ) ;
#19510 = CARTESIAN_POINT ( 'NONE',  ( 29.12701137275935892, 44.61184105132205957, -10.00000000000000000 ) ) ;
#19511 = CARTESIAN_POINT ( 'NONE',  ( 203.6831990939301420, 276.1885599565742382, 13.29506139827553390 ) ) ;
#19512 = CARTESIAN_POINT ( 'NONE',  ( 68.12666880830131788, 66.36964627602041844, 9.486737533835349012 ) ) ;
#19513 = DIRECTION ( 'NONE',  ( -0.000000000000000000, 0.000000000000000000, -1.000000000000000000 ) ) ;
#19514 = ORIENTED_EDGE ( 'NONE', *, *, #50979, .T. ) ;
#19515 = CARTESIAN_POINT ( 'NONE',  ( 0.5273063997304934247, 181.1115022471903444, -5.000000000000047962 ) ) ;
#19516 = CARTESIAN_POINT ( 'NONE',  ( 196.8708119716154954, 268.3476497963631573, -11.07389558091716708 ) ) ;
#19517 = CARTESIAN_POINT ( 'NONE',  ( 120.7695210546522446, 240.5333772461660544, 9.188101187500095079 ) ) ;
#19518 = CARTESIAN_POINT ( 'NONE',  ( 20.27082849090286487, 27.10171378149918908, 9.188101187500008038 ) ) ;
#19519 = CARTESIAN_POINT ( 'NONE',  ( 74.75515603635287221, 67.17787269918751747, 12.46789500065375123 ) ) ;
#19520 = AXIS2_PLACEMENT_3D ( 'NONE', #27495, #50765, #58364 ) ;
#19521 = LINE ( 'NONE', #56973, #46779 ) ;
#19523 = CARTESIAN_POINT ( 'NONE',  ( 110.0000000000000000, 15.00000000000003908, 59.99999999999999289 ) ) ;
#19522 = CARTESIAN_POINT ( 'NONE',  ( 81.72320923516716107, 41.47097560424118967, -5.133185482711140502 ) ) ;
#19524 = CARTESIAN_POINT ( 'NONE',  ( 48.61286661847091040, 84.94359857078811160, -10.00000000000000000 ) ) ;
#19525 = ORIENTED_EDGE ( 'NONE', *, *, #52335, .T. ) ;
#19526 = CARTESIAN_POINT ( 'NONE',  ( 151.0099717111976076, 269.0900518771037468, 15.84752309685681659 ) ) ;
#19527 = CARTESIAN_POINT ( 'NONE',  ( 207.6502225385047780, 270.9862596907630063, -1.369768233574514271 ) ) ;
#19528 = CARTESIAN_POINT ( 'NONE',  ( 187.9019955452718023, 260.0457317612239194, -6.306085470763082235 ) ) ;
#19529 = CARTESIAN_POINT ( 'NONE',  ( 172.7307785454424618, 267.9789046868485229, -16.30596211021181219 ) ) ;
#19530 = CARTESIAN_POINT ( 'NONE',  ( 81.75576429312462778, 55.32182455908718310, -15.92503432444246769 ) ) ;
#19531 = ORIENTED_EDGE ( 'NONE', *, *, #89878, .F. ) ;
#19532 = CARTESIAN_POINT ( 'NONE',  ( 69.30351820464169066, 67.54782995425182435, 8.872334801762805867 ) ) ;
#19533 = CARTESIAN_POINT ( 'NONE',  ( 165.6138761065251970, 269.2084108731353354, -16.71299972576612802 ) ) ;
#19534 = CARTESIAN_POINT ( 'NONE',  ( 84.20645638665105537, 43.21656257813889113, 5.952274718717716517 ) ) ;
#19535 = CARTESIAN_POINT ( 'NONE',  ( 79.92914515571509071, 53.26920964233459443, 15.63750486048350474 ) ) ;
#19536 = CARTESIAN_POINT ( 'NONE',  ( 182.5990217920488590, 295.0943774630480902, 4.729822608770373193 ) ) ;
#19537 = PLANE ( 'NONE',  #29075 ) ;
#19538 = AXIS2_PLACEMENT_3D ( 'NONE', #1517, #56179, #87173 ) ;
#19539 = CARTESIAN_POINT ( 'NONE',  ( 150.6825202918323612, 277.8236102357049049, -1.156507784398024520E-06 ) ) ;
#19540 = CARTESIAN_POINT ( 'NONE',  ( 193.7492780744840957, 282.5563289966625575, 17.04412244182808678 ) ) ;
#19541 = CARTESIAN_POINT ( 'NONE',  ( 45.29353982640898835, 28.01110640527296525, 2.839279412974134775 ) ) ;
#19542 = CARTESIAN_POINT ( 'NONE',  ( 195.3480551831553385, 290.3289108874006388, -16.65360927049558981 ) ) ;
#19543 = EDGE_LOOP ( 'NONE', ( #48985, #90563, #27878, #68756, #64756, #66023, #53904, #39775, #16570, #78314, #55541, #57151, #69658, #10410, #97110, #55371, #20797, #29002, #89464 ) ) ;
#19544 = DIRECTION ( 'NONE',  ( -0.8660254037844387076, -0.4999999999999998890, -0.000000000000000000 ) ) ;
#19545 = CARTESIAN_POINT ( 'NONE',  ( 194.8708600166808651, 293.1207648669033006, -14.79199694356877970 ) ) ;
#19546 = CARTESIAN_POINT ( 'NONE',  ( 156.0722444812057574, 261.8173697120565180, -16.98794231501332419 ) ) ;
#19548 = EDGE_CURVE ( 'NONE', #76128, #61758, #93838, .T. ) ;
#19547 = ORIENTED_EDGE ( 'NONE', *, *, #21918, .F. ) ;
#19549 = CARTESIAN_POINT ( 'NONE',  ( 32.86530875704925592, 117.5470576720593954, 59.99999999999999289 ) ) ;
#19550 = CARTESIAN_POINT ( 'NONE',  ( 82.35285118013293015, 53.50770157854819331, -15.77620284334259004 ) ) ;
#19551 = PLANE ( 'NONE',  #22097 ) ;
#19552 = ORIENTED_EDGE ( 'NONE', *, *, #67306, .T. ) ;
#19553 = CARTESIAN_POINT ( 'NONE',  ( 83.25962220535622293, 225.0024278399160949, -9.188101187500093303 ) ) ;
#19554 = CARTESIAN_POINT ( 'NONE',  ( 77.82431933516703282, 52.07990706851629881, -15.61525674500613015 ) ) ;
#19555 = CARTESIAN_POINT ( 'NONE',  ( -22.42236680055709641, 157.8615022471902591, 0.000000000000000000 ) ) ;
#19556 = DIRECTION ( 'NONE',  ( -0.8660254037844387076, -0.4999999999999998890, -0.000000000000000000 ) ) ;
#19557 = ORIENTED_EDGE ( 'NONE', *, *, #25246, .F. ) ;
#19558 = EDGE_CURVE ( 'NONE', #53564, #86106, #64466, .T. ) ;
#19559 = ORIENTED_EDGE ( 'NONE', *, *, #39122, .F. ) ;
#19560 = DIRECTION ( 'NONE',  ( 0.5000000000000001110, -0.8660254037844384856, -0.000000000000000000 ) ) ;
#19561 = ADVANCED_FACE ( 'NONE', ( #5021 ), #82060, .F. ) ;
#19562 = VERTEX_POINT ( 'NONE', #13618 ) ;
#19563 = CARTESIAN_POINT ( 'NONE',  ( 179.7609715772761376, 289.9450057921314965, -11.88024692884158462 ) ) ;
#19564 = VERTEX_POINT ( 'NONE', #6006 ) ;
#19565 = DIRECTION ( 'NONE',  ( -0.6118251767726359258, -0.7909930170786165782, 0.000000000000000000 ) ) ;
#19566 = CARTESIAN_POINT ( 'NONE',  ( 155.1601726304954809, 261.9016930232608615, -18.56587418422714464 ) ) ;
#19567 = ORIENTED_EDGE ( 'NONE', *, *, #541, .T. ) ;
#19568 = CARTESIAN_POINT ( 'NONE',  ( 182.9467913113457769, 279.7477425878400368, -16.58815582825729962 ) ) ;
#19569 = CARTESIAN_POINT ( 'NONE',  ( 82.17875632138135700, 40.70310602011421253, 3.701530608362966657 ) ) ;
#19570 = CARTESIAN_POINT ( 'NONE',  ( 87.86298961015023679, 44.89260222163543546, 6.207647304897661478 ) ) ;
#19571 = DIRECTION ( 'NONE',  ( 0.4999999999999988343, -0.8660254037844393737, 0.000000000000000000 ) ) ;
#19572 = CARTESIAN_POINT ( 'NONE',  ( 153.4361244163197000, 264.8878321249116539, -17.23169627811277493 ) ) ;
#19573 = CARTESIAN_POINT ( 'NONE',  ( 83.27157833596524483, 41.69773053680957275, -4.903519799690783110 ) ) ;
#19574 = CARTESIAN_POINT ( 'NONE',  ( 8.826716519331432309, 169.2365022471902307, 10.00000000000009948 ) ) ;
#19575 = CARTESIAN_POINT ( 'NONE',  ( 145.1264855360895751, 254.5958772461660544, -9.188101187500095079 ) ) ;
#19576 = CARTESIAN_POINT ( 'NONE',  ( 70.57420050861817629, 60.83333136545436304, -14.51089813485932467 ) ) ;
#19577 = CARTESIAN_POINT ( 'NONE',  ( 4.795442299662375341, 20.95586893147752861, 7.433330006724141015 ) ) ;
#19578 = EDGE_LOOP ( 'NONE', ( #4863, #88 ) ) ;
#19580 = VERTEX_POINT ( 'NONE', #36395 ) ;
#19579 = CARTESIAN_POINT ( 'NONE',  ( 85.37572018521500183, 48.32884972269767587, -12.27680401939018040 ) ) ;
#19581 = CARTESIAN_POINT ( 'NONE',  ( -14.23124088391897146, 105.2031859152619120, 10.44627079400605218 ) ) ;
#19582 = PLANE ( 'NONE',  #49676 ) ;
#19583 = CARTESIAN_POINT ( 'NONE',  ( 125.0725847779322351, 243.0177522451418497, -10.00000000000009592 ) ) ;
#19584 = CARTESIAN_POINT ( 'NONE',  ( 156.7469768102917271, 279.2875448729189429, 7.364017834103635529 ) ) ;
#19585 = CARTESIAN_POINT ( 'NONE',  ( 165.5287013238079794, 246.9198946887887871, -1.935065831620633503 ) ) ;
#19586 = CARTESIAN_POINT ( 'NONE',  ( 172.0841359714602561, 280.2593053177052980, 13.89066565685676480 ) ) ;
#19587 = CARTESIAN_POINT ( 'NONE',  ( 86.73131677312836985, 44.08822098498369968, 4.652549913689809635 ) ) ;
#19588 = CARTESIAN_POINT ( 'NONE',  ( 88.19122672570537702, 43.84786592109882264, -2.112715317146043770 ) ) ;
#19589 = EDGE_LOOP ( 'NONE', ( #7530, #32174, #48828, #98998 ) ) ;
#19591 = EDGE_CURVE ( 'NONE', #4961, #13423, #5262, .T. ) ;
#19590 = CARTESIAN_POINT ( 'NONE',  ( 184.9091135615353494, 272.9493583962221805, -17.03684365370855858 ) ) ;
#19592 = CARTESIAN_POINT ( 'NONE',  ( 66.46320885748657759, 68.94986384069260055, 0.01364106734874200727 ) ) ;
#19593 = VERTEX_POINT ( 'NONE', #76425 ) ;
#19594 = CARTESIAN_POINT ( 'NONE',  ( 194.2914079707598773, 293.7378065512926923, -14.23787508785857270 ) ) ;
#19595 = ADVANCED_FACE ( 'NONE', ( #51610 ), #21221, .F. ) ;
#19596 = EDGE_CURVE ( 'NONE', #91708, #27867, #13128, .T. ) ;
#19597 = CARTESIAN_POINT ( 'NONE',  ( 205.0753842767173580, 269.1534704228733403, -3.005433063649942671 ) ) ;
#19598 = B_SPLINE_CURVE_WITH_KNOTS ( 'NONE', 3,
 ( #66892, #20313, #98318, #59783 ),
 .UNSPECIFIED., .F., .F.,
 ( 4, 4 ),
 ( 0.02408851552819888178, 0.03332966919768538122 ),
 .UNSPECIFIED. ) ;
#19599 = CARTESIAN_POINT ( 'NONE',  ( 203.6564843095729316, 277.9036172154027327, -14.39421774622613803 ) ) ;
#19600 = CARTESIAN_POINT ( 'NONE',  ( 149.3883679478359454, 271.8987519849911223, 12.99187507659642371 ) ) ;
#19601 = CARTESIAN_POINT ( 'NONE',  ( 162.0222989613219227, 273.0741124436839868, 15.00522561680813283 ) ) ;
#19603 = CARTESIAN_POINT ( 'NONE',  ( 88.27664040203158891, 44.35691339321036253, 2.453685708849345115 ) ) ;
#19602 = FACE_OUTER_BOUND ( 'NONE', #21894, .T. ) ;
#19604 = CARTESIAN_POINT ( 'NONE',  ( 203.3788045512062865, 270.0447488680846391, 5.971987935157939020 ) ) ;
#19605 = ORIENTED_EDGE ( 'NONE', *, *, #97446, .T. ) ;
#19606 = CARTESIAN_POINT ( 'NONE',  ( 78.02536995280269139, 60.40816079000541095, -15.95887260008864139 ) ) ;
#19607 = ADVANCED_FACE ( 'NONE', ( #97729 ), #43986, .F. ) ;
#19608 = CARTESIAN_POINT ( 'NONE',  ( 189.8237993498458138, 274.2492852631884830, -15.65096844494817674 ) ) ;
#19609 = ADVANCED_FACE ( 'NONE', ( #66314 ), #78824, .F. ) ;
#19610 = DIRECTION ( 'NONE',  ( -0.9879428538673719062, -0.1548189829846212673, 0.000000000000000000 ) ) ;
#19611 = CARTESIAN_POINT ( 'NONE',  ( 192.8132846206021611, 296.6845899933152850, 11.53748932578252351 ) ) ;
#19612 = VECTOR ( 'NONE', #25159, 1000.000000000000114 ) ;
#19613 = CARTESIAN_POINT ( 'NONE',  ( 80.89756888259256584, 43.32073300323414600, -9.969383766040824213 ) ) ;
#19614 = DIRECTION ( 'NONE',  ( -0.000000000000000000, -0.000000000000000000, -1.000000000000000000 ) ) ;
#19615 = CARTESIAN_POINT ( 'NONE',  ( 12.94935828348961593, 178.2833772461660544, -9.188101187500095079 ) ) ;
#19616 = CARTESIAN_POINT ( 'NONE',  ( 107.4543804714665072, 232.8458772461660544, 9.188101187500095079 ) ) ;
#19617 = CARTESIAN_POINT ( 'NONE',  ( 203.0862352702880003, 278.8913175244117610, -15.09542727681365015 ) ) ;
#19618 = CARTESIAN_POINT ( 'NONE',  ( 73.30483403957811106, 69.17932697374328654, -9.895411455429695025 ) ) ;
#19619 = CARTESIAN_POINT ( 'NONE',  ( 181.2455912396057727, 255.1350553628389832, -2.495996851558535123 ) ) ;
#19620 = B_SPLINE_CURVE_WITH_KNOTS ( 'NONE', 3,
 ( #48114, #79056, #18729, #35408, #33941, #34900, #5022, #80564, #41506, #27325 ),
 .UNSPECIFIED., .F., .F.,
 ( 4, 2, 2, 2, 4 ),
 ( 0.001327043042251581763, 0.001752654217620215225, 0.002178265392988848470, 0.002603876568357481932, 0.003029487743726115394 ),
 .UNSPECIFIED. ) ;
#19621 = DIRECTION ( 'NONE',  ( -0.8660254037844377084, -0.5000000000000014433, -0.000000000000000000 ) ) ;
#19622 = CARTESIAN_POINT ( 'NONE',  ( 197.8980529691977779, 285.8775128688180871, 17.80711829255526979 ) ) ;
#19623 = CARTESIAN_POINT ( 'NONE',  ( 155.5085848088033345, 279.2288744083967345, -7.567598119550592806 ) ) ;
#19624 = CARTESIAN_POINT ( 'NONE',  ( 194.8598199529639317, 293.1398868181796615, -15.91766051364927570 ) ) ;
#19625 = CARTESIAN_POINT ( 'NONE',  ( 84.26883830235146888, 50.64164195736777430, 13.79214756291445454 ) ) ;
#19626 = CARTESIAN_POINT ( 'NONE',  ( 75.28183178272522014, 56.04897244165069026, -16.14794119758950686 ) ) ;
#19627 = CARTESIAN_POINT ( 'NONE',  ( 166.2219174074001273, 253.6012899646903236, -13.47457580965214419 ) ) ;
#19628 = CARTESIAN_POINT ( 'NONE',  ( 174.8830188891286639, 265.0810552416202768, -15.58703472796680600 ) ) ;
#19629 = EDGE_CURVE ( 'NONE', #63672, #16186, #1415, .T. ) ;
#19630 = CARTESIAN_POINT ( 'NONE',  ( 79.55186417146283873, 225.9244531367911293, -4.594050593750046652 ) ) ;
#19631 = CARTESIAN_POINT ( 'NONE',  ( 161.3773209892555371, 251.1332761876949746, -14.50043705923759241 ) ) ;
#19632 = CARTESIAN_POINT ( 'NONE',  ( -16.31118285231257303, 103.1745050122371481, 12.72070314857826467 ) ) ;
#19634 = CARTESIAN_POINT ( 'NONE',  ( 199.7305354183539521, 284.7035601629126518, 18.18279833004080004 ) ) ;
#19633 = CARTESIAN_POINT ( 'NONE',  ( 196.3720681610792553, 290.5205960880691691, 16.18360420724715354 ) ) ;
#19635 = CARTESIAN_POINT ( 'NONE',  ( 151.3124059063077311, 268.5662204852269497, -14.45542936000225609 ) ) ;
#19636 = CARTESIAN_POINT ( 'NONE',  ( 173.5541795782666838, 267.4165219661629180, -17.04824448052345431 ) ) ;
#19637 = CARTESIAN_POINT ( 'NONE',  ( 39.23796756512304285, 23.44966523072497466, -2.296566073217252530E-15 ) ) ;
#19638 = CARTESIAN_POINT ( 'NONE',  ( 77.97190755774620641, 49.62147354114171804, -15.34335462392983729 ) ) ;
#19639 = CARTESIAN_POINT ( 'NONE',  ( 85.95130255176152900, 46.56195125003082325, -9.711085333795121954 ) ) ;
#19640 = ORIENTED_EDGE ( 'NONE', *, *, #89508, .F. ) ;
#19641 = CARTESIAN_POINT ( 'NONE',  ( 29.82838080365165112, 20.14754757982091249, -5.678558825948276656 ) ) ;
#19642 = CARTESIAN_POINT ( 'NONE',  ( 173.1278816705146539, 289.7173446917369120, -0.9128981044102878473 ) ) ;
#19643 = CARTESIAN_POINT ( 'NONE',  ( -30.60512737934784155, 93.72946926685976621, 11.88605707516453691 ) ) ;
#19644 = CARTESIAN_POINT ( 'NONE',  ( 191.5982176700465800, 288.2760343549104505, -15.80419025984858195 ) ) ;
#19645 = ORIENTED_EDGE ( 'NONE', *, *, #47301, .F. ) ;
#19646 = B_SPLINE_CURVE_WITH_KNOTS ( 'NONE', 3,
 ( #87425, #17953, #82282, #28517, #97943, #20443, #52805, #5722, #83253, #76149, #29525, #36114, #12855, #5233, #6723, #98942 ),
 .UNSPECIFIED., .F., .F.,
 ( 4, 1, 2, 2, 2, 1, 2, 2, 4 ),
 ( 0.000000000000000000, 0.1250000000000012212, 0.1875000000000016376, 0.2500000000000020539, 0.5000000000000007772, 0.6250000000000014433, 0.6875000000000007772, 0.7500000000000003331, 1.000000000000000000 ),
 .UNSPECIFIED. ) ;
#19647 = CARTESIAN_POINT ( 'NONE',  ( 86.65390046659096868, 47.16758140886460637, 10.54653844973484489 ) ) ;
#19648 = CARTESIAN_POINT ( 'NONE',  ( 74.55668988929480179, 63.24185806647356145, 14.99962697611943163 ) ) ;
#19649 = CARTESIAN_POINT ( 'NONE',  ( 72.60177889808650775, 71.50969142880882146, 5.552899927521425916 ) ) ;
#19650 = CARTESIAN_POINT ( 'NONE',  ( 131.8023238567216708, 260.2365022471903444, 2.944929066748280225E-16 ) ) ;
#19651 = CARTESIAN_POINT ( 'NONE',  ( 157.6036818288543486, 257.6694109429415107, -16.73826488331764395 ) ) ;
#19652 = CARTESIAN_POINT ( 'NONE',  ( 74.82526768066999523, 53.43972195870694719, 16.54088702656758869 ) ) ;
#19653 = VERTEX_POINT ( 'NONE', #95148 ) ;
#19654 = CARTESIAN_POINT ( 'NONE',  ( 169.2826475696182058, 248.6736941890546291, -1.907850670695832473 ) ) ;
#19655 = ORIENTED_EDGE ( 'NONE', *, *, #15629, .F. ) ;
#19656 = CARTESIAN_POINT ( 'NONE',  ( 203.0398866899141126, 278.9715956204779559, 16.57839218037009132 ) ) ;
#19657 = CARTESIAN_POINT ( 'NONE',  ( 83.96259819183102024, 41.85579124667931694, 1.613362698078202540 ) ) ;
#19658 = CARTESIAN_POINT ( 'NONE',  ( 77.22151312697972969, 62.97658066207817740, -15.28167293043454222 ) ) ;
#19660 = EDGE_CURVE ( 'NONE', #60043, #45522, #47852, .T. ) ;
#19659 = ORIENTED_EDGE ( 'NONE', *, *, #64612, .T. ) ;
#19661 = CARTESIAN_POINT ( 'NONE',  ( 72.03640812230088386, 71.62847206889918539, 5.517176230632431455 ) ) ;
#19662 = CARTESIAN_POINT ( 'NONE',  ( 158.6857353490262881, 255.7952392694948287, 17.63394428141803871 ) ) ;
#19663 = CARTESIAN_POINT ( 'NONE',  ( 158.8266160086023149, 257.5512268093053194, -17.29683829744028856 ) ) ;
#19664 = CARTESIAN_POINT ( 'NONE',  ( 88.18084728802688232, 44.43898297010869669, -4.607830584147578179 ) ) ;
#19665 = CARTESIAN_POINT ( 'NONE',  ( -4.731736819106164837, 24.67387208536690224, 10.00000000000000000 ) ) ;
#19666 = CARTESIAN_POINT ( 'NONE',  ( 28.93411276635479368, 38.74646525600392266, 2.839279412974139660 ) ) ;
#19667 = DIRECTION ( 'NONE',  ( 0.000000000000000000, 0.000000000000000000, 1.000000000000000000 ) ) ;
#19669 = EDGE_CURVE ( 'NONE', #51125, #56410, #97167, .T. ) ;
#19668 = CARTESIAN_POINT ( 'NONE',  ( 176.8917175299031896, 289.5346434493817469, -10.53293604869262978 ) ) ;
#19670 = CARTESIAN_POINT ( 'NONE',  ( 82.88421405995129021, 40.62802518055320888, -0.2805589297870617060 ) ) ;
#19671 = EDGE_CURVE ( 'NONE', #12306, #14940, #78632, .T. ) ;
#19672 = ORIENTED_EDGE ( 'NONE', *, *, #26302, .T. ) ;
#19673 = AXIS2_PLACEMENT_3D ( 'NONE', #33494, #56273, #79132 ) ;
#19674 = ORIENTED_EDGE ( 'NONE', *, *, #43566, .T. ) ;
#19675 = CARTESIAN_POINT ( 'NONE',  ( 41.44395331530407844, 35.87878583063845639, -9.188101187500006262 ) ) ;
#19677 = CARTESIAN_POINT ( 'NONE',  ( 165.9227384538158105, 274.2955112070876567, -15.12533405962566846 ) ) ;
#19676 = CARTESIAN_POINT ( 'NONE',  ( 204.7986527064648214, 275.9253235211867263, 14.74587861556245905 ) ) ;
#19678 = CARTESIAN_POINT ( 'NONE',  ( 85.43645318413936707, 48.61927365843763482, 12.47466632846418122 ) ) ;
#19679 = CARTESIAN_POINT ( 'NONE',  ( 155.1376601545389917, 261.9406857754215707, 18.55063430030667959 ) ) ;
#19680 = CARTESIAN_POINT ( 'NONE',  ( 153.6323727466833873, 269.3172676078306154, -15.66543061290010641 ) ) ;
#19681 = CARTESIAN_POINT ( 'NONE',  ( 180.0662822340164269, 262.4007578510376675, -14.24330825748563534 ) ) ;
#19682 = CARTESIAN_POINT ( 'NONE',  ( 164.4860472601134802, 245.7488043397450781, 5.786386706270143954 ) ) ;
#19683 = CARTESIAN_POINT ( 'NONE',  ( 168.9819228013596728, 267.0053382609680170, 16.74345436343837790 ) ) ;
#19684 = CARTESIAN_POINT ( 'NONE',  ( 182.0074952572218194, 256.7411546301147496, 5.145569241165440566 ) ) ;
#19685 = CARTESIAN_POINT ( 'NONE',  ( 90.05242219234915524, 231.9869531367911293, 4.594050593750046652 ) ) ;
#19686 = ORIENTED_EDGE ( 'NONE', *, *, #4007, .T. ) ;
#19687 = CARTESIAN_POINT ( 'NONE',  ( 149.8528230149711646, 271.4847137799879988, 11.79734874491912322 ) ) ;
#19688 = DIRECTION ( 'NONE',  ( 0.000000000000000000, 0.000000000000000000, 1.000000000000000000 ) ) ;
#19689 = CARTESIAN_POINT ( 'NONE',  ( 166.2705977412429661, 279.3148818941612035, -14.08247858441158940 ) ) ;
#19690 = ORIENTED_EDGE ( 'NONE', *, *, #83453, .T. ) ;
#19691 = VERTEX_POINT ( 'NONE', #72832 ) ;
#19692 = CARTESIAN_POINT ( 'NONE',  ( 87.19297534993042120, 45.95771221245824734, -8.700079422534972906 ) ) ;
#19693 = CARTESIAN_POINT ( 'NONE',  ( -49.40214497367342972, 107.8811501326408546, -10.00000000000000000 ) ) ;
#19694 = CARTESIAN_POINT ( 'NONE',  ( 157.3412122618683497, 258.1240215684019290, 16.75554199904894048 ) ) ;
#19695 = CARTESIAN_POINT ( 'NONE',  ( 7.946103921272086090, 26.36126292948893735, 6.180339887498949913 ) ) ;
#19696 = CARTESIAN_POINT ( 'NONE',  ( 206.8383266605359552, 270.5703304059348397, -4.969267838202788390 ) ) ;
#19697 = CARTESIAN_POINT ( 'NONE',  ( 91.05385083941617097, 229.5024278399160949, -9.188101187500093303 ) ) ;
#19698 = VERTEX_POINT ( 'NONE', #80448 ) ;
#19699 = ORIENTED_EDGE ( 'NONE', *, *, #26079, .F. ) ;
#19700 = EDGE_CURVE ( 'NONE', #71493, #65030, #2418, .T. ) ;
#19701 = CARTESIAN_POINT ( 'NONE',  ( 162.6757594134126350, 248.8843148665554281, -10.86406770146305867 ) ) ;
#19702 = ORIENTED_EDGE ( 'NONE', *, *, #30515, .F. ) ;
#19703 = CARTESIAN_POINT ( 'NONE',  ( 194.7838651859529477, 266.2706033605068114, -8.657540068871613315 ) ) ;
#19704 = CARTESIAN_POINT ( 'NONE',  ( 153.4111665582887838, 266.7507244080648547, 16.54171954082816853 ) ) ;
#19705 = CARTESIAN_POINT ( 'NONE',  ( -43.67044039880972406, 70.09354223814025886, -10.00000000000000000 ) ) ;
#19707 = CARTESIAN_POINT ( 'NONE',  ( 69.62288408176668497, 62.35433023048172885, -13.49615336126608867 ) ) ;
#19706 = CARTESIAN_POINT ( 'NONE',  ( 128.5905526607566856, 254.2369531367911293, -4.594050593750048428 ) ) ;
#19708 = CARTESIAN_POINT ( 'NONE',  ( -12.55328564014489245, 176.8927522451419350, 2.944929066748280225E-16 ) ) ;
#19709 = DIRECTION ( 'NONE',  ( 0.2701803667135219689, 0.9628097264997621529, 0.000000000000000000 ) ) ;
#19710 = ORIENTED_EDGE ( 'NONE', *, *, #18872, .F. ) ;
#19711 = CARTESIAN_POINT ( 'NONE',  ( 157.4493702961534609, 257.9366863577731124, 17.30941950273115637 ) ) ;
#19712 = CARTESIAN_POINT ( 'NONE',  ( 82.37580512874393435, 51.26179720552115526, 14.55059045582508404 ) ) ;
#19713 = CARTESIAN_POINT ( 'NONE',  ( 82.18985274614976788, 40.66879167456242783, -3.543735024996086835 ) ) ;
#19714 = EDGE_CURVE ( 'NONE', #83225, #25393, #34329, .T. ) ;
#19715 = CARTESIAN_POINT ( 'NONE',  ( 80.57917228006874666, 43.44270375979753851, 9.528029932415835290 ) ) ;
#19716 = DIRECTION ( 'NONE',  ( 0.000000000000000000, 0.000000000000000000, 1.000000000000000000 ) ) ;
#19717 = CARTESIAN_POINT ( 'NONE',  ( 49.42830306794132866, 81.76213237698443947, -10.00000000000000000 ) ) ;
#19718 = CARTESIAN_POINT ( 'NONE',  ( 195.6983338289388712, 279.8441605301517257, -16.88118927210886255 ) ) ;
#19719 = CYLINDRICAL_SURFACE ( 'NONE', #96493, 17.82106496071139645 ) ;
#19720 = CARTESIAN_POINT ( 'NONE',  ( 80.96506752577832344, 55.91141337780396015, 16.08528190432092231 ) ) ;
#19721 = DIRECTION ( 'NONE',  ( -0.8660254037844387076, -0.4999999999999998890, -0.000000000000000000 ) ) ;
#19722 = CARTESIAN_POINT ( 'NONE',  ( 167.8549298750992307, 249.5183355316891038, 8.029450975726973638 ) ) ;
#19723 = CARTESIAN_POINT ( 'NONE',  ( -40.14225747417106760, 26.13077817479420872, 177.5919119679930134 ) ) ;
#19724 = CARTESIAN_POINT ( 'NONE',  ( 163.2742264920156572, 247.8477394797576778, -9.850275379362519956 ) ) ;
#19725 = LINE ( 'NONE', #3528, #91594 ) ;
#19726 = EDGE_CURVE ( 'NONE', #16763, #38435, #69301, .T. ) ;
#19727 = PRESENTATION_STYLE_ASSIGNMENT (( #66307 ) ) ;
#19728 = CARTESIAN_POINT ( 'NONE',  ( 74.22259355549384452, 55.16627323567375640, 16.60417442601049842 ) ) ;
#19729 = CARTESIAN_POINT ( 'NONE',  ( 165.9091197491159164, 246.2627970730538323, -2.747640711776688338 ) ) ;
#19730 = CARTESIAN_POINT ( 'NONE',  ( 41.22093855302743748, 25.92755873383629250, 6.180339887498953466 ) ) ;
#19731 = CARTESIAN_POINT ( 'NONE',  ( 80.87487590722817288, 55.61906553629490446, -16.40244339227437820 ) ) ;
#19733 = DIRECTION ( 'NONE',  ( -0.6384778167143362326, 0.7696402260561061581, 0.000000000000000000 ) ) ;
#19732 =( BOUNDED_CURVE ( )  B_SPLINE_CURVE ( 2, ( #2166, #95413, #34069, #88817, #88313, #72067, #2667, #40635, #25969 ),
 .UNSPECIFIED., .F., .T. ) 
 B_SPLINE_CURVE_WITH_KNOTS ( ( 3, 2, 2, 2, 3 ),
 ( 0.3104838709677419373, 0.3118279569892473124, 0.3145161290322580627, 0.3172043010752688130, 0.3185483870967741882 ),
 .UNSPECIFIED. ) 
 CURVE ( )  GEOMETRIC_REPRESENTATION_ITEM ( )  RATIONAL_B_SPLINE_CURVE ( ( 0.9330127018922194093, 0.9330127018922194093, 1.000000000000000000, 0.8660254037844387076, 1.000000000000000000, 0.8660254037844387076, 1.000000000000000000, 0.9330127018922194093, 0.9330127018922194093 ) ) 
 REPRESENTATION_ITEM ( '' )  );
#19734 = CARTESIAN_POINT ( 'NONE',  ( 159.6773882672717946, 272.2419546184144110, -14.76404975350964044 ) ) ;
#19735 = CARTESIAN_POINT ( 'NONE',  ( 81.86168173829938155, 43.19759374944588615, -8.265271606104395374 ) ) ;
#19736 = CARTESIAN_POINT ( 'NONE',  ( 207.1211793645798878, 271.9025893473983047, -6.294110402770905388 ) ) ;
#19737 = CARTESIAN_POINT ( 'NONE',  ( 10.51348828746337638, 183.0024278399160949, -9.188101187500093303 ) ) ;
#19738 = LINE ( 'NONE', #61067, #66290 ) ;
#19739 = EDGE_LOOP ( 'NONE', ( #48544, #6554, #63263, #17690 ) ) ;
#19740 = CARTESIAN_POINT ( 'NONE',  ( 87.35606880162971777, 45.77061481740688720, 8.290963297571634527 ) ) ;
#19741 = DIRECTION ( 'NONE',  ( -0.9515606131578174809, -0.3074612162317687525, 0.000000000000000000 ) ) ;
#19742 = CARTESIAN_POINT ( 'NONE',  ( 40.40883878445526278, 23.73415679381825782, -6.890680421881970419E-14 ) ) ;
#19743 = CARTESIAN_POINT ( 'NONE',  ( 38.60536087060361154, 193.0958772461660544, -9.188101187500095079 ) ) ;
#19744 = CARTESIAN_POINT ( 'NONE',  ( 200.6800100461949228, 283.0590218669948399, 18.32402613046234308 ) ) ;
#19745 = CARTESIAN_POINT ( 'NONE',  ( 190.9586609929293104, 299.8968923453624598, -4.970176667899034229 ) ) ;
#19746 = CARTESIAN_POINT ( 'NONE',  ( 32.56963740530460427, 41.73705186507756082, -3.090169943749475845 ) ) ;
#19747 = CARTESIAN_POINT ( 'NONE',  ( 182.4004271739244700, 284.1903799708203451, 16.39187655311515002 ) ) ;
#19748 = CARTESIAN_POINT ( 'NONE',  ( 146.5046981847821428, 276.8934145268504494, 0.02269072295920678689 ) ) ;
#19749 = CARTESIAN_POINT ( 'NONE',  ( 46.22371820283662203, 112.7232458147606451, -10.00000000000000000 ) ) ;
#19750 = CARTESIAN_POINT ( 'NONE',  ( 71.55070063111804757, 67.78110124390339308, -10.19286156064286786 ) ) ;
#19751 = CARTESIAN_POINT ( 'NONE',  ( 86.98710364365733483, 45.90732384579192171, -8.137934770119690242 ) ) ;
#19752 = DIRECTION ( 'NONE',  ( 0.000000000000000000, 0.000000000000000000, 1.000000000000000000 ) ) ;
#19753 = DIRECTION ( 'NONE',  ( 0.2471055264905481497, -0.9689885751534065284, 0.000000000000000000 ) ) ;
#19754 = CARTESIAN_POINT ( 'NONE',  ( 87.69076027921141758, 45.30224151825790813, -7.205911438339954955 ) ) ;
#19755 = CARTESIAN_POINT ( 'NONE',  ( 91.02696109520442747, 213.3615022471902023, 5.000000000000051514 ) ) ;
#19756 = CARTESIAN_POINT ( 'NONE',  ( 74.91658594121764736, 53.18802753783876369, 16.51533261098013128 ) ) ;
#19757 = LINE ( 'NONE', #64341, #20730 ) ;
#19758 = ORIENTED_EDGE ( 'NONE', *, *, #16554, .T. ) ;
#19759 = CARTESIAN_POINT ( 'NONE',  ( 41.36564329728401646, 200.8149278399160664, -9.188101187500095079 ) ) ;
#19760 = EDGE_LOOP ( 'NONE', ( #49969, #90731, #63613, #81526 ) ) ;
#19761 = CARTESIAN_POINT ( 'NONE',  ( -10.95801343888480339, 85.52545552628633629, 14.52632409138724512 ) ) ;
#19762 = CARTESIAN_POINT ( 'NONE',  ( 147.4811722709131914, 275.2021117973970377, 3.890385073228495916 ) ) ;
#19763 = CARTESIAN_POINT ( 'NONE',  ( 67.39535085695571581, 67.25041444790150535, -8.623144929768267630 ) ) ;
#19764 = ORIENTED_EDGE ( 'NONE', *, *, #65996, .F. ) ;
#19765 = CARTESIAN_POINT ( 'NONE',  ( 171.3468567556325297, 286.5349138614378148, 7.626544187982161382 ) ) ;
#19766 = CARTESIAN_POINT ( 'NONE',  ( 164.9586510554008782, 244.9302305544571823, -1.717556444319656039 ) ) ;
#19767 = DIRECTION ( 'NONE',  ( 0.2649596321166021728, -0.4589235447807153423, -0.8480480961564252906 ) ) ;
#19768 = CARTESIAN_POINT ( 'NONE',  ( 29.64555348686941016, 32.51421378149920827, -9.188101187500004485 ) ) ;
#19769 = CARTESIAN_POINT ( 'NONE',  ( 187.4166251561426293, 263.4339899954952102, 11.64397722261905166 ) ) ;
#19770 = CARTESIAN_POINT ( 'NONE',  ( 86.46983487695372617, 47.48951387118550116, -10.44352480544961637 ) ) ;
#19771 = CARTESIAN_POINT ( 'NONE',  ( 171.5786706455526485, 255.3236219728620711, 12.51996115914846364 ) ) ;
#19773 = VERTEX_POINT ( 'NONE', #98618 ) ;
#19772 = VECTOR ( 'NONE', #58847, 1000.000000000000114 ) ;
#19774 = CARTESIAN_POINT ( 'NONE',  ( 9.881553883097156543, 27.74646525600388713, 2.839279412974139660 ) ) ;
#19775 = CARTESIAN_POINT ( 'NONE',  ( 22.01921768174555893, 36.21091486745860522, -1.111400068045478839E-16 ) ) ;
#19776 = CARTESIAN_POINT ( 'NONE',  ( 173.8867782663501487, 254.5903856161964995, 8.266592030789951195 ) ) ;
#19777 = FACE_OUTER_BOUND ( 'NONE', #99183, .T. ) ;
#19778 = ORIENTED_EDGE ( 'NONE', *, *, #36453, .T. ) ;
#19780 = EDGE_CURVE ( 'NONE', #82018, #55876, #67326, .T. ) ;
#19779 = CARTESIAN_POINT ( 'NONE',  ( 182.3393106838078666, 284.1038920326962511, 14.96556368581471830 ) ) ;
#19781 = CYLINDRICAL_SURFACE ( 'NONE', #96989, 17.82106496071139645 ) ;
#19782 = CARTESIAN_POINT ( 'NONE',  ( -17.42236680055705023, 149.2012482093457777, 0.000000000000000000 ) ) ;
#19783 = ADVANCED_FACE ( 'NONE', ( #60068 ), #99104, .T. ) ;
#19784 = VERTEX_POINT ( 'NONE', #66199 ) ;
#19785 = CARTESIAN_POINT ( 'NONE',  ( 207.4218731373931632, 271.3817724553659332, -5.249531240730909154 ) ) ;
#19786 = CARTESIAN_POINT ( 'NONE',  ( 196.6288634187112052, 290.0758136547079289, -16.31544900032282186 ) ) ;
#19787 = EDGE_LOOP ( 'NONE', ( #8, #62217, #80012, #53185 ) ) ;
#19788 = FACE_OUTER_BOUND ( 'NONE', #39999, .T. ) ;
#19789 = EDGE_CURVE ( 'NONE', #28368, #62719, #83426, .T. ) ;
#19790 = CARTESIAN_POINT ( 'NONE',  ( -22.42236680055709641, 157.8615022471902591, 0.000000000000000000 ) ) ;
#19791 = LINE ( 'NONE', #81611, #59615 ) ;
#19792 = CARTESIAN_POINT ( 'NONE',  ( 78.17513785305828833, 61.62242163703883335, -16.13566992787025356 ) ) ;
#19794 = ADVANCED_FACE ( 'NONE', ( #44871 ), #12510, .F. ) ;
#19793 = CARTESIAN_POINT ( 'NONE',  ( 198.0003830832412461, 286.7757149588804850, 16.94998330638511419 ) ) ;
#19795 = CARTESIAN_POINT ( 'NONE',  ( 110.7287787077026451, 243.9244531367911293, -4.594050593750046652 ) ) ;
#19796 = CARTESIAN_POINT ( 'NONE',  ( -22.42236680055709641, 157.8615022471902591, 0.000000000000000000 ) ) ;
#19797 = CARTESIAN_POINT ( 'NONE',  ( 66.16250339235085676, 220.5530062829863027, -4.648177544792955347E-16 ) ) ;
#19798 = ORIENTED_EDGE ( 'NONE', *, *, #89326, .F. ) ;
#19799 = CARTESIAN_POINT ( 'NONE',  ( 207.5792673731680793, 271.1091576421853233, 2.359198794924813214 ) ) ;
#19800 = VERTEX_POINT ( 'NONE', #42867 ) ;
#19801 = CARTESIAN_POINT ( 'NONE',  ( 40.64525884627276042, 24.26216523072497466, -2.296566073217252530E-15 ) ) ;
#19802 = FACE_BOUND ( 'NONE', #2842, .T. ) ;
#19803 = CARTESIAN_POINT ( 'NONE',  ( -72.48190909937208914, 49.06123820388767598, 10.00000000000000000 ) ) ;
#19804 = CARTESIAN_POINT ( 'NONE',  ( 74.35571174875622091, 222.9244531367911293, -4.594050593750046652 ) ) ;
#19805 = DIRECTION ( 'NONE',  ( -0.9963824715083250405, 0.08498217737244646852, 0.000000000000000000 ) ) ;
#19806 = CARTESIAN_POINT ( 'NONE',  ( 174.1477614194014336, 281.2887866680289335, 15.61518462008415042 ) ) ;
#19807 = CARTESIAN_POINT ( 'NONE',  ( 154.9226727788713731, 262.3130548330639726, 18.22497199616848818 ) ) ;
#19808 = CARTESIAN_POINT ( 'NONE',  ( 175.8169107895047034, 278.1165438142045332, 15.85296464203584499 ) ) ;
#19809 = VERTEX_POINT ( 'NONE', #43879 ) ;
#19810 = CARTESIAN_POINT ( 'NONE',  ( 73.36337205780706938, 63.47506113005868400, -14.09265201955449598 ) ) ;
#19811 = CARTESIAN_POINT ( 'NONE',  ( -35.89898968889472997, 24.97633462685643124, -10.00000000000000000 ) ) ;
#19812 = CARTESIAN_POINT ( 'NONE',  ( 203.5258219653775313, 278.1299310341851765, -16.21052911601769608 ) ) ;
#19813 = EDGE_LOOP ( 'NONE', ( #9298, #93431, #40820, #18946 ) ) ;
#19814 = CARTESIAN_POINT ( 'NONE',  ( 148.1803270710863103, 273.9911401611413453, 8.879999584410908753 ) ) ;
#19815 = CARTESIAN_POINT ( 'NONE',  ( -12.62545442379354554, 163.5177522451418781, -10.00000000000009592 ) ) ;
#19816 = CARTESIAN_POINT ( 'NONE',  ( 207.5785076975260779, 271.1104734389944042, -6.824813054587777650 ) ) ;
#19817 = CARTESIAN_POINT ( 'NONE',  ( 206.4728825436989155, 270.6102857768882473, 2.384334928751958405 ) ) ;
#19818 = DIRECTION ( 'NONE',  ( -0.000000000000000000, 0.000000000000000000, -1.000000000000000000 ) ) ;
#19819 = DIRECTION ( 'NONE',  ( -0.2877784213863714968, 0.9576970189910627429, 0.000000000000000000 ) ) ;
#19820 = CARTESIAN_POINT ( 'NONE',  ( 206.5508451493652444, 272.8904371854448527, 11.05407534521577695 ) ) ;
#19821 = SURFACE_STYLE_FILL_AREA ( #89272 ) ;
#19822 = CARTESIAN_POINT ( 'NONE',  ( 164.3602934812760452, 245.9666162739349318, -7.171958108566009571 ) ) ;
#19823 = CARTESIAN_POINT ( 'NONE',  ( 130.8102634016018442, 237.1423013555409796, -4.594050593750043987 ) ) ;
#19824 = ORIENTED_EDGE ( 'NONE', *, *, #67897, .T. ) ;
#19825 = CARTESIAN_POINT ( 'NONE',  ( 82.93017357788667709, 175.3855496052738374, 36.50000000000000000 ) ) ;
#19826 = CARTESIAN_POINT ( 'NONE',  ( 82.63733999249467388, 228.5177522451419350, 5.000000000000046185 ) ) ;
#19827 = CARTESIAN_POINT ( 'NONE',  ( 203.1526193585190470, 278.7763369107815379, -16.67658907091021447 ) ) ;
#19828 = CARTESIAN_POINT ( 'NONE',  ( 164.3010377730689981, 246.0692501711882869, 7.247566249275159578 ) ) ;
#19829 = CARTESIAN_POINT ( 'NONE',  ( 74.71934731310142297, 60.78794131512849219, 15.41883525433982527 ) ) ;
#19830 = CARTESIAN_POINT ( 'NONE',  ( -61.61048871844075592, 38.59675092633816007, -10.00000000000000000 ) ) ;
#19831 = EDGE_LOOP ( 'NONE', ( #60997, #94246, #3259, #953 ) ) ;
#19832 = CARTESIAN_POINT ( 'NONE',  ( 76.65664154646117368, 55.40719475734993438, 16.15617875289344596 ) ) ;
#19833 = CARTESIAN_POINT ( 'NONE',  ( 72.48661302258760486, 71.52526770760661634, -5.337229783571229014 ) ) ;
#19834 = DIRECTION ( 'NONE',  ( -0.5888918169447047157, 0.8082118706970125022, 0.000000000000000000 ) ) ;
#19835 = CARTESIAN_POINT ( 'NONE',  ( 164.3625597711517230, 265.6729452914248668, -17.82104740451561753 ) ) ;
#19836 = CARTESIAN_POINT ( 'NONE',  ( -30.04356256989597185, 94.88921800892812541, 36.50000000000000000 ) ) ;
#19837 = CARTESIAN_POINT ( 'NONE',  ( 195.3688130124408531, 263.4455885837858204, 0.8642261836844156164 ) ) ;
#19838 = CARTESIAN_POINT ( 'NONE',  ( -13.51183432020139819, 142.4280072687214442, 0.000000000000000000 ) ) ;
#19839 =( REPRESENTATION_RELATIONSHIP ('NONE','NONE', #67038, #94304 ) REPRESENTATION_RELATIONSHIP_WITH_TRANSFORMATION ( #99374 )SHAPE_REPRESENTATION_RELATIONSHIP( ) );
#19840 = CARTESIAN_POINT ( 'NONE',  ( 69.55672757425234920, 70.47494305999370567, 2.963892479765599663 ) ) ;
#19841 = B_SPLINE_CURVE_WITH_KNOTS ( 'NONE', 3,
 ( #94875, #93379, #25437, #55809, #23931, #86802, #71061, #70535, #86301, #54829, #1662, #85813, #16341, #7744, #32546, #63445, #79187, #9764, #40625, #71561, #31035, #80690, #65434, #35023, #19371, #87816, #97360, #42128, #12248, #11752, #58324, #80185, #64444, #49247, #96376, #35531, #56830, #25959 ),
 .UNSPECIFIED., .F., .F.,
 ( 4, 2, 2, 2, 2, 2, 2, 2, 2, 2, 2, 2, 2, 2, 2, 2, 2, 2, 4 ),
 ( 0.0009274247721126415529, 0.001022860814635683565, 0.001118296857158725469, 0.001309168942204771329, 0.001690913112296865868, 0.002454401452480929179, 0.003981378132849053633, 0.004744866473033152940, 0.005126610643125203461, 0.005317482728171264716, 0.005412918770694336544, 0.005508354813217409239, 0.005556072834478982016, 0.005603790855740555660, 0.005699226898263672590, 0.005890098983310050433, 0.006271843153402804384, 0.006653587323495560070, 0.007035331493588314021 ),
 .UNSPECIFIED. ) ;
#19842 = EDGE_CURVE ( 'NONE', #99166, #99285, #85288, .T. ) ;
#19843 = VECTOR ( 'NONE', #81592, 1000.000000000000000 ) ;
#19844 = CARTESIAN_POINT ( 'NONE',  ( 192.4434358697015739, 296.8713576677063770, 11.08430769131553895 ) ) ;
#19845 = AXIS2_PLACEMENT_3D ( 'NONE', #38551, #92795, #47152 ) ;
#19846 = B_SPLINE_SURFACE_WITH_KNOTS ( 'NONE', 3, 1, ( 
 ( #73894, #96729 ),
 ( #13102, #58663 ),
 ( #4483, #20197 ),
 ( #66288, #89635 ),
 ( #11606, #3510 ),
 ( #96226, #65285 ),
 ( #28272, #51067 ),
 ( #59148, #19707 ),
 ( #74413, #4998 ),
 ( #90118, #51581 ),
 ( #67272, #28780 ),
 ( #82538, #43962 ),
 ( #74900, #65771 ),
 ( #90633, #36367 ),
 ( #27294, #98199 ),
 ( #73399, #59661 ),
 ( #34387, #89161 ),
 ( #21196, #3985 ),
 ( #52075, #26790 ),
 ( #81043, #88650 ),
 ( #19216, #50086 ),
 ( #42465, #34871 ),
 ( #15550, #60154 ),
 ( #92130, #54543 ),
 ( #99688, #13589 ),
 ( #14584, #53562 ),
 ( #85006, #83518 ),
 ( #75905, #54048 ),
 ( #30271, #14080 ),
 ( #84514, #91118 ),
 ( #61661, #374 ) ),
 .UNSPECIFIED., .F., .F., .F.,
 ( 4, 3, 3, 3, 3, 3, 3, 3, 3, 3, 4 ),
 ( 2, 2 ),
 ( 0.000000000000000000, 0.1122669598086922238, 0.2243161639709877753, 0.3396355846219357155, 0.4553962076585463259, 0.5677860799922646029, 0.6749047109689955137, 0.7773884377078522645, 0.8775581155834401015, 0.9782364162378043293, 1.000000000000000000 ),
 ( 0.000000000000000000, 1.000000000000000000 ),
 .UNSPECIFIED. ) ;
#19847 = CARTESIAN_POINT ( 'NONE',  ( 12.81113585708611957, 26.13478043621386959, 8.090169943749478065 ) ) ;
#19848 = CARTESIAN_POINT ( 'NONE',  ( 190.0445576990143195, 301.4801656937889902, 4.140328216824785912 ) ) ;
#19849 = CARTESIAN_POINT ( 'NONE',  ( 81.59834852019750429, 41.61476123368048263, 5.652816389801710528 ) ) ;
#19850 = CARTESIAN_POINT ( 'NONE',  ( 169.4526480808381450, 285.1936639049519044, -7.980504902024926572 ) ) ;
#19851 = CARTESIAN_POINT ( 'NONE',  ( 203.1988451939495235, 268.1137895879253961, -4.180311155435266990 ) ) ;
#19852 = CARTESIAN_POINT ( 'NONE',  ( 193.4499168429655924, 288.7348347244117690, 16.02611495321234258 ) ) ;
#19853 = CARTESIAN_POINT ( 'NONE',  ( 131.5677753063155251, 246.7677522451418497, 10.00000000000009592 ) ) ;
#19854 = CARTESIAN_POINT ( 'NONE',  ( 183.2152767118556085, 278.9959196896102753, 17.30803618819086864 ) ) ;
#19855 = ORIENTED_EDGE ( 'NONE', *, *, #6142, .T. ) ;
#19856 = EDGE_CURVE ( 'NONE', #48417, #92799, #90032, .T. ) ;
#19858 = CARTESIAN_POINT ( 'NONE',  ( 196.3021893095863959, 290.6416298092292436, 17.45656988653421138 ) ) ;
#19857 = CIRCLE ( 'NONE', #76480, 70.00000000000001421 ) ;
#19859 = CARTESIAN_POINT ( 'NONE',  ( 190.5674408456512765, 300.5745055173924811, -0.9151048603553563199 ) ) ;
#19860 = CARTESIAN_POINT ( 'NONE',  ( -8.322217149083147802, 159.8768266524159856, -9.188101187500093303 ) ) ;
#19861 = CARTESIAN_POINT ( 'NONE',  ( 39.44458330234355969, 184.3923013555410080, 4.594050593750050204 ) ) ;
#19862 = CARTESIAN_POINT ( 'NONE',  ( 175.7888789257961832, 257.1435258631530019, -10.56737597936652584 ) ) ;
#19863 = CARTESIAN_POINT ( 'NONE',  ( 16.98118013718471886, 32.73705186507753950, -3.090169943749475845 ) ) ;
#19864 = CARTESIAN_POINT ( 'NONE',  ( 85.69812724468053489, 48.75358317490552196, 11.98593812281557902 ) ) ;
#19865 = CARTESIAN_POINT ( 'NONE',  ( 205.2937235227012707, 275.0678357141204629, -12.80017165135291535 ) ) ;
#19866 = CARTESIAN_POINT ( 'NONE',  ( 192.2926338600964584, 292.9423151340307641, -14.26349443232093961 ) ) ;
#19867 = CARTESIAN_POINT ( 'NONE',  ( 147.5693121967435957, 275.0494489676833041, 4.210973343677100189 ) ) ;
#19868 = CARTESIAN_POINT ( 'NONE',  ( 73.85836482019932703, 55.05148726086135014, -16.60244221165485357 ) ) ;
#19870 = CARTESIAN_POINT ( 'NONE',  ( 63.51261232558833569, 214.1427522451419065, 10.00000000000009237 ) ) ;
#19869 = LINE ( 'NONE', #81201, #83367 ) ;
#19871 = CARTESIAN_POINT ( 'NONE',  ( 75.19642846017637794, 67.02491989442394527, 12.74302411039618832 ) ) ;
#19872 = DIRECTION ( 'NONE',  ( -0.9994626398093611197, -0.03277852384265240310, 0.000000000000000000 ) ) ;
#19873 = CARTESIAN_POINT ( 'NONE',  ( 150.2452556859942376, 270.4145788861182496, 14.49525683977126533 ) ) ;
#19874 = CARTESIAN_POINT ( 'NONE',  ( 38.27158024800227309, 206.2365022471903160, 2.944929066748280225E-16 ) ) ;
#19875 = CARTESIAN_POINT ( 'NONE',  ( 182.1377600559704035, 291.7984100848548792, 9.332931847923262580 ) ) ;
#19876 = CARTESIAN_POINT ( 'NONE',  ( 163.2442700311756596, 247.8996255919473697, 11.14021925110252020 ) ) ;
#19877 = CARTESIAN_POINT ( 'NONE',  ( -1.935626891937928917, 175.8149278399160664, 9.188101187500093303 ) ) ;
#19878 = CARTESIAN_POINT ( 'NONE',  ( 168.1818879105967710, 286.4694436765728938, 4.832144866178585296 ) ) ;
#19879 = CARTESIAN_POINT ( 'NONE',  ( 80.58426559298514746, 57.69291223751457665, -16.24425291953823347 ) ) ;
#19880 = CARTESIAN_POINT ( 'NONE',  ( 78.70582684749655300, 59.88532474210303747, 16.12216508957796890 ) ) ;
#19881 = CARTESIAN_POINT ( 'NONE',  ( 32.24243340009443415, 30.56628583063843152, 9.188101187500006262 ) ) ;
#19882 = CARTESIAN_POINT ( 'NONE',  ( 165.0308887387863876, 244.8051112166122891, 1.948365933089477808 ) ) ;
#19883 = CARTESIAN_POINT ( 'NONE',  ( 183.1920691253360474, 278.9237338132715536, 16.88618025906524167 ) ) ;
#19884 = CARTESIAN_POINT ( 'NONE',  ( -58.02784037451009880, 34.21088073648085981, 10.00000000000000000 ) ) ;
#19885 = CARTESIAN_POINT ( 'NONE',  ( 43.11943305279750405, 25.86426979415093186, -3.090169943749474069 ) ) ;
#19886 = DIRECTION ( 'NONE',  ( -1.000000000000000000, 0.000000000000000000, 0.000000000000000000 ) ) ;
#19887 = CARTESIAN_POINT ( 'NONE',  ( 13.54711677929152636, 28.79752408145592213, -5.678558825948271327 ) ) ;
#19888 = CARTESIAN_POINT ( 'NONE',  ( 71.94676095904020485, 72.61122666528670777, 1.254485733363759792 ) ) ;
#19889 = CARTESIAN_POINT ( 'NONE',  ( 82.25327158856319443, 54.24549761180711016, 15.63371342117970642 ) ) ;
#19890 = DIRECTION ( 'NONE',  ( 0.8660254037844373753, 0.5000000000000021094, 0.000000000000000000 ) ) ;
#19891 = CARTESIAN_POINT ( 'NONE',  ( 153.2378184573828150, 277.6881940163261788, -5.169838279812049464 ) ) ;
#19892 = ORIENTED_EDGE ( 'NONE', *, *, #18327, .T. ) ;
#19893 = CARTESIAN_POINT ( 'NONE',  ( 112.8139755218393532, 224.3932355074535394, -2.679491924311248496 ) ) ;
#19894 = CARTESIAN_POINT ( 'NONE',  ( 206.5237403681858552, 272.9373840435757188, -10.81420335655575116 ) ) ;
#19895 = EDGE_CURVE ( 'NONE', #16991, #27498, #41485, .T. ) ;
#19896 = DIRECTION ( 'NONE',  ( 1.110223024625156343E-15, -1.000000000000000000, 0.000000000000000000 ) ) ;
#19897 = ORIENTED_EDGE ( 'NONE', *, *, #43172, .T. ) ;
#19898 = CARTESIAN_POINT ( 'NONE',  ( 153.0070714074088016, 265.6309737354857248, 17.74442213480098474 ) ) ;
#19899 = CARTESIAN_POINT ( 'NONE',  ( 82.81737761406506593, 40.62361263874299055, 0.9906565629087065172 ) ) ;
#19900 = CARTESIAN_POINT ( 'NONE',  ( 66.76973844028468363, 68.39731140017956079, 4.469926681468478158 ) ) ;
#19901 = CARTESIAN_POINT ( 'NONE',  ( 87.44971815361896006, 45.51302063199200632, 7.049767141111613178 ) ) ;
#19902 = ORIENTED_EDGE ( 'NONE', *, *, #40211, .F. ) ;
#19903 = VERTEX_POINT ( 'NONE', #82456 ) ;
#19905 = CARTESIAN_POINT ( 'NONE',  ( 163.7136804588959649, 247.0865828815331042, 6.783386239354816105 ) ) ;
#19904 = DIRECTION ( 'NONE',  ( -1.000000000000000000, 0.000000000000000000, 0.000000000000000000 ) ) ;
#19906 = CARTESIAN_POINT ( 'NONE',  ( 192.8010417052266234, 296.7057953447782097, 12.10593424093686643 ) ) ;
#19907 = ORIENTED_EDGE ( 'NONE', *, *, #13054, .F. ) ;
#19908 = CARTESIAN_POINT ( 'NONE',  ( 80.07812099633126479, 57.44764983040322193, -16.59488970948941500 ) ) ;
#19909 = CARTESIAN_POINT ( 'NONE',  ( 177.7843144939522517, 263.4642486473027816, 15.38512530093995956 ) ) ;
#19910 = ORIENTED_EDGE ( 'NONE', *, *, #24676, .T. ) ;
#19912 = EDGE_CURVE ( 'NONE', #37567, #56511, #89550, .T. ) ;
#19911 = CYLINDRICAL_SURFACE ( 'NONE', #91177, 10.00000000000001066 ) ;
#19913 = CARTESIAN_POINT ( 'NONE',  ( 82.09975393820661793, 49.29335735647264016, -13.66301205482166381 ) ) ;
#19914 = AXIS2_PLACEMENT_3D ( 'NONE', #39353, #94118, #56052 ) ;
#19915 = CARTESIAN_POINT ( 'NONE',  ( 81.24979600617606934, 43.19334784728703625, 9.575909627378866418 ) ) ;
#19916 = ORIENTED_EDGE ( 'NONE', *, *, #8510, .T. ) ;
#19917 = CARTESIAN_POINT ( 'NONE',  ( 202.9887705438587773, 268.0958564390360834, 2.511777696352780254 ) ) ;
#19918 = CARTESIAN_POINT ( 'NONE',  ( 166.1715776501828543, 274.1767206847245006, -15.18696448220450534 ) ) ;
#19919 = DIRECTION ( 'NONE',  ( 0.000000000000000000, 0.000000000000000000, 1.000000000000000000 ) ) ;
#19920 = ORIENTED_EDGE ( 'NONE', *, *, #25233, .F. ) ;
#19921 = CARTESIAN_POINT ( 'NONE',  ( 175.9279835239203180, 278.1198263924018192, -15.71133404561638969 ) ) ;
#19922 = CARTESIAN_POINT ( 'NONE',  ( 169.1667396529449263, 261.6176701127336628, -15.97132217662409381 ) ) ;
#19923 = AXIS2_PLACEMENT_3D ( 'NONE', #64467, #23953, #32568 ) ;
#19924 = EDGE_LOOP ( 'NONE', ( #11337, #60085, #87555, #89998 ) ) ;
#19925 = CARTESIAN_POINT ( 'NONE',  ( 158.7680870133227700, 267.7863907316387326, -16.24686683248629038 ) ) ;
#19926 = ORIENTED_EDGE ( 'NONE', *, *, #29524, .T. ) ;
#19927 = FACE_OUTER_BOUND ( 'NONE', #72898, .T. ) ;
#19928 = EDGE_LOOP ( 'NONE', ( #90848, #23230, #28709, #12809 ) ) ;
#19929 = CARTESIAN_POINT ( 'NONE',  ( 158.9949979552652621, 259.7205239824713203, 16.79231500460955573 ) ) ;
#19930 = CARTESIAN_POINT ( 'NONE',  ( 193.2853656402591014, 295.8669216819805001, 14.14801835725165091 ) ) ;
#19931 = CARTESIAN_POINT ( 'NONE',  ( 188.6236154063645643, 298.5688366442050210, -4.386709406375833176 ) ) ;
#19932 = FACE_OUTER_BOUND ( 'NONE', #9355, .T. ) ;
#19933 = CARTESIAN_POINT ( 'NONE',  ( 192.6773196027083372, 296.9200883123592689, 11.15745042875121484 ) ) ;
#19934 = CARTESIAN_POINT ( 'NONE',  ( 177.6619337662969258, 291.1046247341686239, 6.079945615520735203 ) ) ;
#19935 = CARTESIAN_POINT ( 'NONE',  ( 196.9886126479698305, 289.4527097116482537, -17.08115356036521604 ) ) ;
#19936 = VECTOR ( 'NONE', #76688, 1000.000000000000000 ) ;
#19937 = ORIENTED_EDGE ( 'NONE', *, *, #48568, .F. ) ;
#19938 = CARTESIAN_POINT ( 'NONE',  ( 77.81781567708489433, 56.70989197899351097, -16.20277462095411281 ) ) ;
#19939 = CARTESIAN_POINT ( 'NONE',  ( 173.9076247008792393, 277.9417859016587045, -16.84130823774900776 ) ) ;
#19941 = ORIENTED_EDGE ( 'NONE', *, *, #36136, .F. ) ;
#19940 = DIRECTION ( 'NONE',  ( 0.4999999999999992784, -0.8660254037844390407, 0.000000000000000000 ) ) ;
#19942 = ORIENTED_EDGE ( 'NONE', *, *, #65876, .F. ) ;
#19943 = CARTESIAN_POINT ( 'NONE',  ( 184.7289685188066528, 275.5467696374773254, 16.39282505805186574 ) ) ;
#19944 = CARTESIAN_POINT ( 'NONE',  ( 171.5470852890824744, 259.4466874145439306, -13.88548382802202319 ) ) ;
#19945 = CARTESIAN_POINT ( 'NONE',  ( 187.1602505332256214, 299.4194354331692693, 0.8643973265446426302 ) ) ;
#19946 = CARTESIAN_POINT ( 'NONE',  ( 173.4026771546767804, 273.2456497557084845, -17.70700034978624515 ) ) ;
#19947 = CARTESIAN_POINT ( 'NONE',  ( 159.9741193159504746, 253.5636927791250059, -15.97707229450967503 ) ) ;
#19948 = CARTESIAN_POINT ( 'NONE',  ( 190.3209390717459542, 301.0014591139522508, -1.435067967167677594 ) ) ;
#19949 = ORIENTED_EDGE ( 'NONE', *, *, #37503, .F. ) ;
#19950 = CARTESIAN_POINT ( 'NONE',  ( 169.4525966125490584, 254.8330656995144636, -11.66724334959756604 ) ) ;
#19951 = CARTESIAN_POINT ( 'NONE',  ( 83.15864659133335124, 42.41990866257129511, 6.708876870822152227 ) ) ;
#19952 = CARTESIAN_POINT ( 'NONE',  ( 128.9696990949622091, 245.2677522451418497, 10.00000000000009592 ) ) ;
#19953 = CARTESIAN_POINT ( 'NONE',  ( 164.3138894970802824, 246.0469903322357368, -2.642126690130961020 ) ) ;
#19954 = CARTESIAN_POINT ( 'NONE',  ( 22.88158713136840561, 194.0177522451419350, 5.000000000000046185 ) ) ;
#19955 = CARTESIAN_POINT ( 'NONE',  ( 94.81556191316359161, 234.7369531367911009, -4.594050593750048428 ) ) ;
#19956 = CARTESIAN_POINT ( 'NONE',  ( 82.56404520846588468, 41.04076960736067292, -1.149829612626004360 ) ) ;
#19957 = CARTESIAN_POINT ( 'NONE',  ( 162.9352708800131779, 249.6521066053614391, -11.39866856991230293 ) ) ;
#19958 = CARTESIAN_POINT ( 'NONE',  ( 84.42755274236627372, 50.68105307249222591, 13.76233527223795683 ) ) ;
#19959 = CARTESIAN_POINT ( 'NONE',  ( 207.8018416422513894, 270.7236476996756664, 1.610379135119299754 ) ) ;
#19960 = CARTESIAN_POINT ( 'NONE',  ( 31.32559514186443295, 179.7048013555409796, 4.594050593750051981 ) ) ;
#19961 = EDGE_CURVE ( 'NONE', #11356, #1030, #20606, .T. ) ;
#19962 = CARTESIAN_POINT ( 'NONE',  ( 172.7519013077862269, 288.3158815880753423, -8.994867566259873826 ) ) ;
#19963 = ORIENTED_EDGE ( 'NONE', *, *, #85464, .T. ) ;
#19964 = VERTEX_POINT ( 'NONE', #44378 ) ;
#19965 = CARTESIAN_POINT ( 'NONE',  ( 15.75562222995320560, 27.83478043621387599, -8.090169943749479842 ) ) ;
#19966 = CARTESIAN_POINT ( 'NONE',  ( 147.4872062048032433, 275.6374356566055326, -0.2721491379029486457 ) ) ;
#19967 = CARTESIAN_POINT ( 'NONE',  ( 74.45487526951390578, 66.04645349175549995, 13.54363770489549879 ) ) ;
#19968 = LINE ( 'NONE', #20468, #48379 ) ;
#19969 = DIRECTION ( 'NONE',  ( 0.4999999999999998335, -0.8660254037844388186, 0.000000000000000000 ) ) ;
#19970 = CARTESIAN_POINT ( 'NONE',  ( 161.3145230519951951, 251.2420454056404822, -14.44869077440025151 ) ) ;
#19971 = CARTESIAN_POINT ( 'NONE',  ( 68.52675681298484278, 64.32790167916148505, 11.71367573677816942 ) ) ;
#19972 = CARTESIAN_POINT ( 'NONE',  ( 74.09415402004458429, 67.86909550972291072, -11.62290297944830542 ) ) ;
#19973 = CARTESIAN_POINT ( 'NONE',  ( 53.49034604603116350, 195.5643266524159856, 9.188101187500095079 ) ) ;
#19974 = CARTESIAN_POINT ( 'NONE',  ( 86.89529822776817980, 227.6427522451419065, 10.00000000000009237 ) ) ;
#19975 = ORIENTED_EDGE ( 'NONE', *, *, #78320, .F. ) ;
#19976 = ADVANCED_FACE ( 'NONE', ( #13992 ), #60561, .T. ) ;
#19977 = CARTESIAN_POINT ( 'NONE',  ( 198.0324241745848042, 267.8073025728403422, -7.956821422782448749 ) ) ;
#19978 = B_SPLINE_CURVE_WITH_KNOTS ( 'NONE', 3,
 ( #19663, #59104, #96183, #97179, #57124, #42904, #3465, #89590, #5441, #36324, #4434, #35332, #13060, #74371 ),
 .UNSPECIFIED., .F., .F.,
 ( 4, 2, 2, 2, 2, 2, 4 ),
 ( 2.941618428806969512E-15, 0.0005114949209976904715, 0.001022989841992439286, 0.001278737302489847466, 0.001534484762987255646, 0.001790232223484663826, 0.002045979683982072223 ),
 .UNSPECIFIED. ) ;
#19979 = CARTESIAN_POINT ( 'NONE',  ( 3.462723837431157747, 161.2592609112380160, 2.679491924311254714 ) ) ;
#19980 = CARTESIAN_POINT ( 'NONE',  ( 5.669592554750444435, 164.8923013555410080, 4.594050593750050204 ) ) ;
#19981 = CARTESIAN_POINT ( 'NONE',  ( 181.7327785741209141, 287.1345269289352586, -14.84312672137237143 ) ) ;
#19982 = FACE_OUTER_BOUND ( 'NONE', #76178, .T. ) ;
#19983 = CARTESIAN_POINT ( 'NONE',  ( 193.2100161762185735, 295.9974307820218087, -12.46499585622781758 ) ) ;
#19984 = CARTESIAN_POINT ( 'NONE',  ( 163.7323023463233937, 247.0543288263758086, -6.244751637846886361 ) ) ;
#19985 = CARTESIAN_POINT ( 'NONE',  ( 72.52865609845331107, 57.51546068809462753, 16.29679984399868786 ) ) ;
#19986 = FACE_OUTER_BOUND ( 'NONE', #81169, .T. ) ;
#19987 = CARTESIAN_POINT ( 'NONE',  ( 164.3706594650489023, 245.9486618633701482, -1.665857659249071698 ) ) ;
#19988 = EDGE_CURVE ( 'NONE', #62997, #28370, #94598, .T. ) ;
#19989 = ORIENTED_EDGE ( 'NONE', *, *, #28077, .T. ) ;
#19990 = CARTESIAN_POINT ( 'NONE',  ( -1.565588326081831072, 163.2365022471902023, 10.00000000000009592 ) ) ;
#19991 = B_SPLINE_CURVE_WITH_KNOTS ( 'NONE', 3,
 ( #72562, #56825, #33541, #64940, #81667, #95885, #65427, #3646, #26446, #35524, #18848, #88797, #19365, #50224, #81179, #11745, #80684, #87809, #42608, #74042, #11259, #96874, #12241, #35017, #42121, #97354, #73053, #43099, #18349, #49242, #65918, #34528, #41619, #10743, #80177, #58803, #27442, #3166, #58317, #4630, #66424, #34051, #17849, #48750 ),
 .UNSPECIFIED., .F., .F.,
 ( 4, 2, 2, 2, 2, 2, 2, 2, 2, 2, 2, 2, 2, 2, 2, 2, 2, 2, 2, 2, 2, 4 ),
 ( 0.002247607324231777268, 0.002678942405538197770, 0.002894609946191499528, 0.003002443716518150407, 0.003110277486844801285, 0.003218111257171452164, 0.003325945027498102610, 0.003541612568151359264, 0.003972947649457884284, 0.004835617812070935190, 0.005698287974683985228, 0.006560958137297035267, 0.006992293218603561587, 0.007423628299910086173, 0.007531462070236681974, 0.007585378955399979008, 0.007639295840563276908, 0.007747129610889857097, 0.007854963381216436419, 0.008286298462522705133, 0.008717633543828975581, 0.009148968625135313684 ),
 .UNSPECIFIED. ) ;
#19992 = CARTESIAN_POINT ( 'NONE',  ( 83.61470584636902004, 43.92523517391203569, 8.757796049109066061 ) ) ;
#19993 = VECTOR ( 'NONE', #48402, 1000.000000000000000 ) ;
#19994 = CARTESIAN_POINT ( 'NONE',  ( 123.0967907794404113, 248.0024278399161517, 9.188101187500095079 ) ) ;
#19995 = CARTESIAN_POINT ( 'NONE',  ( 28.62558104116610380, 25.03085787977764198, 9.188101187500006262 ) ) ;
#19996 = CARTESIAN_POINT ( 'NONE',  ( 164.3429939525221926, 245.9965799366839008, 1.284743659783852188 ) ) ;
#19997 = CARTESIAN_POINT ( 'NONE',  ( 181.5281250038626979, 294.0940755821732751, -7.844796568590651553 ) ) ;
#19998 = VECTOR ( 'NONE', #80244, 1000.000000000000000 ) ;
#20000 = LINE ( 'NONE', #53369, #83000 ) ;
#19999 = CARTESIAN_POINT ( 'NONE',  ( 196.4351339088274813, 290.4113630087520050, 17.20526457544535504 ) ) ;
#20001 = FACE_OUTER_BOUND ( 'NONE', #58954, .T. ) ;
#20002 = ORIENTED_EDGE ( 'NONE', *, *, #30122, .F. ) ;
#20003 = CARTESIAN_POINT ( 'NONE',  ( 150.6931560952953646, 269.6387926204777727, 14.65021044537114037 ) ) ;
#20004 = CARTESIAN_POINT ( 'NONE',  ( 163.8130561957613338, 246.9144590562426629, 7.378237555415944726 ) ) ;
#20005 = CARTESIAN_POINT ( 'NONE',  ( -19.65312891409030271, 93.06504152958497400, -10.00000000000000000 ) ) ;
#20006 = CARTESIAN_POINT ( 'NONE',  ( 81.96589639849747755, 58.75522159323007543, -0.2191855733945376195 ) ) ;
#20007 = CARTESIAN_POINT ( 'NONE',  ( 81.47495714615762097, 55.16564477528429933, -15.92599370216107602 ) ) ;
#20008 = ORIENTED_EDGE ( 'NONE', *, *, #74586, .T. ) ;
#20009 = CARTESIAN_POINT ( 'NONE',  ( 71.60067202791792340, 71.17545373159485678, 4.829749188030544538 ) ) ;
#20010 = CARTESIAN_POINT ( 'NONE',  ( 82.85376847310632797, 41.32516217177638396, -4.514684729415445297 ) ) ;
#20011 = EDGE_CURVE ( 'NONE', #19304, #80050, #42737, .T. ) ;
#20012 = ADVANCED_FACE ( 'NONE', ( #84422 ), #52831, .F. ) ;
#20013 = CARTESIAN_POINT ( 'NONE',  ( 71.82608767971663610, 72.19311822168063486, 0.5755032799609223204 ) ) ;
#20014 = CARTESIAN_POINT ( 'NONE',  ( 83.35959653392400526, 42.22915863639402545, 4.663558883483734263 ) ) ;
#20015 = CARTESIAN_POINT ( 'NONE',  ( 196.7494297999078867, 271.1026102776716016, 12.03499651395464376 ) ) ;
#20016 = CARTESIAN_POINT ( 'NONE',  ( 181.9526327277720839, 295.0417315924539707, 4.810195558377932556 ) ) ;
#20017 = DIRECTION ( 'NONE',  ( -0.7893155279419928894, -0.6139877827364751406, 0.000000000000000000 ) ) ;
#20018 = LINE ( 'NONE', #45643, #35487 ) ;
#20019 = EDGE_CURVE ( 'NONE', #75682, #35189, #49665, .T. ) ;
#20020 =( BOUNDED_CURVE ( )  B_SPLINE_CURVE ( 2, ( #37995, #61801, #68908, #15199, #99833, #30417, #61307, #92269, #22817 ),
 .UNSPECIFIED., .F., .T. ) 
 B_SPLINE_CURVE_WITH_KNOTS ( ( 3, 2, 2, 2, 3 ),
 ( 0.2217741935483870941, 0.2231182795698924692, 0.2258064516129032195, 0.2284946236559139698, 0.2298387096774193450 ),
 .UNSPECIFIED. ) 
 CURVE ( )  GEOMETRIC_REPRESENTATION_ITEM ( )  RATIONAL_B_SPLINE_CURVE ( ( 0.9330127018922194093, 0.9330127018922194093, 1.000000000000000000, 0.8660254037844387076, 1.000000000000000000, 0.8660254037844387076, 1.000000000000000000, 0.9330127018922194093, 0.9330127018922194093 ) ) 
 REPRESENTATION_ITEM ( '' )  );
#20021 = ORIENTED_EDGE ( 'NONE', *, *, #13240, .T. ) ;
#20022 = DIRECTION ( 'NONE',  ( 0.4999999999999998890, -0.8660254037844385966, 0.000000000000000000 ) ) ;
#20023 = CARTESIAN_POINT ( 'NONE',  ( 38.99862784774133218, 37.91421378149922816, 9.188101187500008038 ) ) ;
#20024 = CARTESIAN_POINT ( 'NONE',  ( 192.0180279664021157, 287.5583705255741052, -16.23921153416872087 ) ) ;
#20025 = ORIENTED_EDGE ( 'NONE', *, *, #92930, .T. ) ;
#20026 = CARTESIAN_POINT ( 'NONE',  ( -22.42236680055709641, 157.8615022471902591, 0.000000000000000000 ) ) ;
#20027 = CARTESIAN_POINT ( 'NONE',  ( 147.6508870500795467, 274.9081571770856272, -8.950912509993816712 ) ) ;
#20028 = CARTESIAN_POINT ( 'NONE',  ( 156.3551087084618700, 261.3239775484371989, -17.56576820129662053 ) ) ;
#20029 = EDGE_LOOP ( 'NONE', ( #70379, #39291, #92892, #27288 ) ) ;
#20031 = EDGE_CURVE ( 'NONE', #85466, #46359, #84829, .T. ) ;
#20030 = FACE_OUTER_BOUND ( 'NONE', #22685, .T. ) ;
#20032 = CARTESIAN_POINT ( 'NONE',  ( 72.67905965592419193, 70.26320000030698054, -8.002569769838684621 ) ) ;
#20033 = B_SPLINE_CURVE_WITH_KNOTS ( 'NONE', 3,
 ( #59553, #15957, #16950, #47839 ),
 .UNSPECIFIED., .F., .F.,
 ( 4, 4 ),
 ( 0.03953143252384128115, 0.04799691715800366576 ),
 .UNSPECIFIED. ) ;
#20034 = DIRECTION ( 'NONE',  ( 0.4999999999999998890, -0.8660254037844385966, 0.000000000000000000 ) ) ;
#20035 = ORIENTED_EDGE ( 'NONE', *, *, #38829, .T. ) ;
#20036 = CARTESIAN_POINT ( 'NONE',  ( 79.98487687335507701, 226.1744531367911293, 4.594050593750047540 ) ) ;
#20037 = CARTESIAN_POINT ( 'NONE',  ( 202.9996883242178569, 279.0412212322449932, 16.31748462427307089 ) ) ;
#20038 = CARTESIAN_POINT ( 'NONE',  ( 41.51553799054923388, 59.02985107750645000, 177.5919119679930134 ) ) ;
#20039 = CARTESIAN_POINT ( 'NONE',  ( 185.0987280534011177, 259.9520638838685613, -6.416371529008482177 ) ) ;
#20040 = EDGE_CURVE ( 'NONE', #86862, #11831, #67561, .T. ) ;
#20041 = VERTEX_POINT ( 'NONE', #65573 ) ;
#20042 = EDGE_CURVE ( 'NONE', #69466, #49291, #87519, .T. ) ;
#20043 = ORIENTED_EDGE ( 'NONE', *, *, #62049, .F. ) ;
#20044 = CARTESIAN_POINT ( 'NONE',  ( 207.3873553355473121, 271.0594493704188039, 2.178264502744591269 ) ) ;
#20045 = VERTEX_POINT ( 'NONE', #27595 ) ;
#20046 = CARTESIAN_POINT ( 'NONE',  ( 192.6299325303148464, 294.0530281384722002, 14.39848446519248704 ) ) ;
#20047 = VERTEX_POINT ( 'NONE', #51879 ) ;
#20048 = LINE ( 'NONE', #50920, #99402 ) ;
#20049 = DIRECTION ( 'NONE',  ( -0.8660254037844378194, -0.5000000000000013323, -0.000000000000000000 ) ) ;
#20050 = ORIENTED_EDGE ( 'NONE', *, *, #96381, .T. ) ;
#20051 = DIRECTION ( 'NONE',  ( -0.9956898167541090583, 0.09274582908232931189, 0.000000000000000000 ) ) ;
#20052 = CARTESIAN_POINT ( 'NONE',  ( 82.37238700568863692, 40.69398333026209258, 3.209141624528058845 ) ) ;
#20053 = CARTESIAN_POINT ( 'NONE',  ( 152.1113819699424425, 268.9580029282372493, 15.28343548679968933 ) ) ;
#20054 = DIRECTION ( 'NONE',  ( -0.9942962326340534229, -0.1066536533351210708, 0.000000000000000000 ) ) ;
#20055 = DIRECTION ( 'NONE',  ( -1.000000000000000000, 0.000000000000000000, -2.816764622163176999E-16 ) ) ;
#20056 = CARTESIAN_POINT ( 'NONE',  ( 19.47506710560450216, 33.01751292744056343, 6.180339887498949913 ) ) ;
#20057 = CARTESIAN_POINT ( 'NONE',  ( 136.3847812948166336, 258.7369531367911009, -4.594050593750048428 ) ) ;
#20058 = DIRECTION ( 'NONE',  ( -0.1378186779084930869, 0.2387089523694814197, -0.9612616959383223358 ) ) ;
#20059 = ORIENTED_EDGE ( 'NONE', *, *, #65690, .F. ) ;
#20060 = CARTESIAN_POINT ( 'NONE',  ( 76.87919255693888942, 60.90556971193419145, 15.72099009421724602 ) ) ;
#20061 = CARTESIAN_POINT ( 'NONE',  ( 14.00658445089738180, 13.80170272979924917, 7.433330006724137462 ) ) ;
#20062 = VERTEX_POINT ( 'NONE', #35671 ) ;
#20063 = CARTESIAN_POINT ( 'NONE',  ( -34.16292631813981728, 25.86630820016799248, -10.00000000000000000 ) ) ;
#20065 = VERTEX_POINT ( 'NONE', #36158 ) ;
#20064 = CARTESIAN_POINT ( 'NONE',  ( 85.55975315002648074, 48.35019831671618817, -12.20940535940758132 ) ) ;
#20066 = CARTESIAN_POINT ( 'NONE',  ( -14.55094619507370801, 105.4688078659398514, 10.59293022331821099 ) ) ;
#20067 = CARTESIAN_POINT ( 'NONE',  ( 181.8509774751104544, 266.9677320091309412, 16.09658033613713712 ) ) ;
#20068 = CARTESIAN_POINT ( 'NONE',  ( 120.6060784269860449, 251.9860189848785410, -2.679491924311252493 ) ) ;
#20069 = DIRECTION ( 'NONE',  ( -0.8660254037844382635, -0.5000000000000004441, 0.000000000000000000 ) ) ;
#20070 = CARTESIAN_POINT ( 'NONE',  ( 84.85238324705348134, 49.19334207431751338, -13.14179292021528056 ) ) ;
#20071 = DIRECTION ( 'NONE',  ( -1.000000000000000000, 0.000000000000000000, 0.000000000000000000 ) ) ;
#20072 = VECTOR ( 'NONE', #42548, 1000.000000000000000 ) ;
#20073 = CARTESIAN_POINT ( 'NONE',  ( 87.34045233512981099, 44.85499964951561225, 5.787806721962865275 ) ) ;
#20074 = CARTESIAN_POINT ( 'NONE',  ( 88.06934480351134198, 44.11702129290613072, -1.709332125350027765 ) ) ;
#20075 = ORIENTED_EDGE ( 'NONE', *, *, #28774, .T. ) ;
#20076 = CARTESIAN_POINT ( 'NONE',  ( 58.10966550219799132, 178.3759306620403606, -18.47570218321542868 ) ) ;
#20077 = CARTESIAN_POINT ( 'NONE',  ( 66.13500987590335001, 69.30841116337150254, 0.2424399591101732698 ) ) ;
#20078 = AXIS2_PLACEMENT_3D ( 'NONE', #65197, #72325, #34298 ) ;
#20079 = EDGE_LOOP ( 'NONE', ( #64489, #56886, #60875, #34331, #6430, #15961, #54366, #62151, #52164, #31867, #25494, #91192, #83650, #29870, #30095, #23626, #74244, #26299, #71852, #19798, #79958, #55050 ) ) ;
#20080 = CARTESIAN_POINT ( 'NONE',  ( 159.9983927609781063, 276.8049897941343716, 13.27407150049416806 ) ) ;
#20081 = AXIS2_PLACEMENT_3D ( 'NONE', #15006, #76345, #61106 ) ;
#20082 = DIRECTION ( 'NONE',  ( 0.9755587037855241173, -0.2197389712097240766, 0.000000000000000000 ) ) ;
#20083 = FACE_OUTER_BOUND ( 'NONE', #1460, .T. ) ;
#20084 = CARTESIAN_POINT ( 'NONE',  ( 164.7647380297938184, 248.9862001899016946, 10.10785415616959071 ) ) ;
#20085 = CARTESIAN_POINT ( 'NONE',  ( 164.6081132108126326, 274.3788087673100904, 14.77367721212278084 ) ) ;
#20087 = CARTESIAN_POINT ( 'NONE',  ( 88.11245462187771693, 44.31171394170508648, 2.759943262836158873 ) ) ;
#20086 = CARTESIAN_POINT ( 'NONE',  ( 161.2908438277387972, 281.6436246679302258, -7.517958113851705981 ) ) ;
#20088 = ADVANCED_FACE ( 'NONE', ( #19986 ), #59443, .F. ) ;
#20089 = CARTESIAN_POINT ( 'NONE',  ( 160.1764156583825525, 261.1444413449148101, 17.72707215100685829 ) ) ;
#20090 = ORIENTED_EDGE ( 'NONE', *, *, #30343, .F. ) ;
#20091 = B_SPLINE_SURFACE_WITH_KNOTS ( 'NONE', 3, 1, ( 
 ( #97178, #51022 ),
 ( #65723, #21154 ),
 ( #42419, #73844 ),
 ( #80995, #19662 ),
 ( #27745, #67225 ),
 ( #58614, #52033 ),
 ( #98152, #28735 ),
 ( #20154, #13548 ),
 ( #67733, #89589 ),
 ( #82973, #81974 ),
 ( #91072, #27248 ),
 ( #44420, #12551 ),
 ( #51532, #43424 ),
 ( #58131, #98656 ),
 ( #75350, #73352 ),
 ( #74370, #4953 ),
 ( #5930, #20644 ),
 ( #13059, #59609 ),
 ( #97661, #28229 ),
 ( #59103, #3940 ),
 ( #50524, #90075 ),
 ( #29240, #43919 ),
 ( #60106, #74858 ),
 ( #92561, #77326 ),
 ( #44911, #45895 ),
 ( #22627, #62601 ),
 ( #38305, #16018 ),
 ( #37315, #93555 ),
 ( #69713, #38807 ),
 ( #7933, #30728 ),
 ( #92079, #321 ),
 ( #31211, #62097 ),
 ( #815, #53513 ),
 ( #23600, #8422 ) ),
 .UNSPECIFIED., .T., .F., .F.,
 ( 4, 2, 2, 2, 2, 2, 2, 2, 2, 2, 2, 2, 2, 2, 2, 2, 4 ),
 ( 2, 2 ),
 ( 0.000000000000000000, 0.06250000000000000000, 0.1250000000000000000, 0.1875000000000000000, 0.2500000000000000000, 0.3125000000000000000, 0.3750000000000000000, 0.4375000000000000000, 0.5000000000000000000, 0.5625000000000000000, 0.6250000000000000000, 0.6875000000000000000, 0.7500000000000000000, 0.8125000000000000000, 0.8750000000000000000, 0.9375000000000000000, 1.000000000000000000 ),
 ( 0.000000000000000000, 1.000000000000000000 ),
 .UNSPECIFIED. ) ;
#20092 = ORIENTED_EDGE ( 'NONE', *, *, #8174, .F. ) ;
#20093 = FACE_OUTER_BOUND ( 'NONE', #34608, .T. ) ;
#20094 = EDGE_CURVE ( 'NONE', #91664, #32333, #33062, .T. ) ;
#20095 = DIRECTION ( 'NONE',  ( 0.3535533905932783383, -0.6123724356958041293, 0.7071067811865369146 ) ) ;
#20096 = CARTESIAN_POINT ( 'NONE',  ( 66.99892443162359257, 66.90181954958814003, -8.791929524054854284 ) ) ;
#20097 = CARTESIAN_POINT ( 'NONE',  ( 184.6885808911535207, 260.6528513612950064, 10.31057805081157852 ) ) ;
#20098 = CARTESIAN_POINT ( 'NONE',  ( 81.14781783016522354, 43.43044292088951863, -9.929167272279752154 ) ) ;
#20099 = CARTESIAN_POINT ( 'NONE',  ( 22.72264919896475988, 37.02287747747012503, -10.00000000000000000 ) ) ;
#20100 = CARTESIAN_POINT ( 'NONE',  ( 12.78715206816254302, 172.0643266524160140, -9.188101187500093303 ) ) ;
#20101 = CARTESIAN_POINT ( 'NONE',  ( 102.5290345353249961, 223.8768266524159856, 9.188101187500098632 ) ) ;
#20102 = CARTESIAN_POINT ( 'NONE',  ( 155.1601726304954809, 261.9016930232608615, -18.56587418422714464 ) ) ;
#20103 = CARTESIAN_POINT ( 'NONE',  ( 40.63510790894940072, 204.2677522451419350, -5.000000000000047962 ) ) ;
#20104 = CARTESIAN_POINT ( 'NONE',  ( 186.7158489563707064, 295.8341147379624090, -7.679202307086533175 ) ) ;
#20105 = EDGE_CURVE ( 'NONE', #62030, #56261, #18231, .T. ) ;
#20106 = CARTESIAN_POINT ( 'NONE',  ( 77.86030215884842676, 50.85760040121600412, 15.26662539205169544 ) ) ;
#20107 = CARTESIAN_POINT ( 'NONE',  ( 76.16157665297757262, 51.33368209758570799, 15.63302325843619478 ) ) ;
#20108 = DIRECTION ( 'NONE',  ( 1.000000000000000000, 0.000000000000000000, 0.000000000000000000 ) ) ;
#20109 = CARTESIAN_POINT ( 'NONE',  ( 147.6054094044680198, 274.9869267698931594, -8.596541856229405809 ) ) ;
#20110 = EDGE_CURVE ( 'NONE', #75490, #20280, #31546, .T. ) ;
#20111 = CARTESIAN_POINT ( 'NONE',  ( 84.43973019491031096, 50.14528805649905507, 13.86389828189430062 ) ) ;
#20112 = DIRECTION ( 'NONE',  ( -0.001635407438350354676, -0.9999986627203610867, 0.000000000000000000 ) ) ;
#20113 = CARTESIAN_POINT ( 'NONE',  ( 166.1070111784138703, 253.4115428555481344, -13.60050710122670559 ) ) ;
#20114 = EDGE_CURVE ( 'NONE', #50302, #7411, #28218, .T. ) ;
#20115 = DIRECTION ( 'NONE',  ( 0.000000000000000000, 0.000000000000000000, 1.000000000000000000 ) ) ;
#20116 = CARTESIAN_POINT ( 'NONE',  ( 72.86731735994297310, 219.0024278399160664, -9.188101187500093303 ) ) ;
#20117 = CARTESIAN_POINT ( 'NONE',  ( 161.8150574665248200, 250.3750943687383881, -13.25074899737357903 ) ) ;
#20118 = CARTESIAN_POINT ( 'NONE',  ( -14.76680962501131589, 102.8402364515597469, 11.91671626263131856 ) ) ;
#20120 = CARTESIAN_POINT ( 'NONE',  ( 84.07324426729904587, 42.29269841712828537, -3.545903798621591996 ) ) ;
#20119 = CARTESIAN_POINT ( 'NONE',  ( 195.7578697689113199, 291.5844189092309193, 17.18796537138345215 ) ) ;
#20121 = CARTESIAN_POINT ( 'NONE',  ( 199.1867231605587278, 285.6454706231928071, -17.41989184023605475 ) ) ;
#20122 = FACE_OUTER_BOUND ( 'NONE', #78708, .T. ) ;
#20123 = CARTESIAN_POINT ( 'NONE',  ( 36.95804531498377798, 23.19860640527294748, 2.839279412974134775 ) ) ;
#20124 = CARTESIAN_POINT ( 'NONE',  ( 83.00815485991435594, 53.30142267139500234, 15.60062745561815589 ) ) ;
#20125 = CARTESIAN_POINT ( 'NONE',  ( 74.42516694136719480, 55.76460849002628350, 16.59412675241640756 ) ) ;
#20126 = ORIENTED_EDGE ( 'NONE', *, *, #34864, .T. ) ;
#20127 = CARTESIAN_POINT ( 'NONE',  ( 26.45569963029868177, 20.98920272979927049, 7.433330006724137462 ) ) ;
#20128 = LINE ( 'NONE', #42884, #16707 ) ;
#20129 = CARTESIAN_POINT ( 'NONE',  ( -32.26013835757641601, 93.64104699330448511, 10.58366280279360971 ) ) ;
#20130 = CARTESIAN_POINT ( 'NONE',  ( 57.17980156396255609, 210.4865022471903160, 10.00000000000009415 ) ) ;
#20131 = ADVANCED_FACE ( 'NONE', ( #16359 ), #38135, .F. ) ;
#20132 = CARTESIAN_POINT ( 'NONE',  ( 70.96326928872720430, 61.01013475532322161, 14.52989670127069921 ) ) ;
#20133 = DIRECTION ( 'NONE',  ( 0.03487823687205911238, -0.06041087834082882468, 0.9975640502598247528 ) ) ;
#20134 = AXIS2_PLACEMENT_3D ( 'NONE', #96404, #34562, #19399 ) ;
#20135 = CARTESIAN_POINT ( 'NONE',  ( 157.5205412249731012, 268.7636797464979281, 15.65110165726261293 ) ) ;
#20136 = CARTESIAN_POINT ( 'NONE',  ( 189.5059428776464756, 300.4130739301078279, -3.423561384717671796 ) ) ;
#20137 = CARTESIAN_POINT ( 'NONE',  ( 87.34647367080899016, 44.99587983710786432, -6.159439337099199996 ) ) ;
#20138 = CARTESIAN_POINT ( 'NONE',  ( 131.6579862894242865, 253.4865022471903444, -10.00000000000009415 ) ) ;
#20139 = CARTESIAN_POINT ( 'NONE',  ( 157.4211152037729562, 257.9856256133486454, -16.71526195140576831 ) ) ;
#20140 = EDGE_CURVE ( 'NONE', #74959, #31723, #15339, .T. ) ;
#20141 = CARTESIAN_POINT ( 'NONE',  ( 75.47390685083401252, 53.30987980041999919, 16.49587604864008838 ) ) ;
#20142 = ORIENTED_EDGE ( 'NONE', *, *, #905, .F. ) ;
#20143 = CARTESIAN_POINT ( 'NONE',  ( 70.08393322175207629, 63.28384585981274313, 13.68523560319354360 ) ) ;
#20144 = CARTESIAN_POINT ( 'NONE',  ( 188.7258768753199831, 272.5327203015561395, 16.40358330166877465 ) ) ;
#20145 = VERTEX_POINT ( 'NONE', #14371 ) ;
#20146 = CARTESIAN_POINT ( 'NONE',  ( 196.4030970371012472, 264.3490001850324234, -4.693669024083267693 ) ) ;
#20147 = CARTESIAN_POINT ( 'NONE',  ( 81.45101120633425751, 42.17020710753002533, -7.997091885120573451 ) ) ;
#20148 = VERTEX_POINT ( 'NONE', #7760 ) ;
#20149 = CARTESIAN_POINT ( 'NONE',  ( 86.26394923150375860, 43.12119067694047203, 1.349736823004491049 ) ) ;
#20151 = VERTEX_POINT ( 'NONE', #24458 ) ;
#20150 = AXIS2_PLACEMENT_3D ( 'NONE', #33625, #1737, #65021 ) ;
#20153 = EDGE_CURVE ( 'NONE', #31618, #54703, #42384, .T. ) ;
#20152 = CARTESIAN_POINT ( 'NONE',  ( 192.8546065288647924, 292.4362985693752535, 15.15881306499927916 ) ) ;
#20154 = CARTESIAN_POINT ( 'NONE',  ( 205.5299317431642692, 274.6587110751127625, 11.78078220685493882 ) ) ;
#20155 = CARTESIAN_POINT ( 'NONE',  ( 148.9967968810750563, 247.6423013555410080, -4.594050593750043987 ) ) ;
#20156 = CARTESIAN_POINT ( 'NONE',  ( 204.8874959148301400, 273.6675085671400325, 10.84287252419124492 ) ) ;
#20157 = CARTESIAN_POINT ( 'NONE',  ( 153.2583947049096764, 265.1956690150883560, -17.64103123457563882 ) ) ;
#20158 = EDGE_CURVE ( 'NONE', #54381, #24764, #63953, .T. ) ;
#20159 = CARTESIAN_POINT ( 'NONE',  ( 35.31080938399455249, 26.10170272979929607, -7.433330006724141015 ) ) ;
#20160 = CARTESIAN_POINT ( 'NONE',  ( 73.37987013686270643, 60.48738129690996601, -15.24192514929477404 ) ) ;
#20161 = CARTESIAN_POINT ( 'NONE',  ( 176.3865323452404823, 258.8737835494043225, 13.24306684835586623 ) ) ;
#20162 = CARTESIAN_POINT ( 'NONE',  ( 173.9008529106967558, 272.4049662731551962, -17.79092985220220058 ) ) ;
#20163 = ORIENTED_EDGE ( 'NONE', *, *, #55878, .T. ) ;
#20164 = ORIENTED_EDGE ( 'NONE', *, *, #54513, .T. ) ;
#20165 = CARTESIAN_POINT ( 'NONE',  ( 183.0159800400793983, 295.9215593239155169, 0.5241057615201285547 ) ) ;
#20166 = CARTESIAN_POINT ( 'NONE',  ( 84.40498577231251431, 50.09068632715275271, 13.84414505597724521 ) ) ;
#20168 = CARTESIAN_POINT ( 'NONE',  ( 162.8751945631634612, 272.8900720096677333, -16.40198242748087054 ) ) ;
#20167 = CARTESIAN_POINT ( 'NONE',  ( 163.7239493340838123, 247.0687966679708438, 6.286946239157660266 ) ) ;
#20169 = CARTESIAN_POINT ( 'NONE',  ( 110.0000000000000000, 15.00000000000000000, 9.212605237762131694 ) ) ;
#20170 = CARTESIAN_POINT ( 'NONE',  ( 166.4873690803768795, 248.5196436787675225, -7.973532822608550674 ) ) ;
#20171 = CARTESIAN_POINT ( 'NONE',  ( 159.9449220377261440, 283.7382459705826818, 0.01809001837185298528 ) ) ;
#20172 = DIRECTION ( 'NONE',  ( -0.000000000000000000, 1.000000000000000000, -0.000000000000000000 ) ) ;
#20173 = CARTESIAN_POINT ( 'NONE',  ( 58.43017357788679789, 217.8207943907112849, 17.47570218321536117 ) ) ;
#20174 = CARTESIAN_POINT ( 'NONE',  ( 169.8297681824042513, 267.4479351203237911, 17.31714983691947651 ) ) ;
#20175 = CARTESIAN_POINT ( 'NONE',  ( 181.9516171695871378, 256.9925793098663007, 5.069001809681082271 ) ) ;
#20176 = CARTESIAN_POINT ( 'NONE',  ( 97.06207562605321471, 226.8458772461660544, 9.188101187500095079 ) ) ;
#20177 = ORIENTED_EDGE ( 'NONE', *, *, #97538, .T. ) ;
#20178 = LINE ( 'NONE', #64265, #38211 ) ;
#20179 = DIRECTION ( 'NONE',  ( 0.5000000000000014433, -0.8660254037844379305, 0.000000000000000000 ) ) ;
#20180 = CARTESIAN_POINT ( 'NONE',  ( 163.0851559127074495, 276.7488112146713206, -14.21592638994824576 ) ) ;
#20181 = ORIENTED_EDGE ( 'NONE', *, *, #40293, .T. ) ;
#20182 = ORIENTED_EDGE ( 'NONE', *, *, #56931, .F. ) ;
#20183 = CARTESIAN_POINT ( 'NONE',  ( 87.18478751182242092, 46.16420910987052650, -8.338078487178403719 ) ) ;
#20184 = CARTESIAN_POINT ( 'NONE',  ( 178.7254881896226948, 292.9730135732680765, -2.650317027749069076 ) ) ;
#20185 = CARTESIAN_POINT ( 'NONE',  ( 157.2333142128019858, 258.3109064714224132, 16.87956768598436597 ) ) ;
#20186 = CARTESIAN_POINT ( 'NONE',  ( 16.97222724706317720, 11.92755873383624987, 6.180339887498953466 ) ) ;
#20187 = PLANE ( 'NONE',  #51190 ) ;
#20188 = VERTEX_POINT ( 'NONE', #64462 ) ;
#20189 = VERTEX_POINT ( 'NONE', #94894 ) ;
#20190 = CARTESIAN_POINT ( 'NONE',  ( 184.7531445739716105, 265.1985052118166095, -14.31512252865175050 ) ) ;
#20191 = DIRECTION ( 'NONE',  ( 0.000000000000000000, 0.000000000000000000, 1.000000000000000000 ) ) ;
#20192 = ORIENTED_EDGE ( 'NONE', *, *, #71996, .F. ) ;
#20193 = CARTESIAN_POINT ( 'NONE',  ( 194.4117352900907747, 266.1848707878391451, -7.745729181019060938 ) ) ;
#20194 = CARTESIAN_POINT ( 'NONE',  ( 23.47697960001819695, 174.3615022471901739, 5.000000000000051514 ) ) ;
#20195 = CARTESIAN_POINT ( 'NONE',  ( 82.17415024888090613, 44.43251709326036547, 9.654931585787190684 ) ) ;
#20197 = CARTESIAN_POINT ( 'NONE',  ( 69.74385355405661358, 62.24098940029958271, -13.60094204340151158 ) ) ;
#20196 = CARTESIAN_POINT ( 'NONE',  ( 130.0789470495699618, 258.1589784336661637, -6.496448406907675876E-16 ) ) ;
#20198 = CARTESIAN_POINT ( 'NONE',  ( 33.63407072503001416, 49.62913085183823370, 10.00000000000000000 ) ) ;
#20199 = VERTEX_POINT ( 'NONE', #71579 ) ;
#20200 = CARTESIAN_POINT ( 'NONE',  ( 190.3286155001717930, 300.9881631498979004, -5.624828231725103045 ) ) ;
#20201 = CARTESIAN_POINT ( 'NONE',  ( 71.24993629681053164, 61.94327900918170826, 14.19888696492397884 ) ) ;
#20202 = CARTESIAN_POINT ( 'NONE',  ( 82.44819350194325125, 40.44303670712709931, -1.385655820001176597 ) ) ;
#20203 = CARTESIAN_POINT ( 'NONE',  ( 170.2114099174445698, 248.6575072932782575, -0.2697646958337756029 ) ) ;
#20204 = DIRECTION ( 'NONE',  ( 0.000000000000000000, 0.000000000000000000, 1.000000000000000000 ) ) ;
#20205 = CARTESIAN_POINT ( 'NONE',  ( 75.98104421109889017, 51.53574906954565193, 16.18761828508177558 ) ) ;
#20206 = CARTESIAN_POINT ( 'NONE',  ( 195.5083716432090171, 279.7078053236261894, -16.99617889076117905 ) ) ;
#20207 = CARTESIAN_POINT ( 'NONE',  ( -22.42236680055709641, 157.8615022471902591, 0.000000000000000000 ) ) ;
#20208 = CARTESIAN_POINT ( 'NONE',  ( 79.97334651676149520, 50.01100418247790458, 14.56762597300080841 ) ) ;
#20209 = CARTESIAN_POINT ( 'NONE',  ( 206.7852059338757158, 271.6495446167011778, 6.263730558154075645 ) ) ;
#20210 = CARTESIAN_POINT ( 'NONE',  ( 159.6962080797732710, 254.0450491601782232, -15.33973334987084947 ) ) ;
#20211 = CARTESIAN_POINT ( 'NONE',  ( 77.74246467396064020, 62.00370236096145504, 15.64046932493554110 ) ) ;
#20212 = CARTESIAN_POINT ( 'NONE',  ( 207.5886452961740076, 271.0929146030698007, -1.661373005306138184 ) ) ;
#20214 = EDGE_CURVE ( 'NONE', #48247, #54626, #59626, .T. ) ;
#20213 = VECTOR ( 'NONE', #68197, 1000.000000000000114 ) ;
#20215 = B_SPLINE_CURVE_WITH_KNOTS ( 'NONE', 3,
 ( #60565, #38773, #53963, #45860, #76784, #83933, #15465, #29691, #45379, #21600, #30185, #30692, #77288, #7378, #14497, #283, #69679, #37284, #61572, #38265, #6884, #91522, #39258, #93010, #15982, #23564, #29204, #52482, #13995, #44875, #75815, #37773, #6399, #99605, #61071, #92041, #16481, #94522, #26095, #63081, #64594, #25074, #18499, #55954, #80330, #63580, #33185, #78300, #64085, #78800, #79828, #87467 ),
 .UNSPECIFIED., .F., .F.,
 ( 4, 2, 2, 2, 2, 2, 2, 2, 2, 2, 2, 2, 2, 2, 2, 2, 2, 2, 2, 2, 2, 2, 2, 2, 2, 4 ),
 ( 0.0001011000311972802914, 0.001124998771331816661, 0.001380973456365458627, 0.001636948141399100377, 0.001764935483915945754, 0.001892922826432790915, 0.002020910168949636293, 0.002148897511466481454, 0.002404872196500165270, 0.002660846881533849954, 0.003172796251601219322, 0.004196694991736034386, 0.005220593731870849449, 0.005732543101938256114, 0.005988517786971918680, 0.006116505129488747361, 0.006244492472005574307, 0.006308486143264019873, 0.006372479814522463704, 0.006500467157039355702, 0.006756441842073139699, 0.007012416527106922828, 0.007268391212140705958, 0.007524365897174489087, 0.007780340582208273084, 0.008292289952275735260 ),
 .UNSPECIFIED. ) ;
#20216 = B_SPLINE_CURVE_WITH_KNOTS ( 'NONE', 3,
 ( #85191, #20143, #60098, #98142, #21627, #10664, #75341, #25873, #91063, #67217, #74360, #49162, #80098, #29231, #87730, #98648 ),
 .UNSPECIFIED., .F., .F.,
 ( 4, 1, 2, 2, 2, 1, 2, 2, 4 ),
 ( 0.000000000000000000, 0.1250000000000018596, 0.1875000000000026645, 0.2500000000000034972, 0.5000000000000088818, 0.6250000000000092149, 0.6875000000000086597, 0.7500000000000082157, 1.000000000000000000 ),
 .UNSPECIFIED. ) ;
#20217 = CARTESIAN_POINT ( 'NONE',  ( 71.31272509113929914, 71.01324172527584722, -4.873768137004467427 ) ) ;
#20218 = CARTESIAN_POINT ( 'NONE',  ( 185.8360385916904534, 265.6419344405306902, 13.25022526328142902 ) ) ;
#20219 = CARTESIAN_POINT ( 'NONE',  ( 49.65150239490934325, 78.72539382324355017, -10.00000000000000178 ) ) ;
#20220 = ADVANCED_FACE ( 'NONE', ( #1679 ), #37462, .F. ) ;
#20221 = CARTESIAN_POINT ( 'NONE',  ( 27.55345145191056488, 40.00034080476292786, -1.878358725466461243E-16 ) ) ;
#20222 = DIRECTION ( 'NONE',  ( -0.9302793824855987159, 0.3668518372888613377, 0.000000000000000000 ) ) ;
#20223 = CARTESIAN_POINT ( 'NONE',  ( -22.42236680055709641, 157.8615022471902591, 0.000000000000000000 ) ) ;
#20224 = CARTESIAN_POINT ( 'NONE',  ( 82.57051958873132946, 54.16786056752901857, 15.56146448981428776 ) ) ;
#20225 = DIRECTION ( 'NONE',  ( -0.4272584830711297910, -0.9041295198386993803, 0.000000000000000000 ) ) ;
#20226 = EDGE_CURVE ( 'NONE', #86016, #67131, #18553, .T. ) ;
#20227 = CARTESIAN_POINT ( 'NONE',  ( 8.294124642383250645, 187.8464784336662206, 1.353441290958777327E-15 ) ) ;
#20228 = CARTESIAN_POINT ( 'NONE',  ( 42.77981749017101976, 207.0530062829863311, -4.648177544792955347E-16 ) ) ;
#20229 = VERTEX_POINT ( 'NONE', #84072 ) ;
#20230 = CARTESIAN_POINT ( 'NONE',  ( 87.37978634506822573, 45.87160741090568905, 8.420816086386249566 ) ) ;
#20231 = CARTESIAN_POINT ( 'NONE',  ( -19.54038299334472484, 93.15107696413387828, 59.99999999999999289 ) ) ;
#20232 = CARTESIAN_POINT ( 'NONE',  ( 71.97942276284884144, 72.19511207240364570, -1.653363456454256974 ) ) ;
#20233 = CARTESIAN_POINT ( 'NONE',  ( 29.51209413086700906, 187.8458772461660544, 9.188101187500095079 ) ) ;
#20234 = VECTOR ( 'NONE', #52389, 1000.000000000000000 ) ;
#20235 = CARTESIAN_POINT ( 'NONE',  ( 86.79190430688251467, 45.84585087985657736, 8.866399834819148396 ) ) ;
#20236 = CARTESIAN_POINT ( 'NONE',  ( 48.91560817564824504, 80.00000000000000000, 59.99999999999999289 ) ) ;
#20237 = CARTESIAN_POINT ( 'NONE',  ( 190.7403173041394950, 300.2750747078583800, -4.254144485856557800 ) ) ;
#20238 = CARTESIAN_POINT ( 'NONE',  ( 9.573022157908470220, 14.03085787977760646, 9.188101187500006262 ) ) ;
#20239 = CARTESIAN_POINT ( 'NONE',  ( 200.2679923989394695, 268.3464411988675238, -6.479517804580061657 ) ) ;
#20240 = CARTESIAN_POINT ( 'NONE',  ( 178.8232363120552009, 293.8514986339519055, 2.698715758866663705 ) ) ;
#20241 = CARTESIAN_POINT ( 'NONE',  ( 177.5665759502285539, 275.7863988818428993, 17.69313789786682989 ) ) ;
#20242 = CARTESIAN_POINT ( 'NONE',  ( 181.3268249587086416, 279.4937579209391743, -16.12903209385025249 ) ) ;
#20243 = DIRECTION ( 'NONE',  ( 0.8660254037844391517, 0.4999999999999990008, 0.000000000000000000 ) ) ;
#20244 = CARTESIAN_POINT ( 'NONE',  ( 92.59663213601581333, 214.2677522451417929, -5.000000000000041744 ) ) ;
#20245 = CARTESIAN_POINT ( 'NONE',  ( 155.6413013457028001, 278.6139379961560394, 8.732707396284567380 ) ) ;
#20246 = CARTESIAN_POINT ( 'NONE',  ( 100.4810717531845654, 215.4865022471901455, 1.119607411625061291E-15 ) ) ;
#20247 = FACE_OUTER_BOUND ( 'NONE', #87399, .T. ) ;
#20248 = ADVANCED_FACE ( 'NONE', ( #58342 ), #29328, .F. ) ;
#20249 = CARTESIAN_POINT ( 'NONE',  ( 161.6503117857367329, 267.7950018264848495, -17.32522542692637657 ) ) ;
#20250 = VERTEX_POINT ( 'NONE', #45504 ) ;
#20251 = CARTESIAN_POINT ( 'NONE',  ( 58.09093245575348874, 204.3458772461660544, 9.188101187500095079 ) ) ;
#20252 = VERTEX_POINT ( 'NONE', #60194 ) ;
#20253 = CARTESIAN_POINT ( 'NONE',  ( 177.1347673595945764, 262.9921672455169528, 15.53478677465993485 ) ) ;
#20254 = DIRECTION ( 'NONE',  ( -0.2197389712097240488, -0.9755587037855242283, 0.000000000000000000 ) ) ;
#20255 = CARTESIAN_POINT ( 'NONE',  ( 67.25371248956088266, 66.53894546794931841, -8.600501240181268159 ) ) ;
#20256 = VERTEX_POINT ( 'NONE', #22724 ) ;
#20257 = LINE ( 'NONE', #12667, #24876 ) ;
#20259 = EDGE_CURVE ( 'NONE', #11090, #23644, #37897, .T. ) ;
#20258 = CARTESIAN_POINT ( 'NONE',  ( 164.9836323268835940, 244.8869617230113249, -2.696511969808454534 ) ) ;
#20260 = CARTESIAN_POINT ( 'NONE',  ( 32.23239235789582580, 67.26876094202697232, 59.99999999999999289 ) ) ;
#20261 = CARTESIAN_POINT ( 'NONE',  ( 32.07042461746584650, 33.91421378149919974, 9.188101187500008038 ) ) ;
#20262 = CARTESIAN_POINT ( 'NONE',  ( 185.7308318325395646, 263.1015815296372011, 11.16513425297995177 ) ) ;
#20263 = DIRECTION ( 'NONE',  ( -0.8917477921037054722, -0.4525327339300069251, 0.000000000000000000 ) ) ;
#20264 = CARTESIAN_POINT ( 'NONE',  ( 205.0957184426459321, 275.4107905729332515, 13.78964280781899632 ) ) ;
#20265 = VERTEX_POINT ( 'NONE', #74069 ) ;
#20266 = CARTESIAN_POINT ( 'NONE',  ( 17.75393198606386136, 12.11110640527291160, -2.839279412974138328 ) ) ;
#20267 = FACE_OUTER_BOUND ( 'NONE', #42225, .T. ) ;
#20268 = CARTESIAN_POINT ( 'NONE',  ( 175.0005702576303008, 255.0550677227203948, 8.001073647505871023 ) ) ;
#20269 = CARTESIAN_POINT ( 'NONE',  ( -19.65312891409030271, 93.06504152958497400, 59.99999999999999289 ) ) ;
#20270 = ADVANCED_FACE ( 'NONE', ( #68805 ), #91154, .F. ) ;
#20271 = ORIENTED_EDGE ( 'NONE', *, *, #85808, .F. ) ;
#20272 = CARTESIAN_POINT ( 'NONE',  ( 76.61511796410523800, 54.31696088684743273, 16.52897461885082464 ) ) ;
#20273 = CARTESIAN_POINT ( 'NONE',  ( 150.7530568467738590, 269.5350414755053521, 15.60317050893315916 ) ) ;
#20274 = CARTESIAN_POINT ( 'NONE',  ( 159.2186641046529303, 254.8721795879351646, -15.96198087403305443 ) ) ;
#20275 = CIRCLE ( 'NONE', #8902, 0.1418229129683812317 ) ;
#20276 = ORIENTED_EDGE ( 'NONE', *, *, #20478, .F. ) ;
#20278 = CARTESIAN_POINT ( 'NONE',  ( 82.21410988452117863, 40.73976263626466476, 3.762362152834606732 ) ) ;
#20277 = CARTESIAN_POINT ( 'NONE',  ( 161.1093323826042933, 251.5974460702646809, -13.93502574894237078 ) ) ;
#20279 = CARTESIAN_POINT ( 'NONE',  ( 149.2223635749290622, 272.1862799931444670, -12.97307652490353647 ) ) ;
#20280 = VERTEX_POINT ( 'NONE', #37404 ) ;
#20281 = CARTESIAN_POINT ( 'NONE',  ( 66.20320037398873581, 68.63009258879732499, -2.167961533895922610 ) ) ;
#20282 = CARTESIAN_POINT ( 'NONE',  ( 197.8977219949227049, 287.8780861330898801, 17.48564646125164046 ) ) ;
#20283 = CARTESIAN_POINT ( 'NONE',  ( 204.6785851723931557, 274.1332865905380913, -12.34137688749581407 ) ) ;
#20284 = CARTESIAN_POINT ( 'NONE',  ( 78.13161584694131534, 61.81224900762369145, -15.72225761198293981 ) ) ;
#20285 = CARTESIAN_POINT ( 'NONE',  ( 112.6237299221286321, 226.6423013555409796, -4.594050593750043987 ) ) ;
#20286 = CARTESIAN_POINT ( 'NONE',  ( 122.2038756314442054, 231.3615022471901739, 5.000000000000051514 ) ) ;
#20287 = CARTESIAN_POINT ( 'NONE',  ( 117.0077232087375734, 228.3615022471901739, 5.000000000000051514 ) ) ;
#20288 = ORIENTED_EDGE ( 'NONE', *, *, #89441, .F. ) ;
#20289 = CARTESIAN_POINT ( 'NONE',  ( 207.5195222358739784, 271.2126392554839640, 2.810970398613041432 ) ) ;
#20290 = ORIENTED_EDGE ( 'NONE', *, *, #30736, .F. ) ;
#20291 = EDGE_LOOP ( 'NONE', ( #64518, #63078, #31375, #43416 ) ) ;
#20292 = FACE_BOUND ( 'NONE', #67722, .T. ) ;
#20293 = LINE ( 'NONE', #28373, #64481 ) ;
#20294 = CARTESIAN_POINT ( 'NONE',  ( 67.67116493723634107, 216.0024278399160380, -9.188101187500093303 ) ) ;
#20295 = ORIENTED_EDGE ( 'NONE', *, *, #52129, .T. ) ;
#20296 = DIRECTION ( 'NONE',  ( 0.08498217737244646852, 0.9963824715083250405, 0.000000000000000000 ) ) ;
#20297 = CARTESIAN_POINT ( 'NONE',  ( 81.53661897590532703, 55.80016554358400072, 16.37044094275388417 ) ) ;
#20298 = DIRECTION ( 'NONE',  ( 0.8660254037844385966, 0.5000000000000002220, 7.511572993685832627E-16 ) ) ;
#20299 = CARTESIAN_POINT ( 'NONE',  ( 172.4859759874162819, 276.8588516960780339, 15.79461614666721658 ) ) ;
#20300 = VERTEX_POINT ( 'NONE', #68310 ) ;
#20301 = EDGE_CURVE ( 'NONE', #74475, #12306, #26963, .T. ) ;
#20302 =( BOUNDED_CURVE ( )  B_SPLINE_CURVE ( 2, ( #92010, #59541, #92488, #82909, #67661, #14467, #53928, #13967, #13481 ),
 .UNSPECIFIED., .F., .T. ) 
 B_SPLINE_CURVE_WITH_KNOTS ( ( 3, 2, 2, 2, 3 ),
 ( 0.2137096774193548432, 0.2150537634408602183, 0.2177419354838709686, 0.2204301075268817189, 0.2217741935483870941 ),
 .UNSPECIFIED. ) 
 CURVE ( )  GEOMETRIC_REPRESENTATION_ITEM ( )  RATIONAL_B_SPLINE_CURVE ( ( 0.9330127018922194093, 0.9330127018922194093, 1.000000000000000000, 0.8660254037844387076, 1.000000000000000000, 0.8660254037844387076, 1.000000000000000000, 0.9330127018922194093, 0.9330127018922194093 ) ) 
 REPRESENTATION_ITEM ( '' )  );
#20303 = CARTESIAN_POINT ( 'NONE',  ( 70.17130392896066837, 64.17533599878278494, -12.55506970741091521 ) ) ;
#20304 = CARTESIAN_POINT ( 'NONE',  ( 86.70355446391526755, 43.51144900434398721, -2.455171442191615316 ) ) ;
#20305 = CARTESIAN_POINT ( 'NONE',  ( 153.4495116231415750, 264.8646448025247082, -16.73555355292144498 ) ) ;
#20306 = CARTESIAN_POINT ( 'NONE',  ( 155.2922060645262263, 261.6730044072216401, -16.98884022075611355 ) ) ;
#20307 = ORIENTED_EDGE ( 'NONE', *, *, #86286, .T. ) ;
#20308 = DIRECTION ( 'NONE',  ( -0.000000000000000000, -0.000000000000000000, -1.000000000000000000 ) ) ;
#20309 = EDGE_CURVE ( 'NONE', #96180, #79774, #8462, .T. ) ;
#20310 = CARTESIAN_POINT ( 'NONE',  ( 163.7477501808002103, 260.3652044488483739, -16.17942866797859836 ) ) ;
#20311 = DIRECTION ( 'NONE',  ( -1.000000000000000000, 0.000000000000000000, 0.000000000000000000 ) ) ;
#20312 = CARTESIAN_POINT ( 'NONE',  ( 178.3623428208658197, 294.2551730570217501, -1.850815590806885735 ) ) ;
#20313 = CARTESIAN_POINT ( 'NONE',  ( 188.5189276119756698, 259.3703232174731852, -3.088365542045595991 ) ) ;
#20314 = CIRCLE ( 'NONE', #52599, 0.1418229129681522482 ) ;
#20315 = CARTESIAN_POINT ( 'NONE',  ( 148.9285945872975390, 272.6951028054104427, -12.01265727652413240 ) ) ;
#20316 =( LENGTH_UNIT ( ) NAMED_UNIT ( * ) SI_UNIT ( .MILLI., .METRE. ) );
#20317 = ORIENTED_EDGE ( 'NONE', *, *, #62888, .F. ) ;
#20318 = CARTESIAN_POINT ( 'NONE',  ( 164.4698008747318738, 245.7769439046653019, -6.272955660526681854 ) ) ;
#20319 = CARTESIAN_POINT ( 'NONE',  ( 125.2075541532825014, 255.3464784336661353, 1.353441290958777327E-15 ) ) ;
#20320 = ORIENTED_EDGE ( 'NONE', *, *, #64941, .F. ) ;
#20321 = CARTESIAN_POINT ( 'NONE',  ( 81.35887266585007183, 44.29925860026666129, -10.01769064211159055 ) ) ;
#20322 = CARTESIAN_POINT ( 'NONE',  ( 74.34676178584531669, 66.92609087214925978, -12.92232536950610289 ) ) ;
#20323 = CARTESIAN_POINT ( 'NONE',  ( 30.49745206674571563, 75.84738672984741470, 59.99999999999999289 ) ) ;
#20324 =( BOUNDED_CURVE ( )  B_SPLINE_CURVE ( 2, ( #99412, #58878, #13797, #75608, #29989, #36090, #53289, #44184, #36587, #51288, #51812, #6196, #91832 ),
 .UNSPECIFIED., .F., .T. ) 
 B_SPLINE_CURVE_WITH_KNOTS ( ( 3, 2, 2, 2, 2, 2, 3 ),
 ( 0.8625000000000000444, 0.8649999999999999911, 0.8699999999999999956, 0.8750000000000000000, 0.8800000000000000044, 0.8850000000000000089, 0.8875000000000000666 ),
 .UNSPECIFIED. ) 
 CURVE ( )  GEOMETRIC_REPRESENTATION_ITEM ( )  RATIONAL_B_SPLINE_CURVE ( ( 0.9755282581475767101, 0.9755282581475772652, 1.000000000000000000, 0.9510565162951535312, 1.000000000000000000, 0.9510565162951535312, 1.000000000000000000, 0.9510565162951535312, 1.000000000000000000, 0.9510565162951535312, 1.000000000000000000, 0.9755282581475761550, 0.9755282581475767101 ) ) 
 REPRESENTATION_ITEM ( '' )  );
#20325 = VECTOR ( 'NONE', #37852, 1000.000000000000114 ) ;
#20326 = CARTESIAN_POINT ( 'NONE',  ( 204.3574891606595827, 276.6894411969685166, 13.41627538812899978 ) ) ;
#20327 = CARTESIAN_POINT ( 'NONE',  ( 75.11982177093736368, 62.93972712279792603, 14.81955472308038679 ) ) ;
#20328 = CARTESIAN_POINT ( 'NONE',  ( -12.68721568607400485, 24.67147432707382748, 10.00000000000000000 ) ) ;
#20329 = ORIENTED_EDGE ( 'NONE', *, *, #541, .F. ) ;
#20330 = CARTESIAN_POINT ( 'NONE',  ( 76.44304877299126133, 54.35907603249690112, 16.08959775360170141 ) ) ;
#20331 = CARTESIAN_POINT ( 'NONE',  ( 123.7735466722555628, 242.2677522451418497, 10.00000000000009592 ) ) ;
#20332 = CARTESIAN_POINT ( 'NONE',  ( 26.18314342202569023, 41.82794442100486521, -10.00000000000000000 ) ) ;
#20333 = CARTESIAN_POINT ( 'NONE',  ( 48.58805178314243278, 84.67719436603331928, -10.00000000000000000 ) ) ;
#20334 = CARTESIAN_POINT ( 'NONE',  ( 198.5140642857193711, 266.2478974292683915, 0.8911030639010785181 ) ) ;
#20335 = CARTESIAN_POINT ( 'NONE',  ( 79.99999999999998579, 9.999999999999985789, -2.622423327744149102 ) ) ;
#20336 = CARTESIAN_POINT ( 'NONE',  ( 175.1250016605062285, 291.8388325744778058, -4.493358603852836808 ) ) ;
#20337 = CARTESIAN_POINT ( 'NONE',  ( 192.8304677249058727, 268.4476542952539262, 12.38602397553101397 ) ) ;
#20338 = EDGE_CURVE ( 'NONE', #60492, #23235, #49936, .T. ) ;
#20339 = CARTESIAN_POINT ( 'NONE',  ( 15.42909579892843652, 33.00034080476290654, -1.878358725466461243E-16 ) ) ;
#20340 = CARTESIAN_POINT ( 'NONE',  ( 149.2561433752359505, 272.1277716627430436, 12.99353668144589946 ) ) ;
#20341 = CYLINDRICAL_SURFACE ( 'NONE', #32104, 10.00000000000010658 ) ;
#20342 = DIRECTION ( 'NONE',  ( -0.2347357813929480952, 0.4065742997269687908, 0.8829475928589233247 ) ) ;
#20343 = CARTESIAN_POINT ( 'NONE',  ( 203.2369479875374623, 278.6302754407888074, -16.66242713208754367 ) ) ;
#20344 = ADVANCED_FACE ( 'NONE', ( #68371 ), #29678, .T. ) ;
#20345 = CARTESIAN_POINT ( 'NONE',  ( 161.3777720748676643, 251.1324948844963387, 14.05949999684680307 ) ) ;
#20346 = CARTESIAN_POINT ( 'NONE',  ( 135.3927208396968354, 235.6427522451417360, 1.119607411625061291E-15 ) ) ;
#20347 = EDGE_CURVE ( 'NONE', #28481, #82871, #98428, .T. ) ;
#20348 = CARTESIAN_POINT ( 'NONE',  ( 172.3600298132898843, 283.6594854551991034, -12.44358114520080960 ) ) ;
#20349 = VERTEX_POINT ( 'NONE', #29876 ) ;
#20350 = EDGE_CURVE ( 'NONE', #36629, #9601, #22116, .T. ) ;
#20351 = PRODUCT_DEFINITION_FORMATION_WITH_SPECIFIED_SOURCE ( 'ANY', '', #65334, .NOT_KNOWN. ) ;
#20352 = FACE_OUTER_BOUND ( 'NONE', #38170, .T. ) ;
#20353 = CARTESIAN_POINT ( 'NONE',  ( 199.0363797504450929, 285.9058730480928716, -17.12190301149298222 ) ) ;
#20354 = CARTESIAN_POINT ( 'NONE',  ( 0.9332558059805314832, 171.3458772461660544, 9.188101187500095079 ) ) ;
#20355 = CARTESIAN_POINT ( 'NONE',  ( 59.55252387252222945, 199.0643266524159856, -9.188101187500093303 ) ) ;
#20356 = CARTESIAN_POINT ( 'NONE',  ( 85.72142767485377135, 44.68916939864112692, 8.082118614619203001 ) ) ;
#20357 = CARTESIAN_POINT ( 'NONE',  ( 27.11554978534049098, 17.78380873178787169, -6.180339887498949025 ) ) ;
#20358 = CARTESIAN_POINT ( 'NONE',  ( 85.37538261767947745, 48.57005942898851458, 12.46403972397472337 ) ) ;
#20359 = CARTESIAN_POINT ( 'NONE',  ( 157.1269483542914998, 258.4951375425532092, -17.15328932028234377 ) ) ;
#20360 = CARTESIAN_POINT ( 'NONE',  ( 72.30772874869472844, 72.01587971836859481, -3.568979074609765600 ) ) ;
#20361 = CARTESIAN_POINT ( 'NONE',  ( 74.06184603777616360, 55.64324239481884860, -16.58750451651802393 ) ) ;
#20362 = CARTESIAN_POINT ( 'NONE',  ( 167.5986172622920662, 256.5940544082843644, 13.72151094899553847 ) ) ;
#20363 = CARTESIAN_POINT ( 'NONE',  ( 180.9290680551475532, 256.0398517639778220, 1.989246424408670499 ) ) ;
#20364 = CARTESIAN_POINT ( 'NONE',  ( 198.6859012307616581, 286.5129196511462624, 18.23225590904412030 ) ) ;
#20365 = CARTESIAN_POINT ( 'NONE',  ( 179.1279496731769996, 294.4181628194133395, 1.067429419934537105 ) ) ;
#20366 = CARTESIAN_POINT ( 'NONE',  ( 52.48883062679681899, 211.1115022471903444, -5.000000000000047962 ) ) ;
#20367 = FACE_OUTER_BOUND ( 'NONE', #84589, .T. ) ;
#20368 = EDGE_CURVE ( 'NONE', #2785, #35157, #81010, .T. ) ;
#20369 = B_SPLINE_CURVE_WITH_KNOTS ( 'NONE', 3,
 ( #75699, #28087, #98511, #36176, #44766, #21014, #90939, #43775, #6784, #68574, #60461, #14871, #21489, #6286, #99001, #45274 ),
 .UNSPECIFIED., .F., .F.,
 ( 4, 1, 2, 2, 2, 1, 2, 2, 4 ),
 ( 0.000000000000000000, 0.1250000000000009159, 0.1874999999999999167, 0.2499999999999989453, 0.5000000000000002220, 0.6250000000000007772, 0.6875000000000014433, 0.7500000000000021094, 1.000000000000000000 ),
 .UNSPECIFIED. ) ;
#20370 = CARTESIAN_POINT ( 'NONE',  ( 147.6430623265936219, 274.9217099957185155, 8.258152514891218487 ) ) ;
#20371 = CARTESIAN_POINT ( 'NONE',  ( 19.47135178391741661, 191.2369531367911293, -4.594050593750048428 ) ) ;
#20372 = CARTESIAN_POINT ( 'NONE',  ( 72.85625868234197355, 71.07309412281131245, -7.586526616956829727 ) ) ;
#20373 = CARTESIAN_POINT ( 'NONE',  ( 192.6224552386041182, 297.0151161785129261, 12.49354144254605181 ) ) ;
#20374 = CARTESIAN_POINT ( 'NONE',  ( 33.10845880387886808, 31.06628583063843863, -9.188101187500006262 ) ) ;
#20375 = DIRECTION ( 'NONE',  ( 0.3371987438498061929, -0.9414334852479556703, 0.000000000000000000 ) ) ;
#20376 = CARTESIAN_POINT ( 'NONE',  ( 164.8670003495851404, 245.0889742334797177, -1.557028074864921674 ) ) ;
#20377 = CARTESIAN_POINT ( 'NONE',  ( 175.1378461883211912, 279.3152656845848583, 16.63146252814350134 ) ) ;
#20378 = CARTESIAN_POINT ( 'NONE',  ( 176.3865323452404823, 258.8737835494043225, 13.24306684835586623 ) ) ;
#20379 = LINE ( 'NONE', #64983, #21240 ) ;
#20380 =( NAMED_UNIT ( * ) PLANE_ANGLE_UNIT ( ) SI_UNIT ( $, .RADIAN. ) );
#20381 = CARTESIAN_POINT ( 'NONE',  ( 11.44039960990914651, 28.64646525600389282, -2.839279412974133887 ) ) ;
#20382 = CARTESIAN_POINT ( 'NONE',  ( 71.48480579176157335, 72.35852322450823237, 1.080755764661545548 ) ) ;
#20383 = CARTESIAN_POINT ( 'NONE',  ( 82.37037437367128234, 54.25728867273632261, 15.61855531662249419 ) ) ;
#20384 = FACE_OUTER_BOUND ( 'NONE', #17787, .T. ) ;
#20385 = VECTOR ( 'NONE', #91129, 1000.000000000000114 ) ;
#20386 = CARTESIAN_POINT ( 'NONE',  ( 46.88368875251780565, 110.3874725885333135, -10.00000000000000000 ) ) ;
#20387 = ORIENTED_EDGE ( 'NONE', *, *, #989, .F. ) ;
#20388 = B_SPLINE_CURVE_WITH_KNOTS ( 'NONE', 3,
 ( #24733, #1458, #1950, #63744 ),
 .UNSPECIFIED., .F., .F.,
 ( 4, 4 ),
 ( 0.007614618424699901196, 0.01267886371662555085 ),
 .UNSPECIFIED. ) ;
#20389 = CYLINDRICAL_SURFACE ( 'NONE', #22110, 17.82106496071139645 ) ;
#20390 = CARTESIAN_POINT ( 'NONE',  ( 27.73347817269569404, 16.41603393254326093, -1.583844403245362020 ) ) ;
#20391 = CARTESIAN_POINT ( 'NONE',  ( 81.35225493641259220, 42.04531462148436560, 7.888897770668004128 ) ) ;
#20392 = CARTESIAN_POINT ( 'NONE',  ( 42.55442611339157111, 60.96799964870729127, 177.5919119679930134 ) ) ;
#20393 = ORIENTED_EDGE ( 'NONE', *, *, #19417, .F. ) ;
#20394 = CARTESIAN_POINT ( 'NONE',  ( 192.6224552386041182, 297.0151161785129261, 12.49354144254605181 ) ) ;
#20395 = CARTESIAN_POINT ( 'NONE',  ( 67.24554735707404518, 69.34905625991120814, 1.330410485716284397 ) ) ;
#20396 = AXIS2_PLACEMENT_3D ( 'NONE', #36719, #60013, #4338 ) ;
#20397 = CARTESIAN_POINT ( 'NONE',  ( 66.77752810875767864, 68.40544692769398694, 4.459354299965309743 ) ) ;
#20398 = CARTESIAN_POINT ( 'NONE',  ( 203.4357368910538355, 278.2859629599173559, -16.45855118664066197 ) ) ;
#20399 = ORIENTED_EDGE ( 'NONE', *, *, #77995, .T. ) ;
#20400 = ORIENTED_EDGE ( 'NONE', *, *, #22167, .T. ) ;
#20402 = CARTESIAN_POINT ( 'NONE',  ( 164.3330377059402849, 246.0138246616164110, 7.208046019122525294 ) ) ;
#20401 = CARTESIAN_POINT ( 'NONE',  ( 159.7607676839680835, 278.6090423769052222, -9.664001967995806908 ) ) ;
#20403 = CARTESIAN_POINT ( 'NONE',  ( 153.3920560952016956, 264.9641606960921649, 16.50453917291963535 ) ) ;
#20404 = ORIENTED_EDGE ( 'NONE', *, *, #80391, .F. ) ;
#20405 = CARTESIAN_POINT ( 'NONE',  ( 88.12308754723774484, 43.81089488678613009, -2.128676964009123651 ) ) ;
#20406 = CARTESIAN_POINT ( 'NONE',  ( 80.50883317518791671, 57.72730120993125524, 16.59589928958307326 ) ) ;
#20407 = CARTESIAN_POINT ( 'NONE',  ( 177.3985541943506803, 263.1773983921460740, 15.48418877813238481 ) ) ;
#20408 = ORIENTED_EDGE ( 'NONE', *, *, #22000, .T. ) ;
#20409 = LINE ( 'NONE', #82742, #44269 ) ;
#20410 = CARTESIAN_POINT ( 'NONE',  ( 78.83915903249749135, 50.24778389138201362, -14.90005401999855295 ) ) ;
#20411 = CARTESIAN_POINT ( 'NONE',  ( 197.0184425104562820, 289.4010428742387262, -16.90752553128928426 ) ) ;
#20412 = EDGE_CURVE ( 'NONE', #90974, #25829, #37687, .T. ) ;
#20413 = VERTEX_POINT ( 'NONE', #56153 ) ;
#20414 = CARTESIAN_POINT ( 'NONE',  ( 164.5648480107187197, 245.6123174360222094, 3.015887571020871238 ) ) ;
#20415 = VECTOR ( 'NONE', #45830, 1000.000000000000114 ) ;
#20416 = CARTESIAN_POINT ( 'NONE',  ( 73.94609423987252228, 60.77720215842664686, 15.26334679630400259 ) ) ;
#20417 = EDGE_LOOP ( 'NONE', ( #65504, #18088, #9084, #5464 ) ) ;
#20418 = CARTESIAN_POINT ( 'NONE',  ( 177.3086487836147285, 279.3000926714664160, -16.75854559346873884 ) ) ;
#20419 = CARTESIAN_POINT ( 'NONE',  ( 172.2724355110944146, 263.6426226643334303, -15.46355804232799258 ) ) ;
#20420 = EDGE_LOOP ( 'NONE', ( #74488, #2543, #38087, #32961 ) ) ;
#20421 = CARTESIAN_POINT ( 'NONE',  ( 186.0942368718926332, 293.1614520422483565, 12.28461848767796560 ) ) ;
#20422 = AXIS2_PLACEMENT_3D ( 'NONE', #73545, #11264, #12247 ) ;
#20423 = ORIENTED_EDGE ( 'NONE', *, *, #20676, .F. ) ;
#20424 = CARTESIAN_POINT ( 'NONE',  ( 158.0081726929925594, 269.0575936612110013, 15.62741947982547508 ) ) ;
#20425 = EDGE_LOOP ( 'NONE', ( #99903, #7799, #100018, #2495 ) ) ;
#20426 = CARTESIAN_POINT ( 'NONE',  ( 73.07250412799626815, 69.64252590750851368, 9.183134884877944160 ) ) ;
#20427 = CARTESIAN_POINT ( 'NONE',  ( 190.4976253092930278, 300.6954295735222900, -5.764807383508308902 ) ) ;
#20428 = CARTESIAN_POINT ( 'NONE',  ( 83.01075186827047503, 53.40825386585735401, 15.63370843945822664 ) ) ;
#20429 = CARTESIAN_POINT ( 'NONE',  ( -27.42236680055714260, 166.5217562850347406, 1.224646799147364892E-15 ) ) ;
#20430 = CARTESIAN_POINT ( 'NONE',  ( 153.4578721839791342, 264.8501638863745029, 16.85421393845643223 ) ) ;
#20431 = CARTESIAN_POINT ( 'NONE',  ( 178.2182531100257279, 291.4184198334916687, 6.077856116893014082 ) ) ;
#20432 = CARTESIAN_POINT ( 'NONE',  ( 158.4500152958133015, 256.2035183780225793, -16.27180754986873268 ) ) ;
#20433 = ORIENTED_EDGE ( 'NONE', *, *, #26815, .T. ) ;
#20434 = CARTESIAN_POINT ( 'NONE',  ( 77.02178492951776434, 57.00973823531708717, -16.18317106599237221 ) ) ;
#20436 = CARTESIAN_POINT ( 'NONE',  ( 165.0308887387863876, 244.8051112166122891, 1.948365933089477808 ) ) ;
#20435 = CARTESIAN_POINT ( 'NONE',  ( 77.47012825831066607, 49.73992442231940458, -15.48190979613537799 ) ) ;
#20438 = ORIENTED_EDGE ( 'NONE', *, *, #98662, .F. ) ;
#20437 = CARTESIAN_POINT ( 'NONE',  ( 34.75566377745538205, 179.3262482093457493, 3.021315404115420679E-15 ) ) ;
#20439 = LINE ( 'NONE', #48964, #57965 ) ;
#20440 = CARTESIAN_POINT ( 'NONE',  ( 87.63467585155270001, 44.53258862333366608, 5.717273570526079318 ) ) ;
#20441 = ORIENTED_EDGE ( 'NONE', *, *, #47542, .T. ) ;
#20442 = CARTESIAN_POINT ( 'NONE',  ( 71.49018766940498892, 68.39238998699252647, 9.502106742351175583 ) ) ;
#20443 = CARTESIAN_POINT ( 'NONE',  ( 86.09778053344243176, 44.42558544415346944, 7.284472041480639426 ) ) ;
#20444 = CARTESIAN_POINT ( 'NONE',  ( 189.6768609436964539, 274.4077930505946483, -17.07046811116321550 ) ) ;
#20445 = B_SPLINE_CURVE_WITH_KNOTS ( 'NONE', 3,
 ( #68849, #92213, #20787, #13189, #84599, #22767, #61246, #75480, #28875, #66862, #60239, #98791, #6572, #53644, #59238, #53160, #15137, #59751, #68354, #99770, #51678, #74985, #36456, #84115, #67359, #91200, #52647, #91694, #14667, #46034, #90722, #21277, #76475, #76951, #45543, #82627, #44045, #52154, #83103, #6064, #21760, #70868, #39931, #15642, #463, #54133, #61746, #7551 ),
 .UNSPECIFIED., .F., .F.,
 ( 4, 2, 2, 2, 2, 2, 2, 2, 2, 2, 2, 2, 2, 2, 2, 2, 2, 2, 2, 2, 2, 2, 2, 4 ),
 ( 0.0008122609998851836348, 0.001014663487969617254, 0.001115864732011832058, 0.001217065976054046861, 0.001318267220096261882, 0.001419468464138476903, 0.001621870952222960720, 0.002026675928391991673, 0.002431480904561022626, 0.003241090856899082797, 0.004050700809237142534, 0.004860310761575202705, 0.005265115737744153861, 0.005467518225828587805, 0.005568719469870849446, 0.005619320091892030140, 0.005669920713913210834, 0.005771121957955572222, 0.005872323201997933610, 0.006074725690082618222, 0.006479530666252108877, 0.006884335642421599531, 0.007086738130506338787, 0.007289140618591078910 ),
 .UNSPECIFIED. ) ;
#20446 = CARTESIAN_POINT ( 'NONE',  ( 159.9972970628961377, 253.5235477438103544, -14.85214688666258809 ) ) ;
#20447 = CARTESIAN_POINT ( 'NONE',  ( 102.3056452726415984, 218.3262482093457493, 3.021315404115420679E-15 ) ) ;
#20448 = EDGE_LOOP ( 'NONE', ( #46011, #62241, #71129, #64012 ) ) ;
#20449 = CARTESIAN_POINT ( 'NONE',  ( 163.2256942281324541, 247.9317998266098471, -9.780520296312531059 ) ) ;
#20450 = CARTESIAN_POINT ( 'NONE',  ( 85.21461723709045089, 46.08533025597601807, 10.27714634765069057 ) ) ;
#20451 = CARTESIAN_POINT ( 'NONE',  ( 201.0732166862245549, 282.3779679885897167, -18.18766936363638820 ) ) ;
#20452 = CARTESIAN_POINT ( 'NONE',  ( 207.6860335175200589, 270.9242332556395922, 6.913225035677485586 ) ) ;
#20453 = CARTESIAN_POINT ( 'NONE',  ( 31.46967238556409896, 195.6427522451418781, -10.00000000000009415 ) ) ;
#20454 = CARTESIAN_POINT ( 'NONE',  ( 121.7437996339097310, 241.0958772461660544, -9.188101187500095079 ) ) ;
#20455 = CARTESIAN_POINT ( 'NONE',  ( -1.087500518889665591, 25.57194971796827332, -10.00000000000000000 ) ) ;
#20456 = CARTESIAN_POINT ( 'NONE',  ( 164.9401169542619243, 280.4943389099253181, -11.14461050731500436 ) ) ;
#20457 = CARTESIAN_POINT ( 'NONE',  ( 195.7617614321055157, 291.5776783508526364, 16.33009124109666033 ) ) ;
#20458 = CARTESIAN_POINT ( 'NONE',  ( 208.3408670980087152, 269.7900282237308147, 2.175586895783760077 ) ) ;
#20459 = CARTESIAN_POINT ( 'NONE',  ( 35.49282175392953320, 200.4869531367911293, 4.594050593750046652 ) ) ;
#20460 = LINE ( 'NONE', #44717, #77002 ) ;
#20461 = ORIENTED_EDGE ( 'NONE', *, *, #60741, .F. ) ;
#20462 = VERTEX_POINT ( 'NONE', #39947 ) ;
#20463 = CARTESIAN_POINT ( 'NONE',  ( -22.42236680055709641, 157.8615022471902591, 0.000000000000000000 ) ) ;
#20464 = CARTESIAN_POINT ( 'NONE',  ( 185.2758064758799890, 259.6671588269117592, -5.400835621108775797 ) ) ;
#20465 = ADVANCED_FACE ( 'NONE', ( #49081 ), #70884, .T. ) ;
#20466 = CARTESIAN_POINT ( 'NONE',  ( 70.71732918945153301, 71.45486987150104596, -1.088542012041604945 ) ) ;
#20467 = AXIS2_PLACEMENT_3D ( 'NONE', #14450, #44831, #75764 ) ;
#20468 = CARTESIAN_POINT ( 'NONE',  ( 41.47569090598248920, 209.1868197944957899, -17.47570218321533631 ) ) ;
#20469 = CARTESIAN_POINT ( 'NONE',  ( 97.33941792859064890, 238.5530062829863027, -4.648177544792955347E-16 ) ) ;
#20470 = CARTESIAN_POINT ( 'NONE',  ( 161.5757715694810770, 250.7895496999525449, -14.51803553215175135 ) ) ;
#20471 = EDGE_CURVE ( 'NONE', #98305, #28495, #72106, .T. ) ;
#20472 = CARTESIAN_POINT ( 'NONE',  ( 179.3343052093286758, 287.9874940019028031, -12.72641108234611096 ) ) ;
#20473 = CARTESIAN_POINT ( 'NONE',  ( 45.86253193465722688, 68.41350641406140198, 10.00000000000000000 ) ) ;
#20474 = CARTESIAN_POINT ( 'NONE',  ( 101.6177300921037130, 216.1427522451417929, 1.119607411625061291E-15 ) ) ;
#20475 = ORIENTED_EDGE ( 'NONE', *, *, #63363, .F. ) ;
#20476 = B_SPLINE_CURVE_WITH_KNOTS ( 'NONE', 3,
 ( #19290, #89707, #50643, #58731, #44531, #12165, #35452, #5552, #82105, #11677 ),
 .UNSPECIFIED., .F., .F.,
 ( 4, 2, 2, 2, 4 ),
 ( 0.000000000000000000, 0.0002622400424273775392, 0.0005244800848547550784, 0.0007867201272821326176, 0.001048960169709510157 ),
 .UNSPECIFIED. ) ;
#20477 = CARTESIAN_POINT ( 'NONE',  ( 194.8868098799860888, 266.4408012034644457, -7.738736915655594295 ) ) ;
#20478 = EDGE_CURVE ( 'NONE', #63734, #25515, #17266, .T. ) ;
#20479 = CARTESIAN_POINT ( 'NONE',  ( 162.8996025780091941, 248.4966071325470125, 11.23567065566008516 ) ) ;
#20480 = CARTESIAN_POINT ( 'NONE',  ( 208.3226489551340990, 269.8215829728092103, -1.240262689467544366 ) ) ;
#20481 = CARTESIAN_POINT ( 'NONE',  ( 20.58138070222249638, 176.5643266524160140, -9.188101187500093303 ) ) ;
#20482 = CARTESIAN_POINT ( 'NONE',  ( 73.80638704669732419, 68.31061168272384521, -11.57820046455322149 ) ) ;
#20483 = VECTOR ( 'NONE', #15159, 1000.000000000000114 ) ;
#20484 = CARTESIAN_POINT ( 'NONE',  ( 81.13898030988220000, 55.16162329238864004, 16.30930592844974569 ) ) ;
#20485 = CARTESIAN_POINT ( 'NONE',  ( 71.62205979867658812, 59.06269311622425988, -15.34006186618645273 ) ) ;
#20486 = CARTESIAN_POINT ( 'NONE',  ( 71.92052582790191195, 72.15815999434336447, -1.685033094989828228 ) ) ;
#20487 = B_SPLINE_CURVE_WITH_KNOTS ( 'NONE', 3,
 ( #21027, #44288, #27124, #11926, #65601, #73226, #19038, #98524, #50897, #58490, #49910, #58006, #11440, #88986, #34700, #81846, #19540, #42782, #35705, #66603, #92433, #76221, #30597, #61483, #99512, #22980, #70077, #22494, #60474, #53869, #38168, #691, #84831, #68589, #52392, #61967, #15369, #30096, #23473, #92920, #6797, #46267, #77190, #31574, #7797, #45287, #37677, #46794, #38682, #69586, #54364, #90951, #69086, #85337 ),
 .UNSPECIFIED., .F., .F.,
 ( 4, 2, 2, 2, 2, 2, 2, 2, 2, 2, 2, 2, 2, 2, 2, 2, 2, 2, 2, 2, 2, 2, 2, 2, 2, 2, 4 ),
 ( 0.0008054865245305401020, 0.001006788277830038053, 0.001107439154479787028, 0.001208090031129536003, 0.001308740907779284979, 0.001409391784429033737, 0.001610693537728460564, 0.002013297044327447358, 0.002415900550926434152, 0.003221107564124476262, 0.004026314577322517504, 0.004831521590520558747, 0.005234125097119579802, 0.005435426850419054767, 0.005536077727068828246, 0.005586403165393787409, 0.005636728603718745706, 0.005687054042043704870, 0.005737379480368664034, 0.005838030357018627464, 0.006039332110318513559, 0.006240633863618400522, 0.006441935616918286617, 0.006643237370218172712, 0.006844539123518058807, 0.007045840876817945769, 0.007247142630117831864 ),
 .UNSPECIFIED. ) ;
#20488 = CARTESIAN_POINT ( 'NONE',  ( 55.81761577081934433, 203.0333772461660544, 9.188101187500095079 ) ) ;
#20489 = CARTESIAN_POINT ( 'NONE',  ( 41.10966550219804816, 207.8207943907112565, -17.47570218321534696 ) ) ;
#20490 = CARTESIAN_POINT ( 'NONE',  ( -32.30932376655839988, 25.48519649537502119, 10.00000000000000000 ) ) ;
#20491 = CARTESIAN_POINT ( 'NONE',  ( 71.76351473723394747, 71.84897031608997509, 2.971691788643012977 ) ) ;
#20492 = CARTESIAN_POINT ( 'NONE',  ( 66.06994105266723238, 68.53505336611841869, -4.562350030803943746 ) ) ;
#20493 = ORIENTED_EDGE ( 'NONE', *, *, #7079, .F. ) ;
#20494 = AXIS2_PLACEMENT_3D ( 'NONE', #68580, #99505, #55361 ) ;
#20495 = CARTESIAN_POINT ( 'NONE',  ( -2.070769811622824363, 179.6115022471903160, -5.000000000000047962 ) ) ;
#20496 = CARTESIAN_POINT ( 'NONE',  ( 46.74097198175142154, 116.0488203434314727, 10.00000000000000000 ) ) ;
#20497 = CARTESIAN_POINT ( 'NONE',  ( 133.4083396129551602, 238.6423013555409796, -4.594050593750043987 ) ) ;
#20498 = CARTESIAN_POINT ( 'NONE',  ( 28.09632999608277615, 19.14754757982091604, -5.678558825948276656 ) ) ;
#20499 = CARTESIAN_POINT ( 'NONE',  ( 83.62455065227555906, 52.34512318633653649, -15.13772682721065621 ) ) ;
#20500 = CARTESIAN_POINT ( 'NONE',  ( 71.88281838930642209, 59.56282477439597756, -15.74156321294392313 ) ) ;
#20502 = CARTESIAN_POINT ( 'NONE',  ( 74.78994931159289195, 67.11760897871008069, 12.96302903502453852 ) ) ;
#20501 = CARTESIAN_POINT ( 'NONE',  ( 196.0355168007595523, 291.1035201434990540, 17.55377893960077884 ) ) ;
#20503 = CARTESIAN_POINT ( 'NONE',  ( 150.5052742266933876, 269.9642135627172479, -13.76496694288080391 ) ) ;
#20504 = ORIENTED_EDGE ( 'NONE', *, *, #1513, .F. ) ;
#20505 = CARTESIAN_POINT ( 'NONE',  ( 151.3589047706063582, 268.4856820897672378, 14.56544807350869419 ) ) ;
#20506 = CARTESIAN_POINT ( 'NONE',  ( 207.8730126074944451, 270.6003759718510651, -1.781618945033869306 ) ) ;
#20507 = CARTESIAN_POINT ( 'NONE',  ( -10.54235908185773418, 24.92402704602492847, 10.00000000000000000 ) ) ;
#20508 = CARTESIAN_POINT ( 'NONE',  ( 169.7497442303230173, 266.0831907009023212, -17.38058090311056603 ) ) ;
#20509 = CARTESIAN_POINT ( 'NONE',  ( 197.2070174366134836, 273.4893232311666793, -14.13887660181231709 ) ) ;
#20510 = EDGE_LOOP ( 'NONE', ( #12819, #50067, #64992, #25275, #70880, #10061 ) ) ;
#20511 = CARTESIAN_POINT ( 'NONE',  ( 69.78176895985124872, 68.40769324273578889, 8.076221664042178006 ) ) ;
#20512 = PRODUCT_RELATED_PRODUCT_CATEGORY ( 'part', '', ( #89683 ) ) ;
#20513 = CARTESIAN_POINT ( 'NONE',  ( 169.5642877124303709, 282.9217698259369058, -10.96075264092123902 ) ) ;
#20514 = CARTESIAN_POINT ( 'NONE',  ( 84.25291518742466224, 43.27603625466485227, 6.026143753377182222 ) ) ;
#20515 = CARTESIAN_POINT ( 'NONE',  ( -13.11024591527734628, 6.000000000000000000, 32.50000000000000000 ) ) ;
#20516 = CARTESIAN_POINT ( 'NONE',  ( 185.7432137520750359, 296.9624951973794396, 5.510464551842103376 ) ) ;
#20517 = CARTESIAN_POINT ( 'NONE',  ( 148.9549916732168811, 245.2592609112379876, 2.679491924311254714 ) ) ;
#20518 = CARTESIAN_POINT ( 'NONE',  ( 148.4905408331877084, 273.9803389716664697, -7.981520963315253070 ) ) ;
#20519 = CARTESIAN_POINT ( 'NONE',  ( -22.42236680055709641, 157.8615022471902591, 0.000000000000000000 ) ) ;
#20520 = CARTESIAN_POINT ( 'NONE',  ( 9.089523648746947515, 28.18080186712591484, 3.090169943749475401 ) ) ;
#20521 = CARTESIAN_POINT ( 'NONE',  ( 84.21906065053772750, 49.13438831735580692, 13.33485874824731887 ) ) ;
#20522 = ORIENTED_EDGE ( 'NONE', *, *, #71582, .T. ) ;
#20523 = CARTESIAN_POINT ( 'NONE',  ( 73.67256625907812406, 55.34600686115704349, 16.59066767443098911 ) ) ;
#20524 = CARTESIAN_POINT ( 'NONE',  ( 86.17560058389634037, 46.94341623220315540, -10.60084123426473113 ) ) ;
#20525 = DIRECTION ( 'NONE',  ( 0.3374500364938339270, 0.9413434404457866611, 0.000000000000000000 ) ) ;
#20526 = ORIENTED_EDGE ( 'NONE', *, *, #64042, .T. ) ;
#20527 = CARTESIAN_POINT ( 'NONE',  ( 191.6723191112861855, 298.6608002251342100, -9.737039817265848995 ) ) ;
#20528 = CARTESIAN_POINT ( 'NONE',  ( 185.5314771523295292, 291.0755628727823705, 12.15834007696259711 ) ) ;
#20529 = CARTESIAN_POINT ( 'NONE',  ( 204.4325665793906524, 276.5594032932251594, 13.33817701435311598 ) ) ;
#20531 = EDGE_CURVE ( 'NONE', #1361, #45554, #10082, .T. ) ;
#20530 = AXIS2_PLACEMENT_3D ( 'NONE', #63399, #64401, #17294 ) ;
#20532 = CARTESIAN_POINT ( 'NONE',  ( -19.65312891409030271, 93.06504152958497400, 10.00000000000000888 ) ) ;
#20533 = ORIENTED_EDGE ( 'NONE', *, *, #71364, .T. ) ;
#20534 = CARTESIAN_POINT ( 'NONE',  ( 84.12564760914067108, 225.5024278399160949, 9.188101187500095079 ) ) ;
#20535 = CARTESIAN_POINT ( 'NONE',  ( 154.9899569171280973, 262.1965152870598104, 17.85248177135828485 ) ) ;
#20536 = AXIS2_PLACEMENT_3D ( 'NONE', #75993, #36454, #6570 ) ;
#20537 = CARTESIAN_POINT ( 'NONE',  ( 181.1762993832780353, 271.6239722135371721, -17.18960871778338273 ) ) ;
#20538 = CARTESIAN_POINT ( 'NONE',  ( 81.38242352901214360, 41.99299366561535862, -7.776076777262098005 ) ) ;
#20539 = ORIENTED_EDGE ( 'NONE', *, *, #76944, .T. ) ;
#20540 = ORIENTED_EDGE ( 'NONE', *, *, #8290, .F. ) ;
#20541 = AXIS2_PLACEMENT_3D ( 'NONE', #72146, #26042, #87899 ) ;
#20542 = VERTEX_POINT ( 'NONE', #24767 ) ;
#20543 = CARTESIAN_POINT ( 'NONE',  ( 80.60080754873929720, 47.19651915616773152, 12.86587752985571420 ) ) ;
#20545 = ADVANCED_FACE ( 'NONE', ( #47564 ), #63773, .F. ) ;
#20544 = ORIENTED_EDGE ( 'NONE', *, *, #22284, .T. ) ;
#20546 = CARTESIAN_POINT ( 'NONE',  ( 159.4159393015865476, 258.5086116838130010, 17.42071531078585522 ) ) ;
#20547 = CYLINDRICAL_SURFACE ( 'NONE', #96304, 70.00000000000002842 ) ;
#20548 = ORIENTED_EDGE ( 'NONE', *, *, #88172, .F. ) ;
#20549 = CARTESIAN_POINT ( 'NONE',  ( 206.9526720368717463, 272.1944526004363070, -6.912324681932258130 ) ) ;
#20550 = DIRECTION ( 'NONE',  ( 0.4999999999999998890, -0.8660254037844385966, 0.000000000000000000 ) ) ;
#20552 = EDGE_CURVE ( 'NONE', #41822, #12543, #28399, .T. ) ;
#20551 = LINE ( 'NONE', #29630, #47911 ) ;
#20553 = CARTESIAN_POINT ( 'NONE',  ( 148.0826818691893152, 274.1602666119424043, -9.371267383421741926 ) ) ;
#20554 = CARTESIAN_POINT ( 'NONE',  ( 73.20575453205489680, 68.08741268818161529, -10.93745744334090908 ) ) ;
#20555 = CARTESIAN_POINT ( 'NONE',  ( 165.1083560551384721, 265.3609356111044804, -16.61290852168901822 ) ) ;
#20556 = CARTESIAN_POINT ( 'NONE',  ( 76.33261713024396045, 57.84772012576796385, 16.09447198771029619 ) ) ;
#20557 = CARTESIAN_POINT ( 'NONE',  ( 12.79414888559916719, 13.10170272979925166, -7.433330006724141015 ) ) ;
#20558 = ORIENTED_EDGE ( 'NONE', *, *, #3944, .F. ) ;
#20559 = AXIS2_PLACEMENT_3D ( 'NONE', #26068, #58440, #12877 ) ;
#20560 = CARTESIAN_POINT ( 'NONE',  ( 195.6491688553082611, 270.3377900390409536, -13.51386470325394917 ) ) ;
#20562 = ORIENTED_EDGE ( 'NONE', *, *, #39641, .F. ) ;
#20561 = CARTESIAN_POINT ( 'NONE',  ( 199.9472389266075254, 270.2118812112473165, 9.338481273082759770 ) ) ;
#20563 = CARTESIAN_POINT ( 'NONE',  ( 162.9466247808429102, 248.4151622881552441, 11.25765811906727443 ) ) ;
#20564 = CARTESIAN_POINT ( 'NONE',  ( 191.2190380946134951, 260.9445496458436651, 3.106810577783889915 ) ) ;
#20565 = CARTESIAN_POINT ( 'NONE',  ( 149.1167591741855745, 276.2932744649320966, -5.492527394273915675 ) ) ;
#20566 = CARTESIAN_POINT ( 'NONE',  ( 70.50919596007410917, 60.88441437683223256, 14.47383098058850948 ) ) ;
#20567 = VECTOR ( 'NONE', #62848, 1000.000000000000114 ) ;
#20568 = CARTESIAN_POINT ( 'NONE',  ( 192.6560265352977410, 292.3260843751113498, -14.38534841386452534 ) ) ;
#20569 = CARTESIAN_POINT ( 'NONE',  ( 168.0406546387621631, 252.9712069534065222, 11.80637672277989481 ) ) ;
#20570 = CARTESIAN_POINT ( 'NONE',  ( 88.24711315651565258, 44.33861006782984759, -2.398047594449144615 ) ) ;
#20571 = ORIENTED_EDGE ( 'NONE', *, *, #31289, .F. ) ;
#20572 = CARTESIAN_POINT ( 'NONE',  ( 155.5889810493316929, 261.1589750551232214, -18.49677816280062714 ) ) ;
#20573 = CARTESIAN_POINT ( 'NONE',  ( 77.01640707515133499, 61.48716887149203814, -15.64119200545269983 ) ) ;
#20574 = ORIENTED_EDGE ( 'NONE', *, *, #83531, .T. ) ;
#20575 = CARTESIAN_POINT ( 'NONE',  ( 190.1774295428112396, 299.2500249094251217, 7.542682482482700124 ) ) ;
#20576 = CARTESIAN_POINT ( 'NONE',  ( 172.6505904036989136, 280.8448313155626579, -15.39888677054324440 ) ) ;
#20577 = CARTESIAN_POINT ( 'NONE',  ( 164.1338920432579300, 246.3587550674890565, -8.095503919041194152 ) ) ;
#20578 = CARTESIAN_POINT ( 'NONE',  ( 190.6661865267473104, 300.4034729807058852, 4.523489664447863490 ) ) ;
#20579 = CARTESIAN_POINT ( 'NONE',  ( 164.7829470492978601, 274.1661399048329031, 15.02517063526678420 ) ) ;
#20581 = CARTESIAN_POINT ( 'NONE',  ( 87.88164403350640441, 44.18371841277615175, 2.790213129378243728 ) ) ;
#20580 = CARTESIAN_POINT ( 'NONE',  ( 161.4353714413109344, 281.4025874958057329, -6.883957629530069511 ) ) ;
#20582 = CARTESIAN_POINT ( 'NONE',  ( 200.0915598631207786, 267.8243757013111690, 6.133940993518010920 ) ) ;
#20583 = VERTEX_POINT ( 'NONE', #55646 ) ;
#20584 = ORIENTED_EDGE ( 'NONE', *, *, #98161, .F. ) ;
#20585 = DIRECTION ( 'NONE',  ( -0.000000000000000000, 0.000000000000000000, 1.000000000000000000 ) ) ;
#20586 = CARTESIAN_POINT ( 'NONE',  ( 189.9388136067621531, 273.9745203768302986, -15.62273351239337416 ) ) ;
#20587 = ADVANCED_FACE ( 'NONE', ( #78492 ), #8581, .T. ) ;
#20588 = CARTESIAN_POINT ( 'NONE',  ( 186.6544709008256575, 298.6510803302452359, 3.914313306637340339 ) ) ;
#20589 = CARTESIAN_POINT ( 'NONE',  ( 192.7507137768506880, 296.7929658737652971, 11.30364540927242345 ) ) ;
#20590 = CARTESIAN_POINT ( 'NONE',  ( 70.81643854103050728, 70.50536786476077111, 6.457179250934519388 ) ) ;
#20591 = CARTESIAN_POINT ( 'NONE',  ( 191.0453904752189089, 285.8430533356794285, 17.34534042816491350 ) ) ;
#20592 = CARTESIAN_POINT ( 'NONE',  ( 7.753205860782987457, 175.2833772461660544, -9.188101187500095079 ) ) ;
#20593 = CARTESIAN_POINT ( 'NONE',  ( 96.79126913948807953, 232.8149278399160949, 9.188101187500093303 ) ) ;
#20594 = CARTESIAN_POINT ( 'NONE',  ( 36.33098132476075648, 203.3297689869269220, -2.679491924311201423 ) ) ;
#20595 = CARTESIAN_POINT ( 'NONE',  ( 185.4201904309665281, 295.0767498550951586, -7.685989019839836622 ) ) ;
#20596 = CARTESIAN_POINT ( 'NONE',  ( 79.10786694755505266, 56.92203217398106574, 16.19829027401005206 ) ) ;
#20597 = EDGE_CURVE ( 'NONE', #49571, #16524, #1981, .T. ) ;
#20598 = VECTOR ( 'NONE', #76783, 1000.000000000000000 ) ;
#20599 = CARTESIAN_POINT ( 'NONE',  ( -22.42236680055709641, 157.8615022471902591, 0.000000000000000000 ) ) ;
#20600 = VECTOR ( 'NONE', #67429, 1000.000000000000000 ) ;
#20601 = CARTESIAN_POINT ( 'NONE',  ( 164.7873404923249154, 250.7312283864773690, -12.00200811739543383 ) ) ;
#20602 = CARTESIAN_POINT ( 'NONE',  ( 180.5563687299889182, 273.0276302482951110, 17.30336775547517547 ) ) ;
#20603 = CARTESIAN_POINT ( 'NONE',  ( 194.8067605455144076, 293.2317884077015151, -16.00245909155922774 ) ) ;
#20604 = CARTESIAN_POINT ( 'NONE',  ( 84.40498577231251431, 50.09068632715275271, 13.84414505597724521 ) ) ;
#20605 = CARTESIAN_POINT ( 'NONE',  ( 195.9602617257426402, 266.6740640884384561, 8.002040582201244590 ) ) ;
#20606 = LINE ( 'NONE', #51993, #10859 ) ;
#20607 = CARTESIAN_POINT ( 'NONE',  ( 183.1426684129219780, 267.5694331394444703, -16.03671021927237206 ) ) ;
#20608 = VECTOR ( 'NONE', #76987, 1000.000000000000000 ) ;
#20609 =( BOUNDED_CURVE ( )  B_SPLINE_CURVE ( 2, ( #64600, #3802, #49391, #71211, #48900 ),
 .UNSPECIFIED., .F., .T. ) 
 B_SPLINE_CURVE_WITH_KNOTS ( ( 3, 2, 3 ),
 ( 0.9784858563273379772, 0.9784946236559139976, 0.9798387096774193727 ),
 .UNSPECIFIED. ) 
 CURVE ( )  GEOMETRIC_REPRESENTATION_ITEM ( )  RATIONAL_B_SPLINE_CURVE ( ( 0.9991289483004428540, 0.9995630490582195771, 1.000000000000000000, 0.9330127018922194093, 0.9330127018922194093 ) ) 
 REPRESENTATION_ITEM ( '' )  );
#20610 = DIRECTION ( 'NONE',  ( -0.5000000000000013323, 0.8660254037844379305, 0.000000000000000000 ) ) ;
#20611 = CARTESIAN_POINT ( 'NONE',  ( 77.90126356732251622, 215.7833772461660544, -9.188101187500095079 ) ) ;
#20612 = CARTESIAN_POINT ( 'NONE',  ( 7.127696690345725727, 16.06628583063839244, -9.188101187500006262 ) ) ;
#20613 = FACE_OUTER_BOUND ( 'NONE', #39175, .T. ) ;
#20614 = LINE ( 'NONE', #84433, #59508 ) ;
#20616 = CARTESIAN_POINT ( 'NONE',  ( 200.4189218502630467, 283.5112398876054272, 18.06577013929910791 ) ) ;
#20615 = CARTESIAN_POINT ( 'NONE',  ( 157.2464636617698375, 258.2881309577184652, 18.14284729738657731 ) ) ;
#20617 = CARTESIAN_POINT ( 'NONE',  ( 75.67456858315887303, 65.42170317558291970, 14.28506259273864210 ) ) ;
#20618 = CARTESIAN_POINT ( 'NONE',  ( 173.5450725454375061, 267.4326936521503058, -17.29647674659017298 ) ) ;
#20619 = CARTESIAN_POINT ( 'NONE',  ( 39.87427548755113094, 25.94754757982092741, 5.678558825948272215 ) ) ;
#20620 = CARTESIAN_POINT ( 'NONE',  ( 147.5540328368684300, 275.0759135952944234, -4.750028533202499403 ) ) ;
#20621 = DIRECTION ( 'NONE',  ( -0.8660254037844387076, -0.4999999999999998890, -0.000000000000000000 ) ) ;
#20622 = ORIENTED_EDGE ( 'NONE', *, *, #47907, .T. ) ;
#20623 = CARTESIAN_POINT ( 'NONE',  ( 20.18904385193075868, 29.84336893147756342, -7.433330006724137462 ) ) ;
#20624 = CARTESIAN_POINT ( 'NONE',  ( 177.1347673595945764, 262.9921672455169528, 15.53478677465993485 ) ) ;
#20625 = CARTESIAN_POINT ( 'NONE',  ( 193.0142717932987182, 296.3364699985351081, -13.30037542329744937 ) ) ;
#20626 = DIRECTION ( 'NONE',  ( 0.2194785493951409983, -0.9756173257765590190, 0.000000000000000000 ) ) ;
#20627 = VERTEX_POINT ( 'NONE', #31366 ) ;
#20628 = B_SPLINE_CURVE_WITH_KNOTS ( 'NONE', 3,
 ( #34487, #65388, #26900, #81142 ),
 .UNSPECIFIED., .F., .F.,
 ( 4, 4 ),
 ( 0.001193343334414101150, 0.009119723292965509209 ),
 .UNSPECIFIED. ) ;
#20629 = CARTESIAN_POINT ( 'NONE',  ( 70.65831043835135006, 60.85253071434844685, 14.52235072827622098 ) ) ;
#20630 = CARTESIAN_POINT ( 'NONE',  ( 76.03787485198571972, 65.47122818424047352, -14.36642907054480744 ) ) ;
#20631 = CARTESIAN_POINT ( 'NONE',  ( 156.9010835643442192, 268.4413441992039111, 15.68067955713730122 ) ) ;
#20632 = LINE ( 'NONE', #5427, #51713 ) ;
#20633 = CARTESIAN_POINT ( 'NONE',  ( 138.2253456014563255, 250.6115022471902591, 10.00000000000009592 ) ) ;
#20634 = CARTESIAN_POINT ( 'NONE',  ( 69.42144788871625849, 62.89730317705431872, 13.10748580973936939 ) ) ;
#20635 = VECTOR ( 'NONE', #2295, 1000.000000000000114 ) ;
#20636 = ORIENTED_EDGE ( 'NONE', *, *, #85891, .T. ) ;
#20637 = CARTESIAN_POINT ( 'NONE',  ( 190.3167824967908643, 299.0086585129598689, -8.112609889089975823 ) ) ;
#20638 = ORIENTED_EDGE ( 'NONE', *, *, #34687, .T. ) ;
#20639 = DIRECTION ( 'NONE',  ( -0.8660254037844378194, -0.5000000000000014433, 0.000000000000000000 ) ) ;
#20640 = CARTESIAN_POINT ( 'NONE',  ( 87.10115137904762150, 45.28340438443854055, 6.995308688534716879 ) ) ;
#20641 = ORIENTED_EDGE ( 'NONE', *, *, #32982, .T. ) ;
#20642 = DIRECTION ( 'NONE',  ( -1.000000000000000000, -4.892646582057456999E-14, 0.000000000000000000 ) ) ;
#20643 = ORIENTED_EDGE ( 'NONE', *, *, #45660, .F. ) ;
#20644 = CARTESIAN_POINT ( 'NONE',  ( 158.5882721812411376, 255.9640504279652760, 16.09668399467820166 ) ) ;
#20645 = CARTESIAN_POINT ( 'NONE',  ( 194.0724203524910365, 280.7181176903307005, -17.60110234268010032 ) ) ;
#20646 = CARTESIAN_POINT ( 'NONE',  ( 193.1336260368645981, 296.1297423845801404, -13.41923397934924367 ) ) ;
#20647 = CARTESIAN_POINT ( 'NONE',  ( 153.3859906278383676, 264.9746663937372091, -17.41799046551451013 ) ) ;
#20648 = EDGE_CURVE ( 'NONE', #5726, #29964, #24630, .T. ) ;
#20649 = CARTESIAN_POINT ( 'NONE',  ( 41.71939737199939202, 29.80170272979930246, 7.433330006724137462 ) ) ;
#20650 = CARTESIAN_POINT ( 'NONE',  ( 77.74639646092859380, 59.02570175780747519, -16.09564583426548978 ) ) ;
#20651 = ADVANCED_FACE ( 'NONE', ( #79007 ), #73755, .F. ) ;
#20652 = CARTESIAN_POINT ( 'NONE',  ( 166.7213618741906771, 275.6891020104532117, 14.83267127466106139 ) ) ;
#20653 = CARTESIAN_POINT ( 'NONE',  ( 87.25569243610996750, 45.44211441089371561, 7.127650669554064677 ) ) ;
#20654 = VERTEX_POINT ( 'NONE', #12462 ) ;
#20655 = ORIENTED_EDGE ( 'NONE', *, *, #76077, .T. ) ;
#20656 = CARTESIAN_POINT ( 'NONE',  ( 34.81516168915606357, 51.10768172523390973, -10.00000000000000000 ) ) ;
#20658 = CARTESIAN_POINT ( 'NONE',  ( 147.8819534105757043, 274.5079385007862811, -9.338341377131436971 ) ) ;
#20657 = CARTESIAN_POINT ( 'NONE',  ( 164.4864504671816690, 245.7481059646165704, 6.337356894698421783 ) ) ;
#20659 = CARTESIAN_POINT ( 'NONE',  ( 85.31220642273653709, 48.47216915277315508, 12.41700016606928259 ) ) ;
#20660 = CARTESIAN_POINT ( 'NONE',  ( 48.92549481379852949, 97.87922363803308201, -10.00000000000000000 ) ) ;
#20661 = CARTESIAN_POINT ( 'NONE',  ( 77.85362458321634449, 59.68407148126515693, -16.06148647132319240 ) ) ;
#20662 = CARTESIAN_POINT ( 'NONE',  ( 82.12141333937209708, 40.78733220434117612, 1.186632920674746794 ) ) ;
#20664 = EDGE_CURVE ( 'NONE', #35809, #73457, #28140, .T. ) ;
#20663 = CARTESIAN_POINT ( 'NONE',  ( 170.9173439896608500, 287.6710870028733211, -4.607079402279047997 ) ) ;
#20665 = CARTESIAN_POINT ( 'NONE',  ( 76.86303881961467255, 63.31387137873053916, -15.46595148530503927 ) ) ;
#20666 = CARTESIAN_POINT ( 'NONE',  ( 78.91446233654380649, 59.71533271261715470, 16.49719907270641883 ) ) ;
#20667 = VERTEX_POINT ( 'NONE', #58531 ) ;
#20668 = CARTESIAN_POINT ( 'NONE',  ( 148.0446189821823282, 274.7176051505724104, -6.028654458819870499 ) ) ;
#20669 = CARTESIAN_POINT ( 'NONE',  ( 166.4520249213679790, 277.9984640549334358, -13.37092130267346057 ) ) ;
#20670 = AXIS2_PLACEMENT_3D ( 'NONE', #26441, #51206, #89290 ) ;
#20671 = ORIENTED_EDGE ( 'NONE', *, *, #54849, .T. ) ;
#20672 = AXIS2_PLACEMENT_3D ( 'NONE', #66722, #74364, #13542 ) ;
#20673 = ORIENTED_EDGE ( 'NONE', *, *, #98080, .F. ) ;
#20674 = VERTEX_POINT ( 'NONE', #43333 ) ;
#20675 = CARTESIAN_POINT ( 'NONE',  ( 87.06644787366251137, 45.96331769923622801, -8.152425090918923090 ) ) ;
#20676 = EDGE_CURVE ( 'NONE', #12823, #89585, #37230, .T. ) ;
#20678 = B_SPLINE_SURFACE_WITH_KNOTS ( 'NONE', 3, 1, ( 
 ( #93840, #9717 ),
 ( #16785, #55759 ),
 ( #41067, #87767 ),
 ( #31977, #64392 ),
 ( #94824, #18305 ),
 ( #47674, #24393 ),
 ( #49204, #10204 ),
 ( #62881, #78607 ),
 ( #55267, #72005 ),
 ( #80137, #63390 ),
 ( #24883, #86247 ),
 ( #71512, #1099 ),
 ( #34014, #9193 ),
 ( #2609, #32499 ),
 ( #48704, #95356 ),
 ( #64899, #40068 ),
 ( #86751, #71011 ),
 ( #25388, #25911 ),
 ( #33497, #17285 ),
 ( #32984, #1613 ),
 ( #10701, #8692 ),
 ( #63888, #56783 ),
 ( #79637, #94330 ),
 ( #48189, #41579 ),
 ( #95845, #2103 ),
 ( #79136, #72520 ),
 ( #26401, #3129 ),
 ( #40572, #56276 ),
 ( #87274, #17804 ),
 ( #57277, #88254 ),
 ( #18801, #49684 ) ),
 .UNSPECIFIED., .F., .F., .F.,
 ( 4, 3, 3, 3, 3, 3, 3, 3, 3, 3, 4 ),
 ( 2, 2 ),
 ( 0.000000000000000000, 0.1333490885032357076, 0.3007194338854359827, 0.4699862290245028773, 0.5844252810809169585, 0.6686540514502661292, 0.7354980260655498148, 0.8028463152565713523, 0.8633854507757302565, 0.9437142632667330222, 1.000000000000000000 ),
 ( 0.000000000000000000, 1.000000000000000000 ),
 .UNSPECIFIED. ) ;
#20677 = CARTESIAN_POINT ( 'NONE',  ( 86.12135434523638366, 46.98046262810483142, -10.13131473785488090 ) ) ;
#20679 = CARTESIAN_POINT ( 'NONE',  ( 164.4909307685898341, 249.4621815394609143, 9.893007727036904342 ) ) ;
#20680 = CARTESIAN_POINT ( 'NONE',  ( 25.48331929688331599, 38.21091486745862653, 7.012934429366973338E-14 ) ) ;
#20681 = FACE_OUTER_BOUND ( 'NONE', #49213, .T. ) ;
#20682 = EDGE_CURVE ( 'NONE', #73019, #7170, #53503, .T. ) ;
#20683 = ORIENTED_EDGE ( 'NONE', *, *, #52910, .T. ) ;
#20684 = VERTEX_POINT ( 'NONE', #43832 ) ;
#20685 = LINE ( 'NONE', #74893, #46224 ) ;
#20686 = ORIENTED_EDGE ( 'NONE', *, *, #23089, .F. ) ;
#20687 = AXIS2_PLACEMENT_3D ( 'NONE', #16383, #24483, #31073 ) ;
#20688 = CARTESIAN_POINT ( 'NONE',  ( 191.6065101195901832, 264.2025560880797457, -7.910045257811711750 ) ) ;
#20689 = CARTESIAN_POINT ( 'NONE',  ( 49.80235952159635815, 85.00000000000000000, 10.00000000000000000 ) ) ;
#20690 = CARTESIAN_POINT ( 'NONE',  ( 67.18057841095335903, 68.85678461590420341, -3.812741676141380154 ) ) ;
#20692 = FACE_OUTER_BOUND ( 'NONE', #34231, .T. ) ;
#20691 = CARTESIAN_POINT ( 'NONE',  ( 135.7624123097878623, 255.3149278399160949, 9.188101187500093303 ) ) ;
#20693 = CARTESIAN_POINT ( 'NONE',  ( 77.08943580299947484, 49.61595851769167353, 15.51385818994994459 ) ) ;
#20694 = ORIENTED_EDGE ( 'NONE', *, *, #76938, .T. ) ;
#20695 = VECTOR ( 'NONE', #40812, 1000.000000000000000 ) ;
#20696 = CARTESIAN_POINT ( 'NONE',  ( 88.22000632671873177, 44.27423112938744509, 4.003506518527982116 ) ) ;
#20697 = CARTESIAN_POINT ( 'NONE',  ( 82.68211672025338999, 52.94826342379619177, 15.15574935255376232 ) ) ;
#20698 = EDGE_CURVE ( 'NONE', #33736, #56406, #13460, .T. ) ;
#20699 = CARTESIAN_POINT ( 'NONE',  ( 190.5742268578622145, 264.3298435039872061, -9.417883106533958326 ) ) ;
#20700 = CARTESIAN_POINT ( 'NONE',  ( 170.0560250869938841, 248.9713545018433649, -0.2644624926305505497 ) ) ;
#20701 = CARTESIAN_POINT ( 'NONE',  ( 172.6689194511114920, 286.8832926196414519, 10.78400060168022989 ) ) ;
#20702 = B_SPLINE_CURVE_WITH_KNOTS ( 'NONE', 3,
 ( #93187, #70867, #33358, #70351 ),
 .UNSPECIFIED., .F., .F.,
 ( 4, 4 ),
 ( 0.006445490163176449683, 0.01145963672390969655 ),
 .UNSPECIFIED. ) ;
#20703 = CARTESIAN_POINT ( 'NONE',  ( 71.96027346690365789, 72.28811235517684963, 3.313491923126954841 ) ) ;
#20704 = CARTESIAN_POINT ( 'NONE',  ( 199.0069894091751905, 281.8216829437676552, -16.59361213652569589 ) ) ;
#20705 = CARTESIAN_POINT ( 'NONE',  ( 122.6368883333363584, 251.6115022471903160, -5.000000000000047962 ) ) ;
#20706 = EDGE_CURVE ( 'NONE', #100197, #30881, #30548, .T. ) ;
#20707 = CARTESIAN_POINT ( 'NONE',  ( 80.92134340239459789, 55.42731787558462031, 16.01308592331401925 ) ) ;
#20708 = VECTOR ( 'NONE', #75319, 1000.000000000000000 ) ;
#20709 = CARTESIAN_POINT ( 'NONE',  ( 68.18512844359727865, 69.81902233912992983, -2.062004031463703591 ) ) ;
#20710 = CARTESIAN_POINT ( 'NONE',  ( 64.04520420253651025, 195.5327760586659736, 1.948934522072303157E-15 ) ) ;
#20711 = DIRECTION ( 'NONE',  ( 2.816764622163176506E-16, 1.626259812849726698E-16, -1.000000000000000000 ) ) ;
#20712 = CARTESIAN_POINT ( 'NONE',  ( 197.2094417012475560, 287.4525406113273220, 17.46401919701611760 ) ) ;
#20713 = LINE ( 'NONE', #12621, #46257 ) ;
#20714 = EDGE_CURVE ( 'NONE', #76357, #8790, #35390, .T. ) ;
#20715 = DIRECTION ( 'NONE',  ( 0.4999999999999998890, -0.8660254037844385966, 0.000000000000000000 ) ) ;
#20716 = ADVANCED_FACE ( 'NONE', ( #30128 ), #31608, .T. ) ;
#20717 = B_SPLINE_CURVE_WITH_KNOTS ( 'NONE', 3,
 ( #94119, #40359, #16574, #24672 ),
 .UNSPECIFIED., .F., .F.,
 ( 4, 4 ),
 ( 0.000000000000000000, 0.007499696492506968508 ),
 .UNSPECIFIED. ) ;
#20718 = ADVANCED_FACE ( 'NONE', ( #92466 ), #23013, .F. ) ;
#20719 = CARTESIAN_POINT ( 'NONE',  ( 160.0166746459236435, 283.6086068001695253, 2.232576205374148248 ) ) ;
#20720 = CARTESIAN_POINT ( 'NONE',  ( -20.77345734792011456, 95.19581990215550604, 45.19938701403189896 ) ) ;
#20721 = EDGE_CURVE ( 'NONE', #95964, #99288, #15407, .T. ) ;
#20722 = CARTESIAN_POINT ( 'NONE',  ( 12.43831579814173693, 15.38052372038639071, 10.00000000000000533 ) ) ;
#20723 = CARTESIAN_POINT ( 'NONE',  ( 36.72872667615778397, 36.90829794293883026, 10.00000000000000355 ) ) ;
#20724 = CARTESIAN_POINT ( 'NONE',  ( 81.22979812886450190, 55.45288652294036069, -16.34461090620092349 ) ) ;
#20725 = DIRECTION ( 'NONE',  ( -0.7893155279419930004, -0.6139877827364750296, 0.000000000000000000 ) ) ;
#20726 = CARTESIAN_POINT ( 'NONE',  ( 72.13517842779845068, 72.31474564102330760, 3.615969315562344910 ) ) ;
#20727 = CARTESIAN_POINT ( 'NONE',  ( 15.38522827951586081, 173.5643266524160140, -9.188101187500093303 ) ) ;
#20728 = CARTESIAN_POINT ( 'NONE',  ( 69.60933530497638344, 70.67006034057621378, 4.325380387426783102 ) ) ;
#20729 = VERTEX_POINT ( 'NONE', #93468 ) ;
#20730 = VECTOR ( 'NONE', #4037, 1000.000000000000000 ) ;
#20731 = CARTESIAN_POINT ( 'NONE',  ( 182.6063025987909327, 258.0860380675601391, -8.404863973281287315 ) ) ;
#20732 = CARTESIAN_POINT ( 'NONE',  ( 201.0466602553734106, 278.3904726219785744, 15.32208466927121293 ) ) ;
#20733 = CARTESIAN_POINT ( 'NONE',  ( -4.653128914090325807, 78.77562236714182120, 52.49999999999999289 ) ) ;
#20734 = CARTESIAN_POINT ( 'NONE',  ( 33.07613030564196777, 37.83478043621391151, -8.090169943749479842 ) ) ;
#20735 = CARTESIAN_POINT ( 'NONE',  ( 51.59574192737019160, 200.5958772461660544, -9.188101187500095079 ) ) ;
#20736 = AXIS2_PLACEMENT_3D ( 'NONE', #43849, #59031, #43350 ) ;
#20737 = CARTESIAN_POINT ( 'NONE',  ( 200.6129772034685175, 283.1751261563724142, 18.36811917402039640 ) ) ;
#20738 = CARTESIAN_POINT ( 'NONE',  ( 199.0363797504450929, 285.9058730480928716, -17.12190301149298222 ) ) ;
#20739 = CARTESIAN_POINT ( 'NONE',  ( 190.1696443193688708, 301.2635093119881162, -4.804312979389741223 ) ) ;
#20740 = CARTESIAN_POINT ( 'NONE',  ( 10.26584248093601737, 14.43085787977761036, -9.188101187500008038 ) ) ;
#20741 = CARTESIAN_POINT ( 'NONE',  ( 159.1856415905643303, 255.7098345965759734, -16.10742115897274829 ) ) ;
#20742 = CARTESIAN_POINT ( 'NONE',  ( 177.7369556440871463, 292.4164984073148617, 2.588529651253329789 ) ) ;
#20743 = VECTOR ( 'NONE', #69107, 1000.000000000000000 ) ;
#20744 = CARTESIAN_POINT ( 'NONE',  ( 179.5538644306811022, 276.7319085261062241, 16.30229987282069004 ) ) ;
#20745 = CARTESIAN_POINT ( 'NONE',  ( 73.21559929719344950, 63.73101106623266077, 13.92201872992145084 ) ) ;
#20746 = CARTESIAN_POINT ( 'NONE',  ( 68.11513882967693689, 67.84287964856595465, -7.395662205818876345 ) ) ;
#20747 = CARTESIAN_POINT ( 'NONE',  ( 107.8477481777883469, 244.6199935810940929, 2.679491924311251605 ) ) ;
#20748 = DIRECTION ( 'NONE',  ( 0.000000000000000000, 0.000000000000000000, -1.000000000000000000 ) ) ;
#20750 = CARTESIAN_POINT ( 'NONE',  ( 87.71554304996901408, 45.29005973903561966, -7.157883044737483047 ) ) ;
#20749 = VECTOR ( 'NONE', #67061, 1000.000000000000114 ) ;
#20751 = CARTESIAN_POINT ( 'NONE',  ( 101.8522786425098730, 229.6115022471902307, 10.00000000000009592 ) ) ;
#20752 = DIRECTION ( 'NONE',  ( -0.2803049773603352723, 0.9599109957006545235, 0.000000000000000000 ) ) ;
#20753 = CARTESIAN_POINT ( 'NONE',  ( 194.7393124278854657, 285.6008549388717483, -17.52668146566740148 ) ) ;
#20754 = VERTEX_POINT ( 'NONE', #93969 ) ;
#20755 = CARTESIAN_POINT ( 'NONE',  ( 57.30635725539759306, 194.7048013555409796, 4.594050593750051981 ) ) ;
#20756 = VERTEX_POINT ( 'NONE', #7835 ) ;
#20757 = CARTESIAN_POINT ( 'NONE',  ( 166.5660256732271591, 264.7075128827775075, 17.06110633390546027 ) ) ;
#20758 = DIRECTION ( 'NONE',  ( 0.9755587037855241173, -0.2197389712097240211, 0.000000000000000000 ) ) ;
#20759 = CARTESIAN_POINT ( 'NONE',  ( -22.42236680055709641, 157.8615022471902591, 0.000000000000000000 ) ) ;
#20760 = ORIENTED_EDGE ( 'NONE', *, *, #57869, .F. ) ;
#20761 = VECTOR ( 'NONE', #85224, 1000.000000000000000 ) ;
#20762 = LINE ( 'NONE', #84092, #86411 ) ;
#20763 = CARTESIAN_POINT ( 'NONE',  ( 207.6628070930962906, 270.9644626028195376, 7.378217122120054761 ) ) ;
#20764 = CARTESIAN_POINT ( 'NONE',  ( 159.9304399683796589, 266.3231526470470385, -17.61295603372380825 ) ) ;
#20765 = CARTESIAN_POINT ( 'NONE',  ( 36.08541434599421649, 23.76004757982091320, 5.678558825948272215 ) ) ;
#20766 = CARTESIAN_POINT ( 'NONE',  ( 186.4093957424555583, 263.0584473022519774, 11.49005727324106374 ) ) ;
#20767 = CARTESIAN_POINT ( 'NONE',  ( 86.48142457384331294, 47.12364270815633205, -10.06370626518989830 ) ) ;
#20768 = CARTESIAN_POINT ( 'NONE',  ( 204.5773065883323056, 276.3087062438502812, 13.12907315817041187 ) ) ;
#20769 = ORIENTED_EDGE ( 'NONE', *, *, #80453, .T. ) ;
#20770 = CARTESIAN_POINT ( 'NONE',  ( 20.98529944902502820, 27.51421378149918695, -9.188101187500004485 ) ) ;
#20771 = CARTESIAN_POINT ( 'NONE',  ( 28.12420092063944921, 24.43677371833803136, -10.00000000000000355 ) ) ;
#20772 = CARTESIAN_POINT ( 'NONE',  ( 71.10390369104861463, 70.26795136552352972, -6.302501079447722532 ) ) ;
#20773 = CARTESIAN_POINT ( 'NONE',  ( 15.54467260552930341, 34.00295985972733348, 10.00000000000000000 ) ) ;
#20774 = ORIENTED_EDGE ( 'NONE', *, *, #27456, .T. ) ;
#20775 = CARTESIAN_POINT ( 'NONE',  ( 180.0052941831603732, 282.8434537829564874, 15.07745545751880911 ) ) ;
#20776 = CARTESIAN_POINT ( 'NONE',  ( 166.9663977217517470, 261.3869414865291674, 16.80305011033491169 ) ) ;
#20777 = CARTESIAN_POINT ( 'NONE',  ( 206.2313482792274328, 273.4438219973828268, -9.403385562213845361 ) ) ;
#20778 = ORIENTED_EDGE ( 'NONE', *, *, #5651, .F. ) ;
#20779 = AXIS2_PLACEMENT_3D ( 'NONE', #13052, #66721, #52027 ) ;
#20781 = DIRECTION ( 'NONE',  ( 0.000000000000000000, -1.000000000000000000, 0.000000000000000000 ) ) ;
#20780 = CARTESIAN_POINT ( 'NONE',  ( 160.5702328569162489, 282.4873091647734213, -3.166141603222274448 ) ) ;
#20782 = CARTESIAN_POINT ( 'NONE',  ( 71.59328461577142377, 71.47600564087022690, -5.278543987517691605 ) ) ;
#20783 = ORIENTED_EDGE ( 'NONE', *, *, #27888, .F. ) ;
#20784 = CARTESIAN_POINT ( 'NONE',  ( 65.98617016278960534, 69.07574344600425320, -2.064703022102583940 ) ) ;
#20785 = CARTESIAN_POINT ( 'NONE',  ( 198.2414483977475754, 287.2827345394944700, 16.94931984969033678 ) ) ;
#20786 = CARTESIAN_POINT ( 'NONE',  ( 186.0348036264326481, 259.0250182415348945, 6.435743254585703177 ) ) ;
#20787 = CARTESIAN_POINT ( 'NONE',  ( 161.1469752488031588, 263.0258888816042031, -17.74540750750012919 ) ) ;
#20789 = EDGE_CURVE ( 'NONE', #42330, #92664, #25682, .T. ) ;
#20788 = CARTESIAN_POINT ( 'NONE',  ( 124.5044291563551440, 236.5643266524160424, -9.188101187500093303 ) ) ;
#20790 = ORIENTED_EDGE ( 'NONE', *, *, #78516, .T. ) ;
#20791 = CARTESIAN_POINT ( 'NONE',  ( 170.1571642572108658, 264.1681567744807353, 16.32371355451207151 ) ) ;
#20792 = CARTESIAN_POINT ( 'NONE',  ( 73.18322933451462120, 206.3927522451418497, -10.00000000000009237 ) ) ;
#20793 = VECTOR ( 'NONE', #95392, 1000.000000000000114 ) ;
#20794 = ORIENTED_EDGE ( 'NONE', *, *, #54147, .T. ) ;
#20795 = CARTESIAN_POINT ( 'NONE',  ( 148.8217493443905255, 275.2952789360765564, 7.685775767636982003 ) ) ;
#20796 = ORIENTED_EDGE ( 'NONE', *, *, #85697, .F. ) ;
#20797 = ORIENTED_EDGE ( 'NONE', *, *, #60241, .F. ) ;
#20798 = CARTESIAN_POINT ( 'NONE',  ( 198.4334039703542771, 286.9502577349437615, 18.47706603442866680 ) ) ;
#20799 = CARTESIAN_POINT ( 'NONE',  ( 0.4022032943177059061, 45.37891224861880346, 59.99999999999999289 ) ) ;
#20800 = CARTESIAN_POINT ( 'NONE',  ( 82.55649720842890815, 206.2202760586659167, -5.415160957724236172E-17 ) ) ;
#20801 = ADVANCED_FACE ( 'NONE', ( #15920 ), #22927, .F. ) ;
#20802 = CARTESIAN_POINT ( 'NONE',  ( 81.55638901470594249, 55.99673023569365427, 16.04557931222332101 ) ) ;
#20803 = CARTESIAN_POINT ( 'NONE',  ( 42.87900647455834502, 24.75620593066997444, 8.404119662683931360E-14 ) ) ;
#20804 = CARTESIAN_POINT ( 'NONE',  ( 175.3946993052283005, 278.3949788008520159, 15.46601621310474250 ) ) ;
#20805 = EDGE_CURVE ( 'NONE', #65643, #94602, #14947, .T. ) ;
#20806 = DIRECTION ( 'NONE',  ( 0.000000000000000000, 0.000000000000000000, -1.000000000000000000 ) ) ;
#20807 = EDGE_LOOP ( 'NONE', ( #1795, #60860, #38261, #70605 ) ) ;
#20808 = LINE ( 'NONE', #354, #75513 ) ;
#20809 = CARTESIAN_POINT ( 'NONE',  ( 87.07071992409855454, 43.63667771387513028, -1.980884226090577238 ) ) ;
#20810 = CARTESIAN_POINT ( 'NONE',  ( 153.2513309553138470, 265.2079037882803618, -16.24091495603130397 ) ) ;
#20811 = CARTESIAN_POINT ( 'NONE',  ( 66.46251910857498046, 68.82904070585031775, -4.353565755910135948 ) ) ;
#20812 = AXIS2_PLACEMENT_3D ( 'NONE', #76993, #98833, #45103 ) ;
#20813 = ORIENTED_EDGE ( 'NONE', *, *, #22839, .T. ) ;
#20814 = CARTESIAN_POINT ( 'NONE',  ( 77.86555730066852732, 62.20866292688850052, -15.95979438352862445 ) ) ;
#20815 = CARTESIAN_POINT ( 'NONE',  ( 76.08286921349539966, 51.17209099756131252, -15.60946675595210387 ) ) ;
#20816 = CARTESIAN_POINT ( 'NONE',  ( 174.3136715079830026, 253.2187907930447750, -7.762168257024684159 ) ) ;
#20817 = VECTOR ( 'NONE', #75051, 999.9999999999998863 ) ;
#20818 = CARTESIAN_POINT ( 'NONE',  ( 78.75297625639956323, 47.66336229257159118, 14.29739783539339371 ) ) ;
#20819 = CARTESIAN_POINT ( 'NONE',  ( 164.6241018286200699, 245.5096868128744632, 3.031483545445131433 ) ) ;
#20820 = LINE ( 'NONE', #45090, #37961 ) ;
#20821 = ORIENTED_EDGE ( 'NONE', *, *, #25371, .T. ) ;
#20822 = CARTESIAN_POINT ( 'NONE',  ( 46.80963145949299076, 71.09457308843315104, 177.5919119679930134 ) ) ;
#20823 = AXIS2_PLACEMENT_3D ( 'NONE', #93938, #32081, #71114 ) ;
#20824 = CARTESIAN_POINT ( 'NONE',  ( 136.7095408212358052, 258.9244531367911577, -4.594050593750046652 ) ) ;
#20825 = ORIENTED_EDGE ( 'NONE', *, *, #28811, .F. ) ;
#20826 = CARTESIAN_POINT ( 'NONE',  ( -7.266922234329455499, 176.6115022471903160, -5.000000000000047962 ) ) ;
#20827 = CARTESIAN_POINT ( 'NONE',  ( 66.60661563016273590, 67.77273566365288104, -7.043189648870076702 ) ) ;
#20828 = CARTESIAN_POINT ( 'NONE',  ( 168.8563211758018099, 286.0187424789903048, -9.056861680415359217 ) ) ;
#20829 = CARTESIAN_POINT ( 'NONE',  ( 79.16557600000783168, 59.08901585114728050, -16.21880825576194951 ) ) ;
#20830 = DIRECTION ( 'NONE',  ( 1.000000000000000000, 0.000000000000000000, 0.000000000000000000 ) ) ;
#20831 = CYLINDRICAL_SURFACE ( 'NONE', #79359, 70.00000000000002842 ) ;
#20832 = ORIENTED_EDGE ( 'NONE', *, *, #68260, .T. ) ;
#20833 = DIRECTION ( 'NONE',  ( 8.673617379884076887E-16, 0.000000000000000000, -1.000000000000000000 ) ) ;
#20834 = CIRCLE ( 'NONE', #54785, 70.00000000000001421 ) ;
#20835 = CARTESIAN_POINT ( 'NONE',  ( 182.1058308719148613, 275.7167741723378072, -16.43330782191204520 ) ) ;
#20836 = ADVANCED_FACE ( 'NONE', ( #20944 ), #42702, .T. ) ;
#20837 = CARTESIAN_POINT ( 'NONE',  ( 167.5923213779273340, 249.2094892142539493, -5.528754456902119863 ) ) ;
#20838 = CARTESIAN_POINT ( 'NONE',  ( 80.87089094628977648, 50.87823725607803027, 14.71529395728275347 ) ) ;
#20839 = CARTESIAN_POINT ( 'NONE',  ( 200.4669192785465839, 267.1762403986572281, 0.8314407050123316933 ) ) ;
#20840 = CARTESIAN_POINT ( 'NONE',  ( 199.1041333440138317, 265.1832257255362038, 0.2027868546939186056 ) ) ;
#20841 = CARTESIAN_POINT ( 'NONE',  ( 190.1635032421960148, 301.2741459696644029, -5.047660290019184259 ) ) ;
#20842 = EDGE_CURVE ( 'NONE', #66829, #67877, #51827, .T. ) ;
#20843 = CARTESIAN_POINT ( 'NONE',  ( 184.5366411851703390, 281.4491850268337885, 16.25207963496568908 ) ) ;
#20844 = CARTESIAN_POINT ( 'NONE',  ( 193.2770523687239859, 268.3139821420764406, 12.74059143256334359 ) ) ;
#20845 = EDGE_CURVE ( 'NONE', #65280, #13449, #70334, .T. ) ;
#20846 = CARTESIAN_POINT ( 'NONE',  ( 18.00728827979274627, 29.13478043621388380, 8.090169943749478065 ) ) ;
#20847 = B_SPLINE_CURVE_WITH_KNOTS ( 'NONE', 3,
 ( #40413, #42777, #71347, #1938, #32824, #63732, #45767, #90946, #61477, #6295, #6791, #45281, #37186, #77182, #68087, #37672 ),
 .UNSPECIFIED., .F., .F.,
 ( 4, 2, 2, 2, 2, 2, 2, 4 ),
 ( 0.000000000000000000, 0.0005218775415615029088, 0.0007828163123422070919, 0.001043755083122911275, 0.001304693853903615567, 0.001565632624684319641, 0.001826571395465023933, 0.002087510166245728008 ),
 .UNSPECIFIED. ) ;
#20848 = CARTESIAN_POINT ( 'NONE',  ( 149.1856130393175306, 272.2499337880290682, 11.44243872309708188 ) ) ;
#20849 = CARTESIAN_POINT ( 'NONE',  ( 59.82969263072505584, 216.8967562850347122, -4.648177544792955347E-16 ) ) ;
#20850 = CARTESIAN_POINT ( 'NONE',  ( 68.21406460964578855, 69.18034937236612336, -6.080108713557645039 ) ) ;
#20851 = CARTESIAN_POINT ( 'NONE',  ( 198.4772197948566372, 286.8743665007300478, 18.43646439804394532 ) ) ;
#20852 = CARTESIAN_POINT ( 'NONE',  ( 72.23520231138428471, 71.91245603983271906, -3.821936190094874508 ) ) ;
#20853 = CARTESIAN_POINT ( 'NONE',  ( 138.0629658346988151, 250.5177522451418213, -10.00000000000009592 ) ) ;
#20854 = CARTESIAN_POINT ( 'NONE',  ( 172.4124261811984127, 284.1103845159578896, -12.83577416862662979 ) ) ;
#20855 = ORIENTED_EDGE ( 'NONE', *, *, #74554, .F. ) ;
#20856 = CARTESIAN_POINT ( 'NONE',  ( 66.77848686889967667, 67.34565621990024908, -6.901698923710801736 ) ) ;
#20857 = CARTESIAN_POINT ( 'NONE',  ( 199.1944722252943905, 285.6320488493591938, -18.17555833707144686 ) ) ;
#20858 = CARTESIAN_POINT ( 'NONE',  ( 18.76822678699008051, 172.4548013555409796, -4.594050593750042211 ) ) ;
#20859 = B_SPLINE_CURVE_WITH_KNOTS ( 'NONE', 3,
 ( #47635, #94785, #48147, #41028 ),
 .UNSPECIFIED., .F., .F.,
 ( 4, 4 ),
 ( 0.000000000000000000, 0.02192660554268253612 ),
 .UNSPECIFIED. ) ;
#20860 = CARTESIAN_POINT ( 'NONE',  ( 179.6016093521815264, 274.3055133302825084, -17.77051425966819664 ) ) ;
#20861 = CARTESIAN_POINT ( 'NONE',  ( 22.27692774695706035, 28.56454794089041727, 10.00000000000000355 ) ) ;
#20862 = CARTESIAN_POINT ( 'NONE',  ( 85.73895798293081327, 48.63177274617319057, 12.34992197344710796 ) ) ;
#20863 = CARTESIAN_POINT ( 'NONE',  ( 157.0978663001774862, 258.5455091378672137, -17.31223197570816552 ) ) ;
#20864 = CARTESIAN_POINT ( 'NONE',  ( 71.97191893240673721, 71.74017062233478725, -3.901372815243289160 ) ) ;
#20865 = CARTESIAN_POINT ( 'NONE',  ( 149.7854447168632817, 277.1467554076948545, 4.663160563959508842 ) ) ;
#20866 = B_SPLINE_CURVE_WITH_KNOTS ( 'NONE', 3,
 ( #53557, #1378, #46964, #7978, #84508, #15052, #30265, #77375, #100189, #76390, #6964, #54042, #45943, #47456, #8468, #62142, #68757, #86034, #78383, #37850, #862, #92603, #94107, #69260, #24658, #8964, #7458, #39833, #31742, #368, #31255, #30773, #62644, #61655, #84998, #99682, #46443, #16063, #93600, #93089, #38853, #55542, #61154, #86526, #23646, #85518, #22677, #45456, #92125, #72293 ),
 .UNSPECIFIED., .F., .F.,
 ( 4, 2, 2, 2, 2, 2, 2, 2, 2, 2, 2, 2, 2, 2, 2, 2, 2, 2, 2, 2, 2, 2, 2, 2, 4 ),
 ( 0.0002086497370388745807, 0.0006900493116877915497, 0.001171448886336708302, 0.001412148673661194108, 0.001532498567323459671, 0.001652848460985725234, 0.001773198354647990797, 0.001893548248310256360, 0.002134248035634715712, 0.002615647610283591482, 0.003097047184932467251, 0.004059846334230156339, 0.005022645483527845428, 0.005504045058176613645, 0.005744744845501038519, 0.005865094739163214527, 0.005985444632825390535, 0.006045619579656511498, 0.006105794526487632462, 0.006226144420149894339, 0.006466844207474383398, 0.006948243782123404017, 0.007188943569447914760, 0.007429643356772425503, 0.007911042931421497296 ),
 .UNSPECIFIED. ) ;
#20867 = CARTESIAN_POINT ( 'NONE',  ( 182.2373335159190901, 280.9600371166583841, -17.30031729693378040 ) ) ;
#20868 = CARTESIAN_POINT ( 'NONE',  ( 178.6317619811870259, 253.9327355832967612, -4.167451725846189170 ) ) ;
#20869 = CARTESIAN_POINT ( 'NONE',  ( 150.9950855294679570, 269.1158355001903715, 14.12809338255366320 ) ) ;
#20870 = CARTESIAN_POINT ( 'NONE',  ( 179.3203272704038795, 294.0804011742710031, 1.043687953058034301 ) ) ;
#20871 = CARTESIAN_POINT ( 'NONE',  ( 61.65426615018220957, 199.7365022471902023, -10.00000000000009059 ) ) ;
#20872 = CARTESIAN_POINT ( 'NONE',  ( 185.0103834951779334, 294.0474252827615373, 9.686088409191285109 ) ) ;
#20873 = DIRECTION ( 'NONE',  ( 0.1783728972749306640, 0.9839629614562466209, 0.000000000000000000 ) ) ;
#20874 = AXIS2_PLACEMENT_3D ( 'NONE', #39217, #45338, #15935 ) ;
#20875 = CARTESIAN_POINT ( 'NONE',  ( 19.90436448580963713, 191.4869531367911293, 4.594050593750046652 ) ) ;
#20876 = CARTESIAN_POINT ( 'NONE',  ( 168.0283599306779649, 286.1692283979162426, 4.090021465173546034 ) ) ;
#20877 = EDGE_CURVE ( 'NONE', #81790, #81845, #36602, .T. ) ;
#20878 = CARTESIAN_POINT ( 'NONE',  ( 8.321535033790485869, 175.6115022471902307, 10.00000000000009592 ) ) ;
#20879 = CARTESIAN_POINT ( 'NONE',  ( 42.56377214068922399, 30.28920272979930672, -7.433330006724141015 ) ) ;
#20880 = CARTESIAN_POINT ( 'NONE',  ( 145.0115229932138163, 242.9824982072973683, 3.021315404115420679E-15 ) ) ;
#20882 = CARTESIAN_POINT ( 'NONE',  ( 179.7935361763625224, 276.9290168454140257, 16.29839862902545988 ) ) ;
#20881 = VECTOR ( 'NONE', #30683, 1000.000000000000000 ) ;
#20883 = CARTESIAN_POINT ( 'NONE',  ( 185.5167212227024436, 266.6325209536038869, 13.19601323185720254 ) ) ;
#20884 = CARTESIAN_POINT ( 'NONE',  ( 125.5723057710370085, 231.7592609112379876, 2.679491924311254714 ) ) ;
#20885 = CARTESIAN_POINT ( 'NONE',  ( 164.0674942879805371, 281.5465086372613541, 8.868535044241015797 ) ) ;
#20886 = CARTESIAN_POINT ( 'NONE',  ( 0.000000000000000000, 0.000000000000000000, 0.000000000000000000 ) ) ;
#20887 = CARTESIAN_POINT ( 'NONE',  ( 9.333682440526761326, 28.49540643055185640, 3.479690158560446702E-15 ) ) ;
#20888 = CARTESIAN_POINT ( 'NONE',  ( 71.97456596565470477, 72.60744930783873485, 1.463844530419971868 ) ) ;
#20889 = FACE_OUTER_BOUND ( 'NONE', #39470, .T. ) ;
#20890 = CARTESIAN_POINT ( 'NONE',  ( 187.4676533354318906, 272.4601757945604845, -16.88503403312462936 ) ) ;
#20891 = CARTESIAN_POINT ( 'NONE',  ( -27.42236680055714260, 166.5217562850347406, 1.224646799147364892E-15 ) ) ;
#20892 = ORIENTED_EDGE ( 'NONE', *, *, #90616, .T. ) ;
#20893 = VECTOR ( 'NONE', #79537, 1000.000000000000000 ) ;
#20894 = CARTESIAN_POINT ( 'NONE',  ( 47.92671612011951510, 80.40884667711614497, -10.00000000000000000 ) ) ;
#20895 = CARTESIAN_POINT ( 'NONE',  ( 156.5940896385898213, 276.3990306459002682, 10.26584805396775479 ) ) ;
#20896 = CARTESIAN_POINT ( 'NONE',  ( 74.91545508103216378, 53.41488691832748259, -16.53475931695716028 ) ) ;
#20897 = DIRECTION ( 'NONE',  ( -0.7510153523339186954, 0.6602847420308604054, 0.000000000000000000 ) ) ;
#20898 = ORIENTED_EDGE ( 'NONE', *, *, #21888, .F. ) ;
#20899 = CARTESIAN_POINT ( 'NONE',  ( 156.4935365524153497, 263.7981763440885175, 17.67496387420143833 ) ) ;
#20900 = CARTESIAN_POINT ( 'NONE',  ( 67.88857314316685176, 69.78661589965172141, 0.4887884946192302404 ) ) ;
#20902 = CARTESIAN_POINT ( 'NONE',  ( 204.6785851723931557, 274.1332865905380913, -12.34137688749581407 ) ) ;
#20901 = B_SPLINE_CURVE_WITH_KNOTS ( 'NONE', 3,
 ( #31461, #38053, #76582, #52761, #92322, #14281, #29483, #7166, #21875, #68966, #38562, #67981, #83723, #99889, #39050, #53274 ),
 .UNSPECIFIED., .F., .F.,
 ( 4, 1, 2, 2, 2, 1, 2, 2, 4 ),
 ( 0.000000000000000000, 0.1249999999999952538, 0.1874999999999950873, 0.2499999999999949485, 0.4999999999999948930, 0.6249999999999962252, 0.6874999999999970024, 0.7499999999999976685, 1.000000000000000000 ),
 .UNSPECIFIED. ) ;
#20903 = CARTESIAN_POINT ( 'NONE',  ( 202.7602807045765019, 279.4558873931827065, -15.90558713185497020 ) ) ;
#20904 = ORIENTED_EDGE ( 'NONE', *, *, #98009, .F. ) ;
#20905 = AXIS2_PLACEMENT_3D ( 'NONE', #65476, #43148, #95447 ) ;
#20906 =( BOUNDED_CURVE ( )  B_SPLINE_CURVE ( 2, ( #71105, #9808, #41165, #94921, #70575, #32069, #62980, #33593, #79730 ),
 .UNSPECIFIED., .F., .T. ) 
 B_SPLINE_CURVE_WITH_KNOTS ( ( 3, 2, 2, 2, 3 ),
 ( 0.4475806451612903136, 0.4489247311827956888, 0.4516129032258064391, 0.4543010752688171894, 0.4556451612903225645 ),
 .UNSPECIFIED. ) 
 CURVE ( )  GEOMETRIC_REPRESENTATION_ITEM ( )  RATIONAL_B_SPLINE_CURVE ( ( 0.9330127018922194093, 0.9330127018922194093, 1.000000000000000000, 0.8660254037844387076, 1.000000000000000000, 0.8660254037844387076, 1.000000000000000000, 0.9330127018922194093, 0.9330127018922194093 ) ) 
 REPRESENTATION_ITEM ( '' )  );
#20907 = VERTEX_POINT ( 'NONE', #98934 ) ;
#20909 = CARTESIAN_POINT ( 'NONE',  ( 164.2712161151136172, 246.1209027979328710, 7.276091357954241445 ) ) ;
#20908 = CARTESIAN_POINT ( 'NONE',  ( 164.9274015170355767, 246.4109339568823600, -4.339738877753560153 ) ) ;
#20910 = CARTESIAN_POINT ( 'NONE',  ( 192.3606619183491091, 297.4685555102766443, 10.99569063633359889 ) ) ;
#20911 = ORIENTED_EDGE ( 'NONE', *, *, #34437, .F. ) ;
#20912 = CARTESIAN_POINT ( 'NONE',  ( 191.2645787786270262, 299.3670271975948367, 7.309947121636420242 ) ) ;
#20913 = CARTESIAN_POINT ( 'NONE',  ( 80.48345259418954356, 57.73457509892514139, -16.59664598758602949 ) ) ;
#20914 = CARTESIAN_POINT ( 'NONE',  ( 68.74157960831310277, 69.68624548565989585, -5.631338930608605686 ) ) ;
#20915 = VERTEX_POINT ( 'NONE', #88900 ) ;
#20916 = CARTESIAN_POINT ( 'NONE',  ( 87.30643095423958755, 44.98864145313458351, -6.191042897133923084 ) ) ;
#20917 = EDGE_CURVE ( 'NONE', #65735, #81256, #50319, .T. ) ;
#20918 = B_SPLINE_CURVE_WITH_KNOTS ( 'NONE', 3,
 ( #89641, #28788, #36881, #98205, #20203, #28278, #29783, #21689, #44469, #90125, #82035, #20700, #52568, #14088, #99694, #44973, #43968, #74906, #45468, #75911, #6491, #5985, #12611, #66785, #76403, #5491, #51589, #37370, #68275, #60655, #43475, #83026, #13108, #59668, #97711, #36374, #67786, #84031, #14590, #90642, #21202, #98712, #37861, #52081, #68770, #13595, #39354, #100201, #1889, #381 ),
 .UNSPECIFIED., .F., .F.,
 ( 4, 2, 2, 2, 2, 2, 2, 2, 2, 2, 2, 2, 2, 2, 2, 2, 2, 2, 2, 2, 2, 2, 2, 2, 4 ),
 ( 0.0007717967845395873154, 0.0009775820906090470185, 0.001080474743643774268, 0.001183367396678501734, 0.001286260049713228984, 0.001389152702747956450, 0.001594938008817510479, 0.002006508620956503827, 0.002418079233095497826, 0.003241220457373425977, 0.004064361681651354127, 0.004887502905929283145, 0.005299073518068247654, 0.005504858824137695214, 0.005607751477172462362, 0.005659197803689845069, 0.005710644130207229510, 0.005813536783242036557, 0.005916429436276843604, 0.006122214742346457697, 0.006533785354485663333, 0.006739570660555331202, 0.006945355966624997338, 0.007151141272694665207, 0.007356926578764333077 ),
 .UNSPECIFIED. ) ;
#20919 = CARTESIAN_POINT ( 'NONE',  ( 196.7823306783968746, 289.8100005636337073, -17.85370042640856170 ) ) ;
#20920 = CARTESIAN_POINT ( 'NONE',  ( 80.88056646709152631, 43.02648916431432724, 9.632536512155043695 ) ) ;
#20921 = EDGE_LOOP ( 'NONE', ( #82746, #71136, #14264, #75238 ) ) ;
#20922 = CARTESIAN_POINT ( 'NONE',  ( 206.5117639185820906, 272.9581278627833285, 11.28485531511759099 ) ) ;
#20923 = CARTESIAN_POINT ( 'NONE',  ( 74.29078308660947982, 62.27531838756304694, 14.84303450056853180 ) ) ;
#20924 = B_SPLINE_SURFACE_WITH_KNOTS ( 'NONE', 3, 1, ( 
 ( #12915, #13883 ),
 ( #82347, #73702 ),
 ( #35184, #67078 ),
 ( #51379, #97514 ),
 ( #5295, #59966 ),
 ( #57991, #4285 ),
 ( #3806, #65588 ),
 ( #44765, #51894 ),
 ( #34686, #13404 ),
 ( #35691, #81339 ),
 ( #96536, #82835 ),
 ( #66093, #28581 ),
 ( #58956, #27106 ),
 ( #88972, #11913 ),
 ( #19527, #59460 ),
 ( #36175, #29100 ),
 ( #36670, #42769 ),
 ( #97041, #89928 ),
 ( #21013, #27609 ),
 ( #20506, #12407 ),
 ( #89448, #44275 ),
 ( #74719, #75205 ),
 ( #50883, #43774 ),
 ( #5782, #20004 ),
 ( #81831, #43273 ),
 ( #67578, #98510 ),
 ( #74220, #90938 ),
 ( #4809, #21488 ),
 ( #52379, #66591 ),
 ( #68077, #37662 ),
 ( #22480, #61954 ),
 ( #84815, #14870 ),
 ( #68573, #92906 ),
 ( #181, #46775 ) ),
 .UNSPECIFIED., .T., .F., .F.,
 ( 4, 2, 2, 2, 2, 2, 2, 2, 2, 2, 2, 2, 2, 2, 2, 2, 4 ),
 ( 2, 2 ),
 ( 0.000000000000000000, 0.06250000000000000000, 0.1250000000000000000, 0.1875000000000000000, 0.2500000000000000000, 0.3125000000000000000, 0.3750000000000000000, 0.4375000000000000000, 0.5000000000000000000, 0.5625000000000000000, 0.6250000000000000000, 0.6875000000000000000, 0.7500000000000000000, 0.8125000000000000000, 0.8750000000000000000, 0.9375000000000000000, 1.000000000000000000 ),
 ( 0.000000000000000000, 1.000000000000000000 ),
 .UNSPECIFIED. ) ;
#20925 = ORIENTED_EDGE ( 'NONE', *, *, #45457, .T. ) ;
#20926 = CARTESIAN_POINT ( 'NONE',  ( 177.8254925427601449, 279.4843545943256231, -16.44570388904381986 ) ) ;
#20927 = CARTESIAN_POINT ( 'NONE',  ( 172.3690860356537655, 263.8130983119961570, -15.50581088013947273 ) ) ;
#20928 = ORIENTED_EDGE ( 'NONE', *, *, #70020, .T. ) ;
#20929 = EDGE_CURVE ( 'NONE', #15783, #54743, #89385, .T. ) ;
#20930 = CARTESIAN_POINT ( 'NONE',  ( 94.39539123479723060, 213.7592609112380160, 2.679491924311254714 ) ) ;
#20931 = CARTESIAN_POINT ( 'NONE',  ( 147.0456760057551833, 275.9564134551570760, -3.678503029046952033 ) ) ;
#20932 = ORIENTED_EDGE ( 'NONE', *, *, #49251, .T. ) ;
#20933 = EDGE_CURVE ( 'NONE', #72951, #45184, #37591, .T. ) ;
#20934 = ORIENTED_EDGE ( 'NONE', *, *, #56716, .F. ) ;
#20935 = CARTESIAN_POINT ( 'NONE',  ( 73.36558254226180509, 69.84094749084881926, 9.147675672628972521 ) ) ;
#20936 = CARTESIAN_POINT ( 'NONE',  ( 169.0812390597727131, 272.3489582993335603, 16.78971480844334963 ) ) ;
#20937 = CARTESIAN_POINT ( 'NONE',  ( 190.9498149295421570, 299.9122141765958531, -5.138500224925297566 ) ) ;
#20938 = CARTESIAN_POINT ( 'NONE',  ( 188.5431557236284448, 298.7030506545673347, -4.948255474722738079 ) ) ;
#20939 = CARTESIAN_POINT ( 'NONE',  ( 143.8748646542946972, 242.3262482093457777, 3.021315404115420679E-15 ) ) ;
#20940 = CARTESIAN_POINT ( 'NONE',  ( 192.8010417052266234, 296.7057953447782097, 12.10593424093686643 ) ) ;
#20941 = CARTESIAN_POINT ( 'NONE',  ( 191.8416637716208299, 298.3674866694441334, 8.941921481404037308 ) ) ;
#20942 = CARTESIAN_POINT ( 'NONE',  ( 146.5310397537613483, 276.8477895910274356, -0.2793038414862049068 ) ) ;
#20943 = EDGE_LOOP ( 'NONE', ( #96596, #67118, #9129, #28022 ) ) ;
#20944 = FACE_OUTER_BOUND ( 'NONE', #52756, .T. ) ;
#20946 = CARTESIAN_POINT ( 'NONE',  ( 205.8610808625997208, 274.0851439753691920, 10.38803237360972531 ) ) ;
#20945 = CARTESIAN_POINT ( 'NONE',  ( 197.0184425104562820, 289.4010428742387262, -16.90752553128928426 ) ) ;
#20947 = CARTESIAN_POINT ( 'NONE',  ( 67.24983238577166844, 66.59130585728682661, 8.524349129767776034 ) ) ;
#20948 = DIRECTION ( 'NONE',  ( 0.2774202615135334948, -0.9607486656258038549, 0.000000000000000000 ) ) ;
#20949 = CARTESIAN_POINT ( 'NONE',  ( 60.86586985908987657, 190.3595308348468791, 0.000000000000000000 ) ) ;
#20950 = CARTESIAN_POINT ( 'NONE',  ( 101.4461556848294492, 235.5024278399160949, -9.188101187500093303 ) ) ;
#20951 = VERTEX_POINT ( 'NONE', #47197 ) ;
#20952 = CARTESIAN_POINT ( 'NONE',  ( 190.2557389001687511, 301.1143891237862817, -3.302524770651862784 ) ) ;
#20953 = CARTESIAN_POINT ( 'NONE',  ( 77.95341167405027250, 53.58435032990927738, -15.90803922215739163 ) ) ;
#20954 = DIRECTION ( 'NONE',  ( -0.8660254037844387076, -0.4999999999999998890, -0.000000000000000000 ) ) ;
#20955 = CARTESIAN_POINT ( 'NONE',  ( 79.64486573815776183, 45.90865440701455213, 12.93595385939046594 ) ) ;
#20956 = CARTESIAN_POINT ( 'NONE',  ( 160.4869048512927918, 252.6755221785256822, -16.09843817406293809 ) ) ;
#20957 = CARTESIAN_POINT ( 'NONE',  ( 147.9236371514436996, 274.4357401437532076, -9.513995150070424955 ) ) ;
#20958 = ORIENTED_EDGE ( 'NONE', *, *, #73971, .T. ) ;
#20959 = CARTESIAN_POINT ( 'NONE',  ( 170.5132574684816120, 255.5220156066502852, -11.62455434932883769 ) ) ;
#20960 = CARTESIAN_POINT ( 'NONE',  ( 82.35975313173908319, 41.41624149291902057, 5.521678208619409389 ) ) ;
#20961 = EDGE_CURVE ( 'NONE', #62875, #44322, #99922, .T. ) ;
#20962 = CARTESIAN_POINT ( 'NONE',  ( 206.9026071836525205, 272.2811674698855313, 7.240992997279449561 ) ) ;
#20963 = CARTESIAN_POINT ( 'NONE',  ( 34.21208616421487392, 183.8927522451417929, -10.00000000000009059 ) ) ;
#20964 = CARTESIAN_POINT ( 'NONE',  ( 121.2028808523094767, 228.5327760586659451, 1.948934522072302763E-15 ) ) ;
#20965 = DIRECTION ( 'NONE',  ( -0.000000000000000000, -0.000000000000000000, -1.000000000000000000 ) ) ;
#20966 = AXIS2_PLACEMENT_3D ( 'NONE', #60573, #61578, #92528 ) ;
#20967 = CARTESIAN_POINT ( 'NONE',  ( 163.3740049908953438, 249.6749180501957710, -11.76522313559978627 ) ) ;
#20968 = CARTESIAN_POINT ( 'NONE',  ( 105.0197468877793625, 219.8932355074535678, -2.679491924311248496 ) ) ;
#20969 = CARTESIAN_POINT ( 'NONE',  ( 174.9435373006569421, 253.2161234547149604, -3.877573368771597195 ) ) ;
#20970 = CARTESIAN_POINT ( 'NONE',  ( 44.74898890052324418, 187.4548013555409796, -4.594050593750042211 ) ) ;
#20971 = CARTESIAN_POINT ( 'NONE',  ( -18.15312891409030627, 78.77562236714182120, 13.81405534229504894 ) ) ;
#20972 = CIRCLE ( 'NONE', #54920, 70.00000000000001421 ) ;
#20973 = VERTEX_POINT ( 'NONE', #92839 ) ;
#20974 = DIRECTION ( 'NONE',  ( -0.000000000000000000, -0.000000000000000000, -1.000000000000000000 ) ) ;
#20975 = CARTESIAN_POINT ( 'NONE',  ( 180.8664914282228722, 267.5501807654961226, 15.00410415709774270 ) ) ;
#20976 = LINE ( 'NONE', #27575, #91869 ) ;
#20977 = CARTESIAN_POINT ( 'NONE',  ( 81.87680903571094859, 41.76738865979471171, -5.626291927274185589 ) ) ;
#20978 = CARTESIAN_POINT ( 'NONE',  ( 161.8750289368003621, 250.2712207352165592, -13.97436367953006098 ) ) ;
#20979 = VECTOR ( 'NONE', #2905, 1000.000000000000000 ) ;
#20980 = CARTESIAN_POINT ( 'NONE',  ( 179.4151417752438817, 287.8800236340311471, -12.58290191272617520 ) ) ;
#20981 = CARTESIAN_POINT ( 'NONE',  ( 68.61209271804665377, 64.17778009964139585, -12.50907296292702320 ) ) ;
#20982 = CARTESIAN_POINT ( 'NONE',  ( 93.96783902534107824, 238.3927522451419350, 2.944929066748280225E-16 ) ) ;
#20983 = B_SPLINE_SURFACE_WITH_KNOTS ( 'NONE', 3, 1, ( 
 ( #33074, #48278 ),
 ( #85846, #87361 ),
 ( #47754, #8279 ),
 ( #71095, #55352 ),
 ( #16869, #1183 ),
 ( #78692, #9797 ),
 ( #38667, #77696 ),
 ( #31061, #32059 ),
 ( #31557, #24965 ),
 ( #40658, #71595 ),
 ( #17371, #69570 ),
 ( #17890, #39146 ),
 ( #62970, #70058 ),
 ( #94411, #61951 ),
 ( #78187, #675 ),
 ( #63967, #25472 ),
 ( #16373, #77172 ),
 ( #9280, #62446 ),
 ( #1694, #86330 ),
 ( #40154, #93919 ),
 ( #32578, #56363 ),
 ( #93415, #23964 ),
 ( #7776, #178 ),
 ( #47265, #92903 ),
 ( #24473, #23454 ),
 ( #55842, #54346 ),
 ( #8775, #85318 ),
 ( #86837, #15863 ),
 ( #46772, #54865 ),
 ( #39645, #70566 ),
 ( #89804, #64478 ) ),
 .UNSPECIFIED., .F., .F., .F.,
 ( 4, 3, 3, 3, 3, 3, 3, 3, 3, 3, 4 ),
 ( 2, 2 ),
 ( 0.000000000000000000, 0.1122669598086860482, 0.2243161639709787269, 0.3396355846219236696, 0.4553962076585217345, 0.5677860799922416213, 0.6749047109689670920, 0.7773884377078438268, 0.8775581155834327740, 0.9782364162377975569, 1.000000000000000000 ),
 ( 0.000000000000000000, 1.000000000000000000 ),
 .UNSPECIFIED. ) ;
#20984 = ORIENTED_EDGE ( 'NONE', *, *, #52362, .T. ) ;
#20985 = CARTESIAN_POINT ( 'NONE',  ( 194.8262681699237930, 266.4033461770301869, -7.730570064367828564 ) ) ;
#20986 = CARTESIAN_POINT ( 'NONE',  ( 202.3421728196210552, 280.1800714929709670, 16.85915999540957344 ) ) ;
#20987 = CARTESIAN_POINT ( 'NONE',  ( 154.2853090730916676, 265.4170011543745886, 17.16471700533586642 ) ) ;
#20988 = EDGE_CURVE ( 'NONE', #84449, #47085, #84745, .T. ) ;
#20989 = AXIS2_PLACEMENT_3D ( 'NONE', #2081, #71486, #32958 ) ;
#20990 = CARTESIAN_POINT ( 'NONE',  ( 15.38522827951586081, 173.5643266524160140, -9.188101187500093303 ) ) ;
#20991 = CARTESIAN_POINT ( 'NONE',  ( 71.29758602155226299, 68.80057128787699128, -9.575873472329016423 ) ) ;
#20992 = CARTESIAN_POINT ( 'NONE',  ( 80.62260327750492195, 51.59452065496885353, 15.50740165936294801 ) ) ;
#20993 = CARTESIAN_POINT ( 'NONE',  ( 71.61825016222245210, 59.02498431978696658, -15.35031316840264459 ) ) ;
#20994 = CARTESIAN_POINT ( 'NONE',  ( 66.77376812102318127, 68.41195941748605946, -4.433129028897194068 ) ) ;
#20995 = CARTESIAN_POINT ( 'NONE',  ( 50.35065686154756293, 206.0024278399160949, 9.188101187500095079 ) ) ;
#20996 = CARTESIAN_POINT ( 'NONE',  ( 163.7012083107868534, 247.1081852757374975, -6.544933039329257518 ) ) ;
#20997 = CARTESIAN_POINT ( 'NONE',  ( 203.6965450807731770, 276.1611523005571485, 13.27569016410228109 ) ) ;
#20998 = CARTESIAN_POINT ( 'NONE',  ( 69.87062716920111427, 69.39590680716997895, 6.536137438613790707 ) ) ;
#20999 = CARTESIAN_POINT ( 'NONE',  ( 207.6918009085542849, 270.9142438413412037, 7.009114282139513818 ) ) ;
#21000 = ORIENTED_EDGE ( 'NONE', *, *, #18207, .T. ) ;
#21001 = CARTESIAN_POINT ( 'NONE',  ( 10.41442975960284834, 183.4865022471903160, 10.00000000000009237 ) ) ;
#21002 = PLANE ( 'NONE',  #77345 ) ;
#21003 = CARTESIAN_POINT ( 'NONE',  ( 139.3076170325891212, 260.4244531367911577, -4.594050593750046652 ) ) ;
#21004 = CARTESIAN_POINT ( 'NONE',  ( 25.85429974905589745, 23.43085787977764056, -9.188101187500008038 ) ) ;
#21005 = CARTESIAN_POINT ( 'NONE',  ( 207.5820376350654612, 271.1043594078285537, -7.625615357094640778 ) ) ;
#21006 = CARTESIAN_POINT ( 'NONE',  ( 83.58053473790808141, 52.37444464214736684, -15.15899823554475212 ) ) ;
#21007 = CARTESIAN_POINT ( 'NONE',  ( 74.98034739464185350, 53.37963118822899133, -16.04958843571116134 ) ) ;
#21009 = CARTESIAN_POINT ( 'NONE',  ( 188.7211440809105341, 289.5549014049189509, 14.43271874758353235 ) ) ;
#21008 = CARTESIAN_POINT ( 'NONE',  ( 196.3519702320103590, 290.5554067223432639, 17.39042812051341969 ) ) ;
#21010 = CARTESIAN_POINT ( 'NONE',  ( 69.13437078241847189, 64.31265921892629933, 12.00033174088420118 ) ) ;
#21011 = ORIENTED_EDGE ( 'NONE', *, *, #80093, .T. ) ;
#21012 = CARTESIAN_POINT ( 'NONE',  ( 191.4484954869714954, 299.0484741143815199, 8.684991747358081327 ) ) ;
#21013 = CARTESIAN_POINT ( 'NONE',  ( 207.7972699113062731, 270.7315661699511224, -1.706133800161685476 ) ) ;
#21014 = CARTESIAN_POINT ( 'NONE',  ( 69.35136632105268006, 67.21048502454044637, -10.10453561268904821 ) ) ;
#21015 = CARTESIAN_POINT ( 'NONE',  ( 169.6032317452356324, 266.0645475789909824, -16.96121667089491325 ) ) ;
#21016 = ORIENTED_EDGE ( 'NONE', *, *, #41376, .T. ) ;
#21017 = CARTESIAN_POINT ( 'NONE',  ( 71.72012509582434348, 71.32916523519146779, 4.604336662656719703 ) ) ;
#21018 = DIRECTION ( 'NONE',  ( 0.5000000000000012212, -0.8660254037844379305, -0.000000000000000000 ) ) ;
#21019 = CARTESIAN_POINT ( 'NONE',  ( 71.89891490226827386, 72.23425543116729841, 0.5890436832873462425 ) ) ;
#21020 = CYLINDRICAL_SURFACE ( 'NONE', #99173, 10.00000000000001066 ) ;
#21021 = CARTESIAN_POINT ( 'NONE',  ( 196.2244288253768048, 270.9124372856092577, 12.11018688171617619 ) ) ;
#21022 = CARTESIAN_POINT ( 'NONE',  ( 183.7603294395054832, 295.5481930741308929, 4.675700597948987181 ) ) ;
#21023 = CARTESIAN_POINT ( 'NONE',  ( 67.45371725586859668, 68.64851772114370476, 4.944568755435953200 ) ) ;
#21024 = CARTESIAN_POINT ( 'NONE',  ( 150.7575236960178700, 277.9469932911979981, -5.090193068913281593E-05 ) ) ;
#21025 = DIRECTION ( 'NONE',  ( 0.000000000000000000, 0.000000000000000000, 1.000000000000000000 ) ) ;
#21026 = ORIENTED_EDGE ( 'NONE', *, *, #53690, .F. ) ;
#21027 = CARTESIAN_POINT ( 'NONE',  ( 194.3413770922408617, 282.8930799310762723, 17.82077676852630077 ) ) ;
#21028 = CARTESIAN_POINT ( 'NONE',  ( 13.32519098795206780, 19.64441083166259361, -10.00000000000000533 ) ) ;
#21029 = CARTESIAN_POINT ( 'NONE',  ( 83.13824623788876522, 45.58899862045078066, 11.00933188051684297 ) ) ;
#21030 = EDGE_LOOP ( 'NONE', ( #93814, #3014, #36229, #100155 ) ) ;
#21031 = CARTESIAN_POINT ( 'NONE',  ( 25.96864935082050252, 154.0458036431183189, -30.52142883766499892 ) ) ;
#21032 = FACE_OUTER_BOUND ( 'NONE', #94666, .T. ) ;
#21033 = CARTESIAN_POINT ( 'NONE',  ( 159.4145189439792887, 263.9450760762234722, -17.23651461227130710 ) ) ;
#21034 = VERTEX_POINT ( 'NONE', #14314 ) ;
#21035 = AXIS2_PLACEMENT_3D ( 'NONE', #73746, #88011, #20055 ) ;
#21036 = CARTESIAN_POINT ( 'NONE',  ( 191.8000917695741805, 298.4394914891611847, -9.452573400474340914 ) ) ;
#21037 = LINE ( 'NONE', #27133, #5516 ) ;
#21038 = CARTESIAN_POINT ( 'NONE',  ( 204.8284483594339065, 275.8737159363993214, 14.69997973035875383 ) ) ;
#21039 = CARTESIAN_POINT ( 'NONE',  ( 49.89075441544350298, 209.6115022471903160, -5.000000000000047962 ) ) ;
#21040 = ORIENTED_EDGE ( 'NONE', *, *, #82849, .T. ) ;
#21041 = CARTESIAN_POINT ( 'NONE',  ( 86.23641098298273278, 232.8464784336661353, 1.353441290958777525E-15 ) ) ;
#21042 = CARTESIAN_POINT ( 'NONE',  ( 47.39496755818312579, 108.2889530649357681, -10.00000000000000000 ) ) ;
#21043 = CARTESIAN_POINT ( 'NONE',  ( 72.84093999290330146, 56.97456911652175648, -16.40692799624909171 ) ) ;
#21044 = CARTESIAN_POINT ( 'NONE',  ( 181.8616327328832085, 257.2205658361911560, -6.091144281000731020 ) ) ;
#21045 = ORIENTED_EDGE ( 'NONE', *, *, #58865, .T. ) ;
#21046 = ORIENTED_EDGE ( 'NONE', *, *, #39023, .T. ) ;
#21047 = ADVANCED_FACE ( 'NONE', ( #76612 ), #38082, .T. ) ;
#21048 = CARTESIAN_POINT ( 'NONE',  ( 207.2939815914345161, 270.5662793833256501, 1.732060402802277022 ) ) ;
#21049 = EDGE_LOOP ( 'NONE', ( #66987, #50665, #33680, #36674 ) ) ;
#21050 = CARTESIAN_POINT ( 'NONE',  ( 81.81818204529017180, 52.08743214072829630, 15.02062431075104598 ) ) ;
#21051 = ORIENTED_EDGE ( 'NONE', *, *, #25364, .T. ) ;
#21052 = EDGE_CURVE ( 'NONE', #59353, #77173, #95703, .T. ) ;
#21053 = CARTESIAN_POINT ( 'NONE',  ( 48.48788556946983874, 102.1758113618167982, 10.00000000000000000 ) ) ;
#21054 = AXIS2_PLACEMENT_3D ( 'NONE', #71697, #86431, #24561 ) ;
#21055 = VERTEX_POINT ( 'NONE', #86767 ) ;
#21056 = CARTESIAN_POINT ( 'NONE',  ( 165.0728672701316100, 244.7324022674953312, 1.876804411200113210 ) ) ;
#21057 = CARTESIAN_POINT ( 'NONE',  ( 82.66373328861170933, 40.87911596418215510, 3.282672455158152314 ) ) ;
#21058 = EDGE_CURVE ( 'NONE', #3024, #63370, #55775, .T. ) ;
#21059 = FACE_OUTER_BOUND ( 'NONE', #72272, .T. ) ;
#21060 = EDGE_CURVE ( 'NONE', #37680, #24001, #47359, .T. ) ;
#21061 = CARTESIAN_POINT ( 'NONE',  ( 18.71383987920379255, 171.6115022471901739, -5.000000000000041744 ) ) ;
#21062 = B_SPLINE_CURVE_WITH_KNOTS ( 'NONE', 3,
 ( #13790, #6190, #98416, #68476 ),
 .UNSPECIFIED., .F., .F.,
 ( 4, 4 ),
 ( 0.002244590204956481774, 0.004621833422667826624 ),
 .UNSPECIFIED. ) ;
#21063 = CARTESIAN_POINT ( 'NONE',  ( 70.83016151729651710, 68.41586035902774654, -8.977235470963222497 ) ) ;
#21064 = CARTESIAN_POINT ( 'NONE',  ( 164.7521862919904549, 265.1279320591024202, -16.62063656794546418 ) ) ;
#21065 = ORIENTED_EDGE ( 'NONE', *, *, #9843, .T. ) ;
#21066 = CARTESIAN_POINT ( 'NONE',  ( 76.40286963592521374, 58.21049690025673584, 16.06783727834804409 ) ) ;
#21067 = CARTESIAN_POINT ( 'NONE',  ( 4.137530017820134631, 25.49540643055185285, 3.479690158560446702E-15 ) ) ;
#21068 = VERTEX_POINT ( 'NONE', #2625 ) ;
#21069 = CIRCLE ( 'NONE', #3279, 49.99999999999999289 ) ;
#21070 = CARTESIAN_POINT ( 'NONE',  ( 165.4473470637335879, 246.0837842385732301, 3.196113342258863899 ) ) ;
#21072 = ORIENTED_EDGE ( 'NONE', *, *, #77053, .T. ) ;
#21071 = CARTESIAN_POINT ( 'NONE',  ( 199.9558687439891855, 270.1792697243771499, 10.11239592992032144 ) ) ;
#21073 = LINE ( 'NONE', #30640, #57693 ) ;
#21074 = CARTESIAN_POINT ( 'NONE',  ( 159.9997000813754084, 253.5193855937126841, -16.28798248637880519 ) ) ;
#21075 = CARTESIAN_POINT ( 'NONE',  ( 149.9429820946090217, 276.2925415708097034, -5.357056126780523009 ) ) ;
#21076 = CARTESIAN_POINT ( 'NONE',  ( 165.1821270928554952, 246.6881764609589425, -1.872407309469820813 ) ) ;
#21077 = PLANE ( 'NONE',  #28540 ) ;
#21078 = CARTESIAN_POINT ( 'NONE',  ( 85.86558718211738039, 43.20781965171007499, 3.226128779682295722 ) ) ;
#21079 = CARTESIAN_POINT ( 'NONE',  ( 88.28703488708569580, 44.33872872310907809, -2.279783701773686388 ) ) ;
#21080 = ORIENTED_EDGE ( 'NONE', *, *, #9616, .T. ) ;
#21081 = FACE_OUTER_BOUND ( 'NONE', #88630, .T. ) ;
#21082 = B_SPLINE_CURVE_WITH_KNOTS ( 'NONE', 3,
 ( #71933, #18727, #79565, #81551, #63816, #88180 ),
 .UNSPECIFIED., .F., .F.,
 ( 4, 2, 4 ),
 ( 0.000000000000000000, 0.2986716297182049340, 0.5973432594364098680 ),
 .UNSPECIFIED. ) ;
#21083 = CARTESIAN_POINT ( 'NONE',  ( 75.08013308270210473, 67.09339902234965791, -13.09435070823462866 ) ) ;
#21084 = ORIENTED_EDGE ( 'NONE', *, *, #13227, .F. ) ;
#21085 = CYLINDRICAL_SURFACE ( 'NONE', #28961, 49.99999999999999289 ) ;
#21086 = CARTESIAN_POINT ( 'NONE',  ( 174.9842232683056409, 281.3912648188263006, -14.16965494358151290 ) ) ;
#21087 = CARTESIAN_POINT ( 'NONE',  ( 204.0342455540030926, 277.2493155469190356, -14.37282112774435028 ) ) ;
#21088 = CARTESIAN_POINT ( 'NONE',  ( 83.69930633818603383, 44.66246776289806064, -8.864960664055317352 ) ) ;
#21089 = CARTESIAN_POINT ( 'NONE',  ( 104.9037214839949002, 219.8262482093457777, 3.021315404115420679E-15 ) ) ;
#21091 = CARTESIAN_POINT ( 'NONE',  ( 115.4120517331926408, 225.8932355074535678, -2.679491924311248496 ) ) ;
#21090 = CARTESIAN_POINT ( 'NONE',  ( -3.126064726376516667, 162.8768266524159856, -9.188101187500091527 ) ) ;
#21092 = CARTESIAN_POINT ( 'NONE',  ( 188.9023514920928619, 296.9480906869840737, 8.133443239242762246 ) ) ;
#21093 = ORIENTED_EDGE ( 'NONE', *, *, #52522, .T. ) ;
#21094 = ORIENTED_EDGE ( 'NONE', *, *, #24594, .F. ) ;
#21095 = LINE ( 'NONE', #83908, #66220 ) ;
#21096 = DIRECTION ( 'NONE',  ( -1.000000000000000000, 0.000000000000000000, 0.000000000000000000 ) ) ;
#21097 = CARTESIAN_POINT ( 'NONE',  ( 85.62951787902757417, 48.90316132097375856, -12.13537779016860085 ) ) ;
#21098 = CARTESIAN_POINT ( 'NONE',  ( 67.00368147268072505, 66.95831323777278499, -8.716692028962587102 ) ) ;
#21099 = LINE ( 'NONE', #52961, #38797 ) ;
#21100 = CARTESIAN_POINT ( 'NONE',  ( 70.32555767554718784, 69.76210374709671669, 7.334934889506363298 ) ) ;
#21101 = CARTESIAN_POINT ( 'NONE',  ( 149.7728113105055172, 277.1702417969415251, 3.080250329875358961 ) ) ;
#21102 = CARTESIAN_POINT ( 'NONE',  ( 26.88721494746919660, 177.1423013555409796, -4.594050593750043987 ) ) ;
#21103 = CYLINDRICAL_SURFACE ( 'NONE', #83944, 70.00000000000002842 ) ;
#21104 = CARTESIAN_POINT ( 'NONE',  ( 186.2154994046558159, 296.8723033710291475, -7.399325338573278010 ) ) ;
#21105 = CARTESIAN_POINT ( 'NONE',  ( 78.16778150852306339, 52.08950074027319488, 15.56147700446086013 ) ) ;
#21106 = B_SPLINE_CURVE_WITH_KNOTS ( 'NONE', 3,
 ( #77759, #47328, #41220, #93979, #79292, #18457, #62514, #40214, #9863, #8342 ),
 .UNSPECIFIED., .F., .F.,
 ( 4, 2, 2, 2, 4 ),
 ( 0.000000000000000000, 0.0002622400424271630840, 0.0005244800848543261680, 0.0007867201272814892520, 0.001048960169708652336 ),
 .UNSPECIFIED. ) ;
#21107 = DIRECTION ( 'NONE',  ( 0.000000000000000000, -0.000000000000000000, -1.000000000000000000 ) ) ;
#21108 = EDGE_CURVE ( 'NONE', #65984, #16838, #11145, .T. ) ;
#21109 = CARTESIAN_POINT ( 'NONE',  ( 190.7618201014540773, 299.8460682594623563, -4.647714112044580403 ) ) ;
#21110 = LINE ( 'NONE', #43872, #77672 ) ;
#21111 = CARTESIAN_POINT ( 'NONE',  ( 207.8718670335145475, 270.6023601641878713, -6.322166851501095586 ) ) ;
#21112 = CARTESIAN_POINT ( 'NONE',  ( 194.3442947553755005, 294.0328026529847421, -15.97648891113594871 ) ) ;
#21113 = CARTESIAN_POINT ( 'NONE',  ( 85.05685448785742153, 49.86430017123296210, 13.48384481714161787 ) ) ;
#21114 = CARTESIAN_POINT ( 'NONE',  ( -110.0000000000000000, 15.00000000000000000, -59.99999999999999289 ) ) ;
#21115 = CARTESIAN_POINT ( 'NONE',  ( 172.5891611840680469, 287.6914292476137689, -9.739357961162628641 ) ) ;
#21116 = CARTESIAN_POINT ( 'NONE',  ( 162.6382063110229410, 251.1910714611167919, -12.78875127087469998 ) ) ;
#21117 = CARTESIAN_POINT ( 'NONE',  ( 51.53259423990365207, 193.8927522451418213, 10.00000000000009948 ) ) ;
#21118 = AXIS2_PLACEMENT_3D ( 'NONE', #34399, #65297, #43971 ) ;
#21119 = CARTESIAN_POINT ( 'NONE',  ( 172.8718622337294732, 262.9888249722745286, -15.65873574236441357 ) ) ;
#21120 = EDGE_CURVE ( 'NONE', #15680, #8119, #72705, .T. ) ;
#21121 = CARTESIAN_POINT ( 'NONE',  ( 102.2314250767153538, 220.6423013555409796, -4.594050593750043987 ) ) ;
#21122 = CARTESIAN_POINT ( 'NONE',  ( 6.742211794378569323, 25.93396525600388003, 2.839279412974139660 ) ) ;
#21123 = CARTESIAN_POINT ( 'NONE',  ( 84.55537670905214043, 50.62155581810766591, -14.09136642048689936 ) ) ;
#21125 = CARTESIAN_POINT ( 'NONE',  ( 200.4541693463981744, 283.4501894334596841, 17.82706366043037960 ) ) ;
#21124 = CARTESIAN_POINT ( 'NONE',  ( 157.3412122618683497, 258.1240215684019290, 16.75554199904894048 ) ) ;
#21126 = CARTESIAN_POINT ( 'NONE',  ( 149.6746633631864825, 271.4028737796298856, 12.81448833497433881 ) ) ;
#21127 = CARTESIAN_POINT ( 'NONE',  ( 151.1811967613751335, 268.7934813906678642, -15.79361349403328418 ) ) ;
#21128 = FACE_OUTER_BOUND ( 'NONE', #71795, .T. ) ;
#21129 = CARTESIAN_POINT ( 'NONE',  ( 32.54976882715482134, 40.83396525600392835, -2.839279412974133887 ) ) ;
#21130 = CARTESIAN_POINT ( 'NONE',  ( 147.2567621633200474, 275.5908015054806128, -3.647191014543873955 ) ) ;
#21131 = FACE_BOUND ( 'NONE', #20943, .T. ) ;
#21132 = ORIENTED_EDGE ( 'NONE', *, *, #72048, .T. ) ;
#21133 = CARTESIAN_POINT ( 'NONE',  ( 28.29779127713939602, 18.19860640527293327, 2.839279412974134775 ) ) ;
#21134 = CARTESIAN_POINT ( 'NONE',  ( 17.29678581741014654, 10.39040679176981996, 1.333680081654574804E-15 ) ) ;
#21135 = CARTESIAN_POINT ( 'NONE',  ( 193.2100161762185735, 295.9974307820218087, -12.46499585622781758 ) ) ;
#21136 = LINE ( 'NONE', #59591, #93041 ) ;
#21137 = ORIENTED_EDGE ( 'NONE', *, *, #31757, .T. ) ;
#21138 = CARTESIAN_POINT ( 'NONE',  ( 70.94564442840402307, 61.10112560036777296, 15.01654231012169483 ) ) ;
#21139 = CARTESIAN_POINT ( 'NONE',  ( 159.4889735931715222, 254.4039898200529706, 16.88104032092801887 ) ) ;
#21140 = CARTESIAN_POINT ( 'NONE',  ( 193.8324327182400282, 288.0664881071944023, 17.07309623557379297 ) ) ;
#21141 = DIRECTION ( 'NONE',  ( -0.8660254037844387076, -0.4999999999999998890, -0.000000000000000000 ) ) ;
#21142 = CARTESIAN_POINT ( 'NONE',  ( 75.11446029513938072, 52.98301679529475905, -16.48354851564725365 ) ) ;
#21143 = CARTESIAN_POINT ( 'NONE',  ( 135.6272693901030095, 249.1115022471902591, 10.00000000000009592 ) ) ;
#21144 = LINE ( 'NONE', #77704, #84515 ) ;
#21145 = ORIENTED_EDGE ( 'NONE', *, *, #6148, .T. ) ;
#21146 = CARTESIAN_POINT ( 'NONE',  ( 86.10138557494317979, 45.87410591191778053, -9.436449708986739182 ) ) ;
#21147 = ORIENTED_EDGE ( 'NONE', *, *, #36945, .F. ) ;
#21148 = LINE ( 'NONE', #21629, #85540 ) ;
#21149 = DIRECTION ( 'NONE',  ( -0.000000000000000000, -0.000000000000000000, -1.000000000000000000 ) ) ;
#21150 = ORIENTED_EDGE ( 'NONE', *, *, #59561, .T. ) ;
#21151 = CARTESIAN_POINT ( 'NONE',  ( 181.4476193698807549, 290.8642548751454342, -11.08784992509195000 ) ) ;
#21152 = ORIENTED_EDGE ( 'NONE', *, *, #63015, .T. ) ;
#21153 = CARTESIAN_POINT ( 'NONE',  ( 164.7124890890957545, 259.3090575768129042, 16.88404478802990738 ) ) ;
#21154 = CARTESIAN_POINT ( 'NONE',  ( 158.8074094763257449, 255.5844934990455499, 17.62168084431520043 ) ) ;
#21155 = CARTESIAN_POINT ( 'NONE',  ( 190.7959044753356181, 278.1545862522023640, -16.79819019203270969 ) ) ;
#21156 = CARTESIAN_POINT ( 'NONE',  ( 153.8428010968516162, 264.1834474519768605, -18.07686942510439110 ) ) ;
#21157 = CARTESIAN_POINT ( 'NONE',  ( 201.1060504099706350, 282.3210983108598384, -18.18000168485860257 ) ) ;
#21158 = CARTESIAN_POINT ( 'NONE',  ( 42.23901261427005949, 30.10170272979930672, -7.433330006724141015 ) ) ;
#21159 = CARTESIAN_POINT ( 'NONE',  ( 77.93566872935365097, 58.95233904213321097, -16.11642214640332327 ) ) ;
#21160 = EDGE_CURVE ( 'NONE', #20583, #81472, #66752, .T. ) ;
#21161 = CARTESIAN_POINT ( 'NONE',  ( 7.864685750751951865, 30.05722773587472929, -10.00000000000000000 ) ) ;
#21162 = CARTESIAN_POINT ( 'NONE',  ( 87.64900631941344500, 45.32217229061651409, 6.433208773102475853 ) ) ;
#21163 = EDGE_LOOP ( 'NONE', ( #40925, #66595, #78013, #23768, #54126, #58653, #54028, #7796, #35081, #82983, #84493, #54529, #78136, #69192, #12026, #44690, #68321, #69259, #58393, #585, #53764, #68096, #30974, #75224, #22864, #31810, #98451, #62256, #79617, #15498, #28649, #98146, #81282, #29006, #24781, #79127, #94297, #99261, #31084, #36565, #267, #92704, #61875, #51069, #40839, #45924, #73343, #25878, #85832, #10819, #27226, #66995, #10321, #51176 ) ) ;
#21164 = ORIENTED_EDGE ( 'NONE', *, *, #54057, .F. ) ;
#21165 = CARTESIAN_POINT ( 'NONE',  ( 81.65310433048475147, 42.64019311979919280, 7.560891536010023728 ) ) ;
#21167 = DIRECTION ( 'NONE',  ( -0.8660254037844384856, -0.5000000000000002220, -3.252519625699449945E-16 ) ) ;
#21166 = CARTESIAN_POINT ( 'NONE',  ( 204.9427641582406636, 275.6757151647582305, 14.40446820030680897 ) ) ;
#21168 = CARTESIAN_POINT ( 'NONE',  ( 199.3225951545807106, 279.5975192435293479, 16.97220939274292206 ) ) ;
#21169 = CARTESIAN_POINT ( 'NONE',  ( 197.4063992150350373, 273.1943876493294852, -13.35659089524287602 ) ) ;
#21170 = CARTESIAN_POINT ( 'NONE',  ( 73.51647790488874534, 61.26934504900349054, -15.03881460934114678 ) ) ;
#21171 = CARTESIAN_POINT ( 'NONE',  ( 82.32345403531087413, 40.35629778586039151, 1.222851117235266960 ) ) ;
#21172 = CARTESIAN_POINT ( 'NONE',  ( 171.0233422444486280, 287.7839941292462527, -4.495013932621471753 ) ) ;
#21173 = EDGE_CURVE ( 'NONE', #20256, #85118, #19598, .T. ) ;
#21174 = CARTESIAN_POINT ( 'NONE',  ( 76.95483076014906487, 63.96668203270510134, -15.25269828761453894 ) ) ;
#21175 = CARTESIAN_POINT ( 'NONE',  ( 178.1648171342568219, 255.5065660826824114, 4.897822005985157823 ) ) ;
#21176 = CARTESIAN_POINT ( 'NONE',  ( 116.7098534265301595, 244.3149278399160949, -9.188101187500095079 ) ) ;
#21177 = ORIENTED_EDGE ( 'NONE', *, *, #12730, .F. ) ;
#21178 = CARTESIAN_POINT ( 'NONE',  ( 148.0632853866802350, 275.0336310366062094, -5.814038160505428543 ) ) ;
#21179 = CARTESIAN_POINT ( 'NONE',  ( 187.1789365411204926, 291.3781964708418286, -14.15416893886036220 ) ) ;
#21180 = EDGE_LOOP ( 'NONE', ( #56271, #71660, #82731, #18567 ) ) ;
#21181 = VERTEX_POINT ( 'NONE', #5597 ) ;
#21182 = CARTESIAN_POINT ( 'NONE',  ( 184.5564966555429862, 297.9066928836515444, -1.116615600582069101 ) ) ;
#21183 = CARTESIAN_POINT ( 'NONE',  ( 180.7178857814544699, 294.1703499652309119, -2.354211428759664493 ) ) ;
#21184 = CARTESIAN_POINT ( 'NONE',  ( 157.8562613713738472, 257.2319303423452652, 17.81420683562559404 ) ) ;
#21185 = CARTESIAN_POINT ( 'NONE',  ( 159.9647205790309101, 253.5799718689968927, -16.48298384325780219 ) ) ;
#21186 = CARTESIAN_POINT ( 'NONE',  ( -26.39329008703066748, 34.77772847211986829, 59.99999999999999289 ) ) ;
#21187 = ORIENTED_EDGE ( 'NONE', *, *, #54563, .F. ) ;
#21188 = AXIS2_PLACEMENT_3D ( 'NONE', #38049, #38557, #52272 ) ;
#21189 = ORIENTED_EDGE ( 'NONE', *, *, #7613, .F. ) ;
#21190 = LINE ( 'NONE', #76387, #59167 ) ;
#21191 = ORIENTED_EDGE ( 'NONE', *, *, #77006, .F. ) ;
#21192 = DIRECTION ( 'NONE',  ( 1.000000000000000000, 0.000000000000000000, 0.000000000000000000 ) ) ;
#21193 = CARTESIAN_POINT ( 'NONE',  ( -7.429302001086912632, 166.5177522451418781, -10.00000000000009592 ) ) ;
#21194 = CARTESIAN_POINT ( 'NONE',  ( 83.72465858224470026, 48.53636785707922030, 12.63852326360208522 ) ) ;
#21196 = CARTESIAN_POINT ( 'NONE',  ( 69.47943944392696380, 63.02522356655473601, -13.62731951106632344 ) ) ;
#21195 = CARTESIAN_POINT ( 'NONE',  ( 198.0482269745670862, 285.9982792772420908, 17.61538258229827747 ) ) ;
#21197 = CARTESIAN_POINT ( 'NONE',  ( 200.9445292274600092, 282.6008612054670266, -16.62830946367346741 ) ) ;
#21198 = ORIENTED_EDGE ( 'NONE', *, *, #78320, .T. ) ;
#21199 = CARTESIAN_POINT ( 'NONE',  ( 157.1187995864133882, 258.5092516225370218, 18.42986330599266509 ) ) ;
#21200 = CARTESIAN_POINT ( 'NONE',  ( 174.5885488454506174, 256.4458599265808516, 12.05082362884263425 ) ) ;
#21201 = CARTESIAN_POINT ( 'NONE',  ( 189.8223291672571236, 263.2674012269775972, -9.776181882378969235 ) ) ;
#21202 = CARTESIAN_POINT ( 'NONE',  ( 173.4224352300193175, 251.4084521971564072, -0.8939200208722334340 ) ) ;
#21203 = CARTESIAN_POINT ( 'NONE',  ( 178.1545585138619572, 285.2582789952114126, 13.03273863630066209 ) ) ;
#21204 = CARTESIAN_POINT ( 'NONE',  ( 72.03850700256526807, 72.31288868693221161, 3.399215934587860755 ) ) ;
#21205 = DIRECTION ( 'NONE',  ( 0.000000000000000000, -0.000000000000000000, -1.000000000000000000 ) ) ;
#21206 = FACE_OUTER_BOUND ( 'NONE', #74359, .T. ) ;
#21207 = CARTESIAN_POINT ( 'NONE',  ( 69.20277302375480133, 70.19697236206943103, -3.254991052223795034 ) ) ;
#21208 = CARTESIAN_POINT ( 'NONE',  ( 55.84441874286383722, 212.2369531367911293, -4.594050593750048428 ) ) ;
#21209 = CARTESIAN_POINT ( 'NONE',  ( 159.2186641046529303, 254.8721795879351646, -15.96198087403305443 ) ) ;
#21210 = DIRECTION ( 'NONE',  ( 0.5000000000000001110, -0.8660254037844387076, 0.000000000000000000 ) ) ;
#21211 = CARTESIAN_POINT ( 'NONE',  ( 162.9111474110223412, 248.4766108952035211, -9.702990628959184960 ) ) ;
#21212 = CARTESIAN_POINT ( 'NONE',  ( 66.62667948677777474, 67.60859431869941716, 6.219768998119001857 ) ) ;
#21213 = EDGE_CURVE ( 'NONE', #63766, #7578, #97327, .T. ) ;
#21214 = CARTESIAN_POINT ( 'NONE',  ( 207.2337123599961899, 271.7076764818092443, -5.443417788256701861 ) ) ;
#21215 = CARTESIAN_POINT ( 'NONE',  ( 66.60565428985405845, 69.00412068662672027, 1.122078433852597756 ) ) ;
#21216 = CARTESIAN_POINT ( 'NONE',  ( -20.92890603600389099, 95.09343599062782459, 45.19939615752831230 ) ) ;
#21217 = CARTESIAN_POINT ( 'NONE',  ( 111.7912168577913974, 246.8967562850347122, -4.648177544792955347E-16 ) ) ;
#21218 = ADVANCED_FACE ( 'NONE', ( #74019 ), #89750, .F. ) ;
#21219 = CARTESIAN_POINT ( 'NONE',  ( 74.14312167556930433, 66.30466486950707861, 1.224646799147354045E-15 ) ) ;
#21220 = CYLINDRICAL_SURFACE ( 'NONE', #43364, 17.82106496071139645 ) ;
#21221 = PLANE ( 'NONE',  #52700 ) ;
#21222 = CARTESIAN_POINT ( 'NONE',  ( 72.15865790475056940, 72.27389710013802926, 3.820985825366556288 ) ) ;
#21223 = EDGE_CURVE ( 'NONE', #76155, #81724, #4098, .T. ) ;
#21224 = CARTESIAN_POINT ( 'NONE',  ( 9.827979128326980174, 29.57595373812808504, 177.5919119679930134 ) ) ;
#21225 = CARTESIAN_POINT ( 'NONE',  ( 44.94038342867872871, 31.11029122506298705, -8.090169943749478065 ) ) ;
#21226 = DIRECTION ( 'NONE',  ( -0.9974094913373522386, -0.07193265315671491800, 0.000000000000000000 ) ) ;
#21227 = CARTESIAN_POINT ( 'NONE',  ( 71.95941895756688211, 72.18221666786446633, -1.667998158078391580 ) ) ;
#21228 = CARTESIAN_POINT ( 'NONE',  ( 47.42782112377506820, 204.3149278399161233, 9.188101187500093303 ) ) ;
#21229 = CARTESIAN_POINT ( 'NONE',  ( 18.97660828663255117, 29.14336893147755703, 7.433330006724141015 ) ) ;
#21230 = DIRECTION ( 'NONE',  ( 0.8660254037844395958, 0.4999999999999985567, 0.000000000000000000 ) ) ;
#21231 = CARTESIAN_POINT ( 'NONE',  ( 149.6230451358742926, 271.4922791719315001, -12.72565967355361671 ) ) ;
#21232 = CARTESIAN_POINT ( 'NONE',  ( 10.86724236217879458, 11.98920272979924206, 7.433330006724137462 ) ) ;
#21233 = CARTESIAN_POINT ( 'NONE',  ( 198.0457135053186448, 287.1931070555794463, 16.94346135465734449 ) ) ;
#21234 = CARTESIAN_POINT ( 'NONE',  ( 175.6626792159711670, 291.0177071100450235, 2.486975767635404733 ) ) ;
#21235 = CARTESIAN_POINT ( 'NONE',  ( 180.0647771456566204, 276.3369416177878293, 17.44453780294904632 ) ) ;
#21236 = CARTESIAN_POINT ( 'NONE',  ( 82.28994638316029864, 40.89106665807588570, -1.238503865524188230 ) ) ;
#21237 = CARTESIAN_POINT ( 'NONE',  ( 72.95907369655466823, 67.57205448826327654, -11.22974281285723386 ) ) ;
#21238 = CARTESIAN_POINT ( 'NONE',  ( 163.3406587279032181, 256.0941660840857139, -14.91928245677631004 ) ) ;
#21239 = EDGE_CURVE ( 'NONE', #66517, #28862, #43593, .T. ) ;
#21240 = VECTOR ( 'NONE', #27486, 1000.000000000000000 ) ;
#21241 = CARTESIAN_POINT ( 'NONE',  ( 73.65303845931325100, 57.26316287700933572, -15.95429008473792010 ) ) ;
#21242 = CARTESIAN_POINT ( 'NONE',  ( 99.25420243115651431, 238.1115022471902876, -5.000000000000047962 ) ) ;
#21243 = CARTESIAN_POINT ( 'NONE',  ( 200.5621507313343557, 283.2631601884785368, 16.81037192529623425 ) ) ;
#21244 = CARTESIAN_POINT ( 'NONE',  ( 164.8669435086126498, 270.4944952562744334, -16.92984481350135084 ) ) ;
#21245 = ORIENTED_EDGE ( 'NONE', *, *, #41876, .T. ) ;
#21246 = CARTESIAN_POINT ( 'NONE',  ( 56.62968813474974894, 197.3768266524160140, -9.188101187500091527 ) ) ;
#21247 = ORIENTED_EDGE ( 'NONE', *, *, #96749, .T. ) ;
#21248 = DIRECTION ( 'NONE',  ( 0.000000000000000000, 0.000000000000000000, 1.000000000000000000 ) ) ;
#21249 = CARTESIAN_POINT ( 'NONE',  ( 146.8000281410530192, 276.3818880375922049, 4.652863924796177386 ) ) ;
#21250 = DIRECTION ( 'NONE',  ( -0.000000000000000000, -0.000000000000000000, -1.000000000000000000 ) ) ;
#21251 = VERTEX_POINT ( 'NONE', #4606 ) ;
#21252 = CARTESIAN_POINT ( 'NONE',  ( -73.66720466879951346, 50.53642055324488780, -10.00000000000000000 ) ) ;
#21253 = CARTESIAN_POINT ( 'NONE',  ( 79.16585775594589336, 45.99645177219947811, -13.18380221157910981 ) ) ;
#21254 = CARTESIAN_POINT ( 'NONE',  ( 45.80758703142363686, 72.03864405183792030, -10.00000000000000000 ) ) ;
#21255 = CARTESIAN_POINT ( 'NONE',  ( 177.1935088715161157, 274.8242815821236036, -17.29576750977079769 ) ) ;
#21256 = CARTESIAN_POINT ( 'NONE',  ( 206.6389649419900536, 271.5030152196637800, -6.665702415263554670 ) ) ;
#21257 = CARTESIAN_POINT ( 'NONE',  ( 204.6861706212249885, 276.1201482077632363, 14.69005155300678922 ) ) ;
#21258 = VERTEX_POINT ( 'NONE', #35496 ) ;
#21259 = CARTESIAN_POINT ( 'NONE',  ( 25.05680157815287146, 15.26216523072494979, -2.296566073217252530E-15 ) ) ;
#21260 = CARTESIAN_POINT ( 'NONE',  ( 25.04820903906726670, 30.16454794089042579, -10.00000000000000355 ) ) ;
#21261 = CARTESIAN_POINT ( 'NONE',  ( 190.7404869014439726, 298.2747809567102308, -9.591077548819823662 ) ) ;
#21262 = CARTESIAN_POINT ( 'NONE',  ( 175.0387250457744983, 253.3993311541219953, -7.863511161993287146 ) ) ;
#21263 = ADVANCED_FACE ( 'NONE', ( #66400 ), #55316, .F. ) ;
#21264 = EDGE_CURVE ( 'NONE', #55501, #21644, #36268, .T. ) ;
#21265 = VERTEX_POINT ( 'NONE', #20689 ) ;
#21266 = CARTESIAN_POINT ( 'NONE',  ( 75.98104421109889017, 51.53574906954564483, 16.18761828508177203 ) ) ;
#21267 = CARTESIAN_POINT ( 'NONE',  ( 166.9356869029893460, 261.4657499883571177, 16.52387450907458799 ) ) ;
#21268 = CARTESIAN_POINT ( 'NONE',  ( 206.0870578475358172, 273.6937403561189512, -10.07771901274806581 ) ) ;
#21269 = ORIENTED_EDGE ( 'NONE', *, *, #57284, .T. ) ;
#21270 = EDGE_CURVE ( 'NONE', #79646, #73728, #73859, .T. ) ;
#21272 = DIRECTION ( 'NONE',  ( 0.4999999999999992784, -0.8660254037844390407, 0.000000000000000000 ) ) ;
#21271 = LINE ( 'NONE', #83097, #79499 ) ;
#21273 = CARTESIAN_POINT ( 'NONE',  ( 207.6523394534040392, 270.9825930866021508, -2.115019688068903392 ) ) ;
#21274 = CARTESIAN_POINT ( 'NONE',  ( 66.29246560487287354, 68.68673832763016662, -2.132538888833254376 ) ) ;
#21275 = CARTESIAN_POINT ( 'NONE',  ( 188.4688990864094080, 295.3997683978527675, -11.43812978727723717 ) ) ;
#21276 = CARTESIAN_POINT ( 'NONE',  ( 74.14312167556930433, 66.30466486950707861, 1.224646799147354045E-15 ) ) ;
#21277 = CARTESIAN_POINT ( 'NONE',  ( 164.6182694729110949, 265.1159723368043615, -16.62666970452827186 ) ) ;
#21278 = CARTESIAN_POINT ( 'NONE',  ( 130.8102634016018442, 237.1423013555409796, -4.594050593750043987 ) ) ;
#21279 = ADVANCED_FACE ( 'NONE', ( #82535 ), #43959, .T. ) ;
#21280 = B_SPLINE_CURVE_WITH_KNOTS ( 'NONE', 3,
 ( #77394, #45474, #39357, #92140 ),
 .UNSPECIFIED., .F., .F.,
 ( 4, 4 ),
 ( 0.03072821384799830427, 0.03979477762634543725 ),
 .UNSPECIFIED. ) ;
#21281 = DIRECTION ( 'NONE',  ( -0.5000000000000003331, 0.8660254037844385966, -4.336808689942041895E-16 ) ) ;
#21282 = VERTEX_POINT ( 'NONE', #74897 ) ;
#21283 = DIRECTION ( 'NONE',  ( -0.8660254037844379305, -0.5000000000000014433, -0.000000000000000000 ) ) ;
#21284 = DIRECTION ( 'NONE',  ( 0.4999999999999998890, -0.8660254037844385966, 0.000000000000000000 ) ) ;
#21285 = ORIENTED_EDGE ( 'NONE', *, *, #58981, .F. ) ;
#21286 = CARTESIAN_POINT ( 'NONE',  ( 201.2310239275262518, 281.6122570310417359, 16.42038788625619716 ) ) ;
#21287 = ORIENTED_EDGE ( 'NONE', *, *, #21108, .F. ) ;
#21288 = ORIENTED_EDGE ( 'NONE', *, *, #35737, .F. ) ;
#21289 = ADVANCED_FACE ( 'NONE', ( #89158 ), #65282, .F. ) ;
#21290 = CARTESIAN_POINT ( 'NONE',  ( 149.3118911495987788, 247.0312136851381126, 5.028230608967417581 ) ) ;
#21291 = LINE ( 'NONE', #35969, #67737 ) ;
#21292 = EDGE_CURVE ( 'NONE', #1341, #69600, #6283, .T. ) ;
#21293 = CARTESIAN_POINT ( 'NONE',  ( 191.0050299662194107, 260.5068323652516824, -0.1977049704586299195 ) ) ;
#21294 = FACE_OUTER_BOUND ( 'NONE', #23348, .T. ) ;
#21295 = CARTESIAN_POINT ( 'NONE',  ( 81.89485588203808675, 55.22971306509116829, 16.24120679747550966 ) ) ;
#21296 = CARTESIAN_POINT ( 'NONE',  ( 155.3738696901333469, 261.5315588585399951, 17.02116401938635804 ) ) ;
#21297 = CARTESIAN_POINT ( 'NONE',  ( 71.88442714016632351, 67.86911030617876861, 10.31212540994018845 ) ) ;
#21298 = EDGE_LOOP ( 'NONE', ( #16374, #25520 ) ) ;
#21299 = LINE ( 'NONE', #73021, #51195 ) ;
#21300 = CARTESIAN_POINT ( 'NONE',  ( 152.6873874250818517, 266.1846826352417565, -16.66598363829485763 ) ) ;
#21301 = CARTESIAN_POINT ( 'NONE',  ( 66.07615688706256662, 68.56483294533278183, -4.482668677586966410 ) ) ;
#21302 = ORIENTED_EDGE ( 'NONE', *, *, #4908, .T. ) ;
#21303 = CARTESIAN_POINT ( 'NONE',  ( 76.11324214256561049, 51.53514024512487168, -16.17221011286880739 ) ) ;
#21304 = CARTESIAN_POINT ( 'NONE',  ( 174.7528540796445213, 253.3049902866633261, -7.833201063209856763 ) ) ;
#21305 = CARTESIAN_POINT ( 'NONE',  ( 164.3090168944849836, 246.0554299274959931, 2.641760039552302430 ) ) ;
#21306 = CARTESIAN_POINT ( 'NONE',  ( 198.9892818938948551, 281.0772271664100117, 17.34293942954158751 ) ) ;
#21307 = CARTESIAN_POINT ( 'NONE',  ( 164.1821508476733698, 246.2751683663292397, -7.347745041495428175 ) ) ;
#21308 = CARTESIAN_POINT ( 'NONE',  ( 133.4890956248536895, 254.0024278399161233, 9.188101187500095079 ) ) ;
#21309 = ORIENTED_EDGE ( 'NONE', *, *, #48446, .F. ) ;
#21310 = CARTESIAN_POINT ( 'NONE',  ( 25.98835327777827686, 41.64452202306098627, -10.00000000000000000 ) ) ;
#21311 = CARTESIAN_POINT ( 'NONE',  ( 85.64695507815616793, 43.83368588307220648, 5.542843691885481761 ) ) ;
#21312 = CARTESIAN_POINT ( 'NONE',  ( 87.86620516538259551, 44.01520320156028987, -1.811253330505868453 ) ) ;
#21313 = CARTESIAN_POINT ( 'NONE',  ( 73.03643456002411938, 70.76102034836752352, 7.524419617173737862 ) ) ;
#21314 = AXIS2_PLACEMENT_3D ( 'NONE', #48150, #79093, #85715 ) ;
#21315 = DIRECTION ( 'NONE',  ( -0.9825923819316327856, -0.1857746241280557598, 0.000000000000000000 ) ) ;
#21316 = EDGE_LOOP ( 'NONE', ( #25408, #63270, #62858, #21051 ) ) ;
#21317 = CARTESIAN_POINT ( 'NONE',  ( 76.05868104838350519, 52.63099806928217106, 15.90100861162440893 ) ) ;
#21318 = CARTESIAN_POINT ( 'NONE',  ( 182.2771148168560842, 275.8536480385645291, -16.43645293322504486 ) ) ;
#21319 = CARTESIAN_POINT ( 'NONE',  ( 165.3447893439585243, 247.5681563451806824, -5.571162280481247286 ) ) ;
#21320 = CARTESIAN_POINT ( 'NONE',  ( 40.70814378237798081, 60.14496435084704018, 10.00000000000000000 ) ) ;
#21321 = CARTESIAN_POINT ( 'NONE',  ( 202.3532268619428862, 267.6858343578610402, 0.8563957037533130867 ) ) ;
#21322 = CARTESIAN_POINT ( 'NONE',  ( 190.1693911629507738, 301.2639477917662703, -5.112716700269980485 ) ) ;
#21323 = CARTESIAN_POINT ( 'NONE',  ( 183.4588200504678355, 280.8776272736768647, 16.45139132406686144 ) ) ;
#21324 = EDGE_CURVE ( 'NONE', #70724, #90349, #4995, .T. ) ;
#21325 = CARTESIAN_POINT ( 'NONE',  ( 204.6713671561005299, 276.1457885614869951, -12.94307097876490431 ) ) ;
#21326 = CARTESIAN_POINT ( 'NONE',  ( 194.8104010662821111, 269.9905278424700441, 12.02357665573980405 ) ) ;
#21327 = CARTESIAN_POINT ( 'NONE',  ( 29.42770338693789967, 22.15404122711134960, 8.090169943749479842 ) ) ;
#21328 = CARTESIAN_POINT ( 'NONE',  ( -19.65312891409030271, 93.06504152958497400, 10.00000000000000888 ) ) ;
#21329 = DIRECTION ( 'NONE',  ( -0.08592509128337570690, 0.9963016002636669866, 0.000000000000000000 ) ) ;
#21330 = CARTESIAN_POINT ( 'NONE',  ( 68.99620552988632483, 69.28359185914359841, -6.825668283780611745 ) ) ;
#21331 = CARTESIAN_POINT ( 'NONE',  ( 159.9628729326222754, 253.5831720864507588, 15.75051413866357386 ) ) ;
#21332 = CARTESIAN_POINT ( 'NONE',  ( 161.2816932310574884, 251.2989083235077032, 13.15717084518158764 ) ) ;
#21333 = CARTESIAN_POINT ( 'NONE',  ( 147.1562325744354212, 255.7677522451418781, 10.00000000000009592 ) ) ;
#21334 = CARTESIAN_POINT ( 'NONE',  ( 172.2123999945063417, 283.8628369387304815, -12.71294468390556887 ) ) ;
#21335 = ORIENTED_EDGE ( 'NONE', *, *, #91502, .T. ) ;
#21336 = EDGE_CURVE ( 'NONE', #25811, #26754, #91335, .T. ) ;
#21337 = FACE_OUTER_BOUND ( 'NONE', #97961, .T. ) ;
#21338 = CARTESIAN_POINT ( 'NONE',  ( 73.01521690615598459, 70.40106399001336968, -8.092693171194275337 ) ) ;
#21339 = CARTESIAN_POINT ( 'NONE',  ( 150.9115585710837877, 269.2605084359132093, -15.80434701481532578 ) ) ;
#21340 = CARTESIAN_POINT ( 'NONE',  ( 6.400214715252306341, 168.3768266524160140, 9.188101187500096856 ) ) ;
#21341 = VECTOR ( 'NONE', #45531, 999.9999999999998863 ) ;
#21342 = CARTESIAN_POINT ( 'NONE',  ( 181.6561284561640832, 276.3695326334836295, -16.98996653829426862 ) ) ;
#21343 = CARTESIAN_POINT ( 'NONE',  ( 20.86070775165960001, 33.81751292744056769, -6.180339887498951690 ) ) ;
#21344 = CARTESIAN_POINT ( 'NONE',  ( 85.68464957279800842, 48.84619230832644377, 12.06853356899262941 ) ) ;
#21345 = LINE ( 'NONE', #6136, #62537 ) ;
#21346 = CARTESIAN_POINT ( 'NONE',  ( 71.85441816053061359, 72.14404838950795806, -3.648524940272755757 ) ) ;
#21347 = B_SPLINE_CURVE_WITH_KNOTS ( 'NONE', 3,
 ( #96105, #57546, #69384, #30887, #54160, #85121, #43341, #36736, #12474, #98575, #81897, #51447, #96607, #82415, #97105, #98068, #5360, #66158, #35252, #42831, #27674, #59022, #73271, #36240, #60029, #21078, #49963, #27169, #58540, #73766, #89515, #28644, #19587, #67146, #34748, #44337, #51954, #81401, #20073, #19084, #65650 ),
 .UNSPECIFIED., .F., .F.,
 ( 4, 2, 1, 1, 1, 2, 2, 1, 1, 2, 2, 1, 1, 2, 2, 1, 1, 2, 2, 1, 1, 1, 2, 2, 1, 1, 1, 4 ),
 ( 0.1734847945017928272, 0.1799419445447479615, 0.1863990945877031236, 0.1993133946736117823, 0.2251419948454298492, 0.2767991951890666491, 0.2897134952749769732, 0.3026277953608873528, 0.3284563955327087226, 0.3801135958763515732, 0.3930278959622621193, 0.4059421960481726099, 0.4317707962199937577, 0.4834279965636352205, 0.4963422966495451005, 0.5092565967354549805, 0.5350851969072738523, 0.5867423972509125951, 0.5996566973368238074, 0.6125709974227346866, 0.6383995975945537804, 0.6900567979381901917, 0.7933711986254616821, 0.8062854987113712291, 0.8191997987972807760, 0.8450283989690978714, 0.8966855993127316182, 1.000000000000000000 ),
 .UNSPECIFIED. ) ;
#21348 = CARTESIAN_POINT ( 'NONE',  ( 150.1387292596415648, 276.5099847689000967, 3.745717586651703179 ) ) ;
#21350 = CARTESIAN_POINT ( 'NONE',  ( 74.41009865654258704, 203.7677522451417929, -5.000000000000041744 ) ) ;
#21349 = CARTESIAN_POINT ( 'NONE',  ( 196.2467569046250162, 269.4493588965917183, -10.72705572559448761 ) ) ;
#21351 = CARTESIAN_POINT ( 'NONE',  ( 176.3344142305265905, 254.0447395692417842, -3.866504412443106276 ) ) ;
#21352 = EDGE_CURVE ( 'NONE', #84236, #60492, #27987, .T. ) ;
#21353 = CARTESIAN_POINT ( 'NONE',  ( 198.5799742811345823, 286.6963905097911152, 17.08859794237710261 ) ) ;
#21354 = EDGE_CURVE ( 'NONE', #62277, #32844, #96223, .T. ) ;
#21355 = CARTESIAN_POINT ( 'NONE',  ( 64.10800479423814124, 194.4865022471901739, 1.119607411625061291E-15 ) ) ;
#21356 = LINE ( 'NONE', #52241, #11892 ) ;
#21357 = CARTESIAN_POINT ( 'NONE',  ( 190.4750160083620472, 300.7345900314585947, -1.159659205620361400 ) ) ;
#21358 = CARTESIAN_POINT ( 'NONE',  ( 21.36630299834339652, 173.9548013555409796, -4.594050593750042211 ) ) ;
#21359 = CARTESIAN_POINT ( 'NONE',  ( 167.6841820197852257, 287.3320466105657260, 4.942676059668591471 ) ) ;
#21360 = CARTESIAN_POINT ( 'NONE',  ( 78.81389999504742150, 60.06372782575282798, 16.11061031492772955 ) ) ;
#21361 = CARTESIAN_POINT ( 'NONE',  ( 41.95273645663377238, 27.14754757982093381, -5.678558825948276656 ) ) ;
#21362 = CARTESIAN_POINT ( 'NONE',  ( 202.1695757186951994, 279.6930204168322689, -15.81993831395799077 ) ) ;
#21363 = DIRECTION ( 'NONE',  ( -0.8660254037844387076, -0.4999999999999998890, -0.000000000000000000 ) ) ;
#21364 = CARTESIAN_POINT ( 'NONE',  ( 185.1889932722985748, 266.7802408231123081, 13.62321108638839462 ) ) ;
#21365 = LINE ( 'NONE', #44635, #29887 ) ;
#21366 = FACE_OUTER_BOUND ( 'NONE', #85751, .T. ) ;
#21367 = CARTESIAN_POINT ( 'NONE',  ( 12.32504541118064978, 22.51421378149917985, -9.188101187500004485 ) ) ;
#21368 = CARTESIAN_POINT ( 'NONE',  ( 165.4973148452406804, 285.5633041981129736, -0.04349354715313477615 ) ) ;
#21369 = CYLINDRICAL_SURFACE ( 'NONE', #75888, 10.00000000000010658 ) ;
#21370 = CARTESIAN_POINT ( 'NONE',  ( 71.40044295081541748, 59.41588353585593296, 15.20283060994831104 ) ) ;
#21371 = CARTESIAN_POINT ( 'NONE',  ( 32.25894049256043417, 82.26293186637414578, 59.99999999999999289 ) ) ;
#21372 = ORIENTED_EDGE ( 'NONE', *, *, #62001, .T. ) ;
#21373 = CARTESIAN_POINT ( 'NONE',  ( 183.9962501225037101, 290.1813357568594824, 12.16961482813081474 ) ) ;
#21374 = CARTESIAN_POINT ( 'NONE',  ( 3.501222095392049205, 22.99752408145589300, 5.678558825948276656 ) ) ;
#21375 = CARTESIAN_POINT ( 'NONE',  ( 81.16104098974128078, 42.41662614947843934, 7.661191396672336396 ) ) ;
#21376 = CARTESIAN_POINT ( 'NONE',  ( 35.87562414229657293, 44.21091486745863364, 7.012934429366973338E-14 ) ) ;
#21377 = VERTEX_POINT ( 'NONE', #29772 ) ;
#21378 = CARTESIAN_POINT ( 'NONE',  ( 81.30818518503046732, 58.89441083166271085, 0.000000000000000000 ) ) ;
#21379 = PLANE ( 'NONE',  #27200 ) ;
#21380 = CARTESIAN_POINT ( 'NONE',  ( 76.51987890029035100, 63.61070592637643983, 14.91914813192731337 ) ) ;
#21381 = CARTESIAN_POINT ( 'NONE',  ( 155.6066474290145720, 261.1283759879266881, -18.16552045242181279 ) ) ;
#21382 = ORIENTED_EDGE ( 'NONE', *, *, #29384, .T. ) ;
#21383 = ORIENTED_EDGE ( 'NONE', *, *, #44773, .T. ) ;
#21384 = EDGE_CURVE ( 'NONE', #80413, #60766, #54045, .T. ) ;
#21386 = LINE ( 'NONE', #52273, #44259 ) ;
#21385 = DIRECTION ( 'NONE',  ( -0.000000000000000000, 0.000000000000000000, 1.000000000000000000 ) ) ;
#21387 = ORIENTED_EDGE ( 'NONE', *, *, #77658, .T. ) ;
#21388 = CARTESIAN_POINT ( 'NONE',  ( 88.19122672570537702, 43.84786592109882264, -2.112715317146043770 ) ) ;
#21389 = CARTESIAN_POINT ( 'NONE',  ( 31.74858474661088081, 18.73415679381823651, -6.890680421881970419E-14 ) ) ;
#21390 = CARTESIAN_POINT ( 'NONE',  ( 80.68870194293324971, 57.51412305112832968, 16.58365939551020318 ) ) ;
#21391 = CARTESIAN_POINT ( 'NONE',  ( 23.52134341065870160, 13.98415679381821342, 1.224646799147354045E-15 ) ) ;
#21392 = ORIENTED_EDGE ( 'NONE', *, *, #82260, .T. ) ;
#21393 = CARTESIAN_POINT ( 'NONE',  ( 87.64894667038031173, 45.18322468047552576, -6.184650709489425857 ) ) ;
#21394 = EDGE_CURVE ( 'NONE', #91070, #5196, #38857, .T. ) ;
#21395 = EDGE_CURVE ( 'NONE', #11048, #2437, #52203, .T. ) ;
#21396 = CARTESIAN_POINT ( 'NONE',  ( 43.68655075043449898, 184.4824982072973967, 3.021315404115420679E-15 ) ) ;
#21397 = ORIENTED_EDGE ( 'NONE', *, *, #64850, .T. ) ;
#21398 = CARTESIAN_POINT ( 'NONE',  ( 164.2572333502590709, 246.1451216570909253, 2.155809084027023204 ) ) ;
#21399 = EDGE_CURVE ( 'NONE', #14302, #43843, #14581, .T. ) ;
#21400 = CARTESIAN_POINT ( 'NONE',  ( -69.40242143070356917, 43.82067236826411971, 177.5919119679930134 ) ) ;
#21401 = ORIENTED_EDGE ( 'NONE', *, *, #34080, .T. ) ;
#21402 = CARTESIAN_POINT ( 'NONE',  ( 175.6393304058065610, 277.9438274558168018, -15.68642701745271495 ) ) ;
#21403 = CARTESIAN_POINT ( 'NONE',  ( 172.1807612816075448, 264.1729231858467983, -16.32128620121408957 ) ) ;
#21404 = ADVANCED_FACE ( 'NONE', ( #29286 ), #21966, .F. ) ;
#21405 = ORIENTED_EDGE ( 'NONE', *, *, #46818, .F. ) ;
#21406 = CARTESIAN_POINT ( 'NONE',  ( 158.6328712587097414, 275.0136024797188270, -12.55550228384817757 ) ) ;
#21407 = DIRECTION ( 'NONE',  ( 0.2113248654051647635, 0.7886751345948180836, -0.5773502691896270633 ) ) ;
#21408 = DIRECTION ( 'NONE',  ( -0.000000000000000000, -1.000000000000000000, -0.000000000000000000 ) ) ;
#21409 = VERTEX_POINT ( 'NONE', #69763 ) ;
#21410 = ORIENTED_EDGE ( 'NONE', *, *, #76368, .T. ) ;
#21411 = CARTESIAN_POINT ( 'NONE',  ( 73.58067652191090247, 69.78534542737938295, 9.362363942011365125 ) ) ;
#21412 = CARTESIAN_POINT ( 'NONE',  ( 147.5693121967435957, 275.0494489676833041, 4.210973343677100189 ) ) ;
#21413 = CARTESIAN_POINT ( 'NONE',  ( 82.66218641157266234, 53.85062555766314318, 15.82228755104996765 ) ) ;
#21414 = CARTESIAN_POINT ( 'NONE',  ( 10.49025449741314375, 29.55466486950698624, -1.111400068045478839E-16 ) ) ;
#21415 = CARTESIAN_POINT ( 'NONE',  ( 153.4477557824949940, 264.8676860077344486, 17.16010094972647693 ) ) ;
#21416 = CARTESIAN_POINT ( 'NONE',  ( 147.0160867267995854, 276.0076635896675725, 0.7715638482002742382 ) ) ;
#21417 = CARTESIAN_POINT ( 'NONE',  ( 191.8232488616404225, 298.3993822291468518, -9.342381338555176384 ) ) ;
#21418 = ORIENTED_EDGE ( 'NONE', *, *, #78036, .F. ) ;
#21419 = CARTESIAN_POINT ( 'NONE',  ( 73.16723296629628237, 58.29704776030416014, -15.75092464132356262 ) ) ;
#21420 = CARTESIAN_POINT ( 'NONE',  ( 39.65533143765975410, 23.86426979415092475, -3.090169943749474069 ) ) ;
#21421 = AXIS2_PLACEMENT_3D ( 'NONE', #51780, #82720, #67459 ) ;
#21422 = CARTESIAN_POINT ( 'NONE',  ( -62.10935938174410609, 33.76704452855005201, -10.00000000000000000 ) ) ;
#21423 = PLANE ( 'NONE',  #75786 ) ;
#21424 = CARTESIAN_POINT ( 'NONE',  ( 167.1547084800286882, 256.3859753943238502, -15.10362562340490911 ) ) ;
#21425 = VERTEX_POINT ( 'NONE', #44963 ) ;
#21426 = CARTESIAN_POINT ( 'NONE',  ( 149.0943192338760070, 272.4080592974699471, -12.87526400066115606 ) ) ;
#21427 = CARTESIAN_POINT ( 'NONE',  ( 75.54132550460440143, 54.37554586383003397, -16.11515908931868779 ) ) ;
#21428 = CARTESIAN_POINT ( 'NONE',  ( 148.7903119393423026, 273.3731287249261186, 9.064500856912474092 ) ) ;
#21429 = CARTESIAN_POINT ( 'NONE',  ( 79.11618919729676236, 45.91829409069699608, 13.15082663536679242 ) ) ;
#21430 = CARTESIAN_POINT ( 'NONE',  ( 182.8912941787172315, 284.3928553195365794, -14.99677252371531289 ) ) ;
#21431 = CARTESIAN_POINT ( 'NONE',  ( 0.005075371086064872639, 27.18819441265828019, -10.00000000000000000 ) ) ;
#21432 = ORIENTED_EDGE ( 'NONE', *, *, #64048, .F. ) ;
#21433 = CARTESIAN_POINT ( 'NONE',  ( 170.5605287177041305, 255.6265081261690568, -11.70025675400036747 ) ) ;
#21434 = PLANE ( 'NONE',  #74343 ) ;
#21436 = EDGE_CURVE ( 'NONE', #705, #37573, #83660, .T. ) ;
#21435 = CARTESIAN_POINT ( 'NONE',  ( 164.7694554770609159, 245.2579269087094076, -3.003635650077957742 ) ) ;
#21437 = CARTESIAN_POINT ( 'NONE',  ( 36.66582480827072743, 198.6427522451419350, -10.00000000000009415 ) ) ;
#21438 = CARTESIAN_POINT ( 'NONE',  ( 109.7816501962546454, 240.3149278399160949, 9.188101187500093303 ) ) ;
#21439 = CARTESIAN_POINT ( 'NONE',  ( 177.5665759502285539, 275.7863988818428993, 17.69313789786682989 ) ) ;
#21440 = VECTOR ( 'NONE', #8830, 1000.000000000000114 ) ;
#21441 = DIRECTION ( 'NONE',  ( -0.5000000000000003331, 0.8660254037844383745, -5.669937756276021476E-31 ) ) ;
#21442 = CARTESIAN_POINT ( 'NONE',  ( 195.9713281756800427, 291.2146981034049418, 17.52210387885178022 ) ) ;
#21443 = CARTESIAN_POINT ( 'NONE',  ( 172.4017459954111473, 250.5914637853330476, -4.115793628843052332 ) ) ;
#21444 = CARTESIAN_POINT ( 'NONE',  ( 39.90439897628026955, 193.8458772461660544, 9.188101187500095079 ) ) ;
#21445 = CARTESIAN_POINT ( 'NONE',  ( 147.6215775367315644, 275.3445823649863087, -3.142877717583205222 ) ) ;
#21446 = ORIENTED_EDGE ( 'NONE', *, *, #69625, .T. ) ;
#21447 = DIRECTION ( 'NONE',  ( 0.000000000000000000, 0.000000000000000000, 1.000000000000000000 ) ) ;
#21448 = CARTESIAN_POINT ( 'NONE',  ( 179.5196496019146650, 266.1175816663657656, 16.29367087753972498 ) ) ;
#21449 = CARTESIAN_POINT ( 'NONE',  ( 30.58014428988347788, 176.9155109091896634, 2.679491924311254714 ) ) ;
#21450 = CARTESIAN_POINT ( 'NONE',  ( 147.5492216329511166, 275.0842468449245644, 4.751613690710122739 ) ) ;
#21451 = CARTESIAN_POINT ( 'NONE',  ( 81.92950609163860065, 41.13482008182690208, -5.440008311034252309 ) ) ;
#21452 = CARTESIAN_POINT ( 'NONE',  ( 166.6288018012914449, 255.3266329142646498, -14.67773939159194896 ) ) ;
#21453 = CARTESIAN_POINT ( 'NONE',  ( 176.3126652553115150, 285.5045246447724594, -12.04976978329188242 ) ) ;
#21454 = CARTESIAN_POINT ( 'NONE',  ( 164.2885300478071144, 250.0642274256680366, 10.21650006632281205 ) ) ;
#21455 = CARTESIAN_POINT ( 'NONE',  ( 87.40047971330913867, 221.2677522451418497, 10.00000000000009592 ) ) ;
#21456 = ORIENTED_EDGE ( 'NONE', *, *, #50443, .T. ) ;
#21457 = CARTESIAN_POINT ( 'NONE',  ( 195.3926592889443157, 266.7123800746668962, -7.757725527663858145 ) ) ;
#21458 = EDGE_CURVE ( 'NONE', #77337, #6621, #96948, .T. ) ;
#21459 = CARTESIAN_POINT ( 'NONE',  ( 158.7932562801271104, 282.3814901877906891, -1.645599008796116314 ) ) ;
#21460 = CARTESIAN_POINT ( 'NONE',  ( -25.62627769214124740, 24.57763045674671432, -10.00000000000000000 ) ) ;
#21461 = CARTESIAN_POINT ( 'NONE',  ( 19.09298631340924501, 172.6423013555409796, -4.594050593750043987 ) ) ;
#21462 = CARTESIAN_POINT ( 'NONE',  ( 3.297978757390601423, 24.83705186507751606, 3.090169943749475401 ) ) ;
#21463 = CARTESIAN_POINT ( 'NONE',  ( -17.14183914111196927, 105.0694402252967024, 44.45399967932692675 ) ) ;
#21464 = CARTESIAN_POINT ( 'NONE',  ( 71.68777414727941277, 59.55670923871284828, -15.71026032022712293 ) ) ;
#21465 = CARTESIAN_POINT ( 'NONE',  ( 73.15617415350918407, 69.83382733437846923, 9.602067989434942774 ) ) ;
#21467 = CARTESIAN_POINT ( 'NONE',  ( 63.26028190641562787, 198.1423013555410080, -4.594050593750043987 ) ) ;
#21466 = CARTESIAN_POINT ( 'NONE',  ( 194.7211787970855141, 275.0175511178182433, -15.89236621824491635 ) ) ;
#21468 = CARTESIAN_POINT ( 'NONE',  ( 163.9910908123517288, 246.6060940548019289, -7.333295033952830444 ) ) ;
#21469 = CARTESIAN_POINT ( 'NONE',  ( 72.94218364219292994, 57.09986443339001028, 16.39775231352756180 ) ) ;
#21470 = EDGE_CURVE ( 'NONE', #77729, #15709, #38913, .T. ) ;
#21471 = CARTESIAN_POINT ( 'NONE',  ( 68.79257260696145693, 67.61008945445695417, 8.397044590744407344 ) ) ;
#21472 = CARTESIAN_POINT ( 'NONE',  ( 164.9779129355220562, 244.8968679994381148, -1.771286574179712803 ) ) ;
#21473 = ORIENTED_EDGE ( 'NONE', *, *, #25618, .F. ) ;
#21474 = ADVANCED_FACE ( 'NONE', ( #6482 ), #37360, .T. ) ;
#21475 =( BOUNDED_CURVE ( )  B_SPLINE_CURVE ( 2, ( #52085, #50584, #89646, #65784, #59672, #11617, #20705, #75406, #27305 ),
 .UNSPECIFIED., .F., .T. ) 
 B_SPLINE_CURVE_WITH_KNOTS ( ( 3, 2, 2, 2, 3 ),
 ( 0.8669354838709677491, 0.8682795698924731242, 0.8709677419354838745, 0.8736559139784946248, 0.8750000000000000000 ),
 .UNSPECIFIED. ) 
 CURVE ( )  GEOMETRIC_REPRESENTATION_ITEM ( )  RATIONAL_B_SPLINE_CURVE ( ( 0.9330127018922194093, 0.9330127018922194093, 1.000000000000000000, 0.8660254037844387076, 1.000000000000000000, 0.8660254037844387076, 1.000000000000000000, 0.9330127018922194093, 0.9330127018922194093 ) ) 
 REPRESENTATION_ITEM ( '' )  );
#21476 = CARTESIAN_POINT ( 'NONE',  ( 14.88889434582242544, 192.7365022471903444, 2.944929066748280225E-16 ) ) ;
#21477 = CARTESIAN_POINT ( 'NONE',  ( 208.2939409893161553, 269.8713066281881083, 2.523744790997269227 ) ) ;
#21478 = CARTESIAN_POINT ( 'NONE',  ( 134.8967340017684080, 242.5643266524159856, -9.188101187500093303 ) ) ;
#21479 = CARTESIAN_POINT ( 'NONE',  ( 23.73493010604062192, 29.10171378149919974, 9.188101187500008038 ) ) ;
#21480 = CARTESIAN_POINT ( 'NONE',  ( 206.8583977782397483, 272.3577404062329492, -8.036528591665119237 ) ) ;
#21481 = CARTESIAN_POINT ( 'NONE',  ( 202.4560076411394220, 279.0611292670678267, 15.58065739802832717 ) ) ;
#21482 = CARTESIAN_POINT ( 'NONE',  ( 194.4090165346928529, 280.7843443599479656, -17.71307557792658116 ) ) ;
#21484 = CARTESIAN_POINT ( 'NONE',  ( 74.84209865657220462, 67.13651163270155564, 12.97079428878455332 ) ) ;
#21483 = CARTESIAN_POINT ( 'NONE',  ( 88.16334560026523093, 43.89615744693332999, 2.509484348711651602 ) ) ;
#21485 = CARTESIAN_POINT ( 'NONE',  ( 69.01345705981862011, 64.44777229250053097, 12.47991269069003906 ) ) ;
#21486 = ORIENTED_EDGE ( 'NONE', *, *, #8669, .T. ) ;
#21487 = CARTESIAN_POINT ( 'NONE',  ( 166.1047324428320167, 246.6357536469371610, 3.930903826211260998 ) ) ;
#21488 = CARTESIAN_POINT ( 'NONE',  ( 164.1057330408499411, 246.4075278903502237, 7.856393496352101380 ) ) ;
#21489 = CARTESIAN_POINT ( 'NONE',  ( 73.55377261143068779, 66.54097169440498760, -12.86805831085992047 ) ) ;
#21490 = VECTOR ( 'NONE', #40767, 1000.000000000000000 ) ;
#21491 = CARTESIAN_POINT ( 'NONE',  ( 169.9474419461124626, 266.2972067178577049, -16.74373953161226325 ) ) ;
#21492 = CARTESIAN_POINT ( 'NONE',  ( 195.2321946600270337, 271.9407588785367125, -13.42877009059527538 ) ) ;
#21493 = ORIENTED_EDGE ( 'NONE', *, *, #9487, .F. ) ;
#21494 = CARTESIAN_POINT ( 'NONE',  ( 69.76251527479838899, 68.37414511987412880, 8.108736765182461781 ) ) ;
#21495 = VECTOR ( 'NONE', #23841, 1000.000000000000000 ) ;
#21496 = B_SPLINE_CURVE_WITH_KNOTS ( 'NONE', 3,
 ( #71492, #94807, #36450, #67353 ),
 .UNSPECIFIED., .F., .F.,
 ( 4, 4 ),
 ( 0.01205011342145419564, 0.02055108600438866617 ),
 .UNSPECIFIED. ) ;
#21497 = CARTESIAN_POINT ( 'NONE',  ( 6.965316927136144365, 15.97253583063839066, -9.188101187500006262 ) ) ;
#21498 = AXIS2_PLACEMENT_3D ( 'NONE', #68330, #99255, #7033 ) ;
#21499 = B_SPLINE_SURFACE_WITH_KNOTS ( 'NONE', 3, 1, ( 
 ( #74330, #28699 ),
 ( #5407, #59576 ),
 ( #75318, #98114 ),
 ( #13999, #91037 ),
 ( #82941, #67697 ),
 ( #6403, #22590 ),
 ( #51494, #37287 ),
 ( #13025, #68182 ),
 ( #68679, #29694 ),
 ( #60075, #92046 ),
 ( #99111, #21605 ),
 ( #43888, #91527 ),
 ( #22090, #76313 ),
 ( #37777, #99611 ),
 ( #30188, #61074 ),
 ( #81938, #12516 ),
 ( #43388, #24083 ),
 ( #23072, #45863 ),
 ( #15986, #24580 ),
 ( #55463, #78303 ),
 ( #92526, #46885 ),
 ( #62563, #1799 ),
 ( #53966, #84923 ),
 ( #31667, #85437 ),
 ( #69682, #15469 ),
 ( #77810, #31174 ),
 ( #69181, #70173 ),
 ( #16484, #93526 ),
 ( #78803, #62064 ),
 ( #286, #47379 ),
 ( #8393, #85958 ),
 ( #9391, #46364 ),
 ( #93013, #23568 ),
 ( #54459, #77293 ) ),
 .UNSPECIFIED., .T., .F., .F.,
 ( 4, 2, 2, 2, 2, 2, 2, 2, 2, 2, 2, 2, 2, 2, 2, 2, 4 ),
 ( 2, 2 ),
 ( 0.000000000000000000, 0.06250000000000000000, 0.1250000000000000000, 0.1875000000000000000, 0.2500000000000000000, 0.3125000000000000000, 0.3750000000000000000, 0.4375000000000000000, 0.5000000000000000000, 0.5625000000000000000, 0.6250000000000000000, 0.6875000000000000000, 0.7500000000000000000, 0.8125000000000000000, 0.8750000000000000000, 0.9375000000000000000, 1.000000000000000000 ),
 ( 0.000000000000000000, 1.000000000000000000 ),
 .UNSPECIFIED. ) ;
#21500 = B_SPLINE_CURVE_WITH_KNOTS ( 'NONE', 3,
 ( #71792, #31261, #95121, #1882, #87038, #56566, #23651, #8474, #93094, #64173, #46970, #39345, #56046, #868, #70770, #24664, #63669, #25686, #18085, #31747, #24173, #16068, #48981, #69765, #62652, #54542, #9481, #55056, #85525, #86039, #16567, #40352, #47463, #78388, #39839, #32265, #63168, #94112, #86532, #17062, #28164, #35266, #19097, #20580, #57058, #50957, #72298, #73779, #66662, #11985, #20086, #49975, #3398, #42841, #58069, #4368 ),
 .UNSPECIFIED., .F., .F.,
 ( 4, 2, 2, 2, 2, 2, 2, 2, 2, 2, 2, 2, 2, 2, 2, 2, 2, 2, 2, 2, 2, 2, 2, 2, 2, 2, 2, 4 ),
 ( 0.001001512342791581987, 0.001483580493562128202, 0.001965648644332674416, 0.002206682719717947307, 0.002447716795103221064, 0.002568233832795857510, 0.002688750870488493955, 0.002809267908181130400, 0.002929784945873766845, 0.003170819021259039736, 0.003411853096644312192, 0.003893921247414742614, 0.004858057548955562258, 0.005822193850496381468, 0.006304262001266755511, 0.006545296076651900032, 0.006786330152037044552, 0.006846588670883270618, 0.006906847189729496683, 0.006967105708575722749, 0.007027364227421947947, 0.007147881265114443446, 0.007268398302806938945, 0.007509432378191927340, 0.007750466453576916603, 0.007991500528961904132, 0.008232534604346893395, 0.008714602755116832022 ),
 .UNSPECIFIED. ) ;
#21501 = CARTESIAN_POINT ( 'NONE',  ( -11.23413608767112670, 23.57316747377393540, 177.5919119679930134 ) ) ;
#21502 = CARTESIAN_POINT ( 'NONE',  ( 70.48286763772495078, 52.64441083166268243, 0.000000000000000000 ) ) ;
#21503 = CARTESIAN_POINT ( 'NONE',  ( 182.1922674602477628, 295.0151143605804691, 4.768981532823296732 ) ) ;
#21504 = CARTESIAN_POINT ( 'NONE',  ( 163.4178923001155681, 247.5989030008181260, -10.38047187240561442 ) ) ;
#21505 = CARTESIAN_POINT ( 'NONE',  ( -77.42978507651396569, 55.80833764325424085, -10.00000000000000000 ) ) ;
#21506 = EDGE_CURVE ( 'NONE', #87819, #78948, #34899, .T. ) ;
#21507 = CARTESIAN_POINT ( 'NONE',  ( -48.36978223816942801, 29.22654356899180428, 177.5919119679930134 ) ) ;
#21508 = CARTESIAN_POINT ( 'NONE',  ( 16.41743859968233110, 9.288480858562301989, 1.475505719884397138E-15 ) ) ;
#21509 = CARTESIAN_POINT ( 'NONE',  ( 84.37825102736907468, 49.99960613749294680, 13.80049582259581520 ) ) ;
#21510 = EDGE_LOOP ( 'NONE', ( #87645, #15656, #78158, #54352, #79247, #90492, #97311, #11443, #66606, #63395, #78640, #20329, #14404, #5096, #41205, #60846, #2217, #3402, #19699, #24105, #77317, #16679, #54545, #17161, #65989, #28052, #13084, #92255, #8081, #47041, #38786, #13408, #92325, #24559, #68367, #19902, #65161, #73630, #8559, #24387, #5238, #22982, #94922, #34764, #23478, #51668, #36876, #72994, #63277, #5264, #32528 ) ) ;
#21511 = CARTESIAN_POINT ( 'NONE',  ( 48.72058909919672942, 76.89514952714607432, 10.00000000000000000 ) ) ;
#21512 = CARTESIAN_POINT ( 'NONE',  ( 13.67211979723576931, 32.92651376809308772, 10.00000000000000000 ) ) ;
#21513 = CARTESIAN_POINT ( 'NONE',  ( 79.67773314991492839, 45.75892492389007771, -12.20866718477218704 ) ) ;
#21514 = ORIENTED_EDGE ( 'NONE', *, *, #79736, .T. ) ;
#21515 = CARTESIAN_POINT ( 'NONE',  ( 191.5324528500417216, 298.9030556958743432, -8.286652526617016790 ) ) ;
#21516 = FACE_OUTER_BOUND ( 'NONE', #12526, .T. ) ;
#21517 = VECTOR ( 'NONE', #98007, 1000.000000000000227 ) ;
#21518 = CARTESIAN_POINT ( 'NONE',  ( 204.9103773355753617, 275.7318107871104189, 13.62808820451859937 ) ) ;
#21519 = CARTESIAN_POINT ( 'NONE',  ( 88.09383187283991390, 43.67022580382143815, 1.148899272762605506 ) ) ;
#21520 = CARTESIAN_POINT ( 'NONE',  ( 194.3413770922408617, 282.8930799310762723, 17.82077676852630077 ) ) ;
#21521 = ORIENTED_EDGE ( 'NONE', *, *, #50546, .F. ) ;
#21522 = CARTESIAN_POINT ( 'NONE',  ( 95.05956542768423390, 219.5643266524160140, 9.188101187500095079 ) ) ;
#21523 = CARTESIAN_POINT ( 'NONE',  ( 155.1614028326249866, 261.8995622506689074, 18.45604204116099822 ) ) ;
#21524 = CARTESIAN_POINT ( 'NONE',  ( 181.2000081644680733, 271.5771930539713708, -17.25712798740391563 ) ) ;
#21525 = CARTESIAN_POINT ( 'NONE',  ( 81.55438844336480031, 42.25231255016616672, -8.032075583313584843 ) ) ;
#21526 = B_SPLINE_SURFACE_WITH_KNOTS ( 'NONE', 3, 1, ( 
 ( #51850, #67030 ),
 ( #21442, #43226 ),
 ( #68528, #75646 ),
 ( #4760, #35642 ),
 ( #82299, #98460 ),
 ( #83269, #13837 ),
 ( #29539, #14337 ),
 ( #37127, #66543 ),
 ( #58432, #68034 ),
 ( #52820, #89883 ),
 ( #20457, #12869 ),
 ( #83776, #30027 ),
 ( #46723, #31020 ),
 ( #32015, #84279 ),
 ( #70017, #93363 ),
 ( #61912, #77651 ),
 ( #84770, #137 ),
 ( #15306, #70522 ),
 ( #632, #30532 ),
 ( #71050, #38105 ),
 ( #85798, #78648 ),
 ( #69018, #22919 ),
 ( #14824, #60911 ),
 ( #92860, #7729 ),
 ( #99948, #91878 ),
 ( #62924, #46205 ),
 ( #40111, #45713 ),
 ( #31512, #55307 ),
 ( #93875, #76636 ),
 ( #38617, #8237 ),
 ( #69526, #62407 ),
 ( #85272, #77122 ),
 ( #86289, #23920 ),
 ( #61419, #22431 ) ),
 .UNSPECIFIED., .T., .F., .F.,
 ( 4, 2, 2, 2, 2, 2, 2, 2, 2, 2, 2, 2, 2, 2, 2, 2, 4 ),
 ( 2, 2 ),
 ( 0.000000000000000000, 0.06250000000000000000, 0.1250000000000000000, 0.1875000000000000000, 0.2500000000000000000, 0.3125000000000000000, 0.3750000000000000000, 0.4375000000000000000, 0.5000000000000000000, 0.5625000000000000000, 0.6250000000000000000, 0.6875000000000000000, 0.7500000000000000000, 0.8125000000000000000, 0.8750000000000000000, 0.9375000000000000000, 1.000000000000000000 ),
 ( 0.000000000000000000, 1.000000000000000000 ),
 .UNSPECIFIED. ) ;
#21527 = VERTEX_POINT ( 'NONE', #33268 ) ;
#21528 = EDGE_CURVE ( 'NONE', #82304, #92124, #63165, .T. ) ;
#21529 = EDGE_LOOP ( 'NONE', ( #20636, #26507, #62655, #3294 ) ) ;
#21530 = ORIENTED_EDGE ( 'NONE', *, *, #3885, .T. ) ;
#21531 = CARTESIAN_POINT ( 'NONE',  ( 81.54502813046227061, 50.64722393506180254, 14.48977360135641135 ) ) ;
#21532 = ORIENTED_EDGE ( 'NONE', *, *, #49682, .T. ) ;
#21533 = CARTESIAN_POINT ( 'NONE',  ( 158.6496056213609904, 257.8578177934796258, 17.38082990300775776 ) ) ;
#21534 = VERTEX_POINT ( 'NONE', #8472 ) ;
#21535 = CARTESIAN_POINT ( 'NONE',  ( 164.4989919961878684, 245.7263833991736988, 2.405231973350729024 ) ) ;
#21536 = CARTESIAN_POINT ( 'NONE',  ( 82.61071101779671721, 40.83617390237688483, 3.229293852844629331 ) ) ;
#21537 = FACE_OUTER_BOUND ( 'NONE', #59865, .T. ) ;
#21538 = CARTESIAN_POINT ( 'NONE',  ( -23.42324326788986610, 99.77638747395597818, 45.19939615752831230 ) ) ;
#21539 = CARTESIAN_POINT ( 'NONE',  ( 68.35468836908422929, 68.36852720251083326, -6.749963640543104049 ) ) ;
#21540 = CARTESIAN_POINT ( 'NONE',  ( 165.0694571955912409, 264.4563124879717293, -17.70034357220088950 ) ) ;
#21541 = ORIENTED_EDGE ( 'NONE', *, *, #89686, .T. ) ;
#21542 = CARTESIAN_POINT ( 'NONE',  ( 192.0969986600162827, 271.0201763999182845, -15.22553433325905736 ) ) ;
#21543 = CARTESIAN_POINT ( 'NONE',  ( 14.05709621874952475, 23.51421378149918340, -9.188101187500004485 ) ) ;
#21544 = EDGE_CURVE ( 'NONE', #47670, #82380, #39343, .T. ) ;
#21545 = ORIENTED_EDGE ( 'NONE', *, *, #90760, .F. ) ;
#21546 = CARTESIAN_POINT ( 'NONE',  ( 164.2602539243905539, 281.6793576088280133, 8.832505592777787129 ) ) ;
#21548 = ORIENTED_EDGE ( 'NONE', *, *, #23427, .T. ) ;
#21547 = CARTESIAN_POINT ( 'NONE',  ( 9.004826742577897392, 187.5530062829863027, -4.648177544792955347E-16 ) ) ;
#21549 = CARTESIAN_POINT ( 'NONE',  ( 163.1014434023538513, 248.1470085697407058, 9.692260209037655727 ) ) ;
#21550 = CARTESIAN_POINT ( 'NONE',  ( 185.1754690811580701, 257.9748643125362264, 3.025625122693937463 ) ) ;
#21551 = CARTESIAN_POINT ( 'NONE',  ( 160.8824536440269526, 282.3397334439140423, -6.171673602401500425 ) ) ;
#21552 = CARTESIAN_POINT ( 'NONE',  ( 40.40883878445526278, 23.73415679381825782, -6.890680421881970419E-14 ) ) ;
#21553 = CARTESIAN_POINT ( 'NONE',  ( 158.5586670023323563, 257.8002292186573072, 17.26955892278689220 ) ) ;
#21554 = EDGE_CURVE ( 'NONE', #36835, #50903, #86530, .T. ) ;
#21555 = CARTESIAN_POINT ( 'NONE',  ( 200.3134965941964651, 283.6938417875134064, 18.29802468362849766 ) ) ;
#21556 = CARTESIAN_POINT ( 'NONE',  ( 194.7554030189934622, 263.4159149995173266, -0.7846879789437617436 ) ) ;
#21557 = VERTEX_POINT ( 'NONE', #55546 ) ;
#21558 = CARTESIAN_POINT ( 'NONE',  ( 93.48865797453373716, 236.3297689869269220, -2.679491924311252493 ) ) ;
#21559 = CARTESIAN_POINT ( 'NONE',  ( 73.60577444524625434, 62.71670610283283764, -14.51900996758597984 ) ) ;
#21561 = ADVANCED_FACE ( 'NONE', ( #8967 ), #866, .T. ) ;
#21560 = CARTESIAN_POINT ( 'NONE',  ( 9.692741923115875124, 169.7365022471902023, -10.00000000000009237 ) ) ;
#21562 = CARTESIAN_POINT ( 'NONE',  ( 12.56145106960391011, 171.3927522451418213, 10.00000000000009592 ) ) ;
#21563 = CARTESIAN_POINT ( 'NONE',  ( -71.07364842061382149, 47.42355933771584375, 10.00000000000000000 ) ) ;
#21564 = CARTESIAN_POINT ( 'NONE',  ( 174.9738539119461223, 281.6573486160436346, -14.08158005805571023 ) ) ;
#21565 = CARTESIAN_POINT ( 'NONE',  ( 203.4569662549483837, 278.2491926230401305, -15.13189527399345913 ) ) ;
#21566 = CARTESIAN_POINT ( 'NONE',  ( 84.67899269911676186, 44.63087609091873986, -8.050483238754811310 ) ) ;
#21567 = CARTESIAN_POINT ( 'NONE',  ( 164.8513470711439197, 274.0536041136784888, 15.36431698690459058 ) ) ;
#21569 = CARTESIAN_POINT ( 'NONE',  ( 28.91364825607195144, 28.64441083166262203, -10.00000000000000533 ) ) ;
#21568 = CARTESIAN_POINT ( 'NONE',  ( -0.3657822996961275219, 170.5958772461660544, -9.188101187500095079 ) ) ;
#21570 = CARTESIAN_POINT ( 'NONE',  ( 163.5322132292002095, 248.5708327738595926, 9.747496234835503870 ) ) ;
#21571 = ORIENTED_EDGE ( 'NONE', *, *, #56679, .T. ) ;
#21572 = ORIENTED_EDGE ( 'NONE', *, *, #18709, .T. ) ;
#21573 = CARTESIAN_POINT ( 'NONE',  ( 0.005075371086064872639, 27.18819441265827308, -10.00000000000000000 ) ) ;
#21574 = CARTESIAN_POINT ( 'NONE',  ( 195.6664450926536460, 278.3245960621525796, 17.18455885460583232 ) ) ;
#21575 = CARTESIAN_POINT ( 'NONE',  ( 171.9934119896647644, 289.4116381468080021, 2.632332000678004658 ) ) ;
#21576 = CARTESIAN_POINT ( 'NONE',  ( 84.75464104472338533, 42.20820103110227706, 0.3493146913119697938 ) ) ;
#21577 = CARTESIAN_POINT ( 'NONE',  ( 201.9489429292733291, 280.8611656421081193, -16.76649152307749091 ) ) ;
#21578 = CARTESIAN_POINT ( 'NONE',  ( 84.60705283987604730, 47.25696623766521753, 11.22058669928208552 ) ) ;
#21579 = CARTESIAN_POINT ( 'NONE',  ( 153.3817192398776683, 279.2928347461563590, 3.875170408332509808 ) ) ;
#21580 = CARTESIAN_POINT ( 'NONE',  ( 22.80074434730262567, 171.7202760586659736, -5.415160957724236172E-17 ) ) ;
#21581 = CARTESIAN_POINT ( 'NONE',  ( 119.1457234225564008, 239.5958772461660544, -9.188101187500095079 ) ) ;
#21582 = DIRECTION ( 'NONE',  ( 0.000000000000000000, 0.000000000000000000, -1.000000000000000000 ) ) ;
#21583 = LINE ( 'NONE', #82922, #59275 ) ;
#21584 = CARTESIAN_POINT ( 'NONE',  ( 78.68333733368046978, 54.46560497474366258, 15.97876508924327510 ) ) ;
#21585 = VECTOR ( 'NONE', #72117, 1000.000000000000227 ) ;
#21586 = B_SPLINE_CURVE_WITH_KNOTS ( 'NONE', 3,
 ( #22944, #70547, #78167, #9776, #40638, #87828, #33050, #32037, #62949, #33562 ),
 .UNSPECIFIED., .F., .F.,
 ( 4, 2, 2, 2, 4 ),
 ( 8.673617379884035472E-19, 0.0002622400424272934051, 0.0005244800848545859429, 0.0007867201272818784806, 0.001048960169709171018 ),
 .UNSPECIFIED. ) ;
#21587 = CARTESIAN_POINT ( 'NONE',  ( 176.9878821292914211, 283.3466992399841615, -15.40003107629192769 ) ) ;
#21588 = CARTESIAN_POINT ( 'NONE',  ( 82.39043419086114284, 52.72955616827477598, -15.12536216578337012 ) ) ;
#21589 = FACE_OUTER_BOUND ( 'NONE', #85651, .T. ) ;
#21590 = CARTESIAN_POINT ( 'NONE',  ( 184.0471386986133098, 274.9938889884007267, 16.36334711905761097 ) ) ;
#21591 = DIRECTION ( 'NONE',  ( -0.6857383512133925496, -0.7278481391575704063, 0.000000000000000000 ) ) ;
#21592 = CARTESIAN_POINT ( 'NONE',  ( -19.67882664948312765, 93.20451685012037046, 59.99999999999999289 ) ) ;
#21593 = CARTESIAN_POINT ( 'NONE',  ( 84.78687102586546587, 50.23207448519301721, 13.79854428445948678 ) ) ;
#21594 = CARTESIAN_POINT ( 'NONE',  ( 192.9213923665448931, 265.3941825485875370, 7.787462690985773150 ) ) ;
#21595 = EDGE_CURVE ( 'NONE', #76681, #60766, #93092, .T. ) ;
#21596 = CARTESIAN_POINT ( 'NONE',  ( 55.08690683815022027, 192.6115022471902023, -5.000000000000041744 ) ) ;
#21597 = CARTESIAN_POINT ( 'NONE',  ( 182.3156994963505042, 267.7668330571380011, -14.83048941619937011 ) ) ;
#21598 = FACE_OUTER_BOUND ( 'NONE', #65479, .T. ) ;
#21599 = ADVANCED_FACE ( 'NONE', ( #62649 ), #23761, .F. ) ;
#21601 = EDGE_CURVE ( 'NONE', #57534, #34490, #9023, .T. ) ;
#21600 = CARTESIAN_POINT ( 'NONE',  ( 185.1025075027767457, 269.5733332805129976, 15.84353680425453703 ) ) ;
#21602 = EDGE_CURVE ( 'NONE', #30966, #19346, #51458, .T. ) ;
#21603 = CARTESIAN_POINT ( 'NONE',  ( 103.7198194655286017, 224.5643266524159856, -9.188101187500093303 ) ) ;
#21604 = CARTESIAN_POINT ( 'NONE',  ( 161.8408514536557163, 250.3304178724980318, -14.12919723462510646 ) ) ;
#21605 = CARTESIAN_POINT ( 'NONE',  ( 151.0715479399129606, 268.9833987204304435, 14.24612252017116987 ) ) ;
#21606 = CARTESIAN_POINT ( 'NONE',  ( -31.60385337846877718, 62.05373366572042926, -10.00000000000000000 ) ) ;
#21608 = CARTESIAN_POINT ( 'NONE',  ( 200.4562370433687875, 283.4466080772515966, 17.70760574868393533 ) ) ;
#21607 = CARTESIAN_POINT ( 'NONE',  ( 196.2255671652529259, 290.7743432561995860, 16.01325193769018185 ) ) ;
#21609 = CARTESIAN_POINT ( 'NONE',  ( 201.4059013154023603, 270.3081817402440947, -10.22446195156602400 ) ) ;
#21610 = LINE ( 'NONE', #39268, #92430 ) ;
#21611 = DIRECTION ( 'NONE',  ( 0.1887253692075822886, -0.9820299053580098247, 0.000000000000000000 ) ) ;
#21612 = CARTESIAN_POINT ( 'NONE',  ( 42.32740281844729680, 26.29860640527295601, -2.839279412974138328 ) ) ;
#21613 = CARTESIAN_POINT ( 'NONE',  ( 192.8607783413999073, 296.6023284558532396, -11.80574095728561446 ) ) ;
#21614 = FACE_BOUND ( 'NONE', #40100, .T. ) ;
#21615 = EDGE_LOOP ( 'NONE', ( #27858, #70387, #9826, #71355, #88499, #20548, #88494, #35459, #44301, #10616, #18047 ) ) ;
#21616 = CARTESIAN_POINT ( 'NONE',  ( 23.04210978301307122, 28.70171378149919406, -9.188101187500004485 ) ) ;
#21617 = DIRECTION ( 'NONE',  ( -0.000000000000000000, -0.000000000000000000, -1.000000000000000000 ) ) ;
#21618 = CARTESIAN_POINT ( 'NONE',  ( 193.1444937042664094, 296.1109190324805240, -12.15243020627156767 ) ) ;
#21619 = CARTESIAN_POINT ( 'NONE',  ( 196.8104339078508076, 289.7613243423628546, -16.40335862274955403 ) ) ;
#21620 = EDGE_LOOP ( 'NONE', ( #11809, #26138, #27929, #74974 ) ) ;
#21621 = CARTESIAN_POINT ( 'NONE',  ( 70.45587595328763086, 60.93839127955427415, 14.43819332404346767 ) ) ;
#21622 = CARTESIAN_POINT ( 'NONE',  ( 198.3523905153085423, 287.0905771551796306, 18.52598547438866206 ) ) ;
#21623 = CARTESIAN_POINT ( 'NONE',  ( 156.3558586708529106, 268.1492557597510427, 15.72842580066797780 ) ) ;
#21624 = DIRECTION ( 'NONE',  ( 0.9347244501068350253, 0.3553733281669786970, 0.000000000000000000 ) ) ;
#21625 = CARTESIAN_POINT ( 'NONE',  ( 134.4004000680749300, 261.7365022471904012, 2.944929066748280225E-16 ) ) ;
#21626 = ORIENTED_EDGE ( 'NONE', *, *, #19434, .T. ) ;
#21627 = CARTESIAN_POINT ( 'NONE',  ( 70.59845676101609513, 64.76082698965105067, 12.92001219729134398 ) ) ;
#21628 = ORIENTED_EDGE ( 'NONE', *, *, #14654, .F. ) ;
#21629 = CARTESIAN_POINT ( 'NONE',  ( 47.96820964746023463, 80.67316705762479501, 10.00000000000000000 ) ) ;
#21630 = CARTESIAN_POINT ( 'NONE',  ( 86.67248974990208410, 44.58726045995240383, 6.056568617757574380 ) ) ;
#21631 = ORIENTED_EDGE ( 'NONE', *, *, #27427, .T. ) ;
#21632 = CARTESIAN_POINT ( 'NONE',  ( 185.0948665225164120, 293.0251998113765808, -10.41559016972385798 ) ) ;
#21633 = VERTEX_POINT ( 'NONE', #12990 ) ;
#21634 = CARTESIAN_POINT ( 'NONE',  ( 86.42135960654645999, 47.53165121735794685, -10.51235075660278362 ) ) ;
#21635 = CARTESIAN_POINT ( 'NONE',  ( 10.11087252192314345, 14.03677371833799725, 10.00000000000000533 ) ) ;
#21636 = CARTESIAN_POINT ( 'NONE',  ( 190.7742855516683278, 278.1955315082693687, -16.74573926298076998 ) ) ;
#21637 = CARTESIAN_POINT ( 'NONE',  ( 153.7958926348061368, 264.2646952915446263, -18.09980811596817318 ) ) ;
#21638 = CARTESIAN_POINT ( 'NONE',  ( 152.7729059155601021, 266.0365602647466972, -17.50667083025758686 ) ) ;
#21639 = CARTESIAN_POINT ( 'NONE',  ( 40.50696180670117741, 29.10170272979929962, -7.433330006724141015 ) ) ;
#21640 = DIRECTION ( 'NONE',  ( 0.9646071681523453734, -0.2636911283094539593, 0.000000000000000000 ) ) ;
#21641 = DIRECTION ( 'NONE',  ( 0.8660254037844341557, 0.5000000000000082157, -0.000000000000000000 ) ) ;
#21642 = PRODUCT_DEFINITION ( 'UNKNOWN', '', #83512, #78771 ) ;
#21643 = CARTESIAN_POINT ( 'NONE',  ( 189.5078380459772802, 300.6522465952268135, 0.4004850747286866630 ) ) ;
#21644 = VERTEX_POINT ( 'NONE', #50460 ) ;
#21645 = AXIS2_PLACEMENT_3D ( 'NONE', #14163, #6059, #21272 ) ;
#21646 = ORIENTED_EDGE ( 'NONE', *, *, #75470, .T. ) ;
#21647 = CARTESIAN_POINT ( 'NONE',  ( 157.7847820078105201, 257.3557362317297361, -18.02899742403477035 ) ) ;
#21648 = CARTESIAN_POINT ( 'NONE',  ( 182.5291792280718823, 296.7636338796572204, 0.3805386115670883473 ) ) ;
#21650 = CARTESIAN_POINT ( 'NONE',  ( 165.9477391530904242, 274.0934507990922384, -15.17489481902206272 ) ) ;
#21649 = CARTESIAN_POINT ( 'NONE',  ( 164.4294002498235159, 245.8469198396639399, 6.098783631055905374 ) ) ;
#21651 = CARTESIAN_POINT ( 'NONE',  ( 206.6395994010593427, 272.7367103121227387, -10.00948282007047219 ) ) ;
#21652 = CARTESIAN_POINT ( 'NONE',  ( 201.1327128468116143, 274.8997197801397192, -13.94580791315554613 ) ) ;
#21653 = CARTESIAN_POINT ( 'NONE',  ( 78.12619150794976974, 59.56496585069915284, -16.10012152594639900 ) ) ;
#21654 = CARTESIAN_POINT ( 'NONE',  ( 147.8465295590381743, 274.5692944114487091, 9.322947948439978205 ) ) ;
#21655 = CARTESIAN_POINT ( 'NONE',  ( 170.3109497006183801, 287.3311160575474332, -4.623670106724921069 ) ) ;
#21656 = CARTESIAN_POINT ( 'NONE',  ( 77.26689473168350730, 63.03694197878571970, -15.27008446967128386 ) ) ;
#21657 = AXIS2_PLACEMENT_3D ( 'NONE', #45413, #91556, #54492 ) ;
#21658 = CARTESIAN_POINT ( 'NONE',  ( 186.3952907517880817, 286.6368042130659433, -15.42260794059327900 ) ) ;
#21659 = CARTESIAN_POINT ( 'NONE',  ( 115.6001716039901055, 246.7369531367911009, -4.594050593750048428 ) ) ;
#21660 = ORIENTED_EDGE ( 'NONE', *, *, #15260, .T. ) ;
#21662 = B_SPLINE_CURVE_WITH_KNOTS ( 'NONE', 3,
 ( #77756, #54408, #69129, #99552 ),
 .UNSPECIFIED., .F., .F.,
 ( 4, 4 ),
 ( 0.003612368519395985772, 0.01157920093718791538 ),
 .UNSPECIFIED. ) ;
#21661 = CARTESIAN_POINT ( 'NONE',  ( 183.9106092447611900, 260.0878217146031375, -9.644928028340759241 ) ) ;
#21663 = CARTESIAN_POINT ( 'NONE',  ( 33.49697393745356777, 27.84335787977765264, 9.188101187500006262 ) ) ;
#21664 = CARTESIAN_POINT ( 'NONE',  ( 191.1174571109413591, 274.9979070728601869, 15.98165944953893991 ) ) ;
#21665 = EDGE_CURVE ( 'NONE', #75787, #1098, #26178, .T. ) ;
#21666 = ORIENTED_EDGE ( 'NONE', *, *, #87917, .F. ) ;
#21667 = CARTESIAN_POINT ( 'NONE',  ( 74.02653709664873816, 68.32631449583556105, -11.67658431812981412 ) ) ;
#21668 = CARTESIAN_POINT ( 'NONE',  ( 164.5824376406421266, 246.2431216187744667, -2.547103021557204805 ) ) ;
#21669 = CARTESIAN_POINT ( 'NONE',  ( 157.0935036675524827, 258.5530654392286465, 17.32636058289560665 ) ) ;
#21670 = CARTESIAN_POINT ( 'NONE',  ( -77.58047734835668052, 56.02942318228900120, -10.00000000000000000 ) ) ;
#21671 = CYLINDRICAL_SURFACE ( 'NONE', #90081, 17.82106496071139645 ) ;
#21672 = VERTEX_POINT ( 'NONE', #34758 ) ;
#21673 = CARTESIAN_POINT ( 'NONE',  ( 148.6214941521368758, 273.2270163621349752, 10.16346731517885082 ) ) ;
#21674 = EDGE_LOOP ( 'NONE', ( #21826, #59491, #17902, #51437 ) ) ;
#21675 = CARTESIAN_POINT ( 'NONE',  ( 28.00427808217458647, 41.79349426999503692, -10.00000000000000000 ) ) ;
#21676 = ORIENTED_EDGE ( 'NONE', *, *, #30161, .T. ) ;
#21677 = EDGE_CURVE ( 'NONE', #66481, #68024, #64240, .T. ) ;
#21678 = FACE_OUTER_BOUND ( 'NONE', #30663, .T. ) ;
#21679 = CARTESIAN_POINT ( 'NONE',  ( 193.7609008727193043, 262.8443104439116951, 4.759103018491034121 ) ) ;
#21680 = CARTESIAN_POINT ( 'NONE',  ( 158.3972311956721342, 263.3721427664003727, 17.45954809345846215 ) ) ;
#21681 = CARTESIAN_POINT ( 'NONE',  ( 83.46892329719068471, 47.64461127584740296, 12.06929726775783962 ) ) ;
#21683 = FACE_OUTER_BOUND ( 'NONE', #61724, .T. ) ;
#21682 = CARTESIAN_POINT ( 'NONE',  ( -8.669243101527598583, 25.19333184544591475, -10.00000000000000000 ) ) ;
#21684 = CARTESIAN_POINT ( 'NONE',  ( 201.4520623681621316, 281.7217880192456505, -17.56577389517433119 ) ) ;
#21685 = ORIENTED_EDGE ( 'NONE', *, *, #54704, .T. ) ;
#21686 = CARTESIAN_POINT ( 'NONE',  ( 66.60661563016273590, 67.77273566365288104, -7.043189648870076702 ) ) ;
#21687 = CARTESIAN_POINT ( 'NONE',  ( 82.39461015293801438, 51.35258621359815834, 14.58598051198313783 ) ) ;
#21688 = CARTESIAN_POINT ( 'NONE',  ( 82.19476570567245233, 41.21667155281596706, -3.467692515155950339 ) ) ;
#21689 = CARTESIAN_POINT ( 'NONE',  ( 170.0607343483624447, 248.7358776599870964, -0.2674079240231920784 ) ) ;
#21690 = CARTESIAN_POINT ( 'NONE',  ( 189.0380684747346152, 269.9222665765973943, -14.01655753500979351 ) ) ;
#21691 = CARTESIAN_POINT ( 'NONE',  ( 72.15692581984221476, 72.29159277512509618, 3.751890296296631178 ) ) ;
#21692 = DIRECTION ( 'NONE',  ( -0.000000000000000000, -0.000000000000000000, -1.000000000000000000 ) ) ;
#21693 = CARTESIAN_POINT ( 'NONE',  ( -80.27490717900100492, 58.06504152958491005, 10.00000000000000888 ) ) ;
#21694 = CARTESIAN_POINT ( 'NONE',  ( 191.1921138502980568, 283.4129728893950073, -16.58386050240950027 ) ) ;
#21695 = CARTESIAN_POINT ( 'NONE',  ( 82.74681249865726329, 53.90498867430740404, -15.82393922498146566 ) ) ;
#21696 = CARTESIAN_POINT ( 'NONE',  ( 67.34640541081718368, 215.8149278399160949, -9.188101187500095079 ) ) ;
#21697 = CARTESIAN_POINT ( 'NONE',  ( 159.5050723400634638, 254.3761059724978679, -15.34938048045353298 ) ) ;
#21698 = DIRECTION ( 'NONE',  ( 0.000000000000000000, 0.000000000000000000, 1.000000000000000000 ) ) ;
#21699 = DIRECTION ( 'NONE',  ( 0.000000000000000000, 0.000000000000000000, 1.000000000000000000 ) ) ;
#21700 = CARTESIAN_POINT ( 'NONE',  ( 207.2683629543511756, 271.6476598918739001, -6.694388351944108528 ) ) ;
#21701 = CARTESIAN_POINT ( 'NONE',  ( 67.29078699571681454, 69.45351283087119043, 0.2276663097563886018 ) ) ;
#21703 = CARTESIAN_POINT ( 'NONE',  ( -20.78934165772523812, 95.12062749311181165, 45.19946569820528737 ) ) ;
#21702 = CARTESIAN_POINT ( 'NONE',  ( 108.6384560342674064, 221.9824982072974251, 3.021315404115420679E-15 ) ) ;
#21704 = CARTESIAN_POINT ( 'NONE',  ( 43.80372508975956691, 30.45404122711137163, -8.090169943749478065 ) ) ;
#21705 = CARTESIAN_POINT ( 'NONE',  ( -46.49770490450612215, 29.77544742692501600, -10.00000000000000000 ) ) ;
#21706 = CARTESIAN_POINT ( 'NONE',  ( 82.62625517957130228, 54.11794360844533003, 15.53797790719450056 ) ) ;
#21707 = CARTESIAN_POINT ( 'NONE',  ( 72.17098681862357523, 72.08342691454184603, 2.975191886509651162 ) ) ;
#21708 = VECTOR ( 'NONE', #66419, 1000.000000000000000 ) ;
#21709 = ADVANCED_FACE ( 'NONE', ( #73777 ), #4366, .F. ) ;
#21710 = DIRECTION ( 'NONE',  ( -0.000000000000000000, -0.000000000000000000, -1.000000000000000000 ) ) ;
#21712 = CARTESIAN_POINT ( 'NONE',  ( 199.3058668659812724, 277.8561274100368905, 16.30908028197919535 ) ) ;
#21711 = VECTOR ( 'NONE', #90173, 1000.000000000000000 ) ;
#21713 = CARTESIAN_POINT ( 'NONE',  ( 147.8505793332463725, 274.5622799967613332, -9.317516487097901035 ) ) ;
#21714 = CARTESIAN_POINT ( 'NONE',  ( 71.86515158781777757, 72.12545754810727772, -1.692783104835278607 ) ) ;
#21715 = CARTESIAN_POINT ( 'NONE',  ( 46.23738328933649200, 191.3768266524159856, -9.188101187500093303 ) ) ;
#21716 = CARTESIAN_POINT ( 'NONE',  ( 25.24326406500046360, 20.28920272979927475, -7.433330006724141015 ) ) ;
#21717 = CARTESIAN_POINT ( 'NONE',  ( 151.4188942279983223, 268.3817773016460251, -14.77302265413830895 ) ) ;
#21718 = CARTESIAN_POINT ( 'NONE',  ( 149.3629284598386278, 271.9428144707212027, -12.99253781774931049 ) ) ;
#21719 = CARTESIAN_POINT ( 'NONE',  ( 12.88253908977640094, 9.298606405272902720, -2.839279412974138328 ) ) ;
#21720 = CARTESIAN_POINT ( 'NONE',  ( 157.3029956111992362, 258.1902147490555421, -18.22269824972649843 ) ) ;
#21721 = DIRECTION ( 'NONE',  ( -0.9140770918436990078, -0.4055404667435369426, 0.000000000000000000 ) ) ;
#21722 = CARTESIAN_POINT ( 'NONE',  ( 175.6422712798515420, 291.0239839832145208, 2.433063146221782436 ) ) ;
#21723 = CARTESIAN_POINT ( 'NONE',  ( 179.9202220416364355, 276.5770508256506446, 16.41260542237966646 ) ) ;
#21724 = CARTESIAN_POINT ( 'NONE',  ( 73.57124375542366579, 65.07890931487162334, 13.30975167017917471 ) ) ;
#21725 = CARTESIAN_POINT ( 'NONE',  ( 149.1653648461108617, 275.5304674000249179, 7.618651205328232479 ) ) ;
#21726 = CARTESIAN_POINT ( 'NONE',  ( 163.2804934380540658, 256.0196637926906078, -14.90650773794625472 ) ) ;
#21727 = DIRECTION ( 'NONE',  ( -0.000000000000000000, 0.000000000000000000, -1.000000000000000000 ) ) ;
#21728 = CARTESIAN_POINT ( 'NONE',  ( 87.79103035407327127, 45.19801466894013942, -6.906962003849810294 ) ) ;
#21729 = CARTESIAN_POINT ( 'NONE',  ( 97.16130770534417138, 220.2365022471902023, 10.00000000000009592 ) ) ;
#21730 = CARTESIAN_POINT ( 'NONE',  ( 161.2799361541916028, 251.3019516699124836, 14.40628917569557110 ) ) ;
#21731 = CARTESIAN_POINT ( 'NONE',  ( -18.06269525828470890, 104.2312461070085021, 45.19948692389422717 ) ) ;
#21732 = ORIENTED_EDGE ( 'NONE', *, *, #82817, .T. ) ;
#21733 = CARTESIAN_POINT ( 'NONE',  ( 58.87550765610937731, 213.9869531367911009, 4.594050593750046652 ) ) ;
#21734 = EDGE_LOOP ( 'NONE', ( #46283, #73198, #57401, #51411 ) ) ;
#21735 = CARTESIAN_POINT ( 'NONE',  ( 184.1612352507079322, 265.5980064862902168, 14.76078110080899641 ) ) ;
#21736 = CARTESIAN_POINT ( 'NONE',  ( 161.6369034275210481, 251.0970872729290591, 12.75120819296054009 ) ) ;
#21737 = CARTESIAN_POINT ( 'NONE',  ( 25.96864935082050252, 154.0458036431183189, -21.50000000000001421 ) ) ;
#21738 = ORIENTED_EDGE ( 'NONE', *, *, #14349, .T. ) ;
#21739 = LINE ( 'NONE', #97764, #76463 ) ;
#21740 = CARTESIAN_POINT ( 'NONE',  ( 207.6860335175200589, 270.9242332556395922, 6.913225035677485586 ) ) ;
#21741 = DIRECTION ( 'NONE',  ( 1.000000000000000000, 0.000000000000000000, 2.816764622163176999E-16 ) ) ;
#21742 = DIRECTION ( 'NONE',  ( -0.8660254037844387076, -0.4999999999999998890, -0.000000000000000000 ) ) ;
#21743 = CARTESIAN_POINT ( 'NONE',  ( 206.8776226275057297, 271.8386879954387609, -6.083657955821966112 ) ) ;
#21744 = CARTESIAN_POINT ( 'NONE',  ( 157.4243923570103050, 257.9799494174374104, 18.06359219958597606 ) ) ;
#21745 = EDGE_LOOP ( 'NONE', ( #72301, #4485, #72292 ) ) ;
#21746 = PRODUCT_DEFINITION ( 'UNKNOWN', '', #96465, #26066 ) ;
#21747 = CARTESIAN_POINT ( 'NONE',  ( 22.06543860749898656, 21.24335787977763346, -9.188101187500008038 ) ) ;
#21748 = CARTESIAN_POINT ( 'NONE',  ( 70.27050606688109724, 70.17526897919434248, -5.379368406286444859 ) ) ;
#21749 = CARTESIAN_POINT ( 'NONE',  ( -56.06787742410712383, 34.75406423768147590, 10.00000000000000000 ) ) ;
#21750 = ORIENTED_EDGE ( 'NONE', *, *, #21901, .T. ) ;
#21751 = DIRECTION ( 'NONE',  ( -0.000000000000000000, -0.000000000000000000, -1.000000000000000000 ) ) ;
#21752 = CARTESIAN_POINT ( 'NONE',  ( 33.47037235539275457, 49.41749479597460493, -10.00000000000000000 ) ) ;
#21753 = VERTEX_POINT ( 'NONE', #88038 ) ;
#21755 = CARTESIAN_POINT ( 'NONE',  ( -86.81108781737714253, 4.999999999999999112, 0.000000000000000000 ) ) ;
#21754 = DIRECTION ( 'NONE',  ( 0.000000000000000000, 1.000000000000000000, 0.000000000000000000 ) ) ;
#21756 = CARTESIAN_POINT ( 'NONE',  ( 162.6341128535665064, 248.9564488241690299, -10.63508949045170660 ) ) ;
#21757 = CARTESIAN_POINT ( 'NONE',  ( 204.5730103890532519, 276.3161474792809145, 14.88139715235883109 ) ) ;
#21758 = CARTESIAN_POINT ( 'NONE',  ( 188.5952966566430860, 295.4055683097271867, -11.38938388239568056 ) ) ;
#21759 = DIRECTION ( 'NONE',  ( 0.1378186779084994706, -0.2387089523694924387, -0.9612616959383186721 ) ) ;
#21760 = CARTESIAN_POINT ( 'NONE',  ( 164.3743206631776275, 265.6518399700423174, -16.94241144619603290 ) ) ;
#21761 = CARTESIAN_POINT ( 'NONE',  ( 128.2929432021470575, 251.0024278399160949, 9.188101187500095079 ) ) ;
#21762 = CARTESIAN_POINT ( 'NONE',  ( 160.0364848823596731, 255.1851680591929892, -16.26533138570701809 ) ) ;
#21763 = CARTESIAN_POINT ( 'NONE',  ( 83.72013207082297015, 209.9548013555409796, -4.594050593750042211 ) ) ;
#21764 = VERTEX_POINT ( 'NONE', #20084 ) ;
#21765 = CARTESIAN_POINT ( 'NONE',  ( 171.9709265855787521, 264.6047551489337479, 15.86023412204940897 ) ) ;
#21766 = CARTESIAN_POINT ( 'NONE',  ( 204.6282099259498182, 271.7394219149207970, 9.770859781323483872 ) ) ;
#21767 = EDGE_CURVE ( 'NONE', #57975, #86867, #41252, .T. ) ;
#21768 = VERTEX_POINT ( 'NONE', #93868 ) ;
#21769 = CARTESIAN_POINT ( 'NONE',  ( 160.7611904649662051, 253.0402142913282830, 14.60361351347018477 ) ) ;
#21770 = ORIENTED_EDGE ( 'NONE', *, *, #47859, .T. ) ;
#21771 = VERTEX_POINT ( 'NONE', #30148 ) ;
#21772 = FACE_BOUND ( 'NONE', #26126, .T. ) ;
#21773 = CARTESIAN_POINT ( 'NONE',  ( 66.97041650028039328, 68.04972680430266507, 6.918031611078456322 ) ) ;
#21774 = CARTESIAN_POINT ( 'NONE',  ( 194.3094773688834778, 284.8302703302293253, 17.74979085435418469 ) ) ;
#21775 = CARTESIAN_POINT ( 'NONE',  ( 191.7741832257749195, 298.4843664033717801, -8.615487418695501276 ) ) ;
#21776 =( BOUNDED_CURVE ( )  B_SPLINE_CURVE ( 2, ( #79722, #72092, #19885, #87363, #57862, #2693, #11792, #17892, #95440, #42648, #64982, #73580, #27485 ),
 .UNSPECIFIED., .F., .T. ) 
 B_SPLINE_CURVE_WITH_KNOTS ( ( 3, 2, 2, 2, 2, 2, 3 ),
 ( 0.8875000000000000666, 0.8900000000000000133, 0.8950000000000000178, 0.9000000000000000222, 0.9050000000000000266, 0.9100000000000000311, 0.9125000000000000888 ),
 .UNSPECIFIED. ) 
 CURVE ( )  GEOMETRIC_REPRESENTATION_ITEM ( )  RATIONAL_B_SPLINE_CURVE ( ( 0.9755282581475767101, 0.9755282581475772652, 1.000000000000000000, 0.9510565162951535312, 1.000000000000000000, 0.9510565162951535312, 1.000000000000000000, 0.9510565162951535312, 1.000000000000000000, 0.9510565162951535312, 1.000000000000000000, 0.9755282581475761550, 0.9755282581475767101 ) ) 
 REPRESENTATION_ITEM ( '' )  );
#21777 = CARTESIAN_POINT ( 'NONE',  ( 81.26140763373125253, 56.17807541021651474, 16.09937115873037072 ) ) ;
#21778 = CARTESIAN_POINT ( 'NONE',  ( 194.4459411895494725, 293.8567458645873103, 14.31012567920753042 ) ) ;
#21779 = CARTESIAN_POINT ( 'NONE',  ( 70.09004903573875822, 62.97794529296450605, 13.29049216610558126 ) ) ;
#21780 = CARTESIAN_POINT ( 'NONE',  ( 182.0092902691650920, 257.1508607890800135, -6.141684172092635841 ) ) ;
#21781 = VERTEX_POINT ( 'NONE', #24425 ) ;
#21782 = CIRCLE ( 'NONE', #18616, 70.00000000000001421 ) ;
#21783 = EDGE_CURVE ( 'NONE', #38435, #91209, #36404, .T. ) ;
#21784 = B_SPLINE_SURFACE_WITH_KNOTS ( 'NONE', 3, 1, ( 
 ( #78722, #69603 ),
 ( #55874, #9311 ),
 ( #40184, #1728 ),
 ( #78221, #93446 ),
 ( #16403, #92449 ),
 ( #84846, #22995 ),
 ( #54897, #15384 ),
 ( #100028, #23998 ),
 ( #46281, #53886 ),
 ( #77209, #32607 ),
 ( #70601, #63004 ),
 ( #47296, #1214 ),
 ( #62481, #207 ),
 ( #86870, #8312 ),
 ( #8805, #63504 ),
 ( #7812, #94442 ),
 ( #38697, #93949 ),
 ( #54376, #24503 ),
 ( #61980, #55382 ),
 ( #23487, #9829 ),
 ( #17403, #86366 ),
 ( #85351, #24997 ),
 ( #15898, #46805 ),
 ( #77727, #39177 ),
 ( #16896, #48313 ),
 ( #79258, #30614 ),
 ( #40690, #61499 ),
 ( #2729, #87394 ),
 ( #51161, #4576 ),
 ( #97306, #27383 ),
 ( #82125, #25509 ),
 ( #67361, #51681 ),
 ( #59240, #66864 ),
 ( #56399, #12697 ) ),
 .UNSPECIFIED., .T., .F., .F.,
 ( 4, 2, 2, 2, 2, 2, 2, 2, 2, 2, 2, 2, 2, 2, 2, 2, 4 ),
 ( 2, 2 ),
 ( 0.000000000000000000, 0.06250000000000000000, 0.1250000000000000000, 0.1875000000000000000, 0.2500000000000000000, 0.3125000000000000000, 0.3750000000000000000, 0.4375000000000000000, 0.5000000000000000000, 0.5625000000000000000, 0.6250000000000000000, 0.6875000000000000000, 0.7500000000000000000, 0.8125000000000000000, 0.8750000000000000000, 0.9375000000000000000, 1.000000000000000000 ),
 ( 0.000000000000000000, 1.000000000000000000 ),
 .UNSPECIFIED. ) ;
#21785 = CARTESIAN_POINT ( 'NONE',  ( 186.5210254826074276, 287.5177492320627266, 16.01978303813461935 ) ) ;
#21786 = ORIENTED_EDGE ( 'NONE', *, *, #88875, .F. ) ;
#21787 = EDGE_CURVE ( 'NONE', #52455, #57758, #60534, .T. ) ;
#21788 = CARTESIAN_POINT ( 'NONE',  ( 163.9470117944672438, 260.6273701597328341, -16.21158959658340493 ) ) ;
#21789 = CARTESIAN_POINT ( 'NONE',  ( 164.5451017335383597, 246.7547400039435956, 5.445355051732909679 ) ) ;
#21790 = AXIS2_PLACEMENT_3D ( 'NONE', #73940, #67832, #20243 ) ;
#21791 = CARTESIAN_POINT ( 'NONE',  ( 185.1394335896403902, 275.7790610180006752, 16.42070492368160117 ) ) ;
#21792 = CARTESIAN_POINT ( 'NONE',  ( 164.8616299252405213, 245.0982760813026857, 1.544363874765093625 ) ) ;
#21793 = DIRECTION ( 'NONE',  ( -0.4972609476841356457, 0.8612812260087758798, 0.1045284632676436315 ) ) ;
#21794 = CARTESIAN_POINT ( 'NONE',  ( 195.2502824789841895, 279.2012642199275660, 16.31828257502794699 ) ) ;
#21795 = CARTESIAN_POINT ( 'NONE',  ( 162.9177813375093820, 261.5106994340935671, 17.39058219678560135 ) ) ;
#21796 = CARTESIAN_POINT ( 'NONE',  ( 135.0589402170954827, 248.7833772461660544, -9.188101187500095079 ) ) ;
#21797 = ORIENTED_EDGE ( 'NONE', *, *, #12664, .T. ) ;
#21798 = CARTESIAN_POINT ( 'NONE',  ( 81.24342585074298029, 44.30867135165726722, -10.09829603353806071 ) ) ;
#21799 = CARTESIAN_POINT ( 'NONE',  ( 79.49951204047911801, 46.37032438487753438, 12.70281872619212926 ) ) ;
#21800 = CARTESIAN_POINT ( 'NONE',  ( 88.10271290040205372, 43.80081590334129515, -2.139902876137079080 ) ) ;
#21801 = CARTESIAN_POINT ( 'NONE',  ( 79.43566581485079325, 59.14155571097092690, -16.22735706158325542 ) ) ;
#21802 = CARTESIAN_POINT ( 'NONE',  ( 70.96263597670173340, 67.29475622062147977, -10.35096767034863774 ) ) ;
#21803 = ORIENTED_EDGE ( 'NONE', *, *, #50506, .F. ) ;
#21804 = CARTESIAN_POINT ( 'NONE',  ( 76.44905381598371719, 54.38756756234472789, 16.09189434050703582 ) ) ;
#21805 = CARTESIAN_POINT ( 'NONE',  ( 148.0770056944566022, 275.8785175959847038, -3.807152131487734348 ) ) ;
#21806 = B_SPLINE_CURVE_WITH_KNOTS ( 'NONE', 3,
 ( #69417, #29, #30914, #86179, #23806, #24808, #10122, #16713, #62294, #47606, #87194, #40987, #16216, #78534, #2022, #56198, #94748, #32418, #9119, #39991, #33417, #54695, #95274, #71931, #17727, #85157, #1536, #64316, #63313, #48110, #85679, #520, #79052, #9641, #40500, #71432, #32907, #48629, #46603, #79564, #39000, #2535, #93251, #47108, #70413, #1021, #86070, #32792, #38890, #18106 ),
 .UNSPECIFIED., .F., .F.,
 ( 4, 2, 2, 2, 2, 2, 2, 2, 2, 2, 2, 2, 2, 2, 2, 2, 2, 2, 2, 2, 2, 2, 2, 2, 4 ),
 ( 0.0007103610476057106715, 0.001202613152260477609, 0.001694865256915244331, 0.001940991309242592021, 0.002187117361569939494, 0.002310180387733583741, 0.002433243413897227987, 0.002556306440060872667, 0.002679369466224516480, 0.002925495518551847040, 0.003171621570879177600, 0.003663873675533679125, 0.004648377884842772381, 0.005632882094151865637, 0.006125134198806411398, 0.006617386303460958026, 0.006740449329624556736, 0.006801980842706337009, 0.006863512355788118149, 0.006986575381951677828, 0.007109638408115237507, 0.007355764460442497377, 0.007601890512769757247, 0.008094142617424250966, 0.008586394722078742950 ),
 .UNSPECIFIED. ) ;
#21807 = DIRECTION ( 'NONE',  ( -0.8902628732232698017, 0.4554470513245731933, 0.000000000000000000 ) ) ;
#21808 = CARTESIAN_POINT ( 'NONE',  ( 80.53565967596219366, 49.57456898333717277, 14.21858742687847688 ) ) ;
#21809 = CARTESIAN_POINT ( 'NONE',  ( 199.1113007661987240, 266.5577079162528094, 0.8260111218802939081 ) ) ;
#21810 = CARTESIAN_POINT ( 'NONE',  ( 197.6828869641981612, 265.7779761413833626, 0.8200578392135022820 ) ) ;
#21811 = CARTESIAN_POINT ( 'NONE',  ( 147.0538900202505488, 275.9421863647172017, 5.192507380313251986 ) ) ;
#21812 = CARTESIAN_POINT ( 'NONE',  ( 185.0761968336884138, 281.7485531843886406, 16.20522637585934689 ) ) ;
#21813 = VECTOR ( 'NONE', #4691, 1000.000000000000114 ) ;
#21814 = CARTESIAN_POINT ( 'NONE',  ( 164.5416088356626290, 245.6525688679454618, -1.463507744092769292 ) ) ;
#21815 = CARTESIAN_POINT ( 'NONE',  ( 196.8474129767564875, 269.8048104555306281, 12.12537726023140117 ) ) ;
#21816 = EDGE_CURVE ( 'NONE', #23113, #79865, #91003, .T. ) ;
#21817 = EDGE_CURVE ( 'NONE', #80050, #5537, #33893, .T. ) ;
#21818 = CARTESIAN_POINT ( 'NONE',  ( 17.74977768659132593, 33.18080186712593616, 3.090169943749475401 ) ) ;
#21819 = CARTESIAN_POINT ( 'NONE',  ( 68.34576586436469370, 65.68917945663493185, -10.35820680181607401 ) ) ;
#21820 = CARTESIAN_POINT ( 'NONE',  ( 205.1385161361615701, 274.5423688205104895, 11.59183615411821933 ) ) ;
#21821 = CARTESIAN_POINT ( 'NONE',  ( 26.22111236500157361, 16.10801979619929369, 3.090169943749476733 ) ) ;
#21822 = CARTESIAN_POINT ( 'NONE',  ( 198.6012358295098750, 286.6595644277572887, 18.21911298807435386 ) ) ;
#21823 = CARTESIAN_POINT ( 'NONE',  ( 72.29127226384117932, 72.04750469537891888, -3.387169285285207554 ) ) ;
#21824 = CARTESIAN_POINT ( 'NONE',  ( -5.778093977583854013, 155.2202760586659451, -5.415160957724236172E-17 ) ) ;
#21825 = CARTESIAN_POINT ( 'NONE',  ( 172.5963845202620064, 283.7040405909344827, -12.35744486217303084 ) ) ;
#21826 = ORIENTED_EDGE ( 'NONE', *, *, #93450, .T. ) ;
#21827 = EDGE_CURVE ( 'NONE', #29478, #23143, #95388, .T. ) ;
#21828 = CARTESIAN_POINT ( 'NONE',  ( 66.76615945880296010, 67.52988098192712130, -6.530483747860452937 ) ) ;
#21829 = FACE_OUTER_BOUND ( 'NONE', #2748, .T. ) ;
#21830 = CARTESIAN_POINT ( 'NONE',  ( 202.5011135140420606, 274.1303848594789088, -12.97262903380130261 ) ) ;
#21831 = CARTESIAN_POINT ( 'NONE',  ( 198.4344074287054696, 286.9485196940960918, -17.83642855442570152 ) ) ;
#21832 = CARTESIAN_POINT ( 'NONE',  ( 7.428446334363822956, 175.0958772461660544, -9.188101187500095079 ) ) ;
#21833 = CARTESIAN_POINT ( 'NONE',  ( 180.7163234865986681, 274.9646179361455438, -16.46674387372169690 ) ) ;
#21834 = CARTESIAN_POINT ( 'NONE',  ( 27.10026011071931151, 20.81029122506295437, 8.090169943749479842 ) ) ;
#21835 = CARTESIAN_POINT ( 'NONE',  ( 85.70209702422732789, 48.64685655562228561, 12.37813881961889528 ) ) ;
#21836 = CARTESIAN_POINT ( 'NONE',  ( 170.6324991628954990, 271.0675588811652119, -17.59648249145834953 ) ) ;
#21837 = CARTESIAN_POINT ( 'NONE',  ( 71.90245059369782155, 72.17364547496468674, -3.641340926847324244 ) ) ;
#21838 = CARTESIAN_POINT ( 'NONE',  ( 150.1550056273443943, 276.5028295449805000, 3.910624302002001063 ) ) ;
#21839 = EDGE_CURVE ( 'NONE', #76328, #38319, #38692, .T. ) ;
#21840 = EDGE_CURVE ( 'NONE', #12202, #947, #39938, .T. ) ;
#21841 = CARTESIAN_POINT ( 'NONE',  ( 175.7921476968669197, 253.7367219729100327, -3.864758291546732671 ) ) ;
#21842 = CARTESIAN_POINT ( 'NONE',  ( 150.9195128607351251, 269.2467312020988857, 13.93698123781031484 ) ) ;
#21843 = CIRCLE ( 'NONE', #67185, 10.99999999999999112 ) ;
#21844 = CARTESIAN_POINT ( 'NONE',  ( 46.06580888206220692, 210.7365022471903444, 2.944929066748280225E-16 ) ) ;
#21845 = PLANE ( 'NONE',  #49056 ) ;
#21846 = CARTESIAN_POINT ( 'NONE',  ( 190.5674408456512765, 300.5745055173924811, -0.9151048603553563199 ) ) ;
#21847 = CARTESIAN_POINT ( 'NONE',  ( 20.93329029645117245, 173.7048013555409796, 4.594050593750051981 ) ) ;
#21848 = CARTESIAN_POINT ( 'NONE',  ( 164.5737363065680370, 285.5024452864429918, 4.376381487704442463 ) ) ;
#21849 = CARTESIAN_POINT ( 'NONE',  ( 153.3616370783189211, 265.0168479788495688, 17.48287904751960653 ) ) ;
#21850 = CARTESIAN_POINT ( 'NONE',  ( 34.65648599653719231, 40.98502408145595410, -5.678558825948271327 ) ) ;
#21851 = CARTESIAN_POINT ( 'NONE',  ( 202.0661878422603763, 279.1895584290143120, -16.02388874507808225 ) ) ;
#21852 = AXIS2_PLACEMENT_3D ( 'NONE', #9844, #40704, #2239 ) ;
#21853 = CARTESIAN_POINT ( 'NONE',  ( 206.8968397926183229, 272.2911568841838061, 7.145103750817420440 ) ) ;
#21854 = CARTESIAN_POINT ( 'NONE',  ( 185.4724734968301618, 266.2864717598490643, 14.59729369397538612 ) ) ;
#21855 = CARTESIAN_POINT ( 'NONE',  ( 201.5189872289815867, 266.7509884862435570, -2.318412474989284267 ) ) ;
#21856 = CARTESIAN_POINT ( 'NONE',  ( 164.1744119160098023, 281.5290954411402709, 9.010387237428474805 ) ) ;
#21857 = CARTESIAN_POINT ( 'NONE',  ( 9.881553883097156543, 27.74646525600388713, 2.839279412974139660 ) ) ;
#21858 = CARTESIAN_POINT ( 'NONE',  ( 190.5893431400089923, 300.5365696307625853, -0.3099240395267599535 ) ) ;
#21859 = CARTESIAN_POINT ( 'NONE',  ( 71.49559693922878978, 59.13754170620860862, 15.29921231604372878 ) ) ;
#21860 = CARTESIAN_POINT ( 'NONE',  ( 201.1389011169710272, 268.2808080133845010, 7.540724018285327013 ) ) ;
#21861 = ORIENTED_EDGE ( 'NONE', *, *, #18709, .F. ) ;
#21862 = CARTESIAN_POINT ( 'NONE',  ( 86.63427790160775999, 45.49709482439454433, -7.739417912740459649 ) ) ;
#21863 = DIRECTION ( 'NONE',  ( 0.4829524219151267173, -0.8756465943326184886, 0.000000000000000000 ) ) ;
#21864 = CARTESIAN_POINT ( 'NONE',  ( 81.85012752262665003, 42.15354315940976448, 7.594371692912019967 ) ) ;
#21865 = ORIENTED_EDGE ( 'NONE', *, *, #25882, .F. ) ;
#21866 = CARTESIAN_POINT ( 'NONE',  ( 22.87549206224920439, 39.05096577487528009, -10.00000000000000000 ) ) ;
#21867 = CARTESIAN_POINT ( 'NONE',  ( 68.11960572793796587, 69.93251101871156550, 0.1879669648890121281 ) ) ;
#21868 = FACE_OUTER_BOUND ( 'NONE', #12983, .T. ) ;
#21869 = CARTESIAN_POINT ( 'NONE',  ( 155.0619429961492983, 262.0718317407570339, -17.08853361476647592 ) ) ;
#21870 = EDGE_LOOP ( 'NONE', ( #5628, #13645, #44353, #86256 ) ) ;
#21872 = CARTESIAN_POINT ( 'NONE',  ( 164.1259971043086239, 246.3724295028720519, 5.761669507629934905 ) ) ;
#21871 = CARTESIAN_POINT ( 'NONE',  ( 186.2429809382703354, 271.9601928012535268, -16.35413080596582347 ) ) ;
#21873 = VERTEX_POINT ( 'NONE', #65420 ) ;
#21874 = CARTESIAN_POINT ( 'NONE',  ( 201.3505934466285510, 281.8975373467312693, -16.83770227898004279 ) ) ;
#21875 = CARTESIAN_POINT ( 'NONE',  ( 70.79475271764948729, 66.96855654029467075, 11.21893109225559648 ) ) ;
#21876 = CARTESIAN_POINT ( 'NONE',  ( 80.47095457055254997, 57.75622231085855418, 16.59751886879109506 ) ) ;
#21877 = CARTESIAN_POINT ( 'NONE',  ( 72.32955901973197399, 69.72760921849626925, -9.141978898838837964 ) ) ;
#21878 = ORIENTED_EDGE ( 'NONE', *, *, #4007, .F. ) ;
#21879 = DIRECTION ( 'NONE',  ( 0.5000000000000013323, -0.8660254037844378194, 0.000000000000000000 ) ) ;
#21881 = EDGE_CURVE ( 'NONE', #31813, #60349, #5123, .T. ) ;
#21880 = AXIS2_PLACEMENT_3D ( 'NONE', #8724, #31506, #85266 ) ;
#21882 = VERTEX_POINT ( 'NONE', #13237 ) ;
#21883 = CARTESIAN_POINT ( 'NONE',  ( 206.4695239676918845, 273.0312896038346366, 10.41704154450801667 ) ) ;
#21884 = LINE ( 'NONE', #90345, #31593 ) ;
#21885 = ORIENTED_EDGE ( 'NONE', *, *, #57447, .T. ) ;
#21886 = CARTESIAN_POINT ( 'NONE',  ( 149.3883679478359454, 271.8987519849911223, 12.99187507659642371 ) ) ;
#21887 = CARTESIAN_POINT ( 'NONE',  ( 193.2902653713029508, 264.7699875813403310, -9.193237569391540021 ) ) ;
#21888 = EDGE_CURVE ( 'NONE', #56406, #92904, #73534, .T. ) ;
#21889 = ORIENTED_EDGE ( 'NONE', *, *, #40732, .T. ) ;
#21890 = CARTESIAN_POINT ( 'NONE',  ( -17.55320919825948778, 75.98467192273231774, 13.40974089753184195 ) ) ;
#21891 = CARTESIAN_POINT ( 'NONE',  ( 149.0243928082760192, 274.5278390230128025, 9.115363623326919296 ) ) ;
#21892 = DIRECTION ( 'NONE',  ( -0.000000000000000000, -0.000000000000000000, -1.000000000000000000 ) ) ;
#21893 = LINE ( 'NONE', #98918, #17200 ) ;
#21894 = EDGE_LOOP ( 'NONE', ( #62764, #37456, #40683, #33864 ) ) ;
#21895 = ORIENTED_EDGE ( 'NONE', *, *, #85316, .F. ) ;
#21896 = CARTESIAN_POINT ( 'NONE',  ( 79.69350452701492316, 51.55546628257836517, -15.65634712508320803 ) ) ;
#21897 = CARTESIAN_POINT ( 'NONE',  ( 73.43762515466688967, 73.52662068827324049, 2.033788753608857291E-15 ) ) ;
#21898 = CARTESIAN_POINT ( 'NONE',  ( 148.0427192501136062, 274.2294838985851015, 9.385226820296049155 ) ) ;
#21899 = CARTESIAN_POINT ( 'NONE',  ( 149.6071296322179194, 271.5198456328920997, 12.75640156477042453 ) ) ;
#21900 = CARTESIAN_POINT ( 'NONE',  ( 152.8134625983922490, 265.9663140294953791, 17.57333028169644251 ) ) ;
#21901 = EDGE_CURVE ( 'NONE', #56569, #98290, #66418, .T. ) ;
#21902 = CARTESIAN_POINT ( 'NONE',  ( 146.5443760852173227, 276.8246903873589986, -0.3422986961735821065 ) ) ;
#21903 = CARTESIAN_POINT ( 'NONE',  ( 191.0862225170008628, 299.6759493045793192, -9.402218231374108726 ) ) ;
#21904 = CARTESIAN_POINT ( 'NONE',  ( 75.80790870016019767, 57.44398695910171426, -16.10616469783059301 ) ) ;
#21905 = CARTESIAN_POINT ( 'NONE',  ( 71.34475373241517104, 70.22794211031242639, 6.670480703838566505 ) ) ;
#21907 = DIRECTION ( 'NONE',  ( 0.4999999999999992784, -0.8660254037844390407, 0.000000000000000000 ) ) ;
#21906 = CARTESIAN_POINT ( 'NONE',  ( 149.6890529486499872, 271.3779502865075983, -12.51465682618088593 ) ) ;
#21908 = FACE_OUTER_BOUND ( 'NONE', #67035, .T. ) ;
#21909 = CARTESIAN_POINT ( 'NONE',  ( 168.2861312974920338, 286.3523900831025344, 3.986708875144260311 ) ) ;
#21910 = CARTESIAN_POINT ( 'NONE',  ( 78.74568341211313793, 47.64299656527150262, 14.28912099471933850 ) ) ;
#21911 = CARTESIAN_POINT ( 'NONE',  ( 101.2839494695023603, 229.2833772461660544, -9.188101187500095079 ) ) ;
#21912 = ORIENTED_EDGE ( 'NONE', *, *, #97112, .T. ) ;
#21913 = DIRECTION ( 'NONE',  ( 0.4999999999999998890, -0.8660254037844385966, 0.000000000000000000 ) ) ;
#21914 = CARTESIAN_POINT ( 'NONE',  ( 77.34456863197527809, 53.78998963892438212, -15.98317469749341591 ) ) ;
#21915 = CARTESIAN_POINT ( 'NONE',  ( 148.7795025377680815, 273.5541084840127724, 8.957187006633716919 ) ) ;
#21916 = EDGE_CURVE ( 'NONE', #24285, #94448, #97346, .T. ) ;
#21917 = CARTESIAN_POINT ( 'NONE',  ( 79.35938606471496826, 46.19917012563481507, 12.64008113691103752 ) ) ;
#21918 = EDGE_CURVE ( 'NONE', #89828, #2810, #30266, .T. ) ;
#21919 = LINE ( 'NONE', #60900, #43428 ) ;
#21920 = CARTESIAN_POINT ( 'NONE',  ( 193.0622221429366050, 289.4054684591471300, 16.71589558189321778 ) ) ;
#21921 = CARTESIAN_POINT ( 'NONE',  ( 168.0580858286423052, 284.4539385443458741, -7.981534432883824692 ) ) ;
#21922 = VERTEX_POINT ( 'NONE', #20332 ) ;
#21923 = CARTESIAN_POINT ( 'NONE',  ( 170.6462599113855561, 255.5044248170252388, -12.77826996180470864 ) ) ;
#21924 = CARTESIAN_POINT ( 'NONE',  ( -22.42236680055709641, 157.8615022471902591, 0.000000000000000000 ) ) ;
#21925 = CARTESIAN_POINT ( 'NONE',  ( 72.09435550024913653, 71.41332343156211948, 5.094207931309262527 ) ) ;
#21926 = CARTESIAN_POINT ( 'NONE',  ( 44.46005344233076784, 183.1427522451417360, 1.119607411625061291E-15 ) ) ;
#21927 = CARTESIAN_POINT ( 'NONE',  ( 122.2582625392304863, 232.2048013555409796, 4.594050593750051981 ) ) ;
#21928 = CARTESIAN_POINT ( 'NONE',  ( 198.8157103782086210, 286.2880836124806478, -18.60729372713428020 ) ) ;
#21929 = CARTESIAN_POINT ( 'NONE',  ( -76.23101443460923576, 54.01191295053621388, -10.00000000000000000 ) ) ;
#21930 = CARTESIAN_POINT ( 'NONE',  ( 104.9037214839949002, 219.8262482093457777, 3.021315404115420679E-15 ) ) ;
#21931 = CARTESIAN_POINT ( 'NONE',  ( 174.4680951374541849, 252.9015896160454702, -3.884363688654588476 ) ) ;
#21932 = CARTESIAN_POINT ( 'NONE',  ( 29.86365662933068066, 197.2369531367911293, -4.594050593750048428 ) ) ;
#21933 = LINE ( 'NONE', #6743, #30085 ) ;
#21934 = EDGE_CURVE ( 'NONE', #35455, #23265, #91847, .T. ) ;
#21935 = ORIENTED_EDGE ( 'NONE', *, *, #26555, .T. ) ;
#21936 = CARTESIAN_POINT ( 'NONE',  ( 188.4805308512120234, 298.0761574053781828, 7.892637567094712203 ) ) ;
#21937 = CARTESIAN_POINT ( 'NONE',  ( 179.2182182526515248, 265.9655207074544592, 16.25122323871343610 ) ) ;
#21938 = EDGE_CURVE ( 'NONE', #65006, #86000, #14484, .T. ) ;
#21939 = DIRECTION ( 'NONE',  ( -0.000000000000000000, -0.000000000000000000, 1.000000000000000000 ) ) ;
#21940 = CARTESIAN_POINT ( 'NONE',  ( 190.8957779480239765, 300.0058089740729770, -4.541438514207768229 ) ) ;
#21941 = CARTESIAN_POINT ( 'NONE',  ( 81.78504375891562006, 41.48292696562021575, -5.073134180756075473 ) ) ;
#21942 = CARTESIAN_POINT ( 'NONE',  ( 51.80235952159636525, 85.00000000000000000, 59.99999999999999289 ) ) ;
#21943 = CARTESIAN_POINT ( 'NONE',  ( 164.2897805489690768, 249.8104079013010335, 11.36607573508163505 ) ) ;
#21944 = ADVANCED_FACE ( 'NONE', ( #37981 ), #37490, .F. ) ;
#21945 = CARTESIAN_POINT ( 'NONE',  ( 99.01965388075031171, 234.6427522451419065, -10.00000000000009415 ) ) ;
#21946 = ORIENTED_EDGE ( 'NONE', *, *, #9052, .F. ) ;
#21947 = CARTESIAN_POINT ( 'NONE',  ( 78.94155721643031143, 59.44305089757029492, -16.52414004995256036 ) ) ;
#21948 = ADVANCED_FACE ( 'NONE', ( #78017 ), #92258, .F. ) ;
#21949 = CARTESIAN_POINT ( 'NONE',  ( 202.8499463704053198, 279.3005819042728604, 17.04674939340617001 ) ) ;
#21950 = CARTESIAN_POINT ( 'NONE',  ( 163.2000388741132895, 247.9762362032568035, -11.19676374274550312 ) ) ;
#21952 = EDGE_CURVE ( 'NONE', #59274, #80346, #73700, .T. ) ;
#21951 = AXIS2_PLACEMENT_3D ( 'NONE', #66789, #96742, #97715 ) ;
#21953 = CARTESIAN_POINT ( 'NONE',  ( 13.97758990260114231, 185.0024278399160949, 9.188101187500095079 ) ) ;
#21954 = CARTESIAN_POINT ( 'NONE',  ( 68.24462126014344676, 68.81508646265615425, -6.863557568287563804 ) ) ;
#21955 = CARTESIAN_POINT ( 'NONE',  ( -16.48692306231661320, 105.6553858747601424, 44.28718864051150206 ) ) ;
#21956 = CARTESIAN_POINT ( 'NONE',  ( 71.77078610818966808, 59.27153383271750897, -15.30389425934728642 ) ) ;
#21957 = CARTESIAN_POINT ( 'NONE',  ( 73.26476404075305027, 69.81404936883070889, 9.109525140469814986 ) ) ;
#21958 = EDGE_CURVE ( 'NONE', #93932, #43017, #49298, .T. ) ;
#21960 = CARTESIAN_POINT ( 'NONE',  ( 59.20026718252854891, 214.1744531367911293, 4.594050593750047540 ) ) ;
#21959 = CARTESIAN_POINT ( 'NONE',  ( 174.0404940119542232, 287.4816634783161930, 10.83703146888826119 ) ) ;
#21961 = CARTESIAN_POINT ( 'NONE',  ( 207.5583741822599393, 271.1453457103705205, 3.140867606700001424 ) ) ;
#21962 = CARTESIAN_POINT ( 'NONE',  ( 73.76061769417498226, 55.25278673652109518, 16.11964219720597669 ) ) ;
#21963 = DIRECTION ( 'NONE',  ( -0.9932214622066116716, 0.1162373735601425623, 0.000000000000000000 ) ) ;
#21964 = CARTESIAN_POINT ( 'NONE',  ( 66.09818052648262210, 68.58602539020668587, -4.455928803003319061 ) ) ;
#21965 = ORIENTED_EDGE ( 'NONE', *, *, #50546, .T. ) ;
#21966 = CONICAL_SURFACE ( 'NONE', #93154, 2.749999999999999112, 0.7853981633974463916 ) ;
#21967 = CARTESIAN_POINT ( 'NONE',  ( 11.35262394703597977, 187.3615022471903160, 5.000000000000046185 ) ) ;
#21968 = CARTESIAN_POINT ( 'NONE',  ( 163.7595992360150490, 247.0070492265414828, -6.976205010573520049 ) ) ;
#21969 = CARTESIAN_POINT ( 'NONE',  ( 143.3676317564762144, 244.3923013555409511, 4.594050593750050204 ) ) ;
#21970 = CARTESIAN_POINT ( 'NONE',  ( 19.41443888993109823, 32.18502408145592852, 5.678558825948277544 ) ) ;
#21971 = CARTESIAN_POINT ( 'NONE',  ( 207.2934053853322780, 271.6042851290696376, -8.345259833563044793 ) ) ;
#21972 = CARTESIAN_POINT ( 'NONE',  ( 83.48909022670937929, 51.62989903239390088, -14.87641496889664694 ) ) ;
#21973 = CARTESIAN_POINT ( 'NONE',  ( 177.0253895856008057, 252.4355161662766420, -0.1804300260461335903 ) ) ;
#21975 = CARTESIAN_POINT ( 'NONE',  ( 74.65263117529048031, 66.98225998262294922, 13.00178404275292543 ) ) ;
#21974 = CARTESIAN_POINT ( 'NONE',  ( 69.98840988044214839, 70.01348391617253242, 6.516657591370888625 ) ) ;
#21976 = CARTESIAN_POINT ( 'NONE',  ( 166.8083734521890449, 257.5796782931630560, -15.79284703031436798 ) ) ;
#21977 = ORIENTED_EDGE ( 'NONE', *, *, #30850, .T. ) ;
#21978 = CARTESIAN_POINT ( 'NONE',  ( 73.27328646083023500, 70.16270934360544231, -9.274526489422585840 ) ) ;
#21979 = CARTESIAN_POINT ( 'NONE',  ( 151.9862327556172943, 268.5453780521097542, -15.09052660903973120 ) ) ;
#21980 = CARTESIAN_POINT ( 'NONE',  ( 156.4002494452255689, 280.4459135353391730, -5.478302318053954956 ) ) ;
#21981 = CARTESIAN_POINT ( 'NONE',  ( 195.9583358019009722, 272.3999277485804669, -13.38286462214372108 ) ) ;
#21982 = ORIENTED_EDGE ( 'NONE', *, *, #76769, .F. ) ;
#21983 = CARTESIAN_POINT ( 'NONE',  ( 160.1500473090515584, 253.2589765566000608, 16.19674609738075333 ) ) ;
#21984 = CARTESIAN_POINT ( 'NONE',  ( 171.3259067627017487, 284.4620142900025712, -11.36310073225868500 ) ) ;
#21985 = AXIS2_PLACEMENT_3D ( 'NONE', #30272, #45950, #44464 ) ;
#21986 = AXIS2_PLACEMENT_3D ( 'NONE', #48510, #71318, #25715 ) ;
#21987 = CARTESIAN_POINT ( 'NONE',  ( -3.216670782107629911, 25.02209300385173663, 177.5919119679930134 ) ) ;
#21988 = DIRECTION ( 'NONE',  ( 0.5102188382608533468, -0.8600446134263880493, 0.000000000000000000 ) ) ;
#21989 = CIRCLE ( 'NONE', #33350, 70.00000000000001421 ) ;
#21990 = CARTESIAN_POINT ( 'NONE',  ( 149.7799119457360177, 272.8289483412673917, 11.37468589474485903 ) ) ;
#21991 = CARTESIAN_POINT ( 'NONE',  ( 137.7719789713245291, 261.8967562850346553, -4.648177544792955347E-16 ) ) ;
#21992 = CARTESIAN_POINT ( 'NONE',  ( 201.1060504099706350, 282.3210983108598384, -18.18000168485860257 ) ) ;
#21993 = CARTESIAN_POINT ( 'NONE',  ( 97.10949284993499475, 215.3262482093457493, 3.021315404115420679E-15 ) ) ;
#21994 = CARTESIAN_POINT ( 'NONE',  ( 18.70427805463205573, 12.92755873383625520, 6.180339887498953466 ) ) ;
#21995 = CARTESIAN_POINT ( 'NONE',  ( 191.9204824329850396, 287.7260408795398234, -15.99984276108531311 ) ) ;
#21996 = ORIENTED_EDGE ( 'NONE', *, *, #70149, .T. ) ;
#21997 = CARTESIAN_POINT ( 'NONE',  ( 148.9517569034208009, 272.6549844970639924, 12.50737104496728236 ) ) ;
#21998 = DIRECTION ( 'NONE',  ( 0.4999999999999998890, -0.8660254037844385966, 0.000000000000000000 ) ) ;
#21999 = CARTESIAN_POINT ( 'NONE',  ( 82.72443436000141048, 45.32069663430784345, -10.30851497045541088 ) ) ;
#22000 = EDGE_CURVE ( 'NONE', #5671, #32845, #46391, .T. ) ;
#22001 = VERTEX_POINT ( 'NONE', #17 ) ;
#22002 = CARTESIAN_POINT ( 'NONE',  ( 191.0862225170008628, 299.6759493045793192, -9.402218231374108726 ) ) ;
#22003 = CARTESIAN_POINT ( 'NONE',  ( 183.8973593476267752, 262.2032069668072722, -12.40570899861645771 ) ) ;
#22004 = CARTESIAN_POINT ( 'NONE',  ( 163.8003088823192286, 260.8948240748503054, -17.39314492925268141 ) ) ;
#22005 = CARTESIAN_POINT ( 'NONE',  ( 21.40066741106990378, 12.75978393459163840, -1.583844403245362020 ) ) ;
#22006 = ORIENTED_EDGE ( 'NONE', *, *, #21354, .F. ) ;
#22007 = CARTESIAN_POINT ( 'NONE',  ( 99.71410487726059557, 234.5024278399160949, 9.188101187500095079 ) ) ;
#22008 = CARTESIAN_POINT ( 'NONE',  ( 203.0794350760556028, 278.9030958063233925, 15.06053680683988638 ) ) ;
#22009 = CARTESIAN_POINT ( 'NONE',  ( 82.06353261700769508, 41.00057011406286733, -2.892018250819532454 ) ) ;
#22010 = CARTESIAN_POINT ( 'NONE',  ( 179.8103815483993344, 270.2768680805289705, -16.04546734559231780 ) ) ;
#22011 = CARTESIAN_POINT ( 'NONE',  ( 81.35301008429968306, 42.53188570201726293, -7.664210345353390075 ) ) ;
#22012 = EDGE_LOOP ( 'NONE', ( #56943, #54006, #55145, #65409 ) ) ;
#22013 = ORIENTED_EDGE ( 'NONE', *, *, #1628, .T. ) ;
#22014 = VERTEX_POINT ( 'NONE', #61790 ) ;
#22015 = DIRECTION ( 'NONE',  ( 0.4999999999999998890, -0.8660254037844385966, 0.000000000000000000 ) ) ;
#22016 = ORIENTED_EDGE ( 'NONE', *, *, #87191, .T. ) ;
#22017 = CARTESIAN_POINT ( 'NONE',  ( 71.63453813518020752, 72.07236434383467838, 0.7172108931481352423 ) ) ;
#22018 = ORIENTED_EDGE ( 'NONE', *, *, #95774, .T. ) ;
#22019 = FACE_OUTER_BOUND ( 'NONE', #57255, .T. ) ;
#22020 = FACE_OUTER_BOUND ( 'NONE', #67216, .T. ) ;
#22021 = CARTESIAN_POINT ( 'NONE',  ( 48.74043828842092552, 100.0309547576005258, 10.00000000000000000 ) ) ;
#22022 = ADVANCED_FACE ( 'NONE', ( #92736 ), #23290, .T. ) ;
#22023 = CARTESIAN_POINT ( 'NONE',  ( 82.75425455800102270, 53.83811729049745054, -15.80404254388376906 ) ) ;
#22024 = ORIENTED_EDGE ( 'NONE', *, *, #5473, .F. ) ;
#22025 = CARTESIAN_POINT ( 'NONE',  ( 76.15254952159935442, 56.95550950617717945, 16.13614341295277654 ) ) ;
#22026 = CARTESIAN_POINT ( 'NONE',  ( 11.81506597172265316, 27.79752408145591502, -5.678558825948271327 ) ) ;
#22027 = DIRECTION ( 'NONE',  ( -0.4999999999999995004, 0.8660254037844389297, -1.249000902703319567E-14 ) ) ;
#22028 = CARTESIAN_POINT ( 'NONE',  ( 85.64302380165412387, 48.93088599686250006, 12.15651094663528653 ) ) ;
#22030 = ORIENTED_EDGE ( 'NONE', *, *, #899, .T. ) ;
#22029 = CARTESIAN_POINT ( 'NONE',  ( 9.120852146362338431, 187.6199935810941213, 2.679491924311251605 ) ) ;
#22031 = AXIS2_PLACEMENT_3D ( 'NONE', #94095, #86021, #40829 ) ;
#22032 = CARTESIAN_POINT ( 'NONE',  ( -16.76269525828470464, 104.4383445782105042, 12.56748295067274945 ) ) ;
#22033 = CARTESIAN_POINT ( 'NONE',  ( 200.0411626275569574, 270.6720010161316736, -11.59284015024147152 ) ) ;
#22034 = DIRECTION ( 'NONE',  ( -0.5632146860273805622, 0.8263106059122556912, 0.000000000000000000 ) ) ;
#22035 = CARTESIAN_POINT ( 'NONE',  ( 161.3440642087019796, 281.4507293028746062, -6.554503167351243498 ) ) ;
#22036 = ADVANCED_FACE ( 'NONE', ( #91741 ), #15691, .F. ) ;
#22037 = CARTESIAN_POINT ( 'NONE',  ( 77.38507280294756185, 49.73636053508898414, -15.49715387554307355 ) ) ;
#22038 = AXIS2_PLACEMENT_3D ( 'NONE', #74426, #88665, #73414 ) ;
#22039 = CARTESIAN_POINT ( 'NONE',  ( 192.6527964471240750, 292.3325994180497105, -14.38016747683365359 ) ) ;
#22040 = EDGE_CURVE ( 'NONE', #89848, #16529, #8114, .T. ) ;
#22041 = CARTESIAN_POINT ( 'NONE',  ( 168.3057934360732588, 253.3915715900249097, 11.59359703697476718 ) ) ;
#22042 = CARTESIAN_POINT ( 'NONE',  ( 194.2039773765081350, 263.4403579747535105, -0.7712302936324405556 ) ) ;
#22043 = VERTEX_POINT ( 'NONE', #31394 ) ;
#22044 = CARTESIAN_POINT ( 'NONE',  ( 155.6732402535458846, 261.0130338324187846, -18.36886937783899043 ) ) ;
#22045 = CARTESIAN_POINT ( 'NONE',  ( 43.54657591670569872, 62.36930841191391295, -10.00000000000000000 ) ) ;
#22046 = CARTESIAN_POINT ( 'NONE',  ( 6.427104459464150210, 164.5177522451418213, 5.000000000000051514 ) ) ;
#22047 = CARTESIAN_POINT ( 'NONE',  ( 82.72380189249818727, 53.29157908679620448, -15.28871581714063588 ) ) ;
#22048 = CARTESIAN_POINT ( 'NONE',  ( 172.5784562716271466, 280.0954662991010196, -14.34707186603650442 ) ) ;
#22049 = CARTESIAN_POINT ( 'NONE',  ( 163.3366259987258786, 247.7396603637682801, -8.236665301808596240 ) ) ;
#22050 = CARTESIAN_POINT ( 'NONE',  ( 72.13188387548123615, 72.33286681718249156, 1.023135554637200961 ) ) ;
#22051 = CARTESIAN_POINT ( 'NONE',  ( 72.76085654771455324, 70.95487523876634839, 7.692118034595658571 ) ) ;
#22053 = CARTESIAN_POINT ( 'NONE',  ( 87.78081971166569986, 44.10618430004835488, 2.676874261813569245 ) ) ;
#22052 = CARTESIAN_POINT ( 'NONE',  ( -14.30363896367569509, 171.7369531367911293, -4.594050593750048428 ) ) ;
#22054 = CARTESIAN_POINT ( 'NONE',  ( 186.5421728102579948, 295.6688228412515969, 8.171192122117640011 ) ) ;
#22055 = VERTEX_POINT ( 'NONE', #62281 ) ;
#22056 = AXIS2_PLACEMENT_3D ( 'NONE', #16178, #55650, #8585 ) ;
#22057 = ORIENTED_EDGE ( 'NONE', *, *, #71081, .F. ) ;
#22058 = CARTESIAN_POINT ( 'NONE',  ( -19.65312891409030271, 93.06504152958497400, 10.00000000000000888 ) ) ;
#22059 = CARTESIAN_POINT ( 'NONE',  ( 38.04107491472452551, 53.42442038713602415, 10.00000000000000000 ) ) ;
#22060 = B_SPLINE_CURVE_WITH_KNOTS ( 'NONE', 3,
 ( #37679, #69087, #62992, #31575, #70586, #7798, #16391, #38683, #47282, #1200, #46268, #15883, #78207, #55370, #24491, #93433, #54884, #39165, #196, #77191, #100013, #14407, #30598, #61484 ),
 .UNSPECIFIED., .F., .F.,
 ( 4, 2, 2, 2, 2, 2, 2, 2, 2, 2, 2, 4 ),
 ( 0.000000000000000000, 0.1250000000000018596, 0.2500000000000037192, 0.3750000000000055511, 0.4375000000000049405, 0.5000000000000043299, 0.5625000000000036637, 0.6250000000000031086, 0.6875000000000024425, 0.7500000000000017764, 0.8750000000000008882, 1.000000000000000000 ),
 .UNSPECIFIED. ) ;
#22061 = CARTESIAN_POINT ( 'NONE',  ( 175.0451609275794453, 292.0163007842869547, 3.353226643629469539 ) ) ;
#22062 = CIRCLE ( 'NONE', #20494, 0.1418229129681565781 ) ;
#22063 = CARTESIAN_POINT ( 'NONE',  ( -22.42236680055709641, 157.8615022471902591, 0.000000000000000000 ) ) ;
#22064 = CARTESIAN_POINT ( 'NONE',  ( 202.0385627042762451, 280.7059396384401566, -16.09405805615697460 ) ) ;
#22065 =( BOUNDED_CURVE ( )  B_SPLINE_CURVE ( 2, ( #42228, #10357, #26056, #72165, #18966, #3271, #10858, #26556, #41733 ),
 .UNSPECIFIED., .F., .T. ) 
 B_SPLINE_CURVE_WITH_KNOTS ( ( 3, 2, 2, 2, 3 ),
 ( 0.3669354838709677491, 0.3682795698924731242, 0.3709677419354838745, 0.3736559139784946248, 0.3750000000000000000 ),
 .UNSPECIFIED. ) 
 CURVE ( )  GEOMETRIC_REPRESENTATION_ITEM ( )  RATIONAL_B_SPLINE_CURVE ( ( 0.9330127018922194093, 0.9330127018922194093, 1.000000000000000000, 0.8660254037844387076, 1.000000000000000000, 0.8660254037844387076, 1.000000000000000000, 0.9330127018922194093, 0.9330127018922194093 ) ) 
 REPRESENTATION_ITEM ( '' )  );
#22066 = CARTESIAN_POINT ( 'NONE',  ( 70.97982842658589675, 70.74070771080400277, 6.159771955551562428 ) ) ;
#22067 = CARTESIAN_POINT ( 'NONE',  ( 151.5010811193459119, 277.2876517059261232, 3.696019110083865300 ) ) ;
#22069 = EDGE_CURVE ( 'NONE', #57260, #42456, #50712, .T. ) ;
#22068 = B_SPLINE_CURVE_WITH_KNOTS ( 'NONE', 3,
 ( #87940, #56463, #72703, #9890, #25061, #94505, #33682, #3296, #96017, #56954, #2290, #33167, #2799, #63564, #95015, #40748, #32665, #18484, #64071, #17466, #64578, #57454, #3779, #25577, #88433, #42741, #95532, #49369, #73187, #80313, #81314, #10881, #65067, #87454, #41758, #55937, #71693, #86936, #34175, #48880, #17987, #26579, #48376, #18993, #79322, #49865 ),
 .UNSPECIFIED., .F., .F.,
 ( 4, 1, 1, 1, 2, 2, 1, 1, 1, 2, 2, 1, 1, 2, 2, 1, 1, 2, 2, 1, 1, 2, 2, 1, 2, 2, 1, 2, 2, 4 ),
 ( 0.000000000000000000, 0.06249999999999646116, 0.09374999999999453215, 0.1093749999999932415, 0.1171874999999931027, 0.1249999999999929778, 0.1874999999999940326, 0.2187499999999960587, 0.2343749999999957256, 0.2421874999999963363, 0.2499999999999969469, 0.3124999999999927280, 0.3437499999999900635, 0.3593749999999887312, 0.3749999999999873990, 0.4374999999999868994, 0.4687499999999858447, 0.4843749999999845679, 0.4999999999999832356, 0.5624999999999802380, 0.5937499999999784617, 0.6093749999999783507, 0.6249999999999782396, 0.6874999999999817923, 0.7187499999999836797, 0.7499999999999855671, 0.8124999999999887867, 0.8437499999999908962, 0.8749999999999930056, 1.000000000000000000 ),
 .UNSPECIFIED. ) ;
#22070 = CARTESIAN_POINT ( 'NONE',  ( 14.24839638916628459, 179.0333772461660544, 9.188101187500095079 ) ) ;
#22071 = CARTESIAN_POINT ( 'NONE',  ( 112.6505328941731108, 235.8458772461660544, 9.188101187500095079 ) ) ;
#22072 = CARTESIAN_POINT ( 'NONE',  ( 181.2594824857899312, 293.4632464574068536, -6.243252836990251353 ) ) ;
#22073 = LINE ( 'NONE', #68166, #96515 ) ;
#22074 = CARTESIAN_POINT ( 'NONE',  ( 206.1823507212516802, 271.5286882572439140, -8.119960357998227352 ) ) ;
#22075 = ADVANCED_FACE ( 'NONE', ( #70397 ), #45104, .F. ) ;
#22076 = DIRECTION ( 'NONE',  ( -0.3940053768033626169, 0.6824373310787468228, 0.6156614753256509642 ) ) ;
#22077 = CARTESIAN_POINT ( 'NONE',  ( 80.28770547203146180, 53.50931822275166638, -15.65279642959144901 ) ) ;
#22078 = DIRECTION ( 'NONE',  ( -1.000000000000000000, 0.000000000000000000, 0.000000000000000000 ) ) ;
#22079 = CARTESIAN_POINT ( 'NONE',  ( 184.4178076012347276, 274.3843162572107985, 17.30722352241574313 ) ) ;
#22080 = CARTESIAN_POINT ( 'NONE',  ( 190.1225270613304588, 284.8508451989043806, 16.94479376615364075 ) ) ;
#22081 = ADVANCED_FACE ( 'NONE', ( #48096 ), #2521, .T. ) ;
#22082 = CARTESIAN_POINT ( 'NONE',  ( 170.8677527226213044, 279.5558645822755466, 13.90315963116175446 ) ) ;
#22083 = CARTESIAN_POINT ( 'NONE',  ( 192.5651576355940051, 265.2377806318704643, 7.853493163364257512 ) ) ;
#22084 = CARTESIAN_POINT ( 'NONE',  ( 68.07050364499654904, 67.45021790136736684, 7.977111741387843402 ) ) ;
#22085 = B_SPLINE_CURVE_WITH_KNOTS ( 'NONE', 3,
 ( #57110, #51516, #45884, #60591 ),
 .UNSPECIFIED., .F., .F.,
 ( 4, 4 ),
 ( 0.008178853229217460802, 0.01408825881594157406 ),
 .UNSPECIFIED. ) ;
#22086 = CARTESIAN_POINT ( 'NONE',  ( 18.26047324907200675, 192.8967562850347122, -4.648177544792955347E-16 ) ) ;
#22087 = FACE_OUTER_BOUND ( 'NONE', #19813, .T. ) ;
#22088 = CARTESIAN_POINT ( 'NONE',  ( 92.46148921633090367, 218.0643266524160140, 9.188101187500095079 ) ) ;
#22089 = CARTESIAN_POINT ( 'NONE',  ( 11.99789328850488879, 15.43085787977761569, -9.188101187500008038 ) ) ;
#22090 = CARTESIAN_POINT ( 'NONE',  ( 191.2645787786270262, 299.3670271975948367, 7.309947121636420242 ) ) ;
#22091 = CARTESIAN_POINT ( 'NONE',  ( 84.99999999999997158, 27.49999999999999645, 59.99999999999999289 ) ) ;
#22093 = CARTESIAN_POINT ( 'NONE',  ( 152.2297789851355105, 266.9772837032011807, 16.97658142831851080 ) ) ;
#22092 = CARTESIAN_POINT ( 'NONE',  ( 157.3363371328520088, 258.1324655395517311, 18.24585617226787093 ) ) ;
#22094 = CARTESIAN_POINT ( 'NONE',  ( 149.0866298612203593, 272.4213776815879555, 12.86424381646844495 ) ) ;
#22095 = DIRECTION ( 'NONE',  ( -0.8660254037844378194, -0.5000000000000014433, -0.000000000000000000 ) ) ;
#22096 = DIRECTION ( 'NONE',  ( 0.000000000000000000, 0.000000000000000000, 1.000000000000000000 ) ) ;
#22097 = AXIS2_PLACEMENT_3D ( 'NONE', #42793, #58502, #28607 ) ;
#22098 = CARTESIAN_POINT ( 'NONE',  ( 35.00289615805098009, 41.18502408145595695, 5.678558825948276656 ) ) ;
#22099 = CARTESIAN_POINT ( 'NONE',  ( 192.6247335881259630, 297.0111699613833594, -13.30158778996737290 ) ) ;
#22100 = CARTESIAN_POINT ( 'NONE',  ( 169.5727729373952002, 284.0798650663272156, -11.84966624384599676 ) ) ;
#22101 = EDGE_LOOP ( 'NONE', ( #83359, #5559, #22514, #75653 ) ) ;
#22102 = CARTESIAN_POINT ( 'NONE',  ( 32.30976433484754295, 19.44966523072496045, -2.296566073217252530E-15 ) ) ;
#22103 = CARTESIAN_POINT ( 'NONE',  ( 48.05801951159152452, 75.31115804243518141, 10.00000000000000000 ) ) ;
#22104 = AXIS2_PLACEMENT_3D ( 'NONE', #68748, #29272, #15041 ) ;
#22105 = CARTESIAN_POINT ( 'NONE',  ( 147.1034852426517148, 275.8562849197056153, -3.648177088342072327 ) ) ;
#22106 = CARTESIAN_POINT ( 'NONE',  ( 149.3253462891332219, 272.0079086998416074, -12.99539319630191336 ) ) ;
#22107 = B_SPLINE_CURVE_WITH_KNOTS ( 'NONE', 3,
 ( #53421, #54919, #62003, #13941 ),
 .UNSPECIFIED., .F., .F.,
 ( 4, 4 ),
 ( 0.002635550454916707128, 0.01057756139833311744 ),
 .UNSPECIFIED. ) ;
#22108 = ORIENTED_EDGE ( 'NONE', *, *, #16276, .F. ) ;
#22109 = B_SPLINE_SURFACE_WITH_KNOTS ( 'NONE', 3, 1, ( 
 ( #29045, #75149 ),
 ( #75637, #59915 ),
 ( #76156, #5727 ),
 ( #36615, #66535 ),
 ( #90885, #6223 ),
 ( #37608, #83261 ),
 ( #29531, #20449 ),
 ( #51319, #52811 ),
 ( #68520, #50826 ),
 ( #74158, #74662 ),
 ( #5239, #7720 ),
 ( #15299, #39595 ),
 ( #62917, #91867 ),
 ( #31014, #53799 ),
 ( #23913, #1645 ),
 ( #38098, #54813 ),
 ( #55300, #84762 ),
 ( #22424, #62401 ),
 ( #92365, #22912 ),
 ( #71042, #70010 ),
 ( #46199, #85790 ),
 ( #61904, #40101 ),
 ( #86280, #47703 ),
 ( #16322, #625 ),
 ( #99939, #131 ),
 ( #14817, #77115 ),
 ( #54296, #23407 ),
 ( #93356, #47214 ),
 ( #60904, #69009 ),
 ( #53315, #16816 ),
 ( #61411, #84271 ),
 ( #38612, #45704 ),
 ( #69516, #30522 ),
 ( #92854, #78641 ) ),
 .UNSPECIFIED., .T., .F., .F.,
 ( 4, 2, 2, 2, 2, 2, 2, 2, 2, 2, 2, 2, 2, 2, 2, 2, 4 ),
 ( 2, 2 ),
 ( 0.000000000000000000, 0.06250000000000000000, 0.1250000000000000000, 0.1875000000000000000, 0.2500000000000000000, 0.3125000000000000000, 0.3750000000000000000, 0.4375000000000000000, 0.5000000000000000000, 0.5625000000000000000, 0.6250000000000000000, 0.6875000000000000000, 0.7500000000000000000, 0.8125000000000000000, 0.8750000000000000000, 0.9375000000000000000, 1.000000000000000000 ),
 ( 0.000000000000000000, 1.000000000000000000 ),
 .UNSPECIFIED. ) ;
#22110 = AXIS2_PLACEMENT_3D ( 'NONE', #45640, #82723, #91298 ) ;
#22111 = CARTESIAN_POINT ( 'NONE',  ( 70.76739923968082735, 60.93592591164377126, 15.04188609397093757 ) ) ;
#22112 = CARTESIAN_POINT ( 'NONE',  ( 159.9628729326222754, 253.5831720864507588, 15.75051413866357386 ) ) ;
#22113 = CARTESIAN_POINT ( 'NONE',  ( 179.8897980908058116, 262.7712755250011014, -12.78868501294826565 ) ) ;
#22114 = CARTESIAN_POINT ( 'NONE',  ( 172.8210543149999978, 253.0650713199155177, -9.347212986753337560 ) ) ;
#22115 = CARTESIAN_POINT ( 'NONE',  ( 174.5899361521156266, 284.9381008987350583, -13.57821407317514684 ) ) ;
#22116 = B_SPLINE_CURVE_WITH_KNOTS ( 'NONE', 3,
 ( #21774, #61260, #7069, #29387, #98300, #92230, #37954, #23259, #14186, #36972, #22781, #28889, #92709, #52664, #99787, #59766, #53657, #85110, #60255, #83618, #15154, #38458, #91711, #76968, #53177, #15661, #46556, #22273, #77491, #76010, #52167, #8085, #7568, #37459, #69372, #100291, #84132, #68862, #30875, #61761 ),
 .UNSPECIFIED., .F., .F.,
 ( 4, 2, 2, 2, 2, 2, 2, 2, 2, 2, 2, 2, 2, 2, 2, 2, 2, 2, 2, 4 ),
 ( 0.003508113122471474138, 0.003679226956315371794, 0.003764783873237320406, 0.003850340790159269451, 0.004021454624003175347, 0.004192568457847080376, 0.004534796125534887833, 0.004877023793222695289, 0.006245934463974074299, 0.007614845134725453310, 0.007957072802413343166, 0.008128186636257288961, 0.008213743553179261858, 0.008299300470101233021, 0.008320689699331723643, 0.008342078928562212531, 0.008384857387023216327, 0.008470414303945223919, 0.008641528137789279002, 0.008983755805477347534 ),
 .UNSPECIFIED. ) ;
#22117 = ORIENTED_EDGE ( 'NONE', *, *, #90029, .T. ) ;
#22118 = CARTESIAN_POINT ( 'NONE',  ( 187.3434644620873257, 278.8535086450150402, 17.53040139197816671 ) ) ;
#22119 = EDGE_LOOP ( 'NONE', ( #80480, #46773, #30457, #21245 ) ) ;
#22120 = CARTESIAN_POINT ( 'NONE',  ( 78.31186438638634684, 61.61641173835174357, 16.15355831358047567 ) ) ;
#22121 = EDGE_CURVE ( 'NONE', #29087, #7931, #5850, .T. ) ;
#22122 = CARTESIAN_POINT ( 'NONE',  ( 185.3111611773075253, 292.6075343283709458, -10.66299757420777183 ) ) ;
#22123 = ORIENTED_EDGE ( 'NONE', *, *, #23692, .F. ) ;
#22124 = CARTESIAN_POINT ( 'NONE',  ( 39.93146227192245590, 203.8615022471903160, 5.000000000000046185 ) ) ;
#22125 = CARTESIAN_POINT ( 'NONE',  ( -34.46923751714648887, 63.31602547000201042, -10.00000000000000000 ) ) ;
#22126 = CARTESIAN_POINT ( 'NONE',  ( 190.5639199208830803, 278.8100509870810129, -16.51443528190589305 ) ) ;
#22127 = CARTESIAN_POINT ( 'NONE',  ( 193.0564854987053707, 296.2633537159950379, -12.03146446119285429 ) ) ;
#22128 = CARTESIAN_POINT ( 'NONE',  ( 200.6737073311291795, 283.0699384897140476, -17.61533935526990291 ) ) ;
#22129 = DIRECTION ( 'NONE',  ( -0.5864613938488684175, 0.8099771808667466377, 0.000000000000000000 ) ) ;
#22130 = VECTOR ( 'NONE', #24438, 1000.000000000000000 ) ;
#22131 = CARTESIAN_POINT ( 'NONE',  ( 32.59967566254915994, 39.79752408145595410, -5.678558825948271327 ) ) ;
#22132 = AXIS2_PLACEMENT_3D ( 'NONE', #16806, #94350, #32518 ) ;
#22133 = CARTESIAN_POINT ( 'NONE',  ( 81.44589832458051148, 55.42546683620729908, -16.32034488869437538 ) ) ;
#22134 = CARTESIAN_POINT ( 'NONE',  ( 75.79717256834328509, 62.26676178855290544, -15.60790356137264823 ) ) ;
#22135 = CARTESIAN_POINT ( 'NONE',  ( 71.18054559181101126, 205.2365022471902023, 10.00000000000009948 ) ) ;
#22136 = AXIS2_PLACEMENT_3D ( 'NONE', #41984, #42955, #81045 ) ;
#22137 = B_SPLINE_CURVE_WITH_KNOTS ( 'NONE', 3,
 ( #99156, #21168, #54014, #67241 ),
 .UNSPECIFIED., .F., .F.,
 ( 4, 4 ),
 ( 0.000000000000000000, 0.005815978540402074078 ),
 .UNSPECIFIED. ) ;
#22138 = ORIENTED_EDGE ( 'NONE', *, *, #85187, .T. ) ;
#22139 = VERTEX_POINT ( 'NONE', #78521 ) ;
#22140 = CARTESIAN_POINT ( 'NONE',  ( 204.9463377925012253, 275.6695254486514841, -14.15865086131798378 ) ) ;
#22141 = CARTESIAN_POINT ( 'NONE',  ( 169.3729277929404020, 269.0884521908612328, 17.29306383018335680 ) ) ;
#22143 = DIRECTION ( 'NONE',  ( -0.9981117208278915687, 0.06142469166373833167, 0.000000000000000000 ) ) ;
#22142 = DIRECTION ( 'NONE',  ( -0.9919422576440838357, -0.1266907948509198578, 0.000000000000000000 ) ) ;
#22144 = CARTESIAN_POINT ( 'NONE',  ( 177.3799066019990676, 269.9615352214298127, -17.60161419056240817 ) ) ;
#22145 = CARTESIAN_POINT ( 'NONE',  ( 197.4575405150459915, 273.2519002803542207, -13.37676461630871216 ) ) ;
#22146 = CARTESIAN_POINT ( 'NONE',  ( 72.31909173678994307, 61.61524097631632912, -14.63572028674620817 ) ) ;
#22147 = CARTESIAN_POINT ( 'NONE',  ( 147.7870527676176948, 274.6723112360602386, 9.257357958194809555 ) ) ;
#22148 = CARTESIAN_POINT ( 'NONE',  ( 167.1357220015965481, 286.2500965088896692, -4.817194026439638677 ) ) ;
#22149 = CARTESIAN_POINT ( 'NONE',  ( 76.88818783305237048, 63.31965297372375545, -15.46890590930648912 ) ) ;
#22150 = CARTESIAN_POINT ( 'NONE',  ( 186.5810050528308182, 287.0653887321775528, -16.02633163178817810 ) ) ;
#22151 = B_SPLINE_CURVE_WITH_KNOTS ( 'NONE', 3,
 ( #90101, #96207, #10577, #28255, #89618, #41964, #20180, #4462, #34848, #65753, #34366, #50550, #88133, #3003, #72393, #11586, #81506, #73871, #96705, #80513, #11088, #18679, #4978, #51559, #66753, #58641, #72900, #20669, #27274, #35858, #35359, #82005, #3491, #66268, #41452, #73380, #58157, #51046, #42444, #59129, #89138, #12074, #3966, #65264, #33894, #57652, #64779, #42932, #19689, #26770 ),
 .UNSPECIFIED., .F., .F.,
 ( 4, 2, 2, 2, 2, 2, 2, 2, 2, 2, 2, 2, 2, 2, 2, 2, 2, 2, 2, 2, 2, 2, 2, 2, 4 ),
 ( 0.0003075647970707622828, 0.0007717470533795799809, 0.001235929309688397733, 0.001468020437842779179, 0.001584066001920029967, 0.001700111565997280971, 0.001816157130074532193, 0.001932202694151782980, 0.002164293822306383435, 0.002628476078615583043, 0.003092658334924782652, 0.004021022847543170159, 0.004949387360161558100, 0.005413569616470791969, 0.005645660744625372908, 0.005761706308702621744, 0.005877751872779870580, 0.005935774654818462906, 0.005993797436857055232, 0.006109843000934376059, 0.006341934129088985621, 0.006806116385398164846, 0.007270298641707344939, 0.007502389769861964909, 0.007734480898016584879 ),
 .UNSPECIFIED. ) ;
#22152 = CARTESIAN_POINT ( 'NONE',  ( 111.8659576938172364, 226.2048013555410080, 4.594050593750051981 ) ) ;
#22153 = ORIENTED_EDGE ( 'NONE', *, *, #70166, .F. ) ;
#22155 = CARTESIAN_POINT ( 'NONE',  ( 46.15481705937101964, 68.45315478587873770, 10.00000000000000000 ) ) ;
#22154 = B_SPLINE_CURVE_WITH_KNOTS ( 'NONE', 3,
 ( #14698, #59278, #83138, #90255, #51722, #29408, #36497, #67400, #60277, #98325, #48087, #38980, #47088, #32887, #17185, #2001, #25288, #78513 ),
 .UNSPECIFIED., .F., .F.,
 ( 4, 2, 2, 2, 2, 2, 2, 2, 4 ),
 ( 0.0002032915482228868484, 0.0005852909360411848042, 0.0006807907829957838977, 0.0007285407064730834445, 0.0007762906299503830997, 0.0008717904769048328987, 0.0009672903238592826976, 0.001349289711677355980, 0.001731289099495429695 ),
 .UNSPECIFIED. ) ;
#22156 = CARTESIAN_POINT ( 'NONE',  ( 39.71190250773520347, 34.87878583063844928, -9.188101187500006262 ) ) ;
#22157 = CARTESIAN_POINT ( 'NONE',  ( 188.1252097491235702, 273.5990210901503019, 15.73037138839605120 ) ) ;
#22158 = ORIENTED_EDGE ( 'NONE', *, *, #16899, .T. ) ;
#22159 = CARTESIAN_POINT ( 'NONE',  ( 86.83317331226271563, 45.77437086576020420, -8.734311406240857778 ) ) ;
#22160 = CARTESIAN_POINT ( 'NONE',  ( 180.3896065631481065, 294.7457813050739901, -1.965667979761724915 ) ) ;
#22161 = CARTESIAN_POINT ( 'NONE',  ( 196.3519702320103590, 290.5554067223432639, 17.39042812051341969 ) ) ;
#22162 = CARTESIAN_POINT ( 'NONE',  ( 206.0870578475358172, 273.6937403561189512, -10.07771901274806581 ) ) ;
#22163 = EDGE_CURVE ( 'NONE', #40778, #69110, #79553, .T. ) ;
#22164 = CARTESIAN_POINT ( 'NONE',  ( 96.65612621980328356, 216.6115022471901739, -5.000000000000041744 ) ) ;
#22165 = VERTEX_POINT ( 'NONE', #3524 ) ;
#22166 = CARTESIAN_POINT ( 'NONE',  ( 194.7295074538898803, 293.3655946874374081, 16.09945624218667959 ) ) ;
#22167 = EDGE_CURVE ( 'NONE', #50903, #65006, #31514, .T. ) ;
#22168 = EDGE_LOOP ( 'NONE', ( #29738, #58287, #86115, #91170 ) ) ;
#22169 = DIRECTION ( 'NONE',  ( 1.000000000000000000, 1.768426674938641735E-13, 0.000000000000000000 ) ) ;
#22170 = VERTEX_POINT ( 'NONE', #25297 ) ;
#22171 = CARTESIAN_POINT ( 'NONE',  ( 206.4229368915142686, 273.1119807867502800, 10.31819530520674810 ) ) ;
#22172 = CARTESIAN_POINT ( 'NONE',  ( 195.7664554078432104, 265.2673286538130810, 4.151641377481578132 ) ) ;
#22173 = CARTESIAN_POINT ( 'NONE',  ( -19.65312891409030271, 93.06504152958497400, 177.5919119679930134 ) ) ;
#22174 = VECTOR ( 'NONE', #88758, 1000.000000000000000 ) ;
#22175 = CARTESIAN_POINT ( 'NONE',  ( 83.96883838543894285, 49.56557209779730755, 13.24582278230334431 ) ) ;
#22177 = CARTESIAN_POINT ( 'NONE',  ( 157.2948870673828026, 280.9759411348209142, 6.053012778684776940 ) ) ;
#22176 = CARTESIAN_POINT ( 'NONE',  ( -19.92236680055706444, 153.5313752282680184, 0.000000000000000000 ) ) ;
#22178 = CARTESIAN_POINT ( 'NONE',  ( 152.7691010214056462, 266.0431505347400503, -16.40662330462167162 ) ) ;
#22179 = VERTEX_POINT ( 'NONE', #11126 ) ;
#22181 = CARTESIAN_POINT ( 'NONE',  ( -64.54732778733693976, 39.35739861417317087, -10.00000000000000000 ) ) ;
#22180 = VECTOR ( 'NONE', #42070, 1000.000000000000114 ) ;
#22182 = CARTESIAN_POINT ( 'NONE',  ( 72.18837429559984287, 65.02575927599113470, 12.81091265492822551 ) ) ;
#22183 = CARTESIAN_POINT ( 'NONE',  ( 190.0998002681485559, 264.3044181240644548, -9.275971950984974512 ) ) ;
#22184 = CARTESIAN_POINT ( 'NONE',  ( 192.3868339392006135, 271.8215131925324499, 14.10193610252311380 ) ) ;
#22185 = CARTESIAN_POINT ( 'NONE',  ( 192.7248895367048362, 271.5377591740219145, -15.00482078990248169 ) ) ;
#22186 = CARTESIAN_POINT ( 'NONE',  ( 72.11463582380375215, 72.32045887020245800, 3.546959094384879219 ) ) ;
#22187 = CARTESIAN_POINT ( 'NONE',  ( 82.81428708694842555, 42.72530104253821293, 6.546892619254078838 ) ) ;
#22188 = CARTESIAN_POINT ( 'NONE',  ( 18.52134341065869805, 22.64441083166260427, -10.00000000000000533 ) ) ;
#22189 = CARTESIAN_POINT ( 'NONE',  ( 24.34300500380255983, 194.8615022471903160, 5.000000000000046185 ) ) ;
#22190 = ADVANCED_FACE ( 'NONE', ( #56184 ), #81536, .T. ) ;
#22191 = CARTESIAN_POINT ( 'NONE',  ( 82.56662147140762897, 53.48431740468424778, -15.73383048919865068 ) ) ;
#22192 = CARTESIAN_POINT ( 'NONE',  ( 71.08131351252005459, 211.8458772461660544, 9.188101187500095079 ) ) ;
#22193 = CARTESIAN_POINT ( 'NONE',  ( 206.6268150440956504, 272.7588534679261443, -10.76664753678610609 ) ) ;
#22194 = CARTESIAN_POINT ( 'NONE',  ( 193.0142717932987182, 296.3364699985351081, -13.30037542329744937 ) ) ;
#22195 = CARTESIAN_POINT ( 'NONE',  ( -27.42236680055714260, 166.5217562850347406, 1.224646799147364892E-15 ) ) ;
#22196 = CARTESIAN_POINT ( 'NONE',  ( 161.8926315922002743, 250.2407320417157166, -13.77020595223768495 ) ) ;
#22197 = CARTESIAN_POINT ( 'NONE',  ( 193.8003511027313550, 288.1208047801705447, 17.19107869180001913 ) ) ;
#22198 = CONICAL_SURFACE ( 'NONE', #93472, 16.82106496071143908, 0.7853981633974241872 ) ;
#22200 = CARTESIAN_POINT ( 'NONE',  ( -20.94588425035955837, 95.10802420503439691, 45.19938068878172288 ) ) ;
#22199 = CARTESIAN_POINT ( 'NONE',  ( 73.29675513422920119, 69.64584746942686877, -9.922798968680028864 ) ) ;
#22201 = CARTESIAN_POINT ( 'NONE',  ( 3.631266576971075910, 20.83478043621385467, -8.090169943749479842 ) ) ;
#22202 = CARTESIAN_POINT ( 'NONE',  ( 188.0605157086127406, 260.5832606518970920, -7.266969944812869286 ) ) ;
#22203 = CARTESIAN_POINT ( 'NONE',  ( 204.9304696503118919, 275.6970098771450353, -13.62097861578000213 ) ) ;
#22204 = CARTESIAN_POINT ( 'NONE',  ( 157.7045020317009403, 270.7409348844154238, -14.98380028358599603 ) ) ;
#22205 = CARTESIAN_POINT ( 'NONE',  ( 72.09275328296196506, 72.05865058278648405, 2.889467875048744805 ) ) ;
#22206 = AXIS2_PLACEMENT_3D ( 'NONE', #7385, #69686, #75322 ) ;
#22207 = CARTESIAN_POINT ( 'NONE',  ( 52.94873307290088604, 207.5024278399160949, 9.188101187500095079 ) ) ;
#22208 = CARTESIAN_POINT ( 'NONE',  ( 157.5520850189458884, 257.7587792392113215, 16.71892742266126319 ) ) ;
#22209 = DIRECTION ( 'NONE',  ( -0.8660254037844384856, -0.5000000000000002220, 0.000000000000000000 ) ) ;
#22210 = CARTESIAN_POINT ( 'NONE',  ( 78.58300731283269158, 51.01195712413127836, -15.19627590126262895 ) ) ;
#22211 = CARTESIAN_POINT ( 'NONE',  ( -15.56633235393031178, 168.4865022471903160, 10.00000000000009237 ) ) ;
#22212 = CARTESIAN_POINT ( 'NONE',  ( 41.36564329728400935, 200.8149278399160664, -9.188101187500095079 ) ) ;
#22213 = ADVANCED_FACE ( 'NONE', ( #34402 ), #90135, .T. ) ;
#22214 = CARTESIAN_POINT ( 'NONE',  ( 26.56574046957052460, 17.19860640527293327, 2.839279412974134775 ) ) ;
#22215 = CARTESIAN_POINT ( 'NONE',  ( 151.1811967613751335, 268.7934813906678642, -15.79361349403328418 ) ) ;
#22216 = CARTESIAN_POINT ( 'NONE',  ( 149.7200635338602410, 271.3242383773507527, -12.12223662813266500 ) ) ;
#22217 = CARTESIAN_POINT ( 'NONE',  ( 5.211622267866312441, 23.98502408145590081, -5.678558825948271327 ) ) ;
#22218 = CARTESIAN_POINT ( 'NONE',  ( 76.70982964007059479, 63.62857842591434832, 15.32478313419208149 ) ) ;
#22219 = CARTESIAN_POINT ( 'NONE',  ( 75.04168434830708634, 54.38814634816782245, 16.60217853031275936 ) ) ;
#22220 = CARTESIAN_POINT ( 'NONE',  ( 196.3956310503436953, 264.1850728776087180, 4.154333235580330630 ) ) ;
#22221 = CARTESIAN_POINT ( 'NONE',  ( 82.57385212973971989, 41.04541115053230982, -1.138833187496899768 ) ) ;
#22222 = CARTESIAN_POINT ( 'NONE',  ( 149.3592332192440892, 275.3511165631820745, 7.499194079129854806 ) ) ;
#22223 = DIRECTION ( 'NONE',  ( -0.2197389712097134185, -0.9755587037855265597, 0.000000000000000000 ) ) ;
#22224 = CARTESIAN_POINT ( 'NONE',  ( 94.05805000844991071, 225.1115022471902307, 10.00000000000009592 ) ) ;
#22225 = CARTESIAN_POINT ( 'NONE',  ( 200.3414094930810165, 283.6454952284590263, 16.87912319229835489 ) ) ;
#22226 = CARTESIAN_POINT ( 'NONE',  ( 194.4740566694322297, 285.4027869386137581, -17.19371202535040055 ) ) ;
#22227 = ORIENTED_EDGE ( 'NONE', *, *, #95640, .F. ) ;
#22228 = CARTESIAN_POINT ( 'NONE',  ( 61.04057116557046925, 215.2369531367911009, -4.594050593750048428 ) ) ;
#22229 = ORIENTED_EDGE ( 'NONE', *, *, #22897, .T. ) ;
#22230 = CARTESIAN_POINT ( 'NONE',  ( 179.9540635007602418, 264.0123226724073788, 15.22985420633530573 ) ) ;
#22231 = CARTESIAN_POINT ( 'NONE',  ( 146.7879906441258129, 276.4027375938661635, 4.347255311287614887 ) ) ;
#22232 = CARTESIAN_POINT ( 'NONE',  ( 205.2706556652093752, 273.1077904153184477, -10.97544480913108167 ) ) ;
#22233 = EDGE_LOOP ( 'NONE', ( #9841, #18429, #70357, #35673 ) ) ;
#22234 = CARTESIAN_POINT ( 'NONE',  ( 170.4855375986076638, 248.6613294790634541, -0.2716024841417116753 ) ) ;
#22235 = FACE_OUTER_BOUND ( 'NONE', #16280, .T. ) ;
#22236 = CARTESIAN_POINT ( 'NONE',  ( 148.1829914015846157, 273.9865254053503349, -9.304102644963160529 ) ) ;
#22237 = CARTESIAN_POINT ( 'NONE',  ( 177.1267550122267949, 274.7903246707450649, -17.34070711746236526 ) ) ;
#22238 = VECTOR ( 'NONE', #92614, 1000.000000000000000 ) ;
#22239 = CARTESIAN_POINT ( 'NONE',  ( 156.8572647664473152, 258.9622432186664014, 16.97926827742052325 ) ) ;
#22240 = ORIENTED_EDGE ( 'NONE', *, *, #43385, .F. ) ;
#22241 = CARTESIAN_POINT ( 'NONE',  ( 24.91850453858129910, 20.10170272979927475, -7.433330006724141015 ) ) ;
#22242 = CARTESIAN_POINT ( 'NONE',  ( 75.33346472819354744, 56.39419380256580183, 16.13885548225777811 ) ) ;
#22243 = CARTESIAN_POINT ( 'NONE',  ( 169.9290877785755356, 289.3386371799751942, -2.202558799265889267 ) ) ;
#22244 = CARTESIAN_POINT ( 'NONE',  ( 156.5621193438227294, 267.5160442540268946, 16.96304260999163205 ) ) ;
#22245 = ORIENTED_EDGE ( 'NONE', *, *, #16007, .T. ) ;
#22246 = DIRECTION ( 'NONE',  ( -0.8660254037844384856, -0.5000000000000002220, -3.252519625699449945E-16 ) ) ;
#22247 = CARTESIAN_POINT ( 'NONE',  ( 159.2536436069973718, 254.8115933126508992, -15.76697951715411250 ) ) ;
#22248 = VERTEX_POINT ( 'NONE', #66302 ) ;
#22249 = ORIENTED_EDGE ( 'NONE', *, *, #56926, .F. ) ;
#22250 = CARTESIAN_POINT ( 'NONE',  ( 83.53571973624073621, 48.86361953640308542, -12.93375367189796243 ) ) ;
#22251 = AXIS2_PLACEMENT_3D ( 'NONE', #43492, #43980, #53092 ) ;
#22253 = CARTESIAN_POINT ( 'NONE',  ( 30.87961294008499635, 109.1271249547276341, 59.99999999999999289 ) ) ;
#22252 = CARTESIAN_POINT ( 'NONE',  ( 72.77465006231518885, 68.95668891863901706, 10.36720942691999525 ) ) ;
#22254 = CARTESIAN_POINT ( 'NONE',  ( 208.1303168694798273, 270.1547119170880364, -0.9257663487928086132 ) ) ;
#22255 = CARTESIAN_POINT ( 'NONE',  ( 204.8523313866422484, 275.8323493198358847, 14.65426965484541100 ) ) ;
#22256 = CARTESIAN_POINT ( 'NONE',  ( 198.6742831389107096, 286.5330427765190393, 17.60232614297041565 ) ) ;
#22257 = CARTESIAN_POINT ( 'NONE',  ( 78.01627562341427335, 61.04568562798238673, -15.88251659512814662 ) ) ;
#22258 = CARTESIAN_POINT ( 'NONE',  ( 131.4326323866306723, 240.5643266524160140, 9.188101187500095079 ) ) ;
#22259 = CARTESIAN_POINT ( 'NONE',  ( 177.2879723884094290, 269.2816851795835191, 16.08031286173457630 ) ) ;
#22260 = AXIS2_PLACEMENT_3D ( 'NONE', #42426, #3948, #81985 ) ;
#22261 = CARTESIAN_POINT ( 'NONE',  ( 181.5606416776419110, 260.1619400365603383, 9.495244246682995382 ) ) ;
#22262 = CARTESIAN_POINT ( 'NONE',  ( 78.87554214658000262, 216.3458772461660544, 9.188101187500095079 ) ) ;
#22263 = EDGE_LOOP ( 'NONE', ( #28365, #15620, #89667, #52826 ) ) ;
#22264 = CARTESIAN_POINT ( 'NONE',  ( 170.3127733705114224, 263.9010670580030364, 17.23448983536806622 ) ) ;
#22265 = CARTESIAN_POINT ( 'NONE',  ( 182.9145022086223946, 255.8442969664664304, 0.6158721635512950376 ) ) ;
#22266 = ORIENTED_EDGE ( 'NONE', *, *, #95739, .F. ) ;
#22267 = VECTOR ( 'NONE', #55647, 1000.000000000000114 ) ;
#22268 = CARTESIAN_POINT ( 'NONE',  ( -105.0000000000000000, -8.000000000000000000, 14.21260523776214235 ) ) ;
#22269 = VERTEX_POINT ( 'NONE', #51595 ) ;
#22270 = ORIENTED_EDGE ( 'NONE', *, *, #51184, .F. ) ;
#22271 = FACE_BOUND ( 'NONE', #71682, .T. ) ;
#22272 = CARTESIAN_POINT ( 'NONE',  ( 66.62431214535784818, 67.55485982655905275, 6.324360224251575069 ) ) ;
#22273 = CARTESIAN_POINT ( 'NONE',  ( 197.9272639331449284, 286.8449481112537001, 16.93522022078217404 ) ) ;
#22274 = CARTESIAN_POINT ( 'NONE',  ( 191.1000148935602567, 299.6520602076213891, -9.462302242170249400 ) ) ;
#22275 = CARTESIAN_POINT ( 'NONE',  ( -3.153128914090298274, 64.48620320469859735, 0.000000000000000000 ) ) ;
#22276 = CARTESIAN_POINT ( 'NONE',  ( 193.7275870247597425, 295.1009717758319084, 14.48058678254265885 ) ) ;
#22277 = EDGE_CURVE ( 'NONE', #79746, #88881, #89648, .T. ) ;
#22278 = DIRECTION ( 'NONE',  ( -0.000000000000000000, -0.000000000000000000, 1.000000000000000000 ) ) ;
#22279 = CARTESIAN_POINT ( 'NONE',  ( 87.47635513963552967, 45.03054629282576116, 6.933452704933710464 ) ) ;
#22280 = ORIENTED_EDGE ( 'NONE', *, *, #49800, .F. ) ;
#22281 = EDGE_CURVE ( 'NONE', #15004, #65652, #70088, .T. ) ;
#22282 = VECTOR ( 'NONE', #58924, 1000.000000000000000 ) ;
#22284 = EDGE_CURVE ( 'NONE', #33772, #50515, #26692, .T. ) ;
#22283 = CARTESIAN_POINT ( 'NONE',  ( 187.9760109300380861, 288.6839808275937571, 15.87893199255275789 ) ) ;
#22285 = ORIENTED_EDGE ( 'NONE', *, *, #174, .F. ) ;
#22286 = CARTESIAN_POINT ( 'NONE',  ( 76.15722354489868451, 51.53125197354221854, -15.67564492834882373 ) ) ;
#22287 = EDGE_CURVE ( 'NONE', #37352, #61117, #68778, .T. ) ;
#22288 = CARTESIAN_POINT ( 'NONE',  ( 183.8409078303500621, 275.4022649685220472, 16.46562491007150442 ) ) ;
#22289 = CARTESIAN_POINT ( 'NONE',  ( 206.5508451493652444, 272.8904371854448527, 11.05407534521577695 ) ) ;
#22290 = CARTESIAN_POINT ( 'NONE',  ( 149.0203866098534888, 272.5361143586139860, -12.73049804737905255 ) ) ;
#22291 =( NAMED_UNIT ( * ) SI_UNIT ( $, .STERADIAN. ) SOLID_ANGLE_UNIT ( ) );
#22292 = CARTESIAN_POINT ( 'NONE',  ( 162.7946441242182232, 261.4156790044469290, 17.51582106973610564 ) ) ;
#22293 = CARTESIAN_POINT ( 'NONE',  ( 127.8056303646358032, 256.8464784336661637, 1.353441290958777327E-15 ) ) ;
#22294 = ORIENTED_EDGE ( 'NONE', *, *, #31829, .T. ) ;
#22295 = CARTESIAN_POINT ( 'NONE',  ( 87.78141208182009336, 44.24254441107329683, 4.709165031671994406 ) ) ;
#22296 = CARTESIAN_POINT ( 'NONE',  ( 68.96773005203053231, 67.85633357740573501, -9.040919504298567944 ) ) ;
#22297 = CARTESIAN_POINT ( 'NONE',  ( 80.01063490705305981, 44.83894994093007824, -11.28620975940164506 ) ) ;
#22298 = CARTESIAN_POINT ( 'NONE',  ( 201.1388841337167435, 282.2642286331299601, -18.17233400608081340 ) ) ;
#22299 = CARTESIAN_POINT ( 'NONE',  ( 72.70196728203136161, 70.94362825444909504, 7.654249537423025274 ) ) ;
#22300 = LINE ( 'NONE', #30898, #38871 ) ;
#22301 = ORIENTED_EDGE ( 'NONE', *, *, #24417, .T. ) ;
#22302 = CARTESIAN_POINT ( 'NONE',  ( 196.0614467148371602, 264.7781410680017302, 5.416773119000386494 ) ) ;
#22303 = CARTESIAN_POINT ( 'NONE',  ( 148.3010860587701814, 276.5068540982774721, -3.904121881399305050 ) ) ;
#22304 = CARTESIAN_POINT ( 'NONE',  ( 31.94941146435350987, 203.6868197944959320, -22.49999999999984368 ) ) ;
#22305 = AXIS2_PLACEMENT_3D ( 'NONE', #78401, #71303, #48492 ) ;
#22306 = CARTESIAN_POINT ( 'NONE',  ( 184.6824817629046436, 263.5711312746864792, -12.44848753094074389 ) ) ;
#22307 = CARTESIAN_POINT ( 'NONE',  ( 198.6594462311236100, 266.3252094933188232, 0.8312128693835356685 ) ) ;
#22308 = CARTESIAN_POINT ( 'NONE',  ( 190.7908437487391780, 300.1875603386860689, -4.317984972589949955 ) ) ;
#22309 = CARTESIAN_POINT ( 'NONE',  ( 186.8917667502177267, 282.0639843911756088, 17.00272728164306457 ) ) ;
#22310 = AXIS2_PLACEMENT_3D ( 'NONE', #45085, #3, #45573 ) ;
#22311 = AXIS2_PLACEMENT_3D ( 'NONE', #17644, #72866, #80482 ) ;
#22312 = DIRECTION ( 'NONE',  ( -0.9439450758449140499, 0.3301025504114431519, 0.000000000000000000 ) ) ;
#22314 = CARTESIAN_POINT ( 'NONE',  ( 193.5841046816602216, 269.1605544676620525, 12.13440722373979419 ) ) ;
#22313 = CARTESIAN_POINT ( 'NONE',  ( 177.2604144123859271, 264.5285374513375132, -15.40663022330867271 ) ) ;
#22315 = CARTESIAN_POINT ( 'NONE',  ( 24.56267145112387240, 22.38052372038641735, 10.00000000000000533 ) ) ;
#22316 = DIRECTION ( 'NONE',  ( 1.000000000000000000, 0.000000000000000000, 0.000000000000000000 ) ) ;
#22317 = CARTESIAN_POINT ( 'NONE',  ( 166.4998282923256170, 286.5300311998390725, -3.271394949006546593 ) ) ;
#22318 = CARTESIAN_POINT ( 'NONE',  ( 73.98570270871887544, 68.92876820612472955, -11.10152750440661862 ) ) ;
#22319 = CARTESIAN_POINT ( 'NONE',  ( 159.3767386493506137, 254.5983864451355032, 15.47015898230477760 ) ) ;
#22320 = CIRCLE ( 'NONE', #95202, 4.999999999999993783 ) ;
#22321 = CARTESIAN_POINT ( 'NONE',  ( -6.887775800123916881, 157.6423013555410080, -4.594050593750043987 ) ) ;
#22322 = DIRECTION ( 'NONE',  ( 0.8393827800519358950, 0.5435407515102096410, 0.000000000000000000 ) ) ;
#22323 = VERTEX_POINT ( 'NONE', #75918 ) ;
#22324 = VECTOR ( 'NONE', #60114, 1000.000000000000000 ) ;
#22325 = CARTESIAN_POINT ( 'NONE',  ( 66.89157806229785308, 68.17490930942568639, -6.585856375969495247 ) ) ;
#22326 = B_SPLINE_CURVE_WITH_KNOTS ( 'NONE', 3,
 ( #95751, #93741, #9099, #2002, #55668, #48607, #87674, #55177, #48088, #70906, #80036, #78514, #57181, #17186, #10605, #1515, #41477, #3029, #63293, #79028, #88159, #49588, #10103, #80542, #40966, #9619, #40482, #32888, #2513, #89169, #3518, #21203, #82545, #34881, #13109, #97712, #27797, #58671, #27302, #43476, #81051, #89642, #97228, #66296, #51074, #35882, #11614, #66786, #34395, #98206, #96737, #5005 ),
 .UNSPECIFIED., .F., .F.,
 ( 4, 2, 2, 2, 2, 2, 2, 2, 2, 2, 2, 2, 2, 2, 2, 2, 2, 2, 2, 2, 2, 2, 2, 2, 2, 4 ),
 ( 0.0006802182506974893640, 0.001179301278685929155, 0.001678384306674368838, 0.001927925820668672380, 0.002177467334662975488, 0.002302238091660068712, 0.002427008848657161936, 0.002551779605654255594, 0.002676550362651348818, 0.002926091876645458504, 0.003175633390639568624, 0.003674716418627863891, 0.004672882474604453558, 0.005671048530581044092, 0.006170131558569339793, 0.006419673072563446443, 0.006669214586557552227, 0.006731599965056004296, 0.006793985343554457233, 0.006856370722052909303, 0.006918756100551360505, 0.007168297614545246846, 0.007667380642533016058, 0.008166463670520785270, 0.008416005184514652529, 0.008665546698508521523 ),
 .UNSPECIFIED. ) ;
#22327 = CARTESIAN_POINT ( 'NONE',  ( 73.00222835256424503, 70.74352510380845160, -7.508679084761850753 ) ) ;
#22328 = CARTESIAN_POINT ( 'NONE',  ( 151.1451503555562113, 268.8559155969762742, -15.81507177720227553 ) ) ;
#22329 = CARTESIAN_POINT ( 'NONE',  ( 5.371288904610766579, 186.1589784336661637, -6.496448406907676862E-16 ) ) ;
#22330 = EDGE_CURVE ( 'NONE', #2161, #81326, #99186, .T. ) ;
#22331 = CARTESIAN_POINT ( 'NONE',  ( 181.2988614377958356, 275.3026993373888445, -16.43866227028271965 ) ) ;
#22332 = CARTESIAN_POINT ( 'NONE',  ( 18.88643602551048417, 33.83705186507754092, 3.090169943749475401 ) ) ;
#22333 = CARTESIAN_POINT ( 'NONE',  ( 85.27718046765656368, 42.54128723994562478, -1.177150515647308993 ) ) ;
#22334 = CARTESIAN_POINT ( 'NONE',  ( 72.38141447910541615, 201.0494855054051868, -2.679491924311248496 ) ) ;
#22335 = DIRECTION ( 'NONE',  ( 0.5000000000000012212, -0.8660254037844379305, 0.000000000000000000 ) ) ;
#22336 = CARTESIAN_POINT ( 'NONE',  ( 127.8330407560430473, 244.6115022471902591, 10.00000000000009592 ) ) ;
#22337 = B_SPLINE_SURFACE_WITH_KNOTS ( 'NONE', 3, 1, ( 
 ( #42646, #64980 ),
 ( #58352, #36046 ),
 ( #95923, #57360 ),
 ( #51771, #20376 ),
 ( #65963, #66949 ),
 ( #88335, #73578 ),
 ( #74082, #28451 ),
 ( #49770, #27484 ),
 ( #50753, #81706 ),
 ( #12278, #4671 ),
 ( #35561, #66462 ),
 ( #97387, #92780 ),
 ( #29456, #61 ),
 ( #45630, #37049 ),
 ( #21853, #76558 ),
 ( #98379, #36544 ),
 ( #92295, #23333 ),
 ( #54222, #13279 ),
 ( #5655, #68442 ),
 ( #67451, #61337 ),
 ( #53729, #99370 ),
 ( #84203, #22351 ),
 ( #22846, #28968 ),
 ( #53247, #7139 ),
 ( #14257, #84688 ),
 ( #59846, #91785 ),
 ( #38536, #14749 ),
 ( #44141, #52248 ),
 ( #7645, #38026 ),
 ( #77039, #99862 ),
 ( #30447, #90809 ),
 ( #60824, #15229 ),
 ( #6155, #75566 ),
 ( #46125, #69443 ) ),
 .UNSPECIFIED., .T., .F., .F.,
 ( 4, 2, 2, 2, 2, 2, 2, 2, 2, 2, 2, 2, 2, 2, 2, 2, 4 ),
 ( 2, 2 ),
 ( 0.000000000000000000, 0.06250000000000000000, 0.1250000000000000000, 0.1875000000000000000, 0.2500000000000000000, 0.3125000000000000000, 0.3750000000000000000, 0.4375000000000000000, 0.5000000000000000000, 0.5625000000000000000, 0.6250000000000000000, 0.6875000000000000000, 0.7500000000000000000, 0.8125000000000000000, 0.8750000000000000000, 0.9375000000000000000, 1.000000000000000000 ),
 ( 0.000000000000000000, 1.000000000000000000 ),
 .UNSPECIFIED. ) ;
#22338 = CARTESIAN_POINT ( 'NONE',  ( 175.5289681635948398, 253.4651622633166710, -3.633261989091086441 ) ) ;
#22339 = CARTESIAN_POINT ( 'NONE',  ( 191.1394246315239229, 261.3397897443172724, -1.588466913715747442 ) ) ;
#22340 = EDGE_CURVE ( 'NONE', #40695, #77239, #44790, .T. ) ;
#22341 = CARTESIAN_POINT ( 'NONE',  ( 52.92184332868904306, 211.3615022471903160, 5.000000000000046185 ) ) ;
#22342 = CYLINDRICAL_SURFACE ( 'NONE', #99239, 17.82106496071139645 ) ;
#22343 = VECTOR ( 'NONE', #89416, 1000.000000000000227 ) ;
#22344 = CARTESIAN_POINT ( 'NONE',  ( 148.4016473149517594, 273.6078022540229426, 8.470066617688926769 ) ) ;
#22345 = CARTESIAN_POINT ( 'NONE',  ( 26.12944271915780448, 176.7048013555409796, 4.594050593750051981 ) ) ;
#22346 = CARTESIAN_POINT ( 'NONE',  ( 68.59496618099213094, 69.97855879749779717, -4.650311752650147845 ) ) ;
#22347 = EDGE_CURVE ( 'NONE', #49527, #70724, #55562, .T. ) ;
#22348 = CARTESIAN_POINT ( 'NONE',  ( 72.59558277096371626, 71.44241063249414481, 5.693108417517408704 ) ) ;
#22349 = CARTESIAN_POINT ( 'NONE',  ( 46.16617079539854984, 27.44966523072498177, -2.296566073217252530E-15 ) ) ;
#22350 = CARTESIAN_POINT ( 'NONE',  ( 29.12701137275935181, 44.61184105132205957, -10.00000000000000000 ) ) ;
#22351 = CARTESIAN_POINT ( 'NONE',  ( 164.5867587387928950, 245.5743669417666126, -3.022048486790635202 ) ) ;
#22352 = CYLINDRICAL_SURFACE ( 'NONE', #50762, 16.60714546451156792 ) ;
#22353 = CARTESIAN_POINT ( 'NONE',  ( 160.5424585579978896, 278.9220658006375970, -9.787057437366879498 ) ) ;
#22354 = CARTESIAN_POINT ( 'NONE',  ( -19.65312891409030271, 93.06504152958497400, 59.99999999999999289 ) ) ;
#22355 = CARTESIAN_POINT ( 'NONE',  ( 25.69310950058096310, 17.76004757982090254, 5.678558825948272215 ) ) ;
#22356 = CARTESIAN_POINT ( 'NONE',  ( 148.2267527339363369, 273.9107285543102535, 7.913369084260907016 ) ) ;
#22357 = CARTESIAN_POINT ( 'NONE',  ( 71.98731340802646628, 59.17192410441948169, 15.86756879471484183 ) ) ;
#22358 = CARTESIAN_POINT ( 'NONE',  ( 194.2199708651012600, 294.2481379475345875, 15.50834247347371253 ) ) ;
#22359 = VERTEX_POINT ( 'NONE', #32776 ) ;
#22360 = CARTESIAN_POINT ( 'NONE',  ( 185.5050748790181672, 290.8734282190925455, 12.35404501033644920 ) ) ;
#22361 = LINE ( 'NONE', #75088, #76135 ) ;
#22362 = CARTESIAN_POINT ( 'NONE',  ( 4.715407580134756138, 161.9824982072973683, 3.021315404115420679E-15 ) ) ;
#22363 = ORIENTED_EDGE ( 'NONE', *, *, #89267, .F. ) ;
#22365 = DIRECTION ( 'NONE',  ( 4.546899780356473057E-16, -0.000000000000000000, -1.000000000000000000 ) ) ;
#22364 =( BOUNDED_CURVE ( )  B_SPLINE_CURVE ( 2, ( #19742, #52597, #82070, #50606, #81561, #42993, #35911, #66810, #20734, #90162, #69277, #37864, #44976 ),
 .UNSPECIFIED., .F., .T. ) 
 B_SPLINE_CURVE_WITH_KNOTS ( ( 3, 2, 2, 2, 2, 2, 3 ),
 ( 0.8375000000000000222, 0.8399999999999999689, 0.8449999999999999734, 0.8499999999999999778, 0.8549999999999999822, 0.8599999999999999867, 0.8625000000000000444 ),
 .UNSPECIFIED. ) 
 CURVE ( )  GEOMETRIC_REPRESENTATION_ITEM ( )  RATIONAL_B_SPLINE_CURVE ( ( 0.9755282581475767101, 0.9755282581475772652, 1.000000000000000000, 0.9510565162951535312, 1.000000000000000000, 0.9510565162951535312, 1.000000000000000000, 0.9510565162951535312, 1.000000000000000000, 0.9510565162951535312, 1.000000000000000000, 0.9755282581475761550, 0.9755282581475767101 ) ) 
 REPRESENTATION_ITEM ( '' )  );
#22366 = CARTESIAN_POINT ( 'NONE',  ( 69.61553634081849395, 70.72154784002148631, -1.738344088579393043 ) ) ;
#22367 = CARTESIAN_POINT ( 'NONE',  ( 20.28716687417668751, 35.21091486745861232, 7.012934429366973338E-14 ) ) ;
#22368 = CARTESIAN_POINT ( 'NONE',  ( 154.8833801513861772, 262.3811116602312268, -17.49275566389638215 ) ) ;
#22369 = ORIENTED_EDGE ( 'NONE', *, *, #44734, .T. ) ;
#22370 = ORIENTED_EDGE ( 'NONE', *, *, #84497, .T. ) ;
#22372 = CARTESIAN_POINT ( 'NONE',  ( 204.9768178125733016, 275.6167325052707611, 13.98665089523138505 ) ) ;
#22371 = DIRECTION ( 'NONE',  ( 0.4999999999999998890, -0.8660254037844385966, 0.000000000000000000 ) ) ;
#22373 = EDGE_LOOP ( 'NONE', ( #66873, #73886, #11808, #64545 ) ) ;
#22374 = CARTESIAN_POINT ( 'NONE',  ( 150.7226148805041817, 269.5877685077668957, 15.52819754351937576 ) ) ;
#22375 = AXIS2_PLACEMENT_3D ( 'NONE', #79655, #2626, #31992 ) ;
#22376 = DIRECTION ( 'NONE',  ( 0.000000000000000000, 0.000000000000000000, 1.000000000000000000 ) ) ;
#22377 = CARTESIAN_POINT ( 'NONE',  ( 79.85415921798438887, 57.97294913568264008, 16.26669915568274050 ) ) ;
#22378 = CARTESIAN_POINT ( 'NONE',  ( 70.09637832351664599, 69.82647708718234014, -7.001659778457793415 ) ) ;
#22379 = VERTEX_POINT ( 'NONE', #64693 ) ;
#22380 = CARTESIAN_POINT ( 'NONE',  ( 148.2980785574368952, 273.7871886041155562, 9.134436720559454770 ) ) ;
#22381 = VECTOR ( 'NONE', #88209, 1000.000000000000000 ) ;
#22382 = VECTOR ( 'NONE', #2145, 1000.000000000000000 ) ;
#22383 = ORIENTED_EDGE ( 'NONE', *, *, #15747, .F. ) ;
#22384 = CARTESIAN_POINT ( 'NONE',  ( 206.3106310032756596, 273.3065002911688453, 10.17860425536756175 ) ) ;
#22385 = VECTOR ( 'NONE', #87023, 1000.000000000000114 ) ;
#22386 = CARTESIAN_POINT ( 'NONE',  ( 74.48947563274340666, 63.15900717418585231, 14.54963554206422849 ) ) ;
#22387 = ORIENTED_EDGE ( 'NONE', *, *, #81117, .F. ) ;
#22388 = EDGE_CURVE ( 'NONE', #58638, #26637, #7872, .T. ) ;
#22389 = CARTESIAN_POINT ( 'NONE',  ( 149.0359194785865498, 272.5092106407810206, 12.76357969772040590 ) ) ;
#22390 = CARTESIAN_POINT ( 'NONE',  ( -64.54732778733692555, 39.35739861417317087, 177.5919119679930134 ) ) ;
#22391 = VERTEX_POINT ( 'NONE', #93190 ) ;
#22392 = CARTESIAN_POINT ( 'NONE',  ( -14.75193346722050158, 72.91080179107989068, 13.82017248825341937 ) ) ;
#22393 = CARTESIAN_POINT ( 'NONE',  ( -73.83803415018343230, 50.74234351129840093, -10.00000000000000000 ) ) ;
#22394 = DIRECTION ( 'NONE',  ( -0.7080737730998226676, 0.7061384650677096086, 0.000000000000000000 ) ) ;
#22395 = LINE ( 'NONE', #13799, #25304 ) ;
#22396 = ORIENTED_EDGE ( 'NONE', *, *, #52325, .T. ) ;
#22397 = ORIENTED_EDGE ( 'NONE', *, *, #41041, .F. ) ;
#22398 = AXIS2_PLACEMENT_3D ( 'NONE', #68983, #21892, #38069 ) ;
#22399 = CARTESIAN_POINT ( 'NONE',  ( 73.56791514541508548, 69.79467306600464838, 9.342728403714463781 ) ) ;
#22400 = CARTESIAN_POINT ( 'NONE',  ( 146.7845206192450007, 276.4087478532630939, 4.443586170796542945 ) ) ;
#22401 = CARTESIAN_POINT ( 'NONE',  ( 147.6300909839706321, 274.9441770201837585, 8.328755691084779755 ) ) ;
#22402 = CARTESIAN_POINT ( 'NONE',  ( 149.3833831332874240, 271.9073859370555510, 11.40518020539810173 ) ) ;
#22403 = CARTESIAN_POINT ( 'NONE',  ( 171.0589475124673413, 275.4374387251525036, -16.05662091941493586 ) ) ;
#22404 = EDGE_CURVE ( 'NONE', #90349, #6038, #22768, .T. ) ;
#22405 = CARTESIAN_POINT ( 'NONE',  ( 146.5163827660608433, 276.8731762384107356, -0.1825760380121486393 ) ) ;
#22406 = ADVANCED_FACE ( 'NONE', ( #55141 ), #76329, .F. ) ;
#22407 = CARTESIAN_POINT ( 'NONE',  ( 191.7741832257749195, 298.4843664033717801, -8.615487418695501276 ) ) ;
#22408 = CARTESIAN_POINT ( 'NONE',  ( 163.5970988786415035, 257.6140216154675500, 15.49997863511091545 ) ) ;
#22409 = CARTESIAN_POINT ( 'NONE',  ( 70.89288081638191841, 69.42695580627280094, 7.581665190048367364 ) ) ;
#22410 = CARTESIAN_POINT ( 'NONE',  ( 68.20887950783240683, 70.50781471800318911, 6.446984873749973067E-06 ) ) ;
#22411 = CARTESIAN_POINT ( 'NONE',  ( 66.96856610619528283, 66.96525581452927156, 8.678199790520725543 ) ) ;
#22412 = CARTESIAN_POINT ( 'NONE',  ( 167.8632803254916723, 287.0380262542474838, 3.490854160492717462 ) ) ;
#22413 = CARTESIAN_POINT ( 'NONE',  ( 78.12712398815010317, 47.68924013269637641, 14.49032448239827886 ) ) ;
#22414 = CARTESIAN_POINT ( 'NONE',  ( 106.9945647975297760, 223.3923013555410080, 4.594050593750050204 ) ) ;
#22415 = VERTEX_POINT ( 'NONE', #81017 ) ;
#22416 = CARTESIAN_POINT ( 'NONE',  ( 190.6156810949310056, 300.4909509546700974, -4.738288261098400511 ) ) ;
#22417 = CARTESIAN_POINT ( 'NONE',  ( 71.81875712178876370, 69.15799409778134077, 8.801720388420321228 ) ) ;
#22418 = CARTESIAN_POINT ( 'NONE',  ( 3.318370377354149081, 69.04773004486530397, -10.00000000000000000 ) ) ;
#22419 = CARTESIAN_POINT ( 'NONE',  ( 79.01901227882056844, 46.16084846667202868, 12.74958081812160948 ) ) ;
#22420 = CARTESIAN_POINT ( 'NONE',  ( 179.9804799098377543, 283.2464424863279646, -16.00788805095805500 ) ) ;
#22421 = DIRECTION ( 'NONE',  ( 0.5000000000000013323, -0.8660254037844378194, 0.000000000000000000 ) ) ;
#22422 = CARTESIAN_POINT ( 'NONE',  ( 168.9026472910029213, 285.9199674911590705, -7.578321094149770509 ) ) ;
#22423 = ORIENTED_EDGE ( 'NONE', *, *, #5586, .F. ) ;
#22424 = CARTESIAN_POINT ( 'NONE',  ( 207.5920568422024814, 271.0870056320159165, -1.586464549033245186 ) ) ;
#22425 = DIRECTION ( 'NONE',  ( -0.8660254037844387076, -0.4999999999999998890, -0.000000000000000000 ) ) ;
#22426 = CARTESIAN_POINT ( 'NONE',  ( 72.49874796052694137, 71.64632196231394801, 6.095118657294458231 ) ) ;
#22427 = CARTESIAN_POINT ( 'NONE',  ( 34.21208616421480286, 203.8927522451419350, 2.944929066748280225E-16 ) ) ;
#22428 = CARTESIAN_POINT ( 'NONE',  ( 107.8059429699301575, 242.2369531367911009, -4.594050593750048428 ) ) ;
#22429 = CARTESIAN_POINT ( 'NONE',  ( 199.2383506163646132, 285.5560492466715345, -17.78808061564097898 ) ) ;
#22430 = CARTESIAN_POINT ( 'NONE',  ( 36.25628400652970384, 53.06077264917335157, -10.00000000000000000 ) ) ;
#22431 = CARTESIAN_POINT ( 'NONE',  ( 157.2744851780909414, 258.2395962677452985, 18.17792129701959070 ) ) ;
#22432 = CARTESIAN_POINT ( 'NONE',  ( 175.5508771970481803, 253.4024090357540615, -4.579646307325052845 ) ) ;
#22433 = CARTESIAN_POINT ( 'NONE',  ( 38.44315465527655107, 186.8768266524159856, -9.188101187500091527 ) ) ;
#22434 = VECTOR ( 'NONE', #43977, 1000.000000000000000 ) ;
#22435 = FACE_OUTER_BOUND ( 'NONE', #48337, .T. ) ;
#22436 = ORIENTED_EDGE ( 'NONE', *, *, #95215, .T. ) ;
#22437 = CARTESIAN_POINT ( 'NONE',  ( -0.5010987708114443828, 180.5177522451419350, 5.000000000000046185 ) ) ;
#22438 = CARTESIAN_POINT ( 'NONE',  ( 178.1315106821064091, 265.7600619140744129, 15.42674999082912812 ) ) ;
#22439 = FACE_OUTER_BOUND ( 'NONE', #69347, .T. ) ;
#22440 = CARTESIAN_POINT ( 'NONE',  ( 147.4811722709131914, 275.2021117973970377, 3.890385073228495916 ) ) ;
#22441 = CARTESIAN_POINT ( 'NONE',  ( 81.91113339553959349, 41.29801664419279206, -5.856091804582637117 ) ) ;
#22442 = CYLINDRICAL_SURFACE ( 'NONE', #60793, 10.00000000000010658 ) ;
#22443 = CARTESIAN_POINT ( 'NONE',  ( 165.2854559968822343, 250.6596768082254414, 10.19847216201956641 ) ) ;
#22444 = CARTESIAN_POINT ( 'NONE',  ( 114.7524487161676774, 230.3927522451418213, -10.00000000000009059 ) ) ;
#22445 = AXIS2_PLACEMENT_3D ( 'NONE', #37611, #84764, #23915 ) ;
#22446 = DIRECTION ( 'NONE',  ( 0.6355427771210649945, 0.000000000000000000, -0.7720656568254052887 ) ) ;
#22447 = ORIENTED_EDGE ( 'NONE', *, *, #74681, .T. ) ;
#22448 = AXIS2_PLACEMENT_3D ( 'NONE', #515, #99335, #31402 ) ;
#22449 = CARTESIAN_POINT ( 'NONE',  ( 163.1008115941903895, 248.1481028935802442, 11.25332017433677834 ) ) ;
#22450 = CARTESIAN_POINT ( 'NONE',  ( 208.0421103033489771, 270.3074901711881353, -2.473242163239977476 ) ) ;
#22451 = VECTOR ( 'NONE', #35615, 1000.000000000000114 ) ;
#22452 = EDGE_CURVE ( 'NONE', #80984, #92056, #58151, .T. ) ;
#22453 = CARTESIAN_POINT ( 'NONE',  ( 13.89683389070260944, 169.6423013555409796, -4.594050593750043987 ) ) ;
#22454 = CARTESIAN_POINT ( 'NONE',  ( 69.69180481802852967, 68.87891834069074548, -8.182775995575166661 ) ) ;
#22455 = CARTESIAN_POINT ( 'NONE',  ( 194.3301429122894888, 273.0266408274683840, 14.32923346541002374 ) ) ;
#22456 = CARTESIAN_POINT ( 'NONE',  ( 71.72224841297412468, 59.56686840634775848, -15.71315591292551872 ) ) ;
#22457 = CARTESIAN_POINT ( 'NONE',  ( 73.99515186948657686, 54.97541550358009488, -16.60506967685200763 ) ) ;
#22459 = CARTESIAN_POINT ( 'NONE',  ( 66.56148311469628709, 218.4244531367911293, -4.594050593750046652 ) ) ;
#22458 = CARTESIAN_POINT ( 'NONE',  ( 174.6713748507754929, 286.4050021081735622, 10.35879135939865847 ) ) ;
#22460 = EDGE_CURVE ( 'NONE', #74797, #36600, #3744, .T. ) ;
#22461 = CARTESIAN_POINT ( 'NONE',  ( 208.2764314485352770, 269.9016340424377063, 2.433736665191914117 ) ) ;
#22462 = CARTESIAN_POINT ( 'NONE',  ( 73.69000260020860082, 55.31241817090647572, 16.11699230035644703 ) ) ;
#22463 = CARTESIAN_POINT ( 'NONE',  ( -29.75479735258813108, 96.20417995190686611, 44.62577945616610009 ) ) ;
#22464 = CARTESIAN_POINT ( 'NONE',  ( 66.18199044853756163, 68.66682925730346199, -4.353933929110309187 ) ) ;
#22465 = ORIENTED_EDGE ( 'NONE', *, *, #71565, .T. ) ;
#22466 = VECTOR ( 'NONE', #62354, 1000.000000000000114 ) ;
#22467 = CARTESIAN_POINT ( 'NONE',  ( 8.321535033790485869, 175.6115022471902307, 10.00000000000009592 ) ) ;
#22468 = CARTESIAN_POINT ( 'NONE',  ( 164.3053959849042087, 246.0617015268593661, -7.251939739328854273 ) ) ;
#22469 = CARTESIAN_POINT ( 'NONE',  ( 143.8006444583684242, 244.6423013555409796, -4.594050593750043987 ) ) ;
#22470 = CARTESIAN_POINT ( 'NONE',  ( 28.77833178495667710, 28.56628583063842441, 9.188101187500006262 ) ) ;
#22472 = EDGE_CURVE ( 'NONE', #83741, #28867, #16980, .T. ) ;
#22471 = CARTESIAN_POINT ( 'NONE',  ( 165.4376610383445723, 261.3391624790643277, -16.16452297080461165 ) ) ;
#22473 = LINE ( 'NONE', #53366, #58136 ) ;
#22474 = CARTESIAN_POINT ( 'NONE',  ( 195.4968220042985365, 281.1850258734705790, -17.68988808217971709 ) ) ;
#22476 = CARTESIAN_POINT ( 'NONE',  ( 47.03029105687465261, 114.3563895605556269, 10.00000000000000000 ) ) ;
#22475 = CARTESIAN_POINT ( 'NONE',  ( 70.73695309034920342, 71.03131902187277547, 5.127882233600515427 ) ) ;
#22477 = DIRECTION ( 'NONE',  ( -0.4242989612870696758, 0.9055221650797476984, 0.000000000000000000 ) ) ;
#22478 = ORIENTED_EDGE ( 'NONE', *, *, #32486, .T. ) ;
#22479 = CARTESIAN_POINT ( 'NONE',  ( 190.8860811105559208, 300.0226043892405414, 8.636347304323541252 ) ) ;
#22480 = CARTESIAN_POINT ( 'NONE',  ( 208.3738965968843502, 269.7328194535299986, -0.6978089580936264191 ) ) ;
#22481 = CARTESIAN_POINT ( 'NONE',  ( 152.3249143222120381, 268.8125044657937792, -15.54600960379902297 ) ) ;
#22482 = LINE ( 'NONE', #78191, #92020 ) ;
#22483 = CARTESIAN_POINT ( 'NONE',  ( -76.38857681351474582, 54.22815603855766398, 10.00000000000000000 ) ) ;
#22484 = VERTEX_POINT ( 'NONE', #89610 ) ;
#22485 = CARTESIAN_POINT ( 'NONE',  ( 160.2385711492790108, 253.1056487676453628, 14.63819537062152598 ) ) ;
#22486 = DIRECTION ( 'NONE',  ( -0.8660254037844387076, -0.4999999999999998890, -0.000000000000000000 ) ) ;
#22487 = CARTESIAN_POINT ( 'NONE',  ( 71.59874412008122135, 72.43189726433810449, 0.9745913883648592568 ) ) ;
#22488 = ADVANCED_FACE ( 'NONE', ( #28247 ), #98678, .T. ) ;
#22489 = DIRECTION ( 'NONE',  ( 0.4999999999999992784, -0.8660254037844390407, 0.000000000000000000 ) ) ;
#22490 = DIRECTION ( 'NONE',  ( 0.000000000000000000, -0.000000000000000000, -1.000000000000000000 ) ) ;
#22491 = CARTESIAN_POINT ( 'NONE',  ( 186.6036341826941509, 277.9756864068600635, 17.81853497364681616 ) ) ;
#22492 = CARTESIAN_POINT ( 'NONE',  ( 67.90270976675789427, 69.15137710594201792, 4.266361631938849541 ) ) ;
#22493 = CARTESIAN_POINT ( 'NONE',  ( 201.4214977800931763, 281.7747274386935601, -17.04225209925078133 ) ) ;
#22494 = CARTESIAN_POINT ( 'NONE',  ( 191.0170027573799700, 280.9900163574024532, 16.65089222855447204 ) ) ;
#22495 = CARTESIAN_POINT ( 'NONE',  ( 11.78719504716597299, 22.50829794293879260, -10.00000000000000355 ) ) ;
#22496 = CARTESIAN_POINT ( 'NONE',  ( 86.72314128514305764, 46.93129043413777168, 10.24845158530357558 ) ) ;
#22497 = ORIENTED_EDGE ( 'NONE', *, *, #57951, .T. ) ;
#22498 = CARTESIAN_POINT ( 'NONE',  ( 190.6094661480870798, 300.5017155583701083, 4.598210453186021951 ) ) ;
#22499 = CARTESIAN_POINT ( 'NONE',  ( 86.51873334781436142, 47.12553361672021879, -10.58414027450332462 ) ) ;
#22500 = CARTESIAN_POINT ( 'NONE',  ( 83.71391341011990050, 45.20889584457674459, -9.573811886256185844 ) ) ;
#22501 = ORIENTED_EDGE ( 'NONE', *, *, #23408, .F. ) ;
#22502 = CARTESIAN_POINT ( 'NONE',  ( 191.3610003135137276, 299.2000202002271294, -9.855749861282104618 ) ) ;
#22503 = CARTESIAN_POINT ( 'NONE',  ( 79.09474592215633493, 60.19097512726886379, -16.45688605998255127 ) ) ;
#22504 = CARTESIAN_POINT ( 'NONE',  ( 204.2457645315488719, 276.8829539310449945, 14.53406579917280261 ) ) ;
#22505 = CARTESIAN_POINT ( 'NONE',  ( 69.91593357268108377, 62.62562713682927296, 13.43404203153625076 ) ) ;
#22506 = ORIENTED_EDGE ( 'NONE', *, *, #83301, .T. ) ;
#22507 = CARTESIAN_POINT ( 'NONE',  ( 104.3964885861764600, 221.8923013555410080, 4.594050593750050204 ) ) ;
#22508 = CARTESIAN_POINT ( 'NONE',  ( 161.1884843536000744, 251.4603508349806873, 13.21272898143761942 ) ) ;
#22509 = CARTESIAN_POINT ( 'NONE',  ( 181.3300189534027709, 271.3270077267823694, -16.02231281199806645 ) ) ;
#22510 = CARTESIAN_POINT ( 'NONE',  ( 81.81442681794474936, 42.35015792257434697, -7.949573155866509033 ) ) ;
#22511 = ORIENTED_EDGE ( 'NONE', *, *, #41492, .T. ) ;
#22512 = EDGE_CURVE ( 'NONE', #14298, #55257, #66746, .T. ) ;
#22513 = EDGE_LOOP ( 'NONE', ( #15242, #4289, #5943, #1006 ) ) ;
#22514 = ORIENTED_EDGE ( 'NONE', *, *, #26269, .F. ) ;
#22515 = CARTESIAN_POINT ( 'NONE',  ( 81.03644536932286258, 48.60226841593650704, 13.58935439033044901 ) ) ;
#22516 = ORIENTED_EDGE ( 'NONE', *, *, #92628, .F. ) ;
#22517 = LINE ( 'NONE', #216, #37888 ) ;
#22518 = VERTEX_POINT ( 'NONE', #78359 ) ;
#22519 = EDGE_CURVE ( 'NONE', #99910, #83671, #69236, .T. ) ;
#22520 = CARTESIAN_POINT ( 'NONE',  ( 163.8455942243524248, 246.8581015375447691, -7.178103170949780676 ) ) ;
#22521 = CARTESIAN_POINT ( 'NONE',  ( 165.7734550839200836, 271.2459260585341099, 16.34257236049911910 ) ) ;
#22522 = VECTOR ( 'NONE', #62854, 1000.000000000000000 ) ;
#22523 = B_SPLINE_CURVE_WITH_KNOTS ( 'NONE', 3,
 ( #4280, #80848, #42272, #50878 ),
 .UNSPECIFIED., .F., .F.,
 ( 4, 4 ),
 ( 0.004692142627948476911, 0.01023732688395309794 ),
 .UNSPECIFIED. ) ;
#22524 = CARTESIAN_POINT ( 'NONE',  ( 167.2155108587164136, 281.8882477833899998, 11.54502438761175576 ) ) ;
#22525 = CARTESIAN_POINT ( 'NONE',  ( 194.3442947553755005, 294.0328026529847421, -15.97648891113594871 ) ) ;
#22527 = CARTESIAN_POINT ( 'NONE',  ( 82.78312474470216387, 53.88647634593384339, -15.44496935275225269 ) ) ;
#22526 = VECTOR ( 'NONE', #1182, 1000.000000000000114 ) ;
#22528 = EDGE_CURVE ( 'NONE', #96078, #23912, #24167, .T. ) ;
#22529 = ORIENTED_EDGE ( 'NONE', *, *, #13785, .F. ) ;
#22530 = CARTESIAN_POINT ( 'NONE',  ( 82.44310520575160695, 54.28011738120410001, -15.96781897959229113 ) ) ;
#22531 = CARTESIAN_POINT ( 'NONE',  ( 19.31277771287585310, 13.01110640527291551, 2.839279412974134775 ) ) ;
#22532 = CARTESIAN_POINT ( 'NONE',  ( 201.0247283420269184, 278.7743575993829950, -15.66353679845565061 ) ) ;
#22533 = CARTESIAN_POINT ( 'NONE',  ( -68.10632939235270555, 44.28490124273479012, 10.00000000000000000 ) ) ;
#22534 = AXIS2_PLACEMENT_3D ( 'NONE', #98595, #14470, #68652 ) ;
#22536 = ORIENTED_EDGE ( 'NONE', *, *, #66494, .F. ) ;
#22535 = DIRECTION ( 'NONE',  ( -0.8660254037844387076, -0.4999999999999998890, -0.000000000000000000 ) ) ;
#22537 = EDGE_CURVE ( 'NONE', #73589, #47832, #97932, .T. ) ;
#22538 = CARTESIAN_POINT ( 'NONE',  ( 54.05850166760819775, 212.0177522451419065, 5.000000000000046185 ) ) ;
#22539 = EDGE_CURVE ( 'NONE', #95735, #93829, #7297, .T. ) ;
#22540 = CARTESIAN_POINT ( 'NONE',  ( 188.8122907880376147, 259.7915673222115061, 2.322190842852634329 ) ) ;
#22541 = DIRECTION ( 'NONE',  ( 0.5000000000000002220, -0.8660254037844385966, 0.000000000000000000 ) ) ;
#22542 = CARTESIAN_POINT ( 'NONE',  ( 80.47459502809753928, 46.22092247480932770, -12.20579193300740783 ) ) ;
#22543 = CARTESIAN_POINT ( 'NONE',  ( 172.0545069220451921, 254.4921861736880260, 11.48538074941503773 ) ) ;
#22544 = CARTESIAN_POINT ( 'NONE',  ( 157.6090322939100474, 281.6562889287993698, 1.386678441765768932 ) ) ;
#22545 = ORIENTED_EDGE ( 'NONE', *, *, #64042, .F. ) ;
#22546 = CARTESIAN_POINT ( 'NONE',  ( 102.3056452726415984, 218.3262482093457493, 3.021315404115420679E-15 ) ) ;
#22547 = CARTESIAN_POINT ( 'NONE',  ( 72.44797420414980138, 63.04533137475104354, -14.04204238950079819 ) ) ;
#22548 = DIRECTION ( 'NONE',  ( -0.9991767892008870389, -0.04056776950001317328, 0.000000000000000000 ) ) ;
#22549 = CARTESIAN_POINT ( 'NONE',  ( -4.759057006084942643, 181.3927522451419634, 2.944929066748280225E-16 ) ) ;
#22550 = CARTESIAN_POINT ( 'NONE',  ( 196.1441694980680666, 269.5113810647022774, -10.83627284691216808 ) ) ;
#22551 = CARTESIAN_POINT ( 'NONE',  ( 29.30989995549245464, 44.80713248141895377, -10.00000000000000000 ) ) ;
#22552 = CARTESIAN_POINT ( 'NONE',  ( 203.9379510532215818, 277.4161025147623718, -15.87772908648316061 ) ) ;
#22553 = CARTESIAN_POINT ( 'NONE',  ( 84.91875927444918659, 44.62694446506164070, -7.840877269613704570 ) ) ;
#22554 = CARTESIAN_POINT ( 'NONE',  ( 161.9037764296581088, 250.9274884326035533, -12.69612398869453784 ) ) ;
#22556 = CARTESIAN_POINT ( 'NONE',  ( 76.26946404230704957, 64.97317754398874001, 14.67006731301515998 ) ) ;
#22555 = CARTESIAN_POINT ( 'NONE',  ( -8.322217149083147802, 159.8768266524159856, -9.188101187500091527 ) ) ;
#22557 = AXIS2_PLACEMENT_3D ( 'NONE', #32575, #63471, #94407 ) ;
#22558 = CARTESIAN_POINT ( 'NONE',  ( 163.3885797654601788, 248.6152187624725229, 9.728336025080901450 ) ) ;
#22559 = ORIENTED_EDGE ( 'NONE', *, *, #11776, .F. ) ;
#22560 = ORIENTED_EDGE ( 'NONE', *, *, #15071, .T. ) ;
#22561 = CARTESIAN_POINT ( 'NONE',  ( 50.60128122559382291, 92.19983735941717384, -10.00000000000000000 ) ) ;
#22562 = DIRECTION ( 'NONE',  ( -0.8660254037844387076, -0.4999999999999998890, -0.000000000000000000 ) ) ;
#22563 = CARTESIAN_POINT ( 'NONE',  ( 151.2375434627641084, 277.2274377546415849, 6.632753350058649744 ) ) ;
#22564 = CARTESIAN_POINT ( 'NONE',  ( 87.34128990652536118, 44.33892918473014078, 4.514138355736077024 ) ) ;
#22565 = CARTESIAN_POINT ( 'NONE',  ( 162.4372904523162902, 249.2973552232023735, -11.26290998720616621 ) ) ;
#22566 = DIRECTION ( 'NONE',  ( 0.4999999999999998890, -0.8660254037844385966, 0.000000000000000000 ) ) ;
#22567 = B_SPLINE_CURVE_WITH_KNOTS ( 'NONE', 3,
 ( #25007, #47305, #87887, #25519 ),
 .UNSPECIFIED., .F., .F.,
 ( 4, 4 ),
 ( 0.009431583545826283804, 0.01484449304010337575 ),
 .UNSPECIFIED. ) ;
#22568 = CARTESIAN_POINT ( 'NONE',  ( 21.77181853666109745, 189.5024278399161233, 9.188101187500095079 ) ) ;
#22569 = CARTESIAN_POINT ( 'NONE',  ( 116.3854409958760385, 231.8768266524160140, -9.188101187500091527 ) ) ;
#22570 = CARTESIAN_POINT ( 'NONE',  ( 182.0997321953872188, 294.5560652551307044, -6.453979911311197526 ) ) ;
#22571 = CARTESIAN_POINT ( 'NONE',  ( 24.35067441160642687, 40.23626134430271861, 10.00000000000000000 ) ) ;
#22572 = CARTESIAN_POINT ( 'NONE',  ( 149.9839146186740777, 271.6364095184536609, -11.71912693422898677 ) ) ;
#22573 = DIRECTION ( 'NONE',  ( -0.06442261589617469253, -0.9979227057047523886, 0.000000000000000000 ) ) ;
#22574 = CARTESIAN_POINT ( 'NONE',  ( 79.36528506407655925, 53.83448769205969597, -15.81908227153714819 ) ) ;
#22575 = DIRECTION ( 'NONE',  ( -1.000000000000000000, 0.000000000000000000, 5.984665299743594308E-16 ) ) ;
#22576 = DIRECTION ( 'NONE',  ( -1.000000000000000000, 4.892646582057217816E-14, 0.000000000000000000 ) ) ;
#22577 = CARTESIAN_POINT ( 'NONE',  ( 184.3226795282388650, 274.5458599865910969, 17.66928848808302988 ) ) ;
#22578 = CARTESIAN_POINT ( 'NONE',  ( 188.9978738728263465, 284.0756316726331079, 16.44648605183132872 ) ) ;
#22579 = CARTESIAN_POINT ( 'NONE',  ( 70.66241353812237946, 61.03054431235825916, -14.44723600216412329 ) ) ;
#22580 = CARTESIAN_POINT ( 'NONE',  ( 84.37825102736907468, 49.99960613749293969, 13.80049582259582763 ) ) ;
#22581 = CARTESIAN_POINT ( 'NONE',  ( 186.9492098651599861, 298.8821793078109295, -0.5976176902946377378 ) ) ;
#22582 = CARTESIAN_POINT ( 'NONE',  ( 71.20299867106878366, 71.49720395331284806, 2.862355716284322948 ) ) ;
#22583 = CARTESIAN_POINT ( 'NONE',  ( 50.46014644935972626, 188.3932355074535963, -2.679491924311248496 ) ) ;
#22584 = FACE_OUTER_BOUND ( 'NONE', #63786, .T. ) ;
#22585 = VERTEX_POINT ( 'NONE', #8445 ) ;
#22586 = CARTESIAN_POINT ( 'NONE',  ( -22.42236680055709641, 157.8615022471902591, 0.000000000000000000 ) ) ;
#22587 = DIRECTION ( 'NONE',  ( -1.000000000000000000, 0.000000000000000000, 0.000000000000000000 ) ) ;
#22588 = CARTESIAN_POINT ( 'NONE',  ( 94.78875894111908451, 225.5333772461660544, 9.188101187500095079 ) ) ;
#22589 = CARTESIAN_POINT ( 'NONE',  ( 9.658441966945924051, 28.68290643055185996, 3.479690158560446702E-15 ) ) ;
#22591 = EDGE_CURVE ( 'NONE', #36742, #45792, #70231, .T. ) ;
#22590 = CARTESIAN_POINT ( 'NONE',  ( 150.6931560952953646, 269.6387926204777727, 14.65021044537114037 ) ) ;
#22592 = AXIS2_PLACEMENT_3D ( 'NONE', #41833, #74270, #72267 ) ;
#22593 = CARTESIAN_POINT ( 'NONE',  ( 171.3928239984006723, 250.3015599828365509, -5.796133048607560845 ) ) ;
#22595 = CARTESIAN_POINT ( 'NONE',  ( 108.1850894041356810, 233.2677522451418497, 10.00000000000009592 ) ) ;
#22594 = CARTESIAN_POINT ( 'NONE',  ( 19.62422909362874535, 11.73415679381821342, 1.333680081654574804E-15 ) ) ;
#22596 = CARTESIAN_POINT ( 'NONE',  ( 198.2505066714982149, 285.2670451491296149, 0.000000000000000000 ) ) ;
#22597 = CARTESIAN_POINT ( 'NONE',  ( 159.9950753608005130, 276.8117990079294373, 13.35014033362692487 ) ) ;
#22598 = CARTESIAN_POINT ( 'NONE',  ( 138.2253456014562403, 260.6115022471903444, -5.000000000000047962 ) ) ;
#22599 = CARTESIAN_POINT ( 'NONE',  ( 36.01387044229257128, 42.83396525600393545, -2.839279412974133887 ) ) ;
#22600 = CARTESIAN_POINT ( 'NONE',  ( 42.95298936059631245, 26.92755873383629606, 6.180339887498953466 ) ) ;
#22601 = CARTESIAN_POINT ( 'NONE',  ( 198.7178327464537801, 265.3776419993419040, 3.619097246555301961 ) ) ;
#22602 = ORIENTED_EDGE ( 'NONE', *, *, #38592, .T. ) ;
#22603 = CARTESIAN_POINT ( 'NONE',  ( 22.33066906249845118, 34.93396525600390845, 2.839279412974139660 ) ) ;
#22604 = CIRCLE ( 'NONE', #63026, 0.1418229129681591871 ) ;
#22605 = CARTESIAN_POINT ( 'NONE',  ( 160.6332181072797312, 257.2038896978352227, 16.95477083490439441 ) ) ;
#22606 = CARTESIAN_POINT ( 'NONE',  ( 200.0258286195224855, 270.0420316592483800, 9.097251813766577655 ) ) ;
#22607 = B_SPLINE_CURVE_WITH_KNOTS ( 'NONE', 3,
 ( #383, #63176, #17581, #70269, #31758, #47962, #8485, #25173, #93614, #39848, #31271, #878, #30789, #46461, #100203, #39355, #23660, #62158, #9493, #32273, #69276, #94616, #85015, #69775, #16575, #56054, #7993, #38868, #93105, #62662, #70781, #86541, #61669, #54551, #85535, #46980, #54059, #78905 ),
 .UNSPECIFIED., .F., .F.,
 ( 4, 2, 2, 2, 2, 2, 2, 2, 2, 2, 2, 2, 2, 2, 2, 2, 2, 2, 4 ),
 ( 0.003133190382345474832, 0.003329911802006756648, 0.003526633221668038030, 0.003624993931498598273, 0.003723354641329158516, 0.003920076060990278569, 0.004313518900312601073, 0.004706961739634923578, 0.005493847418279567719, 0.006280733096924212729, 0.007854504454213501879, 0.008051225873874617162, 0.008100406228789911595, 0.008149586583705209497, 0.008247947293535850405, 0.008641390132858299544, 0.009034832972180748684, 0.009231554391841950702, 0.009428275811503154455 ),
 .UNSPECIFIED. ) ;
#22609 = VERTEX_POINT ( 'NONE', #89020 ) ;
#22608 = EDGE_CURVE ( 'NONE', #94224, #71267, #10449, .T. ) ;
#22610 = EDGE_CURVE ( 'NONE', #10180, #17718, #7424, .T. ) ;
#22611 = CARTESIAN_POINT ( 'NONE',  ( 84.72527825293784076, 50.50787217764868586, -13.97547420692928277 ) ) ;
#22612 = CARTESIAN_POINT ( 'NONE',  ( 198.4772197948566372, 286.8743665007300478, 18.43646439804394532 ) ) ;
#22613 = CARTESIAN_POINT ( 'NONE',  ( 183.6368557740999279, 264.3442894037191309, -13.58800719496283804 ) ) ;
#22614 = CARTESIAN_POINT ( 'NONE',  ( 169.6113679783735222, 252.3049375988781264, -8.761831181614468278 ) ) ;
#22616 = CARTESIAN_POINT ( 'NONE',  ( 74.98768007058501439, 53.07574299652110739, -16.50056621423362202 ) ) ;
#22615 = VECTOR ( 'NONE', #26681, 1000.000000000000114 ) ;
#22617 = LINE ( 'NONE', #54481, #63036 ) ;
#22618 = ORIENTED_EDGE ( 'NONE', *, *, #86171, .F. ) ;
#22619 = CARTESIAN_POINT ( 'NONE',  ( 187.2446448861898318, 278.7970116248035879, 17.43233615778165202 ) ) ;
#22620 = B_SPLINE_SURFACE_WITH_KNOTS ( 'NONE', 3, 1, ( 
 ( #59580, #5411 ),
 ( #48130, #25853 ),
 ( #80075, #88194 ),
 ( #32926, #12520 ),
 ( #49141, #18744 ),
 ( #2553, #50992 ),
 ( #9657, #79073 ),
 ( #64334, #56215 ),
 ( #51498, #10647 ),
 ( #63830, #81942 ),
 ( #40516, #95294 ),
 ( #3069, #41521 ),
 ( #72464, #13029 ),
 ( #36294, #56729 ),
 ( #43392, #33955 ),
 ( #74335, #67196 ),
 ( #71451, #17747 ),
 ( #87212, #17222 ),
 ( #26343, #87712 ),
 ( #4924, #35802 ),
 ( #66696, #28197 ),
 ( #98118, #94767 ),
 ( #25329, #48647 ),
 ( #79582, #10143 ),
 ( #41008, #21126 ),
 ( #31179, #6891 ),
 ( #14981, #61580 ),
 ( #45867, #29210 ),
 ( #76792, #92050 ),
 ( #38780, #92530 ),
 ( #83941, #13519 ),
 ( #36791, #23078 ),
 ( #53970, #22094 ),
 ( #68683, #90556 ) ),
 .UNSPECIFIED., .T., .F., .F.,
 ( 4, 2, 2, 2, 2, 2, 2, 2, 2, 2, 2, 2, 2, 2, 2, 2, 4 ),
 ( 2, 2 ),
 ( 0.000000000000000000, 0.06250000000000000000, 0.1250000000000000000, 0.1875000000000000000, 0.2500000000000000000, 0.3125000000000000000, 0.3750000000000000000, 0.4375000000000000000, 0.5000000000000000000, 0.5625000000000000000, 0.6250000000000000000, 0.6875000000000000000, 0.7500000000000000000, 0.8125000000000000000, 0.8750000000000000000, 0.9375000000000000000, 1.000000000000000000 ),
 ( 0.000000000000000000, 1.000000000000000000 ),
 .UNSPECIFIED. ) ;
#22621 = CARTESIAN_POINT ( 'NONE',  ( 34.90123498099573851, 22.01110640527294393, 2.839279412974134775 ) ) ;
#22622 = ORIENTED_EDGE ( 'NONE', *, *, #83732, .F. ) ;
#22623 = CARTESIAN_POINT ( 'NONE',  ( 167.9675024332174473, 249.3202678378337964, 6.485191139041705632 ) ) ;
#22624 = CARTESIAN_POINT ( 'NONE',  ( 86.60460766037567737, 43.36433298709366113, 1.857703978550338642 ) ) ;
#22625 = ORIENTED_EDGE ( 'NONE', *, *, #54311, .T. ) ;
#22626 = LINE ( 'NONE', #68214, #86287 ) ;
#22627 = CARTESIAN_POINT ( 'NONE',  ( 206.3068339233826975, 273.3130770264637590, 11.67356747362499547 ) ) ;
#22628 = CARTESIAN_POINT ( 'NONE',  ( 84.98383346588632037, 50.06751842512129258, 13.63401461718180485 ) ) ;
#22629 = CARTESIAN_POINT ( 'NONE',  ( 153.6091969257113874, 264.5880617452517072, -18.08645444069259511 ) ) ;
#22630 = CARTESIAN_POINT ( 'NONE',  ( 153.1961624462112752, 265.3034584490234806, -16.19494717845262954 ) ) ;
#22631 = AXIS2_PLACEMENT_3D ( 'NONE', #25362, #25887, #41553 ) ;
#22632 = CARTESIAN_POINT ( 'NONE',  ( 31.85034293892215373, 41.49540643055189548, 3.479690158560446702E-15 ) ) ;
#22633 = CARTESIAN_POINT ( 'NONE',  ( 81.56133095906432118, 55.49845989692713744, -16.32137983002411730 ) ) ;
#22634 = AXIS2_PLACEMENT_3D ( 'NONE', #95276, #10124, #80563 ) ;
#22635 = CARTESIAN_POINT ( 'NONE',  ( 156.4163639670109092, 273.5530270839410036, -14.20678783894327069 ) ) ;
#22636 = VERTEX_POINT ( 'NONE', #40320 ) ;
#22637 = CARTESIAN_POINT ( 'NONE',  ( 196.1009891436883379, 290.6035456363609342, 16.03271038754406419 ) ) ;
#22638 = ORIENTED_EDGE ( 'NONE', *, *, #66531, .T. ) ;
#22639 = EDGE_LOOP ( 'NONE', ( #58236, #64858, #7523, #3843 ) ) ;
#22640 = CARTESIAN_POINT ( 'NONE',  ( 157.5487431480040925, 257.7645675294749594, -18.29554785922338311 ) ) ;
#22641 = CARTESIAN_POINT ( 'NONE',  ( 163.5242786094305529, 253.3114143684073269, 14.53606660635604975 ) ) ;
#22642 = ADVANCED_FACE ( 'NONE', ( #95602 ), #8407, .F. ) ;
#22644 = CARTESIAN_POINT ( 'NONE',  ( 165.2963502628107619, 246.1214967944202954, 3.165412660861774974 ) ) ;
#22643 = CARTESIAN_POINT ( 'NONE',  ( 152.4004768191108781, 241.6816263820140307, 0.000000000000000000 ) ) ;
#22645 = CARTESIAN_POINT ( 'NONE',  ( 206.5266458972945429, 272.9323515195362120, -9.802257691457246125 ) ) ;
#22646 = CARTESIAN_POINT ( 'NONE',  ( 197.7177225922534944, 272.6128245650874078, -13.25409340876743336 ) ) ;
#22647 = CARTESIAN_POINT ( 'NONE',  ( 72.24150276065003595, 61.63636719674806130, -14.60790590827561530 ) ) ;
#22648 = CARTESIAN_POINT ( 'NONE',  ( 192.5284579606305613, 297.1779242397361713, -13.15228012403107272 ) ) ;
#22649 = CARTESIAN_POINT ( 'NONE',  ( 171.1445398911689608, 250.9114044520595712, -5.572095004965957443 ) ) ;
#22650 = CARTESIAN_POINT ( 'NONE',  ( 165.8412968737758888, 265.9713712601042062, 17.00718710691081981 ) ) ;
#22651 = ADVANCED_FACE ( 'NONE', ( #21059 ), #66137, .T. ) ;
#22652 = CARTESIAN_POINT ( 'NONE',  ( 183.4095142257296800, 284.6173269999417244, -15.03714304829159154 ) ) ;
#22653 = EDGE_CURVE ( 'NONE', #58863, #5335, #75249, .T. ) ;
#22654 = CARTESIAN_POINT ( 'NONE',  ( 119.6601863278771845, 230.7048013555409796, 4.594050593750051981 ) ) ;
#22655 = ORIENTED_EDGE ( 'NONE', *, *, #37082, .T. ) ;
#22656 = CARTESIAN_POINT ( 'NONE',  ( 184.5555326536461678, 260.2792554538418699, -9.747852867291117107 ) ) ;
#22657 = CARTESIAN_POINT ( 'NONE',  ( 34.33172647011804912, 40.79752408145593989, -5.678558825948271327 ) ) ;
#22658 = CARTESIAN_POINT ( 'NONE',  ( 156.6812872898450735, 261.2670451491295012, 0.000000000000000000 ) ) ;
#22659 = EDGE_LOOP ( 'NONE', ( #44848, #35201, #65489, #8179 ) ) ;
#22660 = EDGE_CURVE ( 'NONE', #27862, #92799, #37221, .T. ) ;
#22661 = ORIENTED_EDGE ( 'NONE', *, *, #76587, .F. ) ;
#22662 = CARTESIAN_POINT ( 'NONE',  ( 74.19835002362358978, 68.51042020854130499, -11.60174470505228150 ) ) ;
#22663 = EDGE_CURVE ( 'NONE', #55387, #82505, #20551, .T. ) ;
#22664 = CARTESIAN_POINT ( 'NONE',  ( 69.93873449799818331, 64.21434714275719102, -12.43005340421474259 ) ) ;
#22665 = ADVANCED_FACE ( 'NONE', ( #35235 ), #51938, .F. ) ;
#22666 = CARTESIAN_POINT ( 'NONE',  ( 57.56414817410229290, 217.3207943907112281, -18.47570218321543223 ) ) ;
#22667 = CARTESIAN_POINT ( 'NONE',  ( 192.8425562372348452, 296.6338900660878721, 11.79498561092278841 ) ) ;
#22668 = CARTESIAN_POINT ( 'NONE',  ( 159.5895502557670795, 254.2297859303815244, -16.92708575547316485 ) ) ;
#22669 = CARTESIAN_POINT ( 'NONE',  ( 88.40853095561153907, 233.3967562850347122, -4.648177544792955347E-16 ) ) ;
#22670 = EDGE_LOOP ( 'NONE', ( #48559, #38821 ) ) ;
#22671 = CARTESIAN_POINT ( 'NONE',  ( 195.4960223750947250, 292.0379518991509258, 15.68485942957119406 ) ) ;
#22672 =( BOUNDED_CURVE ( )  B_SPLINE_CURVE ( 2, ( #97798, #88741, #58756, #4577, #73491, #28367, #20287, #66376, #81132 ),
 .UNSPECIFIED., .F., .T. ) 
 B_SPLINE_CURVE_WITH_KNOTS ( ( 3, 2, 2, 2, 3 ),
 ( 0.7782258064516128782, 0.7795698924731182533, 0.7822580645161290036, 0.7849462365591397539, 0.7862903225806451291 ),
 .UNSPECIFIED. ) 
 CURVE ( )  GEOMETRIC_REPRESENTATION_ITEM ( )  RATIONAL_B_SPLINE_CURVE ( ( 0.9330127018922194093, 0.9330127018922194093, 1.000000000000000000, 0.8660254037844387076, 1.000000000000000000, 0.8660254037844387076, 1.000000000000000000, 0.9330127018922194093, 0.9330127018922194093 ) ) 
 REPRESENTATION_ITEM ( '' )  );
#22673 = EDGE_LOOP ( 'NONE', ( #92305, #78451, #99807, #9318 ) ) ;
#22674 = CARTESIAN_POINT ( 'NONE',  ( 61.87308422990769685, 194.9824982072973967, 3.021315404115420679E-15 ) ) ;
#22675 = CARTESIAN_POINT ( 'NONE',  ( 196.4030970371012472, 264.3490001850324234, -4.693669024083267693 ) ) ;
#22676 = VERTEX_POINT ( 'NONE', #81876 ) ;
#22677 = CARTESIAN_POINT ( 'NONE',  ( 188.5598007550805733, 265.1235053368025092, -11.94157573910213799 ) ) ;
#22678 = VECTOR ( 'NONE', #42815, 1000.000000000000114 ) ;
#22679 = CARTESIAN_POINT ( 'NONE',  ( 196.3492756709495382, 264.2680142592890888, 4.029091280256919205 ) ) ;
#22680 = DIRECTION ( 'NONE',  ( -0.000000000000000000, -0.000000000000000000, -1.000000000000000000 ) ) ;
#22681 = CARTESIAN_POINT ( 'NONE',  ( 81.68100823972521596, 43.51052942893925035, 8.843547683132065629 ) ) ;
#22683 = CARTESIAN_POINT ( 'NONE',  ( 156.9442477613751805, 280.6005629174807723, 5.998941275641159976 ) ) ;
#22682 = CARTESIAN_POINT ( 'NONE',  ( 184.8269865458371726, 289.1777887761302850, -13.20314450223754754 ) ) ;
#22684 = CYLINDRICAL_SURFACE ( 'NONE', #86774, 17.82106496071139645 ) ;
#22685 = EDGE_LOOP ( 'NONE', ( #89025, #87862, #15653, #61998, #58422 ) ) ;
#22686 = CARTESIAN_POINT ( 'NONE',  ( 204.7036265338580279, 272.9347255250285684, -9.700744708777794045 ) ) ;
#22687 = CARTESIAN_POINT ( 'NONE',  ( 72.10222062648871599, 64.74920943772764304, 12.95471888058235344 ) ) ;
#22688 = CARTESIAN_POINT ( 'NONE',  ( 82.32067382461301008, 40.78355318730610435, -3.695724402018718546 ) ) ;
#22689 = CARTESIAN_POINT ( 'NONE',  ( -32.97666635132488011, 94.88921800892812541, 43.93259070532314325 ) ) ;
#22690 = CARTESIAN_POINT ( 'NONE',  ( -7.521556465916529710, 24.12430647450515053, 10.00000000000000000 ) ) ;
#22691 = CARTESIAN_POINT ( 'NONE',  ( 174.1511926551437170, 259.1985027499044918, -14.38432268034557993 ) ) ;
#22692 = LINE ( 'NONE', #60163, #79293 ) ;
#22693 = CARTESIAN_POINT ( 'NONE',  ( 52.25428207639063061, 207.6427522451419350, -10.00000000000009592 ) ) ;
#22694 = CARTESIAN_POINT ( 'NONE',  ( 155.6518451030846961, 261.0500913200531841, 17.91778754207898317 ) ) ;
#22695 = CARTESIAN_POINT ( 'NONE',  ( 70.73151905446071908, 61.43491590206733832, -14.82309597659894429 ) ) ;
#22696 = B_SPLINE_CURVE_WITH_KNOTS ( 'NONE', 3,
 ( #29096, #27605, #81827, #81335, #43770, #97510, #73697, #28082, #58471, #13879, #44761, #6280, #74714, #4281, #90437, #11909, #90934, #21484, #58952, #20502, #36171, #28577, #68072, #5291, #98996, #91411, #21975, #35180, #66090, #97036, #89444 ),
 .UNSPECIFIED., .F., .F.,
 ( 4, 3, 3, 3, 3, 3, 3, 3, 3, 3, 4 ),
 ( 0.000000000000000000, 0.1333490885032276307, 0.3007194338854349835, 0.4699862290245034879, 0.5844252810809318355, 0.6686540514502756771, 0.7354980260655390456, 0.8028463152565503691, 0.8633854507757023899, 0.9437142632666907227, 1.000000000000000000 ),
 .UNSPECIFIED. ) ;
#22697 = CARTESIAN_POINT ( 'NONE',  ( 82.48332016352127027, 53.47388482021811740, -15.74481631320921693 ) ) ;
#22698 = CARTESIAN_POINT ( 'NONE',  ( 76.00665944866153723, 220.8149278399160664, 9.188101187500093303 ) ) ;
#22699 = CARTESIAN_POINT ( 'NONE',  ( 159.7132918459648181, 254.0154592091499239, -16.90058287995827158 ) ) ;
#22700 = CARTESIAN_POINT ( 'NONE',  ( 193.2140586456748679, 295.9904290195353269, -12.67640480829088823 ) ) ;
#22701 = CARTESIAN_POINT ( 'NONE',  ( 163.4178923001155681, 247.5989030008181260, -10.38047187240561442 ) ) ;
#22702 = EDGE_CURVE ( 'NONE', #40435, #31854, #42813, .T. ) ;
#22703 = CARTESIAN_POINT ( 'NONE',  ( 197.2380956165551709, 287.7323366031149021, -17.26490520431893572 ) ) ;
#22704 = CARTESIAN_POINT ( 'NONE',  ( 207.1770866921659717, 271.8057550155037347, -5.569195235244989384 ) ) ;
#22705 = DIRECTION ( 'NONE',  ( -0.000000000000000000, -0.000000000000000000, -1.000000000000000000 ) ) ;
#22707 = CARTESIAN_POINT ( 'NONE',  ( -20.78227252765418953, 95.22040553774976956, 45.19937671356586861 ) ) ;
#22706 = CARTESIAN_POINT ( 'NONE',  ( 99.93749413994396491, 240.0530062829862743, -4.648177544792955347E-16 ) ) ;
#22708 = FILL_AREA_STYLE ('',( #6003 ) ) ;
#22709 = PLANE ( 'NONE',  #89665 ) ;
#22710 = CARTESIAN_POINT ( 'NONE',  ( 205.5937218600166432, 274.5482233517041095, -12.97537981636971338 ) ) ;
#22711 = CARTESIAN_POINT ( 'NONE',  ( 157.2333142128019858, 258.3109064714224132, 16.87956768598436597 ) ) ;
#22712 = CARTESIAN_POINT ( 'NONE',  ( 72.15692581984221476, 72.29159277512509618, 3.751890296296640059 ) ) ;
#22713 = CARTESIAN_POINT ( 'NONE',  ( 54.35637144981559743, 196.0643266524159856, -9.188101187500093303 ) ) ;
#22714 = CARTESIAN_POINT ( 'NONE',  ( 157.7233946900069839, 257.4620621851055375, 16.86796251324260254 ) ) ;
#22716 = EDGE_CURVE ( 'NONE', #18420, #93728, #74964, .T. ) ;
#22715 = CARTESIAN_POINT ( 'NONE',  ( 180.1168005803277481, 295.2192856762299016, -2.191971455912026467 ) ) ;
#22717 = CARTESIAN_POINT ( 'NONE',  ( 82.59751384975028543, 49.84330820394566786, -13.79983639419522312 ) ) ;
#22718 = CARTESIAN_POINT ( 'NONE',  ( 150.8371008641169908, 248.7048013555409511, 4.594050593750051981 ) ) ;
#22719 = LINE ( 'NONE', #100230, #58699 ) ;
#22720 = CARTESIAN_POINT ( 'NONE',  ( 26.73894555032740783, 17.29860640527292759, -2.839279412974138328 ) ) ;
#22721 = CARTESIAN_POINT ( 'NONE',  ( 150.6916211261701619, 269.6414512649903941, -15.44346024757110847 ) ) ;
#22722 = CARTESIAN_POINT ( 'NONE',  ( 196.8104339078508076, 289.7613243423628546, -16.40335862274955403 ) ) ;
#22723 = CARTESIAN_POINT ( 'NONE',  ( 8.064688198948626763, 22.84336893147754211, -7.433330006724137462 ) ) ;
#22724 = CARTESIAN_POINT ( 'NONE',  ( 185.9427433571077586, 257.7868782628476083, -2.501399907045548598 ) ) ;
#22725 = CARTESIAN_POINT ( 'NONE',  ( 76.98684284838461167, 63.68060895951392553, 15.36346902396294745 ) ) ;
#22726 = CARTESIAN_POINT ( 'NONE',  ( -13.99899119970020145, 104.8759001898749688, 43.88975813191157016 ) ) ;
#22727 = CARTESIAN_POINT ( 'NONE',  ( 198.4334039703542771, 286.9502577349437615, 18.47706603442866680 ) ) ;
#22728 = CARTESIAN_POINT ( 'NONE',  ( 82.44105267360316702, 40.97854391121963147, -1.240873595747258529 ) ) ;
#22729 = CARTESIAN_POINT ( 'NONE',  ( 152.3777131358734209, 276.3565970158849154, 7.198581938326709562 ) ) ;
#22730 = ADVANCED_FACE ( 'NONE', ( #22020 ), #73745, .F. ) ;
#22731 = EDGE_CURVE ( 'NONE', #87101, #29478, #89971, .T. ) ;
#22732 = CARTESIAN_POINT ( 'NONE',  ( 76.13179367649587448, 56.49312099246306929, -16.15038315265565672 ) ) ;
#22733 = CARTESIAN_POINT ( 'NONE',  ( 87.79271458260285499, 45.16522989489592987, -6.842624051142037089 ) ) ;
#22734 = CARTESIAN_POINT ( 'NONE',  ( 121.2656814440110935, 227.4865022471901455, 1.119607411625061291E-15 ) ) ;
#22735 = CARTESIAN_POINT ( 'NONE',  ( 181.1866291719431104, 292.1633450213508922, -10.35974650001995556 ) ) ;
#22736 = CARTESIAN_POINT ( 'NONE',  ( 192.9105100888655500, 284.4402630435000674, -16.74955499512010348 ) ) ;
#22737 = VERTEX_POINT ( 'NONE', #59509 ) ;
#22738 = CARTESIAN_POINT ( 'NONE',  ( 50.23025173566475132, 97.10399052176643409, 10.00000000000000000 ) ) ;
#22739 = EDGE_LOOP ( 'NONE', ( #48710, #69821, #6910, #66880 ) ) ;
#22740 = CARTESIAN_POINT ( 'NONE',  ( 159.2289198208967775, 254.8544161663325838, -15.88961297684315888 ) ) ;
#22741 = CARTESIAN_POINT ( 'NONE',  ( 187.0639549125049541, 276.7591803672281117, -16.89325600899905666 ) ) ;
#22742 = CARTESIAN_POINT ( 'NONE',  ( -63.08903959183645327, 39.77784189046417396, -10.00000000000000000 ) ) ;
#22743 = ORIENTED_EDGE ( 'NONE', *, *, #49267, .T. ) ;
#22744 = CARTESIAN_POINT ( 'NONE',  ( 60.71607196274899110, 215.8615022471903160, 5.000000000000046185 ) ) ;
#22745 = CARTESIAN_POINT ( 'NONE',  ( 79.06774487169295185, 46.04232138122480933, -12.65057773476749858 ) ) ;
#22746 = CARTESIAN_POINT ( 'NONE',  ( 194.1852025340051284, 294.3083584634874796, -15.46421316575964688 ) ) ;
#22747 = CARTESIAN_POINT ( 'NONE',  ( 177.1176718376224244, 274.7376581003516094, -16.86326964924343130 ) ) ;
#22748 = DIRECTION ( 'NONE',  ( 0.4999999999999998890, -0.8660254037844385966, 0.000000000000000000 ) ) ;
#22749 = ORIENTED_EDGE ( 'NONE', *, *, #82386, .F. ) ;
#22750 = B_SPLINE_CURVE_WITH_KNOTS ( 'NONE', 3,
 ( #20168, #51035, #74871, #35848, #5453, #42919, #67240, #98170, #52048, #59628, #81992, #52533, #97675, #91085, #74383, #82986, #6452, #13562, #44434, #35347, #75367, #58145, #5947, #28242, #36840, #68232, #67749, #98673, #29254, #21650, #83483, #44927, #43440, #37330, #12565, #89125, #19677, #12063, #62112, #39802, #15022, #93059, #45913, #54507, #23614, #7949, #78354, #53033 ),
 .UNSPECIFIED., .F., .F.,
 ( 4, 2, 2, 2, 2, 2, 2, 2, 2, 2, 2, 2, 2, 2, 2, 2, 2, 2, 2, 2, 2, 2, 2, 4 ),
 ( 0.0004852726061935422742, 0.0009346415430110950173, 0.001159326011419822573, 0.001384010479828550128, 0.001496352714032899486, 0.001608694948237248843, 0.001833379416645954932, 0.002282748353463394646, 0.003181486227098212494, 0.004080224100733030775, 0.004978961974367849055, 0.005428330911185216996, 0.005653015379593942166, 0.005765357613798340747, 0.005821528730900540904, 0.005877699848002740195, 0.005933870965104939485, 0.005990042082207139643, 0.006102384316411719502, 0.006327068784821065703, 0.006776437721639757238, 0.007225806658458449640, 0.007450491126867776759, 0.007675175595277103878 ),
 .UNSPECIFIED. ) ;
#22751 = CARTESIAN_POINT ( 'NONE',  ( 16.26188567080226477, 32.49540643055187417, 3.479690158560446702E-15 ) ) ;
#22752 = LINE ( 'NONE', #1462, #40313 ) ;
#22753 = CARTESIAN_POINT ( 'NONE',  ( 75.11209585957564627, 67.04221104021077338, -12.68919168548209342 ) ) ;
#22754 = ORIENTED_EDGE ( 'NONE', *, *, #84816, .T. ) ;
#22755 = DIRECTION ( 'NONE',  ( 0.4556638457577293910, 0.000000000000000000, 0.8901519306664880116 ) ) ;
#22756 = B_SPLINE_CURVE_WITH_KNOTS ( 'NONE', 3,
 ( #96056, #10924, #71732, #63104, #33207, #80865, #24602, #72745, #11439, #64616, #42291, #64106, #25617, #18025, #10418, #79854 ),
 .UNSPECIFIED., .F., .F.,
 ( 4, 2, 2, 2, 2, 2, 2, 4 ),
 ( 8.673617379884035472E-19, 0.0003786681000627679949, 0.0007573362001255351224, 0.001136004300188302304, 0.001514672400251069377, 0.001893340500313836451, 0.002272008600376603741, 0.003029344800502137888 ),
 .UNSPECIFIED. ) ;
#22757 = CARTESIAN_POINT ( 'NONE',  ( -1.367124174595798713, 160.0177522451418213, 5.000000000000051514 ) ) ;
#22758 = ORIENTED_EDGE ( 'NONE', *, *, #37319, .F. ) ;
#22759 = AXIS2_PLACEMENT_3D ( 'NONE', #37191, #68093, #99015 ) ;
#22760 = CARTESIAN_POINT ( 'NONE',  ( 173.1024016144300504, 285.3904325752632758, 10.53327312915123493 ) ) ;
#22761 = EDGE_CURVE ( 'NONE', #16006, #44175, #74762, .T. ) ;
#22763 = CARTESIAN_POINT ( 'NONE',  ( 67.73377762630668997, 65.63987058315933609, -10.78464639375587453 ) ) ;
#22762 = CARTESIAN_POINT ( 'NONE',  ( 72.19508862719266062, 67.24605117460401971, 11.71507738192612535 ) ) ;
#22764 = CARTESIAN_POINT ( 'NONE',  ( 162.6396274730868186, 248.9468972229755082, -10.26162218571527518 ) ) ;
#22765 = CARTESIAN_POINT ( 'NONE',  ( 164.4272222519600746, 245.8506922426221593, 7.021336339662529902 ) ) ;
#22766 = CARTESIAN_POINT ( 'NONE',  ( 160.0072461633487535, 253.5063153963366744, 16.23938890643736244 ) ) ;
#22767 = CARTESIAN_POINT ( 'NONE',  ( 161.0258333705537552, 262.9627432743089344, -17.59774463166796465 ) ) ;
#22768 = LINE ( 'NONE', #9580, #86824 ) ;
#22769 = CARTESIAN_POINT ( 'NONE',  ( 177.6687795445700999, 268.6483195260574917, 16.58452684940672484 ) ) ;
#22770 = CARTESIAN_POINT ( 'NONE',  ( 195.5801065724998580, 291.4439665296084740, -15.68012860244166440 ) ) ;
#22771 = CARTESIAN_POINT ( 'NONE',  ( 72.21814540286966633, 206.3768266524159856, -9.188101187500091527 ) ) ;
#22772 = ORIENTED_EDGE ( 'NONE', *, *, #71251, .T. ) ;
#22773 = CARTESIAN_POINT ( 'NONE',  ( 170.3956142831928275, 263.8003389354304886, 15.85802135508393107 ) ) ;
#22774 = CARTESIAN_POINT ( 'NONE',  ( 167.2900023830132170, 283.1360949131732809, -11.47530909209802275 ) ) ;
#22775 = ORIENTED_EDGE ( 'NONE', *, *, #88991, .F. ) ;
#22776 = PLANE ( 'NONE',  #956 ) ;
#22777 = ORIENTED_EDGE ( 'NONE', *, *, #54639, .F. ) ;
#22778 = FACE_BOUND ( 'NONE', #27557, .T. ) ;
#22779 = CARTESIAN_POINT ( 'NONE',  ( 66.97470778035078354, 67.57858517361454176, 6.667077613036518358 ) ) ;
#22780 = ADVANCED_FACE ( 'NONE', ( #5340 ), #98048, .T. ) ;
#22781 = CARTESIAN_POINT ( 'NONE',  ( 194.3503960779362956, 284.8058050914982573, 17.28495561203828146 ) ) ;
#22782 = CARTESIAN_POINT ( 'NONE',  ( 191.3041230083617563, 299.2985345825480863, -9.819045872446528378 ) ) ;
#22783 = CARTESIAN_POINT ( 'NONE',  ( 81.17822002178407104, 55.59913327053874355, 16.37131925982175318 ) ) ;
#22784 = CARTESIAN_POINT ( 'NONE',  ( 193.7114073116034945, 295.1289958610702797, 14.86160832869823345 ) ) ;
#22785 = CARTESIAN_POINT ( 'NONE',  ( 71.83756684404445991, 67.75224793704757076, 10.40286433491243656 ) ) ;
#22786 = CARTESIAN_POINT ( 'NONE',  ( 79.98487687335507701, 226.1744531367911293, 4.594050593750047540 ) ) ;
#22787 = EDGE_LOOP ( 'NONE', ( #76211, #50391, #14278, #90324 ) ) ;
#22788 = CARTESIAN_POINT ( 'NONE',  ( 161.5034534227228562, 250.9148084044473990, -12.72651426731975732 ) ) ;
#22789 = VERTEX_POINT ( 'NONE', #90977 ) ;
#22790 = CARTESIAN_POINT ( 'NONE',  ( 76.27683532132236621, 51.60822212622871774, -15.67723923137847386 ) ) ;
#22791 = CARTESIAN_POINT ( 'NONE',  ( 76.28360139951196572, 65.00893075233551599, -14.26754816652215219 ) ) ;
#22792 = ADVANCED_FACE ( 'NONE', ( #21537 ), #83365, .T. ) ;
#22793 = CARTESIAN_POINT ( 'NONE',  ( 206.1215120922853146, 273.6340638536760821, 10.12238414215620885 ) ) ;
#22794 = CARTESIAN_POINT ( 'NONE',  ( 32.30839531297598910, 123.0650415295850593, -40.00000000000000000 ) ) ;
#22795 = CARTESIAN_POINT ( 'NONE',  ( 195.3365262966702289, 279.2463014027769646, 16.32157205693540192 ) ) ;
#22796 = CARTESIAN_POINT ( 'NONE',  ( 161.1581524785962642, 260.6267798172495986, 16.70816614512294862 ) ) ;
#22797 = ORIENTED_EDGE ( 'NONE', *, *, #38969, .T. ) ;
#22798 = CARTESIAN_POINT ( 'NONE',  ( 88.26308438319264837, 44.34169033064829080, 4.149168146237482979 ) ) ;
#22799 = CARTESIAN_POINT ( 'NONE',  ( 156.7165066408136909, 274.2344053129649524, 13.65978042195306585 ) ) ;
#22800 = CARTESIAN_POINT ( 'NONE',  ( 161.9461893331167914, 280.9078031139047198, -10.53061385661272276 ) ) ;
#22801 = CARTESIAN_POINT ( 'NONE',  ( 201.3715986869907510, 281.8611552031986776, -17.89433714524984964 ) ) ;
#22802 = CARTESIAN_POINT ( 'NONE',  ( 79.48254265572808208, 59.20565343284910398, -16.22433428824159662 ) ) ;
#22803 = CARTESIAN_POINT ( 'NONE',  ( -19.65312891409030271, 93.06504152958497400, -10.00000000000000888 ) ) ;
#22804 = EDGE_LOOP ( 'NONE', ( #43817, #72902, #87127, #30741 ) ) ;
#22805 = CARTESIAN_POINT ( 'NONE',  ( 195.8898456738714060, 265.0745416412873965, 5.322143108867450678 ) ) ;
#22806 = CARTESIAN_POINT ( 'NONE',  ( 181.8076198581489393, 291.5803737294537541, 10.22569155168986299 ) ) ;
#22807 = DIRECTION ( 'NONE',  ( 0.09248003802711830812, -0.9957145386939485476, 0.000000000000000000 ) ) ;
#22808 = CARTESIAN_POINT ( 'NONE',  ( 184.5976612927380245, 263.6176899794377846, -12.36297651287966204 ) ) ;
#22809 = CARTESIAN_POINT ( 'NONE',  ( 198.9491760152053530, 265.4618440174380680, 1.652013691215429736 ) ) ;
#22810 = ORIENTED_EDGE ( 'NONE', *, *, #62989, .F. ) ;
#22811 = CARTESIAN_POINT ( 'NONE',  ( 190.8957779480239765, 300.0058089740729770, -4.541438514207768229 ) ) ;
#22812 = CARTESIAN_POINT ( 'NONE',  ( -13.80441806700167007, 103.9794969232740272, 43.95776411517724824 ) ) ;
#22813 = DIRECTION ( 'NONE',  ( 0.5000000000000048850, -0.8660254037844358210, 0.000000000000000000 ) ) ;
#22815 = CARTESIAN_POINT ( 'NONE',  ( 73.72034998377742454, 55.25731110591803485, 16.59469895887937341 ) ) ;
#22814 = CARTESIAN_POINT ( 'NONE',  ( 169.8069776206597226, 261.6727971985682757, -16.70353856883196286 ) ) ;
#22816 = CARTESIAN_POINT ( 'NONE',  ( 29.44299306155908624, 19.12755873383627403, -6.180339887498949025 ) ) ;
#22817 = CARTESIAN_POINT ( 'NONE',  ( 19.39713158799116499, 193.5530062829863311, -4.648177544792955347E-16 ) ) ;
#22818 = CARTESIAN_POINT ( 'NONE',  ( 162.7666423248381022, 284.7022503539437253, -3.997099778975750528 ) ) ;
#22819 = CARTESIAN_POINT ( 'NONE',  ( -72.39633208959961053, 47.04162880533178992, -10.00000000000000000 ) ) ;
#22820 = CARTESIAN_POINT ( 'NONE',  ( 159.6898930778639283, 254.0559870643349143, 16.90891900388599822 ) ) ;
#22821 = CARTESIAN_POINT ( 'NONE',  ( 148.3831018964633870, 243.1427522451417644, 1.119607411625061291E-15 ) ) ;
#22822 = DIRECTION ( 'NONE',  ( 0.8755176446346986108, -0.4831861483251662648, 0.000000000000000000 ) ) ;
#22823 = ORIENTED_EDGE ( 'NONE', *, *, #97348, .T. ) ;
#22824 = CARTESIAN_POINT ( 'NONE',  ( 178.8060443869409539, 256.5898062107611963, 8.688066605584527480 ) ) ;
#22825 = CARTESIAN_POINT ( 'NONE',  ( 72.71270868682043442, 70.26182901474604137, -8.036085614855659642 ) ) ;
#22826 = CARTESIAN_POINT ( 'NONE',  ( 81.58025826021204807, 41.65040128036911682, 5.760828700905646471 ) ) ;
#22827 = CARTESIAN_POINT ( 'NONE',  ( 12.62459875707045143, 178.0958772461660544, -9.188101187500095079 ) ) ;
#22828 = CARTESIAN_POINT ( 'NONE',  ( 30.05030659499110968, 29.30066082961423746, -10.00000000000000533 ) ) ;
#22829 = CARTESIAN_POINT ( 'NONE',  ( 81.78504375891562006, 41.48292696562020865, -5.073134180756075473 ) ) ;
#22830 = CARTESIAN_POINT ( 'NONE',  ( 170.0816090270627683, 270.7169371497489010, -17.26929808975160796 ) ) ;
#22831 = CARTESIAN_POINT ( 'NONE',  ( 179.2598940579185580, 287.6958704249323091, 13.53542817836178003 ) ) ;
#22832 = PLANE ( 'NONE',  #31153 ) ;
#22833 = CARTESIAN_POINT ( 'NONE',  ( 191.4420812244453600, 260.8157448279923187, -1.331758356259544085 ) ) ;
#22834 = ADVANCED_FACE ( 'NONE', ( #8816 ), #6823, .T. ) ;
#22835 = EDGE_CURVE ( 'NONE', #85740, #37839, #63017, .T. ) ;
#22836 = CARTESIAN_POINT ( 'NONE',  ( 70.17018262072913615, 217.9865022471902876, 10.00000000000009237 ) ) ;
#22837 = CARTESIAN_POINT ( 'NONE',  ( 68.31414817410235685, 198.7012482093460335, 5.278111984874361800E-14 ) ) ;
#22838 = CARTESIAN_POINT ( 'NONE',  ( 148.3280470635002928, 273.7352816289870248, 9.058704604771318003 ) ) ;
#22839 = EDGE_CURVE ( 'NONE', #43149, #78972, #54390, .T. ) ;
#22840 = CARTESIAN_POINT ( 'NONE',  ( 26.64321143294855077, 192.3149278399161233, 9.188101187500093303 ) ) ;
#22841 = DIRECTION ( 'NONE',  ( -0.7845058662180028897, -0.6201213960746241316, 0.000000000000000000 ) ) ;
#22842 = EDGE_CURVE ( 'NONE', #82272, #97333, #99717, .T. ) ;
#22843 =( NAMED_UNIT ( * ) SI_UNIT ( $, .STERADIAN. ) SOLID_ANGLE_UNIT ( ) );
#22844 = CARTESIAN_POINT ( 'NONE',  ( 34.45502471548058310, 41.93396525600392977, 2.839279412974139660 ) ) ;
#22845 = FACE_OUTER_BOUND ( 'NONE', #49303, .T. ) ;
#22846 = CARTESIAN_POINT ( 'NONE',  ( 207.1601050488701503, 271.8351680844880889, 6.320235450527015075 ) ) ;
#22847 = CARTESIAN_POINT ( 'NONE',  ( 185.8037470671009714, 266.7899001189457522, 13.20055515182332684 ) ) ;
#22848 = CARTESIAN_POINT ( 'NONE',  ( 163.1981911828994498, 281.1124743395109817, -10.20120161817862581 ) ) ;
#22849 = CARTESIAN_POINT ( 'NONE',  ( 160.4111170237447084, 280.0480387167077083, 9.177741064962299689 ) ) ;
#22850 = CARTESIAN_POINT ( 'NONE',  ( 17.35762855594305520, 30.99752408145591431, 5.678558825948277544 ) ) ;
#22851 = CARTESIAN_POINT ( 'NONE',  ( 6.386372903753387398, 27.18528772668516069, -1.583844403245363575 ) ) ;
#22852 = CARTESIAN_POINT ( 'NONE',  ( 72.04081558064058299, 59.27854915901136934, 15.84716367784278646 ) ) ;
#22853 = CARTESIAN_POINT ( 'NONE',  ( 155.2695601165254402, 261.7122283397445131, 16.98599069618989077 ) ) ;
#22854 = VERTEX_POINT ( 'NONE', #91976 ) ;
#22855 = CARTESIAN_POINT ( 'NONE',  ( 81.47170367160930482, 45.92781089733199451, -12.16060789928866193 ) ) ;
#22856 = CARTESIAN_POINT ( 'NONE',  ( 79.14312167556931854, 57.64441083166269664, 0.000000000000000000 ) ) ;
#22857 = CARTESIAN_POINT ( 'NONE',  ( 81.40183131072419087, 42.44732485736221150, 7.480571600138957500 ) ) ;
#22858 = CARTESIAN_POINT ( 'NONE',  ( 158.6884840273770010, 272.1760528269434189, 15.70102783839913840 ) ) ;
#22859 = ORIENTED_EDGE ( 'NONE', *, *, #15139, .F. ) ;
#22860 = PLANE ( 'NONE',  #39248 ) ;
#22861 = CARTESIAN_POINT ( 'NONE',  ( 72.59758381146951933, 71.34453924857655238, -5.950632915609824103 ) ) ;
#22862 = CARTESIAN_POINT ( 'NONE',  ( 72.67827274082560507, 57.12963284915914386, 16.37181230888942096 ) ) ;
#22863 = CARTESIAN_POINT ( 'NONE',  ( 84.01948337656611443, 41.51492700183946738, 2.577254461289238741 ) ) ;
#22864 = ORIENTED_EDGE ( 'NONE', *, *, #98844, .F. ) ;
#22865 = ORIENTED_EDGE ( 'NONE', *, *, #17098, .F. ) ;
#22867 = DIRECTION ( 'NONE',  ( -0.000000000000000000, 0.000000000000000000, 1.000000000000000000 ) ) ;
#22866 = LINE ( 'NONE', #5678, #71370 ) ;
#22868 = ORIENTED_EDGE ( 'NONE', *, *, #81465, .T. ) ;
#22869 = CARTESIAN_POINT ( 'NONE',  ( 190.8860811105559208, 300.0226043892405414, 8.636347304323541252 ) ) ;
#22870 = CARTESIAN_POINT ( 'NONE',  ( 20.92694685269868771, 35.58029201028043076, 1.583844403245363353 ) ) ;
#22871 = CARTESIAN_POINT ( 'NONE',  ( 80.03821161748030022, 58.13657998254147685, 16.26793327978904458 ) ) ;
#22872 = DIRECTION ( 'NONE',  ( 0.3693965786901519111, -0.9292718480896805522, 0.000000000000000000 ) ) ;
#22873 = ORIENTED_EDGE ( 'NONE', *, *, #84999, .T. ) ;
#22874 = CARTESIAN_POINT ( 'NONE',  ( 147.6207754342248961, 274.9603120256437592, 8.795690793376332195 ) ) ;
#22875 = VERTEX_POINT ( 'NONE', #39685 ) ;
#22876 = CARTESIAN_POINT ( 'NONE',  ( 35.56482384635839367, 110.6301519124606756, 59.99999999999999289 ) ) ;
#22877 = CARTESIAN_POINT ( 'NONE',  ( 158.3316779918856696, 265.2189361393055833, 17.13948956058090545 ) ) ;
#22878 = ORIENTED_EDGE ( 'NONE', *, *, #41896, .F. ) ;
#22879 = CARTESIAN_POINT ( 'NONE',  ( 190.6893905452545823, 300.3632824417117604, 3.294993852933539191 ) ) ;
#22880 = FACE_OUTER_BOUND ( 'NONE', #67161, .T. ) ;
#22881 = ORIENTED_EDGE ( 'NONE', *, *, #12141, .T. ) ;
#22882 = CARTESIAN_POINT ( 'NONE',  ( -13.14444822889210762, 72.23936417694854129, 14.22349210779893625 ) ) ;
#22883 = CARTESIAN_POINT ( 'NONE',  ( 142.9371257517045137, 259.7655487066560340, -7.305945665944389766 ) ) ;
#22884 = CARTESIAN_POINT ( 'NONE',  ( -17.26243516413818924, 24.35187462261283997, 10.00000000000000000 ) ) ;
#22885 = DIRECTION ( 'NONE',  ( -0.2588190451027150840, -0.9659258262890161317, 8.659560562356675748E-17 ) ) ;
#22886 = ORIENTED_EDGE ( 'NONE', *, *, #63187, .T. ) ;
#22887 = VERTEX_POINT ( 'NONE', #92461 ) ;
#22888 = CARTESIAN_POINT ( 'NONE',  ( 190.8422434538341861, 299.4678640767844513, 6.131100907076111106 ) ) ;
#22889 = DIRECTION ( 'NONE',  ( -0.8660254037844387076, -0.4999999999999998890, -0.000000000000000000 ) ) ;
#22890 = CARTESIAN_POINT ( 'NONE',  ( 169.7005567072155259, 288.7155782076579271, 4.430715832634252394 ) ) ;
#22891 = CARTESIAN_POINT ( 'NONE',  ( 189.9462859318020946, 301.6503773875500087, -1.164147598593831656 ) ) ;
#22892 = CARTESIAN_POINT ( 'NONE',  ( 149.6036070299368532, 271.5259469590175740, 11.63513718912356865 ) ) ;
#22893 = CARTESIAN_POINT ( 'NONE',  ( 170.6523519555879034, 275.2952615463115649, -16.30984520614018507 ) ) ;
#22894 = CARTESIAN_POINT ( 'NONE',  ( 191.0517893919347614, 299.7355892266572255, 9.200480906495027256 ) ) ;
#22895 = CARTESIAN_POINT ( 'NONE',  ( 147.1731211915891322, 275.7356719181125868, 0.5879280619134324981 ) ) ;
#22896 = CARTESIAN_POINT ( 'NONE',  ( 163.2687272288607403, 257.7479913314281816, 15.56745367196672092 ) ) ;
#22897 = EDGE_CURVE ( 'NONE', #6222, #32604, #100260, .T. ) ;
#22898 = CARTESIAN_POINT ( 'NONE',  ( 69.56645282547259512, 66.75238641213026369, 10.02794500564488445 ) ) ;
#22900 = DIRECTION ( 'NONE',  ( 0.000000000000000000, -0.000000000000000000, -1.000000000000000000 ) ) ;
#22899 = CARTESIAN_POINT ( 'NONE',  ( 196.6288634187112052, 290.0758136547079289, -16.31544900032282186 ) ) ;
#22901 = CARTESIAN_POINT ( 'NONE',  ( 73.74091326739588226, 64.78503309551670952, -13.53863873432484155 ) ) ;
#22902 = CARTESIAN_POINT ( 'NONE',  ( 78.75079241178771383, 47.65652836985446328, 14.29454575176127840 ) ) ;
#22903 = ORIENTED_EDGE ( 'NONE', *, *, #93627, .T. ) ;
#22904 = CARTESIAN_POINT ( 'NONE',  ( 190.5823735273246200, 300.5486413540409103, -3.280301628010032111 ) ) ;
#22905 = CARTESIAN_POINT ( 'NONE',  ( 36.38358746446922254, 51.11404133282111673, -10.00000000000000000 ) ) ;
#22906 = CARTESIAN_POINT ( 'NONE',  ( 87.62838477539726512, 44.93552847577709031, -6.577990587745525808 ) ) ;
#22907 = CARTESIAN_POINT ( 'NONE',  ( 79.49445812923981691, 46.35745038683718633, 12.69593692779722538 ) ) ;
#22908 = CARTESIAN_POINT ( 'NONE',  ( 179.6007985214840801, 282.9056516878069374, -15.77944700681856460 ) ) ;
#22909 = CARTESIAN_POINT ( 'NONE',  ( 81.46918866590169728, 53.89730630895333974, -16.01726311077535669 ) ) ;
#22910 = CARTESIAN_POINT ( 'NONE',  ( 169.0589559950515763, 284.9876656434325355, -7.953138351973477072 ) ) ;
#22911 = ORIENTED_EDGE ( 'NONE', *, *, #54935, .F. ) ;
#22912 = CARTESIAN_POINT ( 'NONE',  ( 162.6425574510925003, 248.9418223522047526, -10.70838742014210077 ) ) ;
#22914 = ADVANCED_FACE ( 'NONE', ( #93461 ), #24014, .F. ) ;
#22913 = CARTESIAN_POINT ( 'NONE',  ( 72.24104924332462474, 71.74196171561413848, 5.528620549063446354 ) ) ;
#22915 = CARTESIAN_POINT ( 'NONE',  ( 52.39861964368810732, 194.3927522451417929, -10.00000000000009059 ) ) ;
#22916 = CARTESIAN_POINT ( 'NONE',  ( 133.0835800865360170, 238.4548013555409796, -4.594050593750042211 ) ) ;
#22917 = FACE_OUTER_BOUND ( 'NONE', #44197, .T. ) ;
#22918 = CARTESIAN_POINT ( 'NONE',  ( 172.9438399295877957, 262.8668947608421718, -16.49499919880818766 ) ) ;
#22919 = CARTESIAN_POINT ( 'NONE',  ( 157.8740713127050981, 257.2010826190796706, 17.31862062017425075 ) ) ;
#22920 = CARTESIAN_POINT ( 'NONE',  ( 176.0127109592394277, 252.6004560315867593, -4.768680066900455650 ) ) ;
#22921 = CARTESIAN_POINT ( 'NONE',  ( 39.63359248971512017, 199.8149278399161233, 9.188101187500093303 ) ) ;
#22922 = DIRECTION ( 'NONE',  ( 0.5000000000000013323, -0.8660254037844378194, 0.000000000000000000 ) ) ;
#22923 = CARTESIAN_POINT ( 'NONE',  ( 85.71994772693146558, 48.50907089644480408, -12.26219287530962454 ) ) ;
#22924 = ORIENTED_EDGE ( 'NONE', *, *, #8854, .T. ) ;
#22925 = CARTESIAN_POINT ( 'NONE',  ( 71.14213006355628011, 63.76511893021699962, 13.21577267896801544 ) ) ;
#22926 = CARTESIAN_POINT ( 'NONE',  ( 177.9596406573189427, 265.6046161183090248, 15.53676538602235269 ) ) ;
#22927 = B_SPLINE_SURFACE_WITH_KNOTS ( 'NONE', 3, 1, ( 
 ( #25017, #34621 ),
 ( #64028, #25534 ),
 ( #27037, #56422 ),
 ( #80274, #40713 ),
 ( #86386, #88395 ),
 ( #94464, #87418 ),
 ( #72148, #49334 ),
 ( #33127, #55897 ),
 ( #95979, #9331 ),
 ( #86891, #65521 ),
 ( #42213, #17425 ),
 ( #47807, #95493 ),
 ( #71656, #10839 ),
 ( #48334, #40203 ),
 ( #33642, #11359 ),
 ( #71149, #26541 ),
 ( #94970, #79777 ),
 ( #17946, #48845 ),
 ( #18445, #10342 ),
 ( #41208, #32627 ),
 ( #49828, #57414 ),
 ( #1748, #2752 ),
 ( #64534, #26044 ),
 ( #56914, #87901 ),
 ( #80785, #5713 ),
 ( #12847, #13334 ),
 ( #35620, #28016 ),
 ( #97444, #73634 ),
 ( #35115, #89861 ),
 ( #96974, #75622 ),
 ( #66519, #51302 ),
 ( #81761, #4736 ),
 ( #43200, #12335 ),
 ( #83244, #59901 ) ),
 .UNSPECIFIED., .T., .F., .F.,
 ( 4, 2, 2, 2, 2, 2, 2, 2, 2, 2, 2, 2, 2, 2, 2, 2, 4 ),
 ( 2, 2 ),
 ( 0.000000000000000000, 0.06250000000000000000, 0.1250000000000000000, 0.1875000000000000000, 0.2500000000000000000, 0.3125000000000000000, 0.3750000000000000000, 0.4375000000000000000, 0.5000000000000000000, 0.5625000000000000000, 0.6250000000000000000, 0.6875000000000000000, 0.7500000000000000000, 0.8125000000000000000, 0.8750000000000000000, 0.9375000000000000000, 1.000000000000000000 ),
 ( 0.000000000000000000, 1.000000000000000000 ),
 .UNSPECIFIED. ) ;
#22928 = B_SPLINE_CURVE_WITH_KNOTS ( 'NONE', 3,
 ( #8955, #94097, #32251, #61645, #84989, #9465, #69747, #79404, #77363, #86023, #32749, #39823, #54033, #9970, #48462, #86516, #7968, #23140, #30764, #55530, #62132, #87024, #69250, #63151, #77872, #15534, #54526, #358, #63653, #25146, #46434, #38841, #100178, #93078, #85507, #71275, #92594, #70754, #23634, #1367, #16054, #70246, #24648, #852, #47938, #31731 ),
 .UNSPECIFIED., .F., .F.,
 ( 4, 1, 2, 2, 1, 2, 2, 1, 1, 2, 2, 1, 1, 2, 2, 1, 1, 2, 2, 1, 1, 1, 2, 2, 1, 1, 1, 2, 2, 4 ),
 ( 0.000000000000000000, 0.06250000000000761891, 0.09375000000001204592, 0.1250000000000164591, 0.1875000000000217604, 0.2187500000000238420, 0.2500000000000258682, 0.3125000000000270894, 0.3437500000000293654, 0.3593750000000304756, 0.3750000000000315858, 0.4375000000000447420, 0.4687500000000518474, 0.4843750000000553446, 0.5000000000000587308, 0.5625000000000682787, 0.5937500000000717204, 0.6093750000000711653, 0.6250000000000706102, 0.6875000000000704992, 0.7187500000000703881, 0.7343750000000703881, 0.7421875000000709433, 0.7500000000000713873, 0.8125000000000638378, 0.8437500000000596190, 0.8593750000000576206, 0.8671875000000563993, 0.8750000000000552891, 1.000000000000000000 ),
 .UNSPECIFIED. ) ;
#22929 = LINE ( 'NONE', #69536, #59476 ) ;
#22930 = CARTESIAN_POINT ( 'NONE',  ( 166.0261724905091114, 252.1720833225167837, -12.65714730546942768 ) ) ;
#22931 = CARTESIAN_POINT ( 'NONE',  ( 5.181765596169280563, 27.61866642244642023, 177.5919119679930134 ) ) ;
#22932 = CARTESIAN_POINT ( 'NONE',  ( -71.61465314115659453, 63.06504152958490295, 203.6502102582797420 ) ) ;
#22933 = CARTESIAN_POINT ( 'NONE',  ( 182.1964890600146987, 262.8133727455790449, 12.68220177327409637 ) ) ;
#22934 = CARTESIAN_POINT ( 'NONE',  ( 112.0100349375168918, 242.1427522451419065, -10.00000000000009415 ) ) ;
#22935 = CARTESIAN_POINT ( 'NONE',  ( 41.03800390905408335, 35.64441083166263979, -10.00000000000000533 ) ) ;
#22936 = ORIENTED_EDGE ( 'NONE', *, *, #78821, .T. ) ;
#22937 = CARTESIAN_POINT ( 'NONE',  ( 163.1691520398773321, 248.0297337694385931, 11.21816141384514331 ) ) ;
#22938 = B_SPLINE_CURVE_WITH_KNOTS ( 'NONE', 3,
 ( #42895, #35321, #88595, #73344, #66233, #97170, #34814, #26240, #88097, #49526, #80479, #94494, #16452, #85929, #24552, #9361, #63058, #24055, #64568, #86926, #41242, #95525, #34167, #18474, #78776, #26070, #47350, #9883, #25054, #48367, #55929, #56946, #72693, #41749, #71181, #40740, #94000, #87932, #49361, #10371, #65059, #95006, #48873, #80305, #47836, #79807 ),
 .UNSPECIFIED., .F., .F.,
 ( 4, 1, 2, 2, 1, 2, 2, 1, 1, 2, 2, 1, 1, 2, 2, 1, 1, 2, 2, 1, 1, 1, 2, 2, 1, 1, 1, 2, 2, 4 ),
 ( 0.000000000000000000, 0.06250000000000634215, 0.09375000000001049161, 0.1250000000000146272, 0.1875000000000240918, 0.2187500000000283662, 0.2500000000000326406, 0.3125000000000425215, 0.3437500000000481282, 0.3593750000000495715, 0.3750000000000510703, 0.4375000000000504596, 0.4687500000000502376, 0.4843750000000494604, 0.5000000000000487388, 0.5625000000000442979, 0.5937500000000436318, 0.6093750000000419664, 0.6250000000000403011, 0.6875000000000366374, 0.7187500000000347500, 0.7343750000000338618, 0.7421875000000334177, 0.7500000000000329736, 0.8125000000000348610, 0.8437500000000348610, 0.8593750000000339728, 0.8671875000000327516, 0.8750000000000314193, 1.000000000000000000 ),
 .UNSPECIFIED. ) ;
#22939 = CARTESIAN_POINT ( 'NONE',  ( 162.8223739550644211, 248.6303710312858186, -11.16939803179192658 ) ) ;
#22940 = CARTESIAN_POINT ( 'NONE',  ( 17.63104780087548562, 190.1744531367911293, 4.594050593750047540 ) ) ;
#22941 = CARTESIAN_POINT ( 'NONE',  ( 12.03141808487008824, 12.11029122506292488, -8.090169943749478065 ) ) ;
#22942 = CARTESIAN_POINT ( 'NONE',  ( 196.2011903101464441, 273.6939821814302150, 14.92212602658747223 ) ) ;
#22943 = PLANE ( 'NONE',  #57782 ) ;
#22944 = CARTESIAN_POINT ( 'NONE',  ( 66.60661563016273590, 67.77273566365288104, -7.043189648870076702 ) ) ;
#22946 = CARTESIAN_POINT ( 'NONE',  ( 66.96803994030899787, 197.2202760586659736, -5.415160957724236172E-17 ) ) ;
#22945 = CARTESIAN_POINT ( 'NONE',  ( 174.7884235540875011, 286.3353386219461640, 10.46792632123525735 ) ) ;
#22947 = CARTESIAN_POINT ( 'NONE',  ( 208.2939409893161553, 269.8713066281881083, 2.523744790997269227 ) ) ;
#22948 = CARTESIAN_POINT ( 'NONE',  ( 73.06869489861219336, 57.16488433617836762, 16.39886474625613388 ) ) ;
#22949 = CARTESIAN_POINT ( 'NONE',  ( 51.02741275436270030, 200.2677522451418781, 10.00000000000009592 ) ) ;
#22950 = CARTESIAN_POINT ( 'NONE',  ( 8.494131180097229006, 27.83705186507752671, 3.090169943749475401 ) ) ;
#22951 =( BOUNDED_CURVE ( )  B_SPLINE_CURVE ( 2, ( #69868, #480, #54656, #85632, #16177, #47073, #77990, #70888, #35365 ),
 .UNSPECIFIED., .F., .T. ) 
 B_SPLINE_CURVE_WITH_KNOTS ( ( 3, 2, 2, 2, 3 ),
 ( 0.3991935483870967527, 0.4005376344086021279, 0.4032258064516128782, 0.4059139784946236285, 0.4072580645161290591 ),
 .UNSPECIFIED. ) 
 CURVE ( )  GEOMETRIC_REPRESENTATION_ITEM ( )  RATIONAL_B_SPLINE_CURVE ( ( 0.9330127018922194093, 0.9330127018922194093, 1.000000000000000000, 0.8660254037844387076, 1.000000000000000000, 0.8660254037844387076, 1.000000000000000000, 0.9330127018922179660, 0.9330127018922194093 ) ) 
 REPRESENTATION_ITEM ( '' )  );
#22952 = VERTEX_POINT ( 'NONE', #2241 ) ;
#22953 = CARTESIAN_POINT ( 'NONE',  ( 15.68275096595825246, 169.8615022471901739, 5.000000000000051514 ) ) ;
#22954 = CARTESIAN_POINT ( 'NONE',  ( 207.5195222358739784, 271.2126392554839640, 2.810970398613041432 ) ) ;
#22955 = CARTESIAN_POINT ( 'NONE',  ( 136.6287848093373043, 243.5643266524160140, 9.188101187500095079 ) ) ;
#22956 = CARTESIAN_POINT ( 'NONE',  ( 32.78250297933140445, 27.43085787977765477, -9.188101187500008038 ) ) ;
#22957 = CARTESIAN_POINT ( 'NONE',  ( 164.1341878931737313, 260.3349919959172780, -16.13799654372055059 ) ) ;
#22958 = EDGE_CURVE ( 'NONE', #24776, #39107, #28822, .T. ) ;
#22959 = CARTESIAN_POINT ( 'NONE',  ( 189.1600758314701238, 261.3976643428155171, 6.743524540470962947 ) ) ;
#22960 = CARTESIAN_POINT ( 'NONE',  ( 193.8652130780152731, 280.5836658925297229, -17.72338988841175933 ) ) ;
#22962 = CARTESIAN_POINT ( 'NONE',  ( 185.5475819381700546, 277.7404700938030260, -17.45495574986458109 ) ) ;
#22961 = CARTESIAN_POINT ( 'NONE',  ( 67.99021540693823340, 66.60164882251528695, 9.921589984831021169 ) ) ;
#22963 = CARTESIAN_POINT ( 'NONE',  ( 68.55207038212054727, 64.21588461577663054, 11.81441866468647994 ) ) ;
#22964 = ORIENTED_EDGE ( 'NONE', *, *, #42132, .T. ) ;
#22965 = LINE ( 'NONE', #37177, #53552 ) ;
#22966 =( NAMED_UNIT ( * ) SI_UNIT ( $, .STERADIAN. ) SOLID_ANGLE_UNIT ( ) );
#22967 = CARTESIAN_POINT ( 'NONE',  ( 5.396842180905148112, 18.51421378149916563, -9.188101187500004485 ) ) ;
#22968 = CARTESIAN_POINT ( 'NONE',  ( 156.5681255643642089, 279.9925795744871948, -5.322131134865745850 ) ) ;
#22969 = CARTESIAN_POINT ( 'NONE',  ( 16.17343562415726765, 11.19860640527290840, 2.839279412974134775 ) ) ;
#22970 = ORIENTED_EDGE ( 'NONE', *, *, #2899, .T. ) ;
#22971 = CARTESIAN_POINT ( 'NONE',  ( 159.9921098401940469, 253.5325322770800653, 16.01215344049969502 ) ) ;
#22972 = CARTESIAN_POINT ( 'NONE',  ( 168.1981980474926104, 282.0723965943072926, -10.92329350232336260 ) ) ;
#22973 = CARTESIAN_POINT ( 'NONE',  ( 69.78620060459685703, 62.54818963133106280, 13.43547245615845576 ) ) ;
#22974 = CARTESIAN_POINT ( 'NONE',  ( 200.8654040100879854, 282.2982806454822367, -16.59380369206422756 ) ) ;
#22975 = CARTESIAN_POINT ( 'NONE',  ( 48.81784752633560487, 86.82484054835779830, 10.00000000000000000 ) ) ;
#22976 = CARTESIAN_POINT ( 'NONE',  ( 149.7519917370995586, 271.6399139028688410, 11.58851940123675917 ) ) ;
#22977 = CARTESIAN_POINT ( 'NONE',  ( 162.7459776558209228, 248.7626933030860812, -9.895605163646791880 ) ) ;
#22978 = CARTESIAN_POINT ( 'NONE',  ( 153.1961624462112752, 265.3034584490234806, -16.19494717845262954 ) ) ;
#22979 = ORIENTED_EDGE ( 'NONE', *, *, #53690, .T. ) ;
#22980 = CARTESIAN_POINT ( 'NONE',  ( 191.1637967482625129, 281.0701639715127271, 16.65787912226990386 ) ) ;
#22981 = FACE_OUTER_BOUND ( 'NONE', #72870, .T. ) ;
#22982 = ORIENTED_EDGE ( 'NONE', *, *, #3450, .F. ) ;
#22983 = CARTESIAN_POINT ( 'NONE',  ( 149.3883679478359454, 271.8987519849911223, 12.99187507659642371 ) ) ;
#22984 = DIRECTION ( 'NONE',  ( 0.8434505012732891327, -0.5372068985985168910, 0.000000000000000000 ) ) ;
#22985 = CARTESIAN_POINT ( 'NONE',  ( 85.44270010841485430, 45.05997736202789383, -8.111341735673667230 ) ) ;
#22986 = ORIENTED_EDGE ( 'NONE', *, *, #57301, .F. ) ;
#22987 = CARTESIAN_POINT ( 'NONE',  ( 146.5913834600193582, 276.7432712258716947, -0.4909717733184599253 ) ) ;
#22988 = CARTESIAN_POINT ( 'NONE',  ( 78.99848661620950452, 60.24637179098724005, -16.44349368446546578 ) ) ;
#22989 = CARTESIAN_POINT ( 'NONE',  ( 149.7109319212262051, 271.3400547943878109, -12.38605961032017433 ) ) ;
#22991 = VECTOR ( 'NONE', #83105, 1000.000000000000227 ) ;
#22990 = CARTESIAN_POINT ( 'NONE',  ( 69.35874604783040809, 62.81868137753772174, 13.70911004653519250 ) ) ;
#22992 = ORIENTED_EDGE ( 'NONE', *, *, #61020, .F. ) ;
#22993 = CARTESIAN_POINT ( 'NONE',  ( 103.8820256808556906, 230.7833772461660544, -9.188101187500095079 ) ) ;
#22994 = CARTESIAN_POINT ( 'NONE',  ( 161.1089126327036354, 251.5981730984191529, 13.95161017039218976 ) ) ;
#22995 = CARTESIAN_POINT ( 'NONE',  ( 150.6931560952953646, 269.6387926204777727, 14.65021044537114037 ) ) ;
#22996 = CARTESIAN_POINT ( 'NONE',  ( 142.2974213780761090, 241.4155109091895781, 2.679491924311254714 ) ) ;
#22997 = VERTEX_POINT ( 'NONE', #55393 ) ;
#22998 = ORIENTED_EDGE ( 'NONE', *, *, #47829, .F. ) ;
#22999 = ORIENTED_EDGE ( 'NONE', *, *, #97908, .F. ) ;
#23000 = CARTESIAN_POINT ( 'NONE',  ( 80.31295028949705284, 46.37567276318792153, 12.40275564728421109 ) ) ;
#23001 = ORIENTED_EDGE ( 'NONE', *, *, #4555, .F. ) ;
#23002 = CARTESIAN_POINT ( 'NONE',  ( 67.73206951906773554, 67.71102699734191788, 7.258094484230766419 ) ) ;
#23003 = VERTEX_POINT ( 'NONE', #48325 ) ;
#23004 = CARTESIAN_POINT ( 'NONE',  ( 207.5195222358739784, 271.2126392554839640, 2.810970398613041432 ) ) ;
#23005 = CARTESIAN_POINT ( 'NONE',  ( 82.07162566433116524, 45.76690361501738380, 11.08599694920283341 ) ) ;
#23006 = CARTESIAN_POINT ( 'NONE',  ( 170.8277526913387021, 283.1399606207687043, 11.93616677736253351 ) ) ;
#23007 = CARTESIAN_POINT ( 'NONE',  ( 194.2154056360670040, 294.2560451561701029, -15.66696967429384557 ) ) ;
#23008 = CARTESIAN_POINT ( 'NONE',  ( 69.37941880040793308, 68.43494161156023381, -7.694138334527842460 ) ) ;
#23009 = EDGE_LOOP ( 'NONE', ( #65604, #87668, #40344, #94322 ) ) ;
#23010 = CARTESIAN_POINT ( 'NONE',  ( 164.9582166835089367, 246.4294246379055835, 1.883828838449762566 ) ) ;
#23011 = CARTESIAN_POINT ( 'NONE',  ( 12.16147613323643029, 27.99752408145590721, 5.678558825948277544 ) ) ;
#23012 = EDGE_CURVE ( 'NONE', #50839, #84127, #4807, .T. ) ;
#23013 = PLANE ( 'NONE',  #31637 ) ;
#23014 = CARTESIAN_POINT ( 'NONE',  ( 80.61280386015431532, 57.63106766464478881, 16.59051181579431500 ) ) ;
#23016 = ORIENTED_EDGE ( 'NONE', *, *, #54765, .F. ) ;
#23015 = DIRECTION ( 'NONE',  ( -0.8660254037844377084, -0.5000000000000014433, -0.000000000000000000 ) ) ;
#23017 = CARTESIAN_POINT ( 'NONE',  ( 162.6476498368881494, 248.9330020812748785, 10.75824100428386743 ) ) ;
#23018 = CARTESIAN_POINT ( 'NONE',  ( 184.9682936869809566, 258.1092236034054395, 2.986271678517576245 ) ) ;
#23019 = DIRECTION ( 'NONE',  ( 0.5778974349098185970, 0.4186690413702512936, 0.7005360722495072023 ) ) ;
#23020 = CARTESIAN_POINT ( 'NONE',  ( 67.73742752091094133, 65.62596870563270102, -10.80114651390334757 ) ) ;
#23021 = CARTESIAN_POINT ( 'NONE',  ( 161.4025183475459073, 251.0896330829197041, 14.50747140106038735 ) ) ;
#23022 = CARTESIAN_POINT ( 'NONE',  ( 158.0246744607735252, 281.0366367605934101, 2.042212327287092233 ) ) ;
#23023 = VERTEX_POINT ( 'NONE', #24515 ) ;
#23024 = CARTESIAN_POINT ( 'NONE',  ( 194.5803494922524806, 293.6239438553467380, -14.52903234192032222 ) ) ;
#23026 = EDGE_CURVE ( 'NONE', #85510, #39184, #30077, .T. ) ;
#23025 = DIRECTION ( 'NONE',  ( -0.8615733660689046669, -0.5076330711061851630, 0.000000000000000000 ) ) ;
#23027 = CARTESIAN_POINT ( 'NONE',  ( 9.963374858250592325, 169.8927522451418213, 10.00000000000009592 ) ) ;
#23028 = CARTESIAN_POINT ( 'NONE',  ( 82.56883094741532148, 53.27102910656019930, -15.30881521583544647 ) ) ;
#23029 = CARTESIAN_POINT ( 'NONE',  ( 169.9469112398214747, 250.9785751410766750, -8.718312767540300712 ) ) ;
#23030 = CARTESIAN_POINT ( 'NONE',  ( 169.7647569238031338, 280.6421679560587563, -14.26277949995917638 ) ) ;
#23031 = DIRECTION ( 'NONE',  ( -0.7548338719222550397, 0.6559160203858850346, 0.000000000000000000 ) ) ;
#23033 = CARTESIAN_POINT ( 'NONE',  ( -0.9341114727036189391, 170.2677522451418781, 10.00000000000009592 ) ) ;
#23032 = CARTESIAN_POINT ( 'NONE',  ( 0.9332558059805314832, 171.3458772461660544, 9.188101187500095079 ) ) ;
#23034 = ORIENTED_EDGE ( 'NONE', *, *, #95752, .T. ) ;
#23035 = ORIENTED_EDGE ( 'NONE', *, *, #24461, .T. ) ;
#23036 = CARTESIAN_POINT ( 'NONE',  ( 165.6218532904677829, 246.1078588663072253, -2.807711028975429013 ) ) ;
#23037 = DIRECTION ( 'NONE',  ( 0.8660254037844385966, 0.5000000000000004441, 0.000000000000000000 ) ) ;
#23038 = ADVANCED_FACE ( 'NONE', ( #26036 ), #57407, .T. ) ;
#23039 = CARTESIAN_POINT ( 'NONE',  ( 82.98418032785382081, 46.47283061845390506, -11.29752663545136215 ) ) ;
#23040 = FACE_OUTER_BOUND ( 'NONE', #45422, .T. ) ;
#23041 = CARTESIAN_POINT ( 'NONE',  ( 201.9751774886444480, 280.8157260523632317, -16.30213982533239303 ) ) ;
#23042 = CARTESIAN_POINT ( 'NONE',  ( 82.55199557336824512, 43.02032421242048343, 7.382427009242009674 ) ) ;
#23043 = CARTESIAN_POINT ( 'NONE',  ( 149.7411355705484652, 277.2267774073285977, 3.080663611250638922 ) ) ;
#23044 = CARTESIAN_POINT ( 'NONE',  ( 9.403806464923315289, 185.4244531367911293, -4.594050593750046652 ) ) ;
#23045 = CARTESIAN_POINT ( 'NONE',  ( 122.2582625392304863, 232.2048013555409796, 4.594050593750051981 ) ) ;
#23046 = CARTESIAN_POINT ( 'NONE',  ( 203.0026270830780675, 279.0361311525880978, -16.61345826058821373 ) ) ;
#23047 = CARTESIAN_POINT ( 'NONE',  ( 178.9928779471620430, 291.8529855680378660, -6.150425450240065928 ) ) ;
#23048 = CARTESIAN_POINT ( 'NONE',  ( 195.8954499045513558, 275.1620197951183400, 15.78109384089318823 ) ) ;
#23049 = CARTESIAN_POINT ( 'NONE',  ( 26.05470188313195123, 197.3967562850347122, -4.648177544792955347E-16 ) ) ;
#23050 = CARTESIAN_POINT ( 'NONE',  ( 177.2884455301937408, 283.4926669082274771, -15.35860094086973326 ) ) ;
#23051 = AXIS2_PLACEMENT_3D ( 'NONE', #24479, #87370, #48287 ) ;
#23052 = CARTESIAN_POINT ( 'NONE',  ( -17.68663747114990770, 172.8464784336661353, 1.353441290958777327E-15 ) ) ;
#23053 = CARTESIAN_POINT ( 'NONE',  ( 157.0848929289108469, 258.5679796760466047, 17.57466231005294688 ) ) ;
#23054 = CARTESIAN_POINT ( 'NONE',  ( 155.6559071247401960, 261.0430556921643870, 17.79853447468815375 ) ) ;
#23055 = FACE_OUTER_BOUND ( 'NONE', #4133, .T. ) ;
#23056 = CARTESIAN_POINT ( 'NONE',  ( 190.1509686661389367, 284.8912016344419840, 17.04044544971958430 ) ) ;
#23057 = EDGE_CURVE ( 'NONE', #60539, #49096, #56967, .T. ) ;
#23058 = EDGE_CURVE ( 'NONE', #62248, #10169, #59176, .T. ) ;
#23059 = AXIS2_PLACEMENT_3D ( 'NONE', #84331, #84824, #46260 ) ;
#23060 = CARTESIAN_POINT ( 'NONE',  ( 189.2409861230456727, 262.5526351957132078, 8.112751438749265631 ) ) ;
#23061 = CARTESIAN_POINT ( 'NONE',  ( 171.4203603884429299, 279.8539503503338324, 13.89678279489301360 ) ) ;
#23062 = CARTESIAN_POINT ( 'NONE',  ( -110.0000000000000284, 4.999999999999999112, 14.21260523776214590 ) ) ;
#23063 = CARTESIAN_POINT ( 'NONE',  ( 191.1192699377806719, 299.6187094927299199, -9.526914969203620132 ) ) ;
#23064 = CARTESIAN_POINT ( 'NONE',  ( 190.4281805785508084, 300.8157113754859893, -1.233909217199055774 ) ) ;
#23065 = CARTESIAN_POINT ( 'NONE',  ( 181.2056177239550152, 266.0170940294115098, -15.02664418762704024 ) ) ;
#23066 = ORIENTED_EDGE ( 'NONE', *, *, #96502, .T. ) ;
#23067 = CARTESIAN_POINT ( 'NONE',  ( 152.3064147080143584, 267.5489654531014594, -15.38666967861120050 ) ) ;
#23068 = EDGE_CURVE ( 'NONE', #28623, #48026, #59382, .T. ) ;
#23069 = CARTESIAN_POINT ( 'NONE',  ( 188.2735287570237688, 299.1710073388255751, -5.251721556916531419 ) ) ;
#23070 = CARTESIAN_POINT ( 'NONE',  ( 93.65192705076950119, 231.0024278399160949, -9.188101187500093303 ) ) ;
#23071 = CARTESIAN_POINT ( 'NONE',  ( 13.78045586392592092, 26.14336893147754282, 7.433330006724141015 ) ) ;
#23072 = CARTESIAN_POINT ( 'NONE',  ( 191.5281967176683509, 298.9104275333885994, 7.715154960566919407 ) ) ;
#23073 = EDGE_CURVE ( 'NONE', #88859, #85517, #31704, .T. ) ;
#23074 = CARTESIAN_POINT ( 'NONE',  ( 75.16541093910677773, 58.59821464833535742, -16.37950748201892992 ) ) ;
#23075 = AXIS2_PLACEMENT_3D ( 'NONE', #61529, #62009, #13947 ) ;
#23077 = CARTESIAN_POINT ( 'NONE',  ( 191.8998383512474106, 277.1803453812353837, 16.60231051853036277 ) ) ;
#23076 = CARTESIAN_POINT ( 'NONE',  ( 66.42189003655407475, 68.72454749333068946, 2.359676567546969750 ) ) ;
#23078 = CARTESIAN_POINT ( 'NONE',  ( 149.1140077604129885, 272.3739577691819136, 12.91581545547286503 ) ) ;
#23079 = CARTESIAN_POINT ( 'NONE',  ( 150.9115585710837877, 269.2605084359132093, -15.80434701481532578 ) ) ;
#23080 = CARTESIAN_POINT ( 'NONE',  ( 146.5889662694323761, 243.8932355074535678, -2.679491924311248496 ) ) ;
#23081 = DIRECTION ( 'NONE',  ( 0.000000000000000000, 0.000000000000000000, 1.000000000000000000 ) ) ;
#23082 = CARTESIAN_POINT ( 'NONE',  ( 132.1371673402316844, 235.5494855054051868, -2.679491924311248496 ) ) ;
#23083 = CARTESIAN_POINT ( 'NONE',  ( 83.00815485991435594, 53.30142267139499523, 15.60062745561815767 ) ) ;
#23084 = EDGE_LOOP ( 'NONE', ( #75246, #18935, #77702, #41532 ) ) ;
#23085 = CARTESIAN_POINT ( 'NONE',  ( 25.24689923506580769, 37.68290643055188838, 3.479690158560446702E-15 ) ) ;
#23086 = CARTESIAN_POINT ( 'NONE',  ( 70.43005528255592651, 64.46647551784276686, -13.05606537066291573 ) ) ;
#23087 = CARTESIAN_POINT ( 'NONE',  ( 200.3894610702548675, 269.4183277505318301, 8.919713072033628620 ) ) ;
#23088 = CARTESIAN_POINT ( 'NONE',  ( 196.9728329903666122, 289.4800408803428695, -17.53478045286815856 ) ) ;
#23089 = EDGE_CURVE ( 'NONE', #25756, #44273, #88118, .T. ) ;
#23090 = EDGE_CURVE ( 'NONE', #85466, #26183, #89854, .T. ) ;
#23091 = ORIENTED_EDGE ( 'NONE', *, *, #64612, .F. ) ;
#23092 = CARTESIAN_POINT ( 'NONE',  ( -19.65312891409030271, 93.06504152958497400, 59.99999999999999289 ) ) ;
#23093 = CARTESIAN_POINT ( 'NONE',  ( 78.89717507877558944, 49.06168382820697360, 14.38932173611067356 ) ) ;
#23094 = CARTESIAN_POINT ( 'NONE',  ( 183.4202745723773091, 264.5322101262771639, -13.24744625114140817 ) ) ;
#23095 = CARTESIAN_POINT ( 'NONE',  ( 169.3369456435013944, 252.0587115110951117, -8.674031833049340889 ) ) ;
#23096 = FACE_OUTER_BOUND ( 'NONE', #68577, .T. ) ;
#23097 = ORIENTED_EDGE ( 'NONE', *, *, #57438, .T. ) ;
#23098 = CARTESIAN_POINT ( 'NONE',  ( 188.6533994728961829, 279.6148911687740224, 16.71976415023760509 ) ) ;
#23099 = CARTESIAN_POINT ( 'NONE',  ( 31.98863997849372254, 36.65586893147758474, -7.433330006724137462 ) ) ;
#23100 = VERTEX_POINT ( 'NONE', #27533 ) ;
#23101 = CARTESIAN_POINT ( 'NONE',  ( 179.8347084456439688, 290.9760905973820968, 10.83644005890302253 ) ) ;
#23102 = CARTESIAN_POINT ( 'NONE',  ( 81.78504375891562006, 41.48292696562020865, -5.073134180756075473 ) ) ;
#23103 = ORIENTED_EDGE ( 'NONE', *, *, #14634, .T. ) ;
#23104 = CARTESIAN_POINT ( 'NONE',  ( 86.33714660501533444, 47.00371335520402738, -10.02508334048726546 ) ) ;
#23105 = LINE ( 'NONE', #53018, #10381 ) ;
#23106 = CARTESIAN_POINT ( 'NONE',  ( 190.5525489982964302, 278.5900507645195034, -16.51546226578511423 ) ) ;
#23107 = CARTESIAN_POINT ( 'NONE',  ( 153.5731768013688736, 264.6504504307081334, -18.06482034778880674 ) ) ;
#23108 = CARTESIAN_POINT ( 'NONE',  ( 185.3081074539437907, 278.3520910533009101, 17.82413638460242922 ) ) ;
#23109 = FACE_OUTER_BOUND ( 'NONE', #43582, .T. ) ;
#23110 = CARTESIAN_POINT ( 'NONE',  ( 93.96857342517719758, 15.00000000000000000, 0.000000000000000000 ) ) ;
#23111 = CARTESIAN_POINT ( 'NONE',  ( 81.53672410393728853, 56.04530558232496418, -16.40539795406884949 ) ) ;
#23112 = DIRECTION ( 'NONE',  ( -0.5000000000000082157, 0.8660254037844338226, 0.000000000000000000 ) ) ;
#23113 = VERTEX_POINT ( 'NONE', #35613 ) ;
#23114 = B_SPLINE_CURVE_WITH_KNOTS ( 'NONE', 3,
 ( #3437, #19638, #57097, #72343, #34798, #34314, #65212, #96154, #64212, #80462, #11033, #3915, #73328, #89089, #88080, #65700 ),
 .UNSPECIFIED., .F., .F.,
 ( 4, 1, 2, 2, 2, 1, 2, 2, 4 ),
 ( 0.000000000000000000, 0.1249999999999995559, 0.1874999999999993339, 0.2499999999999991118, 0.4999999999999977240, 0.6249999999999972244, 0.6874999999999971134, 0.7499999999999970024, 1.000000000000000000 ),
 .UNSPECIFIED. ) ;
#23115 = CARTESIAN_POINT ( 'NONE',  ( 197.8980529691977779, 285.8775128688180871, 17.80711829255526979 ) ) ;
#23116 = ORIENTED_EDGE ( 'NONE', *, *, #15079, .T. ) ;
#23117 = VERTEX_POINT ( 'NONE', #66999 ) ;
#23118 = CARTESIAN_POINT ( 'NONE',  ( 172.9269288353417835, 271.0868964859365633, 16.42719315256508850 ) ) ;
#23119 = ORIENTED_EDGE ( 'NONE', *, *, #37709, .T. ) ;
#23120 = CARTESIAN_POINT ( 'NONE',  ( 190.0466317824856048, 300.2728036453518143, -3.352836199975675058 ) ) ;
#23121 = CARTESIAN_POINT ( 'NONE',  ( 76.20055470335279324, 65.09253202017347917, 14.18943646504600054 ) ) ;
#23122 = CARTESIAN_POINT ( 'NONE',  ( 198.5444618742102705, 273.8348775512076259, -13.44695229262796055 ) ) ;
#23123 = DIRECTION ( 'NONE',  ( 0.000000000000000000, 0.000000000000000000, 1.000000000000000000 ) ) ;
#23124 = CARTESIAN_POINT ( 'NONE',  ( 82.45865130729738723, 40.97087310285034079, 1.023290110074061898 ) ) ;
#23125 = CARTESIAN_POINT ( 'NONE',  ( 171.4102349331081996, 250.9416128396940735, -5.608677351237023601 ) ) ;
#23126 = CYLINDRICAL_SURFACE ( 'NONE', #95486, 70.00000000000002842 ) ;
#23127 = CARTESIAN_POINT ( 'NONE',  ( 178.3260541269674775, 254.9471070209705204, 5.880822174413203207 ) ) ;
#23128 = CARTESIAN_POINT ( 'NONE',  ( 112.9213393807382886, 229.8768266524160140, 9.188101187500098632 ) ) ;
#23129 = CARTESIAN_POINT ( 'NONE',  ( 70.58939099706752529, 60.68707437868734189, -14.57694795185084580 ) ) ;
#23130 = CARTESIAN_POINT ( 'NONE',  ( 37.11382629638189457, 33.37878583063844218, 9.188101187500006262 ) ) ;
#23131 = CARTESIAN_POINT ( 'NONE',  ( -89.11465314115662295, 93.37593066204024694, -30.52142883766498116 ) ) ;
#23132 = ORIENTED_EDGE ( 'NONE', *, *, #28836, .T. ) ;
#23133 = ADVANCED_FACE ( 'NONE', ( #19932 ), #19454, .F. ) ;
#23134 = CARTESIAN_POINT ( 'NONE',  ( 86.78119538955827750, 45.86439926875618767, -8.245237605873949605 ) ) ;
#23135 = CARTESIAN_POINT ( 'NONE',  ( 71.60199290673480732, 63.90083948714775630, -13.28680243790413051 ) ) ;
#23136 = VECTOR ( 'NONE', #6538, 1000.000000000000000 ) ;
#23137 = EDGE_CURVE ( 'NONE', #97892, #82529, #12298, .T. ) ;
#23138 = CARTESIAN_POINT ( 'NONE',  ( -71.61465314115659453, 63.06504152958490295, -60.00000000000000000 ) ) ;
#23139 = CARTESIAN_POINT ( 'NONE',  ( 205.6812242890302400, 270.0455300709248831, -5.666524662691169389 ) ) ;
#23140 = CARTESIAN_POINT ( 'NONE',  ( 72.92328079741919566, 65.18747506910628431, 13.02211304875830677 ) ) ;
#23141 = CARTESIAN_POINT ( 'NONE',  ( 200.9812045408918380, 282.5373376992193926, -16.61165062382494284 ) ) ;
#23142 = CARTESIAN_POINT ( 'NONE',  ( -65.22359575898936157, 56.10326143670914689, 59.99999999999999289 ) ) ;
#23143 = VERTEX_POINT ( 'NONE', #82267 ) ;
#23144 = DIRECTION ( 'NONE',  ( -0.000000000000000000, 0.000000000000000000, 1.000000000000000000 ) ) ;
#23145 = VERTEX_POINT ( 'NONE', #83237 ) ;
#23146 = CARTESIAN_POINT ( 'NONE',  ( 148.2352135776142177, 273.8960739431854563, -9.245976304249309052 ) ) ;
#23147 = DIRECTION ( 'NONE',  ( 0.5000000000000013323, -0.8660254037844378194, 0.000000000000000000 ) ) ;
#23148 = EDGE_LOOP ( 'NONE', ( #15611, #93801, #36585 ) ) ;
#23150 = ADVANCED_FACE ( 'NONE', ( #5705 ), #305, .F. ) ;
#23149 = DIRECTION ( 'NONE',  ( 0.5000000000000013323, -0.8660254037844378194, 0.000000000000000000 ) ) ;
#23151 = AXIS2_PLACEMENT_3D ( 'NONE', #71340, #63723, #39396 ) ;
#23152 = CARTESIAN_POINT ( 'NONE',  ( 159.7079830814418244, 278.3650007144455003, 10.37211021382808696 ) ) ;
#23153 = CARTESIAN_POINT ( 'NONE',  ( 192.4799288706118148, 262.6369605892642767, 4.631236763554750446 ) ) ;
#23154 = CARTESIAN_POINT ( 'NONE',  ( 158.2231871454910959, 263.2639962149535791, 17.34092271714001399 ) ) ;
#23155 = CARTESIAN_POINT ( 'NONE',  ( 69.97821611620445026, 71.48374793263995741, -1.182227389098916781 ) ) ;
#23157 = CARTESIAN_POINT ( 'NONE',  ( 157.1201528510747210, 280.1329342086722249, 5.821162413553630621 ) ) ;
#23156 = CARTESIAN_POINT ( 'NONE',  ( 184.2460973547030392, 288.7912027798610097, -14.42049990347707222 ) ) ;
#23158 = CARTESIAN_POINT ( 'NONE',  ( 153.1961624462112752, 265.3034584490234806, -16.19494717845262954 ) ) ;
#23159 = ORIENTED_EDGE ( 'NONE', *, *, #64821, .T. ) ;
#23160 = CARTESIAN_POINT ( 'NONE',  ( 146.7845206192450007, 276.4087478532630939, 4.443586170796542945 ) ) ;
#23162 = CARTESIAN_POINT ( 'NONE',  ( 71.94540097076600205, 64.24250455633612944, 13.20799783956320539 ) ) ;
#23161 = B_SPLINE_SURFACE_WITH_KNOTS ( 'NONE', 3, 1, ( 
 ( #25866, #17760 ),
 ( #10158, #80594 ),
 ( #72974, #3565 ),
 ( #72478, #50143 ),
 ( #63843, #34445 ),
 ( #89214, #65344 ),
 ( #81584, #41024 ),
 ( #34931, #57727 ),
 ( #88208, #81097 ),
 ( #73459, #4042 ),
 ( #94782, #19762 ),
 ( #71466, #2057 ),
 ( #25341, #33971 ),
 ( #2566, #56742 ),
 ( #87724, #18260 ),
 ( #10658, #3081 ),
 ( #51646, #59208 ),
 ( #37419, #12663 ),
 ( #73953, #68325 ),
 ( #74957, #13647 ),
 ( #59726, #4539 ),
 ( #60211, #90692 ),
 ( #99251, #43532 ),
 ( #35931, #6036 ),
 ( #29836, #5541 ),
 ( #74471, #12153 ),
 ( #52620, #44520 ),
 ( #53132, #60707 ),
 ( #29346, #21249 ),
 ( #36425, #5051 ),
 ( #91668, #22231 ),
 ( #67333, #52127 ),
 ( #66833, #51129 ),
 ( #67843, #43015 ) ),
 .UNSPECIFIED., .T., .F., .F.,
 ( 4, 2, 2, 2, 2, 2, 2, 2, 2, 2, 2, 2, 2, 2, 2, 2, 4 ),
 ( 2, 2 ),
 ( 0.000000000000000000, 0.06250000000000000000, 0.1250000000000000000, 0.1875000000000000000, 0.2500000000000000000, 0.3125000000000000000, 0.3750000000000000000, 0.4375000000000000000, 0.5000000000000000000, 0.5625000000000000000, 0.6250000000000000000, 0.6875000000000000000, 0.7500000000000000000, 0.8125000000000000000, 0.8750000000000000000, 0.9375000000000000000, 1.000000000000000000 ),
 ( 0.000000000000000000, 1.000000000000000000 ),
 .UNSPECIFIED. ) ;
#23163 = CARTESIAN_POINT ( 'NONE',  ( 188.8764293144468240, 259.6972905960182061, 3.583694637520717041 ) ) ;
#23164 = CARTESIAN_POINT ( 'NONE',  ( 182.4203110637134273, 275.0573665403885570, -17.01792947190426020 ) ) ;
#23165 = CARTESIAN_POINT ( 'NONE',  ( 76.32488315910845245, 203.3262482093458061, 3.021315404115420679E-15 ) ) ;
#23167 = EDGE_CURVE ( 'NONE', #76243, #51511, #47192, .T. ) ;
#23166 = CARTESIAN_POINT ( 'NONE',  ( 189.1711897435683909, 270.1262327773276297, -14.07582082338928053 ) ) ;
#23168 = CARTESIAN_POINT ( 'NONE',  ( 163.8758338523056182, 285.7844739252391264, -2.579456967851244897 ) ) ;
#23169 = EDGE_CURVE ( 'NONE', #13784, #13192, #33683, .T. ) ;
#23170 = CARTESIAN_POINT ( 'NONE',  ( 83.23481903784592362, 43.31313429786332847, 7.200028244731907279 ) ) ;
#23171 = LINE ( 'NONE', #53082, #75414 ) ;
#23172 = CARTESIAN_POINT ( 'NONE',  ( 188.4805308512120234, 298.0761574053781828, 7.892637567094712203 ) ) ;
#23173 = CARTESIAN_POINT ( 'NONE',  ( 71.09952580927735255, 66.44067406087256700, -11.85013464261816374 ) ) ;
#23174 = CARTESIAN_POINT ( 'NONE',  ( 77.57650404090335883, 215.5958772461660544, -9.188101187500095079 ) ) ;
#23175 = CARTESIAN_POINT ( 'NONE',  ( 36.46736065678477701, 181.8615022471902023, 5.000000000000051514 ) ) ;
#23176 = FACE_OUTER_BOUND ( 'NONE', #64618, .T. ) ;
#23177 = LINE ( 'NONE', #14601, #41431 ) ;
#23178 = CARTESIAN_POINT ( 'NONE',  ( 154.8579861482817535, 262.4250953638155011, -17.69813260923097786 ) ) ;
#23179 = CARTESIAN_POINT ( 'NONE',  ( 161.8408514536557163, 250.3304178724980318, -14.12919723462510646 ) ) ;
#23180 = CARTESIAN_POINT ( 'NONE',  ( 202.8211298556536804, 279.3504935719197988, 17.07914446815911447 ) ) ;
#23181 = CARTESIAN_POINT ( 'NONE',  ( 163.0019261236505486, 284.2031270801829805, 6.030241692761612704 ) ) ;
#23183 = CARTESIAN_POINT ( 'NONE',  ( 76.45248566530659673, 51.50253309734852536, 15.63309938903474361 ) ) ;
#23182 = CARTESIAN_POINT ( 'NONE',  ( 73.58959834336499739, 69.25141985266563438, -10.00371726299768405 ) ) ;
#23184 = CARTESIAN_POINT ( 'NONE',  ( 4.858991816890471327, 18.50829794293877839, -10.00000000000000355 ) ) ;
#23185 = EDGE_CURVE ( 'NONE', #78092, #48457, #46608, .T. ) ;
#23186 = CARTESIAN_POINT ( 'NONE',  ( 166.0702642583571844, 249.2115659832978167, -9.324519184667250826 ) ) ;
#23187 = CARTESIAN_POINT ( 'NONE',  ( 163.9712156549718429, 246.6405188371923600, -4.902504724781694634 ) ) ;
#23188 = CARTESIAN_POINT ( 'NONE',  ( 196.2255671652529259, 290.7743432561995860, 16.01325193769018185 ) ) ;
#23189 = CARTESIAN_POINT ( 'NONE',  ( -6.130263895410211994, 157.2677522451417929, -5.000000000000041744 ) ) ;
#23190 = EDGE_CURVE ( 'NONE', #45441, #54753, #34978, .T. ) ;
#23191 = CARTESIAN_POINT ( 'NONE',  ( 58.41569198217266035, 204.5333772461660544, 9.188101187500095079 ) ) ;
#23192 = CARTESIAN_POINT ( 'NONE',  ( 163.8894951723502800, 247.1650863376556231, -6.266457964612296649 ) ) ;
#23193 = CARTESIAN_POINT ( 'NONE',  ( 88.10956888842845558, 44.04735113414163550, 0.5588696975863149952 ) ) ;
#23194 = EDGE_CURVE ( 'NONE', #81343, #39182, #95466, .T. ) ;
#23195 = CARTESIAN_POINT ( 'NONE',  ( 82.22870199775800870, 49.95230068291388648, -13.96007491776960840 ) ) ;
#23196 = CARTESIAN_POINT ( 'NONE',  ( -12.03006195514386434, 173.8615022471903160, 5.000000000000046185 ) ) ;
#23197 = DIRECTION ( 'NONE',  ( -0.000000000000000000, 0.000000000000000000, 1.000000000000000000 ) ) ;
#23198 = B_SPLINE_CURVE_WITH_KNOTS ( 'NONE', 3,
 ( #93976, #47814, #78751, #9339 ),
 .UNSPECIFIED., .F., .F.,
 ( 4, 4 ),
 ( 0.005707261542966231803, 0.01134347631022532103 ),
 .UNSPECIFIED. ) ;
#23199 = CARTESIAN_POINT ( 'NONE',  ( 15.88121511744419756, 186.6427522451419350, -10.00000000000009592 ) ) ;
#23200 = CARTESIAN_POINT ( 'NONE',  ( 25.85429974905589390, 23.43085787977764411, -9.188101187500008038 ) ) ;
#23201 = CARTESIAN_POINT ( 'NONE',  ( 151.0013883899287066, 269.1049186256390726, -14.25461351222133466 ) ) ;
#23202 = CARTESIAN_POINT ( 'NONE',  ( 196.6317700900902139, 290.0707791521982131, -17.91116578096951883 ) ) ;
#23203 = CARTESIAN_POINT ( 'NONE',  ( 11.99789328850488879, 15.43085787977761569, -9.188101187500008038 ) ) ;
#23204 = CARTESIAN_POINT ( 'NONE',  ( 63.55789136502527015, 201.3768266524160140, 9.188101187500096856 ) ) ;
#23205 = CARTESIAN_POINT ( 'NONE',  ( 77.10733807873376122, 63.61886353868632682, 15.40965320646045100 ) ) ;
#23206 = DIRECTION ( 'NONE',  ( -0.8660254037844380415, -0.5000000000000009992, 0.000000000000000000 ) ) ;
#23207 = EDGE_CURVE ( 'NONE', #38156, #22585, #48199, .T. ) ;
#23208 = CARTESIAN_POINT ( 'NONE',  ( 198.0006249058153003, 287.6998530631771587, 18.31850453277666801 ) ) ;
#23209 = DIRECTION ( 'NONE',  ( 0.8660254037844395958, 0.4999999999999985567, 0.000000000000000000 ) ) ;
#23210 = CARTESIAN_POINT ( 'NONE',  ( 153.4632428020424300, 264.8408617030205505, 17.93840816349579015 ) ) ;
#23211 = CARTESIAN_POINT ( 'NONE',  ( 79.17827112357750252, 55.43091488132045441, -16.07850425917232684 ) ) ;
#23212 = CARTESIAN_POINT ( 'NONE',  ( 87.67760366270776728, 45.22517868708455069, -6.234814096420206120 ) ) ;
#23213 = CARTESIAN_POINT ( 'NONE',  ( 117.4407359106297406, 238.6115022471902307, 10.00000000000009592 ) ) ;
#23214 = CARTESIAN_POINT ( 'NONE',  ( 200.7523954295751594, 282.9336467052548869, 18.23634913067694185 ) ) ;
#23215 = CARTESIAN_POINT ( 'NONE',  ( -27.42236680055714260, 166.5217562850347406, 1.224646799147364892E-15 ) ) ;
#23216 = EDGE_LOOP ( 'NONE', ( #56660, #52057, #88102, #83110 ) ) ;
#23217 = AXIS2_PLACEMENT_3D ( 'NONE', #20005, #56492, #50884 ) ;
#23218 = CARTESIAN_POINT ( 'NONE',  ( 77.33837241094562387, 49.21827100037820202, 15.32655703911426670 ) ) ;
#23219 = CARTESIAN_POINT ( 'NONE',  ( 82.78345634833956979, 53.69061190982764487, 15.38144188222361208 ) ) ;
#23220 = ORIENTED_EDGE ( 'NONE', *, *, #10456, .F. ) ;
#23221 = CARTESIAN_POINT ( 'NONE',  ( 159.6962080797732710, 254.0450491601782232, -15.33973334987084947 ) ) ;
#23222 = CARTESIAN_POINT ( 'NONE',  ( 189.6282054824295642, 278.2883837369565754, -16.50473759827790587 ) ) ;
#23223 = FACE_OUTER_BOUND ( 'NONE', #78382, .T. ) ;
#23224 = ORIENTED_EDGE ( 'NONE', *, *, #51085, .F. ) ;
#23226 = ORIENTED_EDGE ( 'NONE', *, *, #10876, .F. ) ;
#23225 = AXIS2_PLACEMENT_3D ( 'NONE', #83176, #46111, #84187 ) ;
#23227 = CARTESIAN_POINT ( 'NONE',  ( 79.98829826350832661, 44.59498145193617802, 11.76229303994366582 ) ) ;
#23228 = CARTESIAN_POINT ( 'NONE',  ( 148.0826818691893152, 274.1602666119424043, -9.371267383421741926 ) ) ;
#23229 = CARTESIAN_POINT ( 'NONE',  ( -19.65312891409030271, 93.06504152958497400, -40.00000000000000000 ) ) ;
#23230 = ORIENTED_EDGE ( 'NONE', *, *, #81631, .F. ) ;
#23231 = CARTESIAN_POINT ( 'NONE',  ( 24.28583178621855865, 34.99752408145592142, 5.678558825948276656 ) ) ;
#23232 = FACE_OUTER_BOUND ( 'NONE', #78874, .T. ) ;
#23233 = CARTESIAN_POINT ( 'NONE',  ( 8.106622824862185439, 30.17147933776455204, -10.00000000000000000 ) ) ;
#23234 = DIRECTION ( 'NONE',  ( 0.8660254037844382635, 0.5000000000000004441, 1.232595164407830946E-32 ) ) ;
#23235 = VERTEX_POINT ( 'NONE', #42092 ) ;
#23236 = CARTESIAN_POINT ( 'NONE',  ( 183.8754313647489198, 256.5225093191261294, -2.022205659181245174 ) ) ;
#23237 = CARTESIAN_POINT ( 'NONE',  ( -24.06189489623784183, 146.7012482093458914, 8.087813781312181686E-14 ) ) ;
#23238 = ORIENTED_EDGE ( 'NONE', *, *, #19700, .F. ) ;
#23239 = CARTESIAN_POINT ( 'NONE',  ( 174.5584865442874616, 286.5715570807610106, 11.73736338454468076 ) ) ;
#23240 =( BOUNDED_CURVE ( )  B_SPLINE_CURVE ( 2, ( #62304, #17214, #48121, #79065, #40509, #10133, #49133, #80067, #71443, #2031, #31910, #33428, #64325 ),
 .UNSPECIFIED., .F., .T. ) 
 B_SPLINE_CURVE_WITH_KNOTS ( ( 3, 2, 2, 2, 2, 2, 3 ),
 ( 0.6875000000000000000, 0.6899999999999999467, 0.6949999999999999512, 0.6999999999999999556, 0.7049999999999999600, 0.7099999999999999645, 0.7125000000000000222 ),
 .UNSPECIFIED. ) 
 CURVE ( )  GEOMETRIC_REPRESENTATION_ITEM ( )  RATIONAL_B_SPLINE_CURVE ( ( 0.9755282581475768211, 0.9755282581475768211, 1.000000000000000000, 0.9510565162951535312, 1.000000000000000000, 0.9510565162951535312, 1.000000000000000000, 0.9510565162951535312, 1.000000000000000000, 0.9510565162951535312, 1.000000000000000000, 0.9755282581475761550, 0.9755282581475767101 ) ) 
 REPRESENTATION_ITEM ( '' )  );
#23242 = CARTESIAN_POINT ( 'NONE',  ( 67.76021416997799918, 65.93326558605815535, -10.49598374965347425 ) ) ;
#23241 = CARTESIAN_POINT ( 'NONE',  ( 67.78340610521031806, 65.54725019734833324, 10.17040391041397029 ) ) ;
#23243 = DIRECTION ( 'NONE',  ( -0.000000000000000000, -0.000000000000000000, 1.000000000000000000 ) ) ;
#23244 = CARTESIAN_POINT ( 'NONE',  ( 204.3371846825755824, 276.7246095846310823, 14.72513001683937262 ) ) ;
#23245 = CARTESIAN_POINT ( 'NONE',  ( 188.1399729590822858, 294.5748838946434489, -10.97770313550398669 ) ) ;
#23246 = CARTESIAN_POINT ( 'NONE',  ( 204.7237927799493775, 276.0549847173622879, -12.81020997223575364 ) ) ;
#23247 = CARTESIAN_POINT ( 'NONE',  ( 136.0871718362070339, 255.5024278399161233, 9.188101187500095079 ) ) ;
#23248 = CARTESIAN_POINT ( 'NONE',  ( 177.5089039944837452, 268.9213076647187677, 16.19086122322285348 ) ) ;
#23249 = CARTESIAN_POINT ( 'NONE',  ( 179.2327624300868365, 257.7468971898826453, 10.15833653911241186 ) ) ;
#23250 = CARTESIAN_POINT ( 'NONE',  ( 67.34640541081718368, 215.8149278399160949, -9.188101187500095079 ) ) ;
#23251 = VERTEX_POINT ( 'NONE', #76385 ) ;
#23252 = FACE_OUTER_BOUND ( 'NONE', #81274, .T. ) ;
#23253 = CARTESIAN_POINT ( 'NONE',  ( 73.91099221338522796, 59.87250767674520091, -15.97378689575042898 ) ) ;
#23254 = CARTESIAN_POINT ( 'NONE',  ( 156.6812872898450735, 261.2670451491295012, 0.000000000000000000 ) ) ;
#23255 = ORIENTED_EDGE ( 'NONE', *, *, #83732, .T. ) ;
#23256 = CARTESIAN_POINT ( 'NONE',  ( 195.5605487959511777, 291.9261888597969232, -15.74379588760244175 ) ) ;
#23257 = VERTEX_POINT ( 'NONE', #12207 ) ;
#23258 = CARTESIAN_POINT ( 'NONE',  ( 66.59391288086393956, 67.82822080634741724, 6.925870058277245001 ) ) ;
#23259 = CARTESIAN_POINT ( 'NONE',  ( 194.1833477612660204, 284.7236497737663399, 17.42380001248895027 ) ) ;
#23260 = CARTESIAN_POINT ( 'NONE',  ( 146.7818291168261453, 276.4134096722012828, -0.7617065417431535534 ) ) ;
#23261 = FACE_OUTER_BOUND ( 'NONE', #100152, .T. ) ;
#23262 = CARTESIAN_POINT ( 'NONE',  ( 155.6276701977099890, 261.0919634844306643, 17.49722577287685255 ) ) ;
#23263 = CARTESIAN_POINT ( 'NONE',  ( 72.19772409968021520, 68.63628420467338742, 9.688590869373431502 ) ) ;
#23264 = CARTESIAN_POINT ( 'NONE',  ( 72.19064823929512897, 221.6744531367911293, 4.594050593750047540 ) ) ;
#23265 = VERTEX_POINT ( 'NONE', #34495 ) ;
#23266 = VERTEX_POINT ( 'NONE', #26906 ) ;
#23267 = CARTESIAN_POINT ( 'NONE',  ( 200.3487535410712610, 283.6327749642065896, -17.20506751786975030 ) ) ;
#23268 = ORIENTED_EDGE ( 'NONE', *, *, #2129, .T. ) ;
#23269 = LINE ( 'NONE', #16684, #79125 ) ;
#23270 = B_SPLINE_CURVE_WITH_KNOTS ( 'NONE', 3,
 ( #37196, #60479, #90956, #43294, #36690, #36193, #74242, #60983, #53390, #67599, #75222, #82366, #37682, #22499, #12936, #59481, #91948, #13425, #75721, #67099, #43795, #52397, #68594, #74738, #4827, #82855, #44294, #58977, #20524, #59986, #14410 ),
 .UNSPECIFIED., .F., .F.,
 ( 4, 3, 3, 3, 3, 3, 3, 3, 3, 3, 4 ),
 ( 0.000000000000000000, 0.1333490885032353190, 0.3007194338854385363, 0.4699862290245196972, 0.5844252810809350551, 0.6686540514502717913, 0.7354980260655500368, 0.8028463152565585847, 0.8633854507757243724, 0.9437142632667462339, 1.000000000000000000 ),
 .UNSPECIFIED. ) ;
#23271 = EDGE_CURVE ( 'NONE', #55813, #58122, #57785, .T. ) ;
#23272 = CARTESIAN_POINT ( 'NONE',  ( 76.12288495599533178, 65.36913255257266542, -14.03413756946655511 ) ) ;
#23273 = CARTESIAN_POINT ( 'NONE',  ( 205.9240884482826175, 273.9760116357041966, 10.27504561427317142 ) ) ;
#23274 = CARTESIAN_POINT ( 'NONE',  ( 160.4962995477943650, 275.9333967852908813, 14.18032076246626794 ) ) ;
#23275 = DIRECTION ( 'NONE',  ( -0.000000000000000000, -0.000000000000000000, -1.000000000000000000 ) ) ;
#23276 = CARTESIAN_POINT ( 'NONE',  ( 162.6191010640297065, 261.4165189579067032, 16.98501175862150347 ) ) ;
#23277 = VERTEX_POINT ( 'NONE', #60639 ) ;
#23278 = CARTESIAN_POINT ( 'NONE',  ( 188.6595133177037269, 294.9934435437166371, 11.67654844209925891 ) ) ;
#23279 = CARTESIAN_POINT ( 'NONE',  ( 185.5760615167922367, 259.8211877333729376, 5.844598467702574851 ) ) ;
#23280 = CARTESIAN_POINT ( 'NONE',  ( 29.52096178950397842, 38.81751292744058190, -6.180339887498951690 ) ) ;
#23282 = ADVANCED_FACE ( 'NONE', ( #68255 ), #66394, .T. ) ;
#23281 = CARTESIAN_POINT ( 'NONE',  ( 152.6621968174709991, 266.2283140474973493, -17.02835521334403168 ) ) ;
#23283 = CARTESIAN_POINT ( 'NONE',  ( 72.47401207315012073, 70.81051498135123268, 7.656770371261354846 ) ) ;
#23284 = ADVANCED_FACE ( 'NONE', ( #52553 ), #31029, .F. ) ;
#23285 = VECTOR ( 'NONE', #20051, 1000.000000000000114 ) ;
#23286 = CARTESIAN_POINT ( 'NONE',  ( 32.30839531297598910, 123.0650415295850593, 10.00000000000000888 ) ) ;
#23287 = ORIENTED_EDGE ( 'NONE', *, *, #79595, .F. ) ;
#23288 = FACE_OUTER_BOUND ( 'NONE', #82900, .T. ) ;
#23289 = CARTESIAN_POINT ( 'NONE',  ( -22.42236680055709641, 157.8615022471902591, 0.000000000000000000 ) ) ;
#23290 = PLANE ( 'NONE',  #85139 ) ;
#23291 = CARTESIAN_POINT ( 'NONE',  ( 186.3860696682239677, 265.1981530971773964, -11.87193015803705087 ) ) ;
#23292 = CARTESIAN_POINT ( 'NONE',  ( 83.73865579866679809, 51.98612588642360066, 14.96617132975018549 ) ) ;
#23293 = CARTESIAN_POINT ( 'NONE',  ( 156.7306434729829903, 272.3907090408932845, 14.28438741009544977 ) ) ;
#23294 = ORIENTED_EDGE ( 'NONE', *, *, #50025, .F. ) ;
#23295 = AXIS2_PLACEMENT_3D ( 'NONE', #66347, #83083, #82096 ) ;
#23296 = CARTESIAN_POINT ( 'NONE',  ( -13.11024591527734628, 6.000000000000000000, -32.50000000000000000 ) ) ;
#23297 = CARTESIAN_POINT ( 'NONE',  ( -17.25743208833890208, 103.2403577256391998, 44.62839627432005329 ) ) ;
#23298 = PLANE ( 'NONE',  #93887 ) ;
#23300 = CARTESIAN_POINT ( 'NONE',  ( 73.76528436707422998, 55.26057213895941089, 16.11941679284131723 ) ) ;
#23299 = CARTESIAN_POINT ( 'NONE',  ( 155.4216552449402684, 261.4487918497463284, 18.51722274565528892 ) ) ;
#23301 = CARTESIAN_POINT ( 'NONE',  ( 176.2109476536867589, 285.4385534205517843, -12.05244463992889514 ) ) ;
#23302 = CARTESIAN_POINT ( 'NONE',  ( 22.85147042958088193, 25.14441083166261137, 10.00000000000000533 ) ) ;
#23303 = CARTESIAN_POINT ( 'NONE',  ( 190.0550686570564949, 301.4619601804237732, 4.203010638620038542 ) ) ;
#23304 = CARTESIAN_POINT ( 'NONE',  ( 164.0717493910576650, 284.1959068738492533, -3.117773458651499574 ) ) ;
#23305 = CARTESIAN_POINT ( 'NONE',  ( 133.4825598088814047, 236.3262482093457493, 3.021315404115420679E-15 ) ) ;
#23306 = CARTESIAN_POINT ( 'NONE',  ( 191.8140490939860285, 262.3104730638163460, 2.949596223079247626 ) ) ;
#23307 = EDGE_CURVE ( 'NONE', #96434, #7039, #7453, .T. ) ;
#23308 = CARTESIAN_POINT ( 'NONE',  ( -4.289699588770600869, 159.1423013555410080, -4.594050593750043987 ) ) ;
#23309 = CARTESIAN_POINT ( 'NONE',  ( 29.30989995549245464, 44.80713248141894667, -10.00000000000000000 ) ) ;
#23310 = ORIENTED_EDGE ( 'NONE', *, *, #66566, .F. ) ;
#23311 = CYLINDRICAL_SURFACE ( 'NONE', #45977, 17.82106496071139645 ) ;
#23312 = EDGE_CURVE ( 'NONE', #20229, #25358, #18836, .T. ) ;
#23313 = CARTESIAN_POINT ( 'NONE',  ( 73.10205918017362592, 70.55621008947603912, -7.923255499225144050 ) ) ;
#23314 = CARTESIAN_POINT ( 'NONE',  ( 138.6787122315880083, 239.3262482093457493, 3.021315404115420679E-15 ) ) ;
#23315 = CARTESIAN_POINT ( 'NONE',  ( 31.76832553566411121, 98.72342451966777332, 59.99999999999999289 ) ) ;
#23316 = CARTESIAN_POINT ( 'NONE',  ( 32.86828966629671811, 177.5327760586659736, 1.948934522072302763E-15 ) ) ;
#23317 = CARTESIAN_POINT ( 'NONE',  ( 75.48012123272684448, 53.33211347937982794, 16.49774674189050927 ) ) ;
#23318 = CARTESIAN_POINT ( 'NONE',  ( 30.91633199877554716, 29.80066082961423746, 10.00000000000000533 ) ) ;
#23319 = CARTESIAN_POINT ( 'NONE',  ( 76.72630680417243809, 51.77891733241483507, 16.15279506092123540 ) ) ;
#23320 = CARTESIAN_POINT ( 'NONE',  ( 170.4337869423260372, 270.9453688967402059, -17.51992477341579146 ) ) ;
#23321 = CARTESIAN_POINT ( 'NONE',  ( 9.620573139467140322, 176.3615022471902307, -10.00000000000009592 ) ) ;
#23322 = EDGE_CURVE ( 'NONE', #30767, #33732, #39827, .T. ) ;
#23323 = CARTESIAN_POINT ( 'NONE',  ( 178.9036571371011632, 255.1432592131925787, -3.948543175344032541 ) ) ;
#23324 = CARTESIAN_POINT ( 'NONE',  ( 162.6991225460172927, 284.8212170328912975, -3.897741803361528756 ) ) ;
#23325 = B_SPLINE_CURVE_WITH_KNOTS ( 'NONE', 3,
 ( #9277, #40150, #1690, #45750 ),
 .UNSPECIFIED., .F., .F.,
 ( 4, 4 ),
 ( 0.03903437031820212316, 0.04753079826317264944 ),
 .UNSPECIFIED. ) ;
#23326 = CARTESIAN_POINT ( 'NONE',  ( 74.57247842330004062, 213.8615022471902591, -10.00000000000009592 ) ) ;
#23327 = DIRECTION ( 'NONE',  ( -0.6201213960746324583, 0.7845058662179964504, 0.000000000000000000 ) ) ;
#23328 = CARTESIAN_POINT ( 'NONE',  ( 203.3837935586101935, 270.0850993924222507, 6.058045230343306109 ) ) ;
#23329 = CARTESIAN_POINT ( 'NONE',  ( 22.50244069716294959, 192.9869531367911293, 4.594050593750046652 ) ) ;
#23330 = CARTESIAN_POINT ( 'NONE',  ( 72.79894534421406149, 70.83549005279603250, -7.921956013610881975 ) ) ;
#23331 = CARTESIAN_POINT ( 'NONE',  ( -4.878521687326337286, 80.51981399750955859, 13.50774849792892418 ) ) ;
#23332 = CARTESIAN_POINT ( 'NONE',  ( 198.8157103782086210, 286.2880836124806478, -18.60729372713428020 ) ) ;
#23333 = CARTESIAN_POINT ( 'NONE',  ( 164.3138894970802824, 246.0469903322357368, -2.642126690130961020 ) ) ;
#23334 = CARTESIAN_POINT ( 'NONE',  ( 155.4186054393023255, 261.4540742680644598, 17.05753227160644769 ) ) ;
#23335 = CARTESIAN_POINT ( 'NONE',  ( 179.8888715531147682, 274.4711782159853328, -17.82026667163308531 ) ) ;
#23336 = CARTESIAN_POINT ( 'NONE',  ( 159.8982049494451019, 278.5378777402860919, -9.810204408616700178 ) ) ;
#23337 = CARTESIAN_POINT ( 'NONE',  ( 156.7442704525034571, 261.1579551113846378, 17.82061976529222846 ) ) ;
#23338 = SHAPE_DEFINITION_REPRESENTATION ( #28168, #35972 ) ;
#23339 = CARTESIAN_POINT ( 'NONE',  ( 20.65934362447757167, 23.87878583063841376, -9.188101187500006262 ) ) ;
#23340 = LINE ( 'NONE', #30949, #51545 ) ;
#23341 = LINE ( 'NONE', #54229, #21495 ) ;
#23342 = CARTESIAN_POINT ( 'NONE',  ( 186.2747035149648696, 267.7638619178059685, -15.07880563748316227 ) ) ;
#23343 = ORIENTED_EDGE ( 'NONE', *, *, #79542, .T. ) ;
#23344 = CARTESIAN_POINT ( 'NONE',  ( 165.0528804069804494, 264.4852527057752241, -17.76608744198970768 ) ) ;
#23345 = CARTESIAN_POINT ( 'NONE',  ( 41.60633307851366425, 35.97253583063845639, -9.188101187500006262 ) ) ;
#23346 = CARTESIAN_POINT ( 'NONE',  ( 81.65310433048475147, 42.64019311979919991, 7.560891536010019287 ) ) ;
#23347 = CARTESIAN_POINT ( 'NONE',  ( 82.80564809338142140, 40.64392876451551473, -1.326136484204850197 ) ) ;
#23348 = EDGE_LOOP ( 'NONE', ( #11556, #86494, #10754, #78662 ) ) ;
#23349 = DIRECTION ( 'NONE',  ( -0.9708212084269268738, 0.2398044646550215042, 0.000000000000000000 ) ) ;
#23350 = CARTESIAN_POINT ( 'NONE',  ( 72.40747426417379984, 71.81324781307232286, -5.589457107701495175 ) ) ;
#23351 = CARTESIAN_POINT ( 'NONE',  ( -66.34925969370661392, 42.61035540433362456, -10.00000000000000000 ) ) ;
#23352 = CARTESIAN_POINT ( 'NONE',  ( 174.5432515410337544, 282.4104588529930311, -15.15290805577315680 ) ) ;
#23353=STYLED_ITEM('',(#100338),#45023);
#23354 = EDGE_CURVE ( 'NONE', #29582, #35319, #68829, .T. ) ;
#23355 = ORIENTED_EDGE ( 'NONE', *, *, #31964, .F. ) ;
#23356 = DIRECTION ( 'NONE',  ( -0.8660254037844387076, -0.4999999999999998890, -0.000000000000000000 ) ) ;
#23357 = ORIENTED_EDGE ( 'NONE', *, *, #94207, .T. ) ;
#23358 = CARTESIAN_POINT ( 'NONE',  ( 153.3859906278383676, 264.9746663937372091, -17.41799046551451013 ) ) ;
#23359 = CARTESIAN_POINT ( 'NONE',  ( 71.64316818921395225, 72.05741665177615118, -3.509880912999884917 ) ) ;
#23360 = DIRECTION ( 'NONE',  ( -0.8660254037844379305, -0.5000000000000014433, -0.000000000000000000 ) ) ;
#23361 = DIRECTION ( 'NONE',  ( 1.000000000000000000, 1.804112415015878984E-15, 0.000000000000000000 ) ) ;
#23363 = EDGE_LOOP ( 'NONE', ( #18412, #51644, #99432, #18690 ) ) ;
#23362 = EDGE_CURVE ( 'NONE', #13462, #82272, #362, .T. ) ;
#23364 = CARTESIAN_POINT ( 'NONE',  ( 190.3691966041315311, 300.9178746160123410, 0.1783449565851275009 ) ) ;
#23365 = CIRCLE ( 'NONE', #36319, 70.00000000000001421 ) ;
#23366 = CARTESIAN_POINT ( 'NONE',  ( 149.0598351764325002, 272.4677874370131576, -11.59078276432863674 ) ) ;
#23367 = ORIENTED_EDGE ( 'NONE', *, *, #3285, .T. ) ;
#23368 = CARTESIAN_POINT ( 'NONE',  ( 174.9148042186883174, 263.6164057622452219, -16.35743113487313138 ) ) ;
#23369 = CARTESIAN_POINT ( 'NONE',  ( 42.32809528168264990, 126.1521775423068163, 10.00000000000000000 ) ) ;
#23370 = ORIENTED_EDGE ( 'NONE', *, *, #44772, .T. ) ;
#23371 = CARTESIAN_POINT ( 'NONE',  ( 26.87427219475921092, 30.91421378149919974, 9.188101187500008038 ) ) ;
#23372 = CARTESIAN_POINT ( 'NONE',  ( 148.9517569034208009, 272.6549844970639924, 12.50737104496728236 ) ) ;
#23373 = LINE ( 'NONE', #77608, #70923 ) ;
#23374 = ORIENTED_EDGE ( 'NONE', *, *, #62981, .T. ) ;
#23375 = PLANE ( 'NONE',  #95141 ) ;
#23376 = CARTESIAN_POINT ( 'NONE',  ( 159.5956778034477281, 255.1851156857001115, 15.94425648350737745 ) ) ;
#23377 = CARTESIAN_POINT ( 'NONE',  ( 74.93017357788676236, 189.2419560658248940, -17.47570218321535052 ) ) ;
#23378 = CARTESIAN_POINT ( 'NONE',  ( -59.29375005653866282, 35.37083770076974076, 177.5919119679930134 ) ) ;
#23379 = EDGE_LOOP ( 'NONE', ( #86465, #50146, #4722, #89582 ) ) ;
#23380 = VERTEX_POINT ( 'NONE', #17051 ) ;
#23381 = CARTESIAN_POINT ( 'NONE',  ( 86.85148033070495899, 46.48268733558807497, 9.045030158509874241 ) ) ;
#23382 = CARTESIAN_POINT ( 'NONE',  ( 77.00817486789590305, 205.2677522451417929, -5.000000000000041744 ) ) ;
#23383 = CARTESIAN_POINT ( 'NONE',  ( 190.0515794655415789, 301.4680036374047063, -1.296825456579539626 ) ) ;
#23384 = ORIENTED_EDGE ( 'NONE', *, *, #83883, .T. ) ;
#23385 = CARTESIAN_POINT ( 'NONE',  ( 190.0445576990143195, 301.4801656937889902, 4.140328216824785912 ) ) ;
#23386 = CARTESIAN_POINT ( 'NONE',  ( 171.0076562725379858, 275.6637320423262736, -16.75718656872113499 ) ) ;
#23387 = CARTESIAN_POINT ( 'NONE',  ( 146.5086121934486982, 276.8866352649785654, -0.04230388357226919777 ) ) ;
#23388 = CARTESIAN_POINT ( 'NONE',  ( 193.1028332910263998, 296.1830769848763225, -12.04975758233223893 ) ) ;
#23389 = CARTESIAN_POINT ( 'NONE',  ( 190.0259678364800493, 301.5123642802043946, 4.004183174499006626 ) ) ;
#23390 = CARTESIAN_POINT ( 'NONE',  ( 82.93017357788667709, 175.3855496052738374, 36.50000000000000000 ) ) ;
#23391 = CARTESIAN_POINT ( 'NONE',  ( 96.99346744615054661, 215.2592609112380160, 2.679491924311254714 ) ) ;
#23392 = CARTESIAN_POINT ( 'NONE',  ( 67.59761362805406293, 66.71094541649533483, 8.633997586817105940 ) ) ;
#23393 = CARTESIAN_POINT ( 'NONE',  ( 154.5219726700536569, 264.1077093662300399, -17.00691965702323216 ) ) ;
#23394 = CARTESIAN_POINT ( 'NONE',  ( 78.12507825963197661, 47.72428238059148953, 14.50788938415275986 ) ) ;
#23395 = CARTESIAN_POINT ( 'NONE',  ( 108.1307024963493149, 242.4244531367911293, -4.594050593750046652 ) ) ;
#23396 = ORIENTED_EDGE ( 'NONE', *, *, #87559, .F. ) ;
#23397 = CARTESIAN_POINT ( 'NONE',  ( 191.8329718516215223, 298.3825415164982928, -8.871589506312979267 ) ) ;
#23398 = DIRECTION ( 'NONE',  ( -0.03487823687206607903, 0.06041087834084090530, 0.9975640502598237536 ) ) ;
#23399 = CARTESIAN_POINT ( 'NONE',  ( 87.65912573706349065, 45.31011780831707370, -7.252675111195947544 ) ) ;
#23400 = CARTESIAN_POINT ( 'NONE',  ( 203.2187760522547819, 278.6617501559703101, -15.08675642319914978 ) ) ;
#23401 = EDGE_CURVE ( 'NONE', #58030, #48601, #46958, .T. ) ;
#23402 = CARTESIAN_POINT ( 'NONE',  ( 190.9889137617930714, 298.2006275540064735, -9.555045851526354994 ) ) ;
#23403 = EDGE_CURVE ( 'NONE', #4764, #61618, #48205, .T. ) ;
#23404 = CARTESIAN_POINT ( 'NONE',  ( 83.82342001511069896, 52.04024975599947567, -14.96847033955516260 ) ) ;
#23405 = CARTESIAN_POINT ( 'NONE',  ( 165.8799236907572379, 283.6072792123424620, -8.180192921770395031 ) ) ;
#23406 = ORIENTED_EDGE ( 'NONE', *, *, #2276, .T. ) ;
#23407 = CARTESIAN_POINT ( 'NONE',  ( 163.2000388741132895, 247.9762362032568035, -11.19676374274550312 ) ) ;
#23408 = EDGE_CURVE ( 'NONE', #98986, #24620, #81400, .T. ) ;
#23409 = CARTESIAN_POINT ( 'NONE',  ( 72.17587820367440088, 71.48161267280252673, 5.042060180291768390 ) ) ;
#23410 = CARTESIAN_POINT ( 'NONE',  ( 51.53259423990365917, 193.8927522451418213, 10.00000000000009592 ) ) ;
#23411 = CARTESIAN_POINT ( 'NONE',  ( 135.6816562978893330, 239.9548013555409796, -4.594050593750042211 ) ) ;
#23412 = CARTESIAN_POINT ( 'NONE',  ( 150.8168331730346949, 269.4245776381016526, -15.71017957295074652 ) ) ;
#23413 = CARTESIAN_POINT ( 'NONE',  ( 168.8785100482814698, 272.6966330010931756, 17.41127854651366391 ) ) ;
#23414 = CARTESIAN_POINT ( 'NONE',  ( 39.80235952159635815, 84.99999999999998579, 59.99999999999999289 ) ) ;
#23415 = CARTESIAN_POINT ( 'NONE',  ( 79.99999999999998579, 9.999999999999985789, -2.622423327744149102 ) ) ;
#23416 = CARTESIAN_POINT ( 'NONE',  ( 52.11020483269097525, 191.7048013555409796, 4.594050593750051981 ) ) ;
#23417 = CARTESIAN_POINT ( 'NONE',  ( 68.49666587867349676, 66.34648026219538508, -9.764362443893059407 ) ) ;
#23418 = ORIENTED_EDGE ( 'NONE', *, *, #46881, .T. ) ;
#23419 = CARTESIAN_POINT ( 'NONE',  ( 71.29672626941692215, 64.26515988479742703, 12.96738178296346966 ) ) ;
#23420 = CARTESIAN_POINT ( 'NONE',  ( -69.85371643402891095, 44.28081239092799848, 177.5919119679930134 ) ) ;
#23421 = CARTESIAN_POINT ( 'NONE',  ( 80.20857538925844210, 44.21345027839176112, -11.30608575764589752 ) ) ;
#23422 = CARTESIAN_POINT ( 'NONE',  ( 190.9586609929293104, 299.8968923453624598, -4.970176667899034229 ) ) ;
#23423 = CARTESIAN_POINT ( 'NONE',  ( 110.0000000000000000, 0.000000000000000000, 59.99999999999999289 ) ) ;
#23424 = VECTOR ( 'NONE', #69123, 1000.000000000000000 ) ;
#23425 = CARTESIAN_POINT ( 'NONE',  ( -19.65312891409030271, 93.06504152958497400, -60.00000000000000000 ) ) ;
#23426 = CARTESIAN_POINT ( 'NONE',  ( 178.5107126437189038, 260.9283949996104752, 13.53338759835929395 ) ) ;
#23427 = EDGE_CURVE ( 'NONE', #18286, #3234, #83624, .T. ) ;
#23428 = CARTESIAN_POINT ( 'NONE',  ( 105.5870131927823081, 241.7677522451419065, -5.000000000000047962 ) ) ;
#23429 = B_SPLINE_SURFACE_WITH_KNOTS ( 'NONE', 3, 1, ( 
 ( #82725, #89343 ),
 ( #74093, #28984 ),
 ( #13295, #3699 ),
 ( #4686, #97399 ),
 ( #67466, #89817 ),
 ( #98392, #88852 ),
 ( #20391, #74607 ),
 ( #36062, #5181 ),
 ( #44154, #75090 ),
 ( #5669, #59859 ),
 ( #90822, #21375 ),
 ( #52264, #11313 ),
 ( #45644, #84214 ),
 ( #75580, #29963 ),
 ( #85202, #54234 ),
 ( #14761, #6167 ),
 ( #83203, #7661 ),
 ( #83710, #91302 ),
 ( #53260, #22857 ),
 ( #38549, #53741 ),
 ( #91800, #52748 ),
 ( #84701, #76571 ),
 ( #44646, #61353 ),
 ( #61845, #15746 ),
 ( #92308, #8167 ),
 ( #21864, #14268 ),
 ( #7152, #15240 ),
 ( #30461, #45159 ),
 ( #93294, #46137 ),
 ( #92792, #76097 ),
 ( #39038, #23346 ) ),
 .UNSPECIFIED., .F., .F., .F.,
 ( 4, 3, 3, 3, 3, 3, 3, 3, 3, 3, 4 ),
 ( 2, 2 ),
 ( 0.000000000000000000, 0.1122669598086733639, 0.2243161639709615740, 0.3396355846219071828, 0.4553962076585117424, 0.5677860799922423984, 0.6749047109689585433, 0.7773884377078229546, 0.8775581155834157876, 0.9782364162377870098, 1.000000000000000000 ),
 ( 0.000000000000000000, 1.000000000000000000 ),
 .UNSPECIFIED. ) ;
#23430 = DIRECTION ( 'NONE',  ( 1.000000000000000000, 0.000000000000000000, 0.000000000000000000 ) ) ;
#23431 = VERTEX_POINT ( 'NONE', #88523 ) ;
#23432 = AXIS2_PLACEMENT_3D ( 'NONE', #26486, #72604, #10785 ) ;
#23433 = CARTESIAN_POINT ( 'NONE',  ( 147.9710862514405960, 274.3535558917855042, 7.785500222159708272 ) ) ;
#23434 = CARTESIAN_POINT ( 'NONE',  ( 20.71649992267561302, 12.36477965099639853, 1.583844403245364907 ) ) ;
#23435 = CARTESIAN_POINT ( 'NONE',  ( 25.77753312492912841, 179.5643266524160140, -9.188101187500093303 ) ) ;
#23436 = CARTESIAN_POINT ( 'NONE',  ( 16.72324493992723049, 11.78380873178785748, -6.180339887498949025 ) ) ;
#23437 = LINE ( 'NONE', #31539, #54834 ) ;
#23438 = DIRECTION ( 'NONE',  ( 0.000000000000000000, -0.000000000000000000, -1.000000000000000000 ) ) ;
#23439 = PLANE ( 'NONE',  #29679 ) ;
#23441 = CARTESIAN_POINT ( 'NONE',  ( 61.01376819352597636, 206.0333772461660544, 9.188101187500095079 ) ) ;
#23440 = CARTESIAN_POINT ( 'NONE',  ( 194.8648160861291103, 275.0048917464952183, -16.07792121436337851 ) ) ;
#23442 = CARTESIAN_POINT ( 'NONE',  ( 200.1782072557437857, 283.9281697954355650, 18.05177561285849208 ) ) ;
#23443 = CARTESIAN_POINT ( 'NONE',  ( 73.09454433421316821, 57.18998214774231315, 16.39745951563025628 ) ) ;
#23444 = CARTESIAN_POINT ( 'NONE',  ( 69.17743059381074033, 64.85395446877666359, 12.24194748396287480 ) ) ;
#23445 = CARTESIAN_POINT ( 'NONE',  ( 9.082762260191243442, 27.01751292744054567, 6.180339887498949913 ) ) ;
#23446 = ORIENTED_EDGE ( 'NONE', *, *, #16924, .F. ) ;
#23447 = CARTESIAN_POINT ( 'NONE',  ( 26.94108121515588294, 196.3615022471903160, 5.000000000000046185 ) ) ;
#23448 = CARTESIAN_POINT ( 'NONE',  ( 208.0045976720423084, 270.3724639545367836, 2.002128742561712471 ) ) ;
#23449 = CARTESIAN_POINT ( 'NONE',  ( 143.0153750664825054, 259.5024278399160949, -9.188101187500093303 ) ) ;
#23450 = CARTESIAN_POINT ( 'NONE',  ( 29.08566721201706784, 38.83396525600392124, -2.839279412974133887 ) ) ;
#23451 = CARTESIAN_POINT ( 'NONE',  ( 189.1724466617436349, 261.8427108266350274, 6.584756579409549282 ) ) ;
#23452 = CARTESIAN_POINT ( 'NONE',  ( 205.8610808625997208, 274.0851439753691920, 10.38803237360972531 ) ) ;
#23453 = CARTESIAN_POINT ( 'NONE',  ( 202.5128468779458331, 267.1751508879428343, 0.8823122286173835649 ) ) ;
#23454 = CARTESIAN_POINT ( 'NONE',  ( 66.45738049687504656, 68.75004886898103962, 2.331916367499077047 ) ) ;
#23455 = VERTEX_POINT ( 'NONE', #25673 ) ;
#23456 = CARTESIAN_POINT ( 'NONE',  ( 166.8533131785278272, 247.0304541540030243, 3.784327470570368224 ) ) ;
#23457 = DIRECTION ( 'NONE',  ( 1.000000000000000000, 0.000000000000000000, 0.000000000000000000 ) ) ;
#23458 = EDGE_CURVE ( 'NONE', #33315, #98890, #31335, .T. ) ;
#23459 = CARTESIAN_POINT ( 'NONE',  ( 178.1412175327710656, 285.9644113652241231, 12.86296424501218461 ) ) ;
#23460 = DIRECTION ( 'NONE',  ( 0.1266907948509090887, -0.9919422576440851680, 0.000000000000000000 ) ) ;
#23461 = CARTESIAN_POINT ( 'NONE',  ( 6.194340351808173217, 26.68290643055185285, 3.479690158560446702E-15 ) ) ;
#23462 = VERTEX_POINT ( 'NONE', #9974 ) ;
#23463 = DIRECTION ( 'NONE',  ( -0.4556638457577367740, 0.000000000000000000, 0.8901519306664842368 ) ) ;
#23464 = VECTOR ( 'NONE', #97267, 1000.000000000000114 ) ;
#23465 = DIRECTION ( 'NONE',  ( 0.5000000000000048850, -0.8660254037844358210, 0.000000000000000000 ) ) ;
#23466 = CARTESIAN_POINT ( 'NONE',  ( 192.0332533962074706, 298.0356437054567778, 11.70630383928353346 ) ) ;
#23467 = CARTESIAN_POINT ( 'NONE',  ( 73.51948839908328637, 69.73627507762921596, -9.361350578256052657 ) ) ;
#23468 = CARTESIAN_POINT ( 'NONE',  ( 181.4283053378885597, 267.7238133557910373, 16.48022347432943135 ) ) ;
#23469 = CARTESIAN_POINT ( 'NONE',  ( 208.3194307158603067, 269.8271571267425770, -2.120200867047394855 ) ) ;
#23470 = CYLINDRICAL_SURFACE ( 'NONE', #6332, 14.99999999999967493 ) ;
#23471 = ORIENTED_EDGE ( 'NONE', *, *, #70133, .F. ) ;
#23472 = VERTEX_POINT ( 'NONE', #56554 ) ;
#23473 = CARTESIAN_POINT ( 'NONE',  ( 190.7633961518363890, 281.0789110243076721, 16.67417094886322460 ) ) ;
#23474 = CARTESIAN_POINT ( 'NONE',  ( 171.6334153394907389, 249.3410379734025923, 0.9431220288450494760 ) ) ;
#23475 = ORIENTED_EDGE ( 'NONE', *, *, #50394, .F. ) ;
#23476 = CARTESIAN_POINT ( 'NONE',  ( 69.85203827438495239, 67.76287465637892637, 9.808276934428768357 ) ) ;
#23477 = CARTESIAN_POINT ( 'NONE',  ( 82.46142967334674267, 45.35300679235661647, -10.49381007413441580 ) ) ;
#23478 = ORIENTED_EDGE ( 'NONE', *, *, #87220, .F. ) ;
#23479 = CARTESIAN_POINT ( 'NONE',  ( 146.8637854207107409, 276.2714571898724216, 0.7988785540157756770 ) ) ;
#23480 = CARTESIAN_POINT ( 'NONE',  ( 79.50781411973173363, 59.26880192752088305, -16.22028800479747801 ) ) ;
#23481 = DIRECTION ( 'NONE',  ( -0.8660254037844387076, -0.4999999999999998890, -0.000000000000000000 ) ) ;
#23482 = CARTESIAN_POINT ( 'NONE',  ( 75.31289280905393468, 53.62176160565092431, -16.53289957284814093 ) ) ;
#23483 = CARTESIAN_POINT ( 'NONE',  ( 69.93520613851926271, 62.85125605636124391, 13.88333920316857650 ) ) ;
#23484 = ORIENTED_EDGE ( 'NONE', *, *, #90641, .F. ) ;
#23485 = CARTESIAN_POINT ( 'NONE',  ( 161.3193951073452581, 251.2336067582368742, 13.01220207292984377 ) ) ;
#23486 = CARTESIAN_POINT ( 'NONE',  ( 136.1324508756439400, 242.7365022471902307, 10.00000000000009948 ) ) ;
#23487 = CARTESIAN_POINT ( 'NONE',  ( 191.5694459269389824, 298.8389818071599962, 7.944420692511652504 ) ) ;
#23488 = CARTESIAN_POINT ( 'NONE',  ( 48.29091023345864642, 82.53782597618220507, 10.00000000000000000 ) ) ;
#23489 = ORIENTED_EDGE ( 'NONE', *, *, #68382, .F. ) ;
#23490 = ORIENTED_EDGE ( 'NONE', *, *, #72763, .F. ) ;
#23491 = ORIENTED_EDGE ( 'NONE', *, *, #62695, .F. ) ;
#23492 = CARTESIAN_POINT ( 'NONE',  ( 73.12515255232021616, 60.21910268995390680, 15.28705970489183841 ) ) ;
#23493 = VECTOR ( 'NONE', #19919, 1000.000000000000000 ) ;
#23494 = ORIENTED_EDGE ( 'NONE', *, *, #75401, .F. ) ;
#23495 = DIRECTION ( 'NONE',  ( -0.8660254037844387076, -0.4999999999999998890, -0.000000000000000000 ) ) ;
#23496 = EDGE_LOOP ( 'NONE', ( #26354, #46080, #57923, #60999 ) ) ;
#23497 = CARTESIAN_POINT ( 'NONE',  ( 207.6932907333322191, 270.9116633891313199, 2.120963121341169710 ) ) ;
#23498 = CARTESIAN_POINT ( 'NONE',  ( 81.14441644904596274, 43.83121929228919811, 9.603772945707428121 ) ) ;
#23499 = CARTESIAN_POINT ( 'NONE',  ( 167.0456650196674673, 282.1831978616474998, 12.11327121657329542 ) ) ;
#23500 = CARTESIAN_POINT ( 'NONE',  ( 147.9791529310278122, 274.3395839928920168, -7.789432462804474433 ) ) ;
#23501 = CARTESIAN_POINT ( 'NONE',  ( 67.07370046796862084, 68.19344093013617680, -5.526046699112809435 ) ) ;
#23502 = CARTESIAN_POINT ( 'NONE',  ( -22.42236680055709641, 157.8615022471902591, 0.000000000000000000 ) ) ;
#23503 = ORIENTED_EDGE ( 'NONE', *, *, #9183, .F. ) ;
#23504 = CARTESIAN_POINT ( 'NONE',  ( 166.0832898494950030, 246.9231440688584769, 1.898682735395063714 ) ) ;
#23505 = CARTESIAN_POINT ( 'NONE',  ( 20.49695707787433463, 14.76004757982089188, 5.678558825948272215 ) ) ;
#23506 = CARTESIAN_POINT ( 'NONE',  ( 198.4136990093444126, 277.2144854508601384, -15.28644943941467993 ) ) ;
#23507 = CARTESIAN_POINT ( 'NONE',  ( -70.00000000000000000, 15.00000000000000000, 59.99999999999999289 ) ) ;
#23509 = ORIENTED_EDGE ( 'NONE', *, *, #23307, .F. ) ;
#23508 = CARTESIAN_POINT ( 'NONE',  ( 206.9275546910526486, 270.9267086679434442, 4.961599381757848981 ) ) ;
#23510 = CARTESIAN_POINT ( 'NONE',  ( 147.0294190956623481, 275.9845712494116583, -4.172428427132245154 ) ) ;
#23511 = CARTESIAN_POINT ( 'NONE',  ( 70.37934122712871954, 61.23818324669216651, 14.28954007458889386 ) ) ;
#23512 = CARTESIAN_POINT ( 'NONE',  ( 206.6912923161529818, 272.6471755567893638, -9.325620632947922317 ) ) ;
#23513 = CARTESIAN_POINT ( 'NONE',  ( 165.5694811585547654, 246.8511483137207563, -2.318198762934976731 ) ) ;
#23514 = EDGE_CURVE ( 'NONE', #6423, #48869, #49462, .T. ) ;
#23515 = CARTESIAN_POINT ( 'NONE',  ( 80.82947773944196967, 46.16309167796865864, -12.01060402535779836 ) ) ;
#23516 = CARTESIAN_POINT ( 'NONE',  ( 172.0057192551458343, 254.5726738447181106, 11.30606058533757796 ) ) ;
#23517 = ADVANCED_FACE ( 'NONE', ( #82893 ), #21077, .F. ) ;
#23518 = CARTESIAN_POINT ( 'NONE',  ( 194.8319568529400385, 263.3227001520926933, -0.7902351138979081258 ) ) ;
#23519 =( BOUNDED_CURVE ( )  B_SPLINE_CURVE ( 2, ( #47290, #78215, #92928, #87748, #30607, #15892, #45782, #85345, #80119, #38178, #15378, #8801, #77200 ),
 .UNSPECIFIED., .F., .T. ) 
 B_SPLINE_CURVE_WITH_KNOTS ( ( 3, 2, 2, 2, 2, 2, 3 ),
 ( 0.1375000000000000111, 0.1400000000000000133, 0.1449999999999999900, 0.1499999999999999944, 0.1549999999999999989, 0.1600000000000000033, 0.1625000000000000056 ),
 .UNSPECIFIED. ) 
 CURVE ( )  GEOMETRIC_REPRESENTATION_ITEM ( )  RATIONAL_B_SPLINE_CURVE ( ( 0.9755282581475768211, 0.9755282581475768211, 1.000000000000000000, 0.9510565162951535312, 1.000000000000000000, 0.9510565162951535312, 1.000000000000000000, 0.9510565162951535312, 1.000000000000000000, 0.9510565162951535312, 1.000000000000000000, 0.9755282581475768211, 0.9755282581475768211 ) ) 
 REPRESENTATION_ITEM ( '' )  );
#23520 = VERTEX_POINT ( 'NONE', #5358 ) ;
#23521 = CARTESIAN_POINT ( 'NONE',  ( 194.2565597998853377, 294.1847640534938364, -14.09590134157931374 ) ) ;
#23522 = CARTESIAN_POINT ( 'NONE',  ( 74.70969265356585254, 66.80295132244253864, -13.14574923971307463 ) ) ;
#23523 = DIRECTION ( 'NONE',  ( -0.4340522123146939859, 0.9008877160804890094, 0.000000000000000000 ) ) ;
#23524 = EDGE_CURVE ( 'NONE', #79763, #21882, #90612, .T. ) ;
#23525 = CARTESIAN_POINT ( 'NONE',  ( 5.488910272030937065, 180.6427522451419350, -10.00000000000009415 ) ) ;
#23526 = CARTESIAN_POINT ( 'NONE',  ( 83.31357524521028779, 231.1589784336661353, -6.496448406907676862E-16 ) ) ;
#23527 = CARTESIAN_POINT ( 'NONE',  ( 196.1279896863303520, 269.6123170192805105, -10.99537109092639220 ) ) ;
#23528 = CARTESIAN_POINT ( 'NONE',  ( 164.4568492923521887, 247.7993767033852919, 8.703614106482779889 ) ) ;
#23529 = LINE ( 'NONE', #53437, #83900 ) ;
#23531 = DIRECTION ( 'NONE',  ( 0.1710100716628310258, -0.2961981327260192476, 0.9396926207859104263 ) ) ;
#23530 = CARTESIAN_POINT ( 'NONE',  ( 8.375921941576814689, 166.4548013555410080, -4.594050593750042211 ) ) ;
#23532 = CARTESIAN_POINT ( 'NONE',  ( 161.7910648966377209, 250.4166507187868831, 13.19274492748169436 ) ) ;
#23533 = VERTEX_POINT ( 'NONE', #67145 ) ;
#23534 = ORIENTED_EDGE ( 'NONE', *, *, #70529, .F. ) ;
#23535 = CARTESIAN_POINT ( 'NONE',  ( 197.5258556021618688, 265.2381013607024443, -2.939624273662967635 ) ) ;
#23536 =( BOUNDED_CURVE ( )  B_SPLINE_CURVE ( 2, ( #94276, #95299, #24831, #86694, #71456, #87716, #95794, #26348, #57224 ),
 .UNSPECIFIED., .F., .T. ) 
 B_SPLINE_CURVE_WITH_KNOTS ( ( 3, 2, 2, 2, 3 ),
 ( 0.6250000000000000000, 0.6263440860215053752, 0.6290322580645161255, 0.6317204301075268758, 0.6330645161290322509 ),
 .UNSPECIFIED. ) 
 CURVE ( )  GEOMETRIC_REPRESENTATION_ITEM ( )  RATIONAL_B_SPLINE_CURVE ( ( 0.9330127018922194093, 0.9330127018922194093, 1.000000000000000000, 0.8660254037844387076, 1.000000000000000000, 0.8660254037844387076, 1.000000000000000000, 0.9330127018922194093, 0.9330127018922194093 ) ) 
 REPRESENTATION_ITEM ( '' )  );
#23537 = CARTESIAN_POINT ( 'NONE',  ( 112.6979501180548766, 224.3262482093457777, 3.021315404115420679E-15 ) ) ;
#23538 = AXIS2_PLACEMENT_3D ( 'NONE', #42462, #12599, #34868 ) ;
#23539 = CARTESIAN_POINT ( 'NONE',  ( 163.8835510476618254, 277.4261113242017132, -14.47671527678674330 ) ) ;
#23540 = CARTESIAN_POINT ( 'NONE',  ( 82.26786778050022519, 42.61060261517380354, 6.935189047524418449 ) ) ;
#23541 = CARTESIAN_POINT ( 'NONE',  ( 74.18809600170575891, 68.48282398988669684, -11.62097119590897520 ) ) ;
#23542 = B_SPLINE_CURVE_WITH_KNOTS ( 'NONE', 3,
 ( #78916, #47970, #26688, #80438 ),
 .UNSPECIFIED., .F., .F.,
 ( 4, 4 ),
 ( 0.008386952484578737849, 0.01475959061312598006 ),
 .UNSPECIFIED. ) ;
#23543 = CARTESIAN_POINT ( 'NONE',  ( 35.30381256655795852, 185.0643266524160140, 9.188101187500095079 ) ) ;
#23544 = CARTESIAN_POINT ( 'NONE',  ( 119.6866422041566693, 252.1589784336661637, -6.496448406907675876E-16 ) ) ;
#23545 = CARTESIAN_POINT ( 'NONE',  ( 199.3879857545408640, 277.4998007522424359, 15.19030560797578389 ) ) ;
#23546 = ORIENTED_EDGE ( 'NONE', *, *, #53148, .F. ) ;
#23547 = CARTESIAN_POINT ( 'NONE',  ( 153.2461334198073075, 273.7581969524157444, -11.86170745181470387 ) ) ;
#23548 = DIRECTION ( 'NONE',  ( -0.3696446237802352708, -0.9291732088853876803, 0.000000000000000000 ) ) ;
#23549 = CARTESIAN_POINT ( 'NONE',  ( 80.65606772055953400, 57.41663775889262666, -16.23641822966148851 ) ) ;
#23550 = CARTESIAN_POINT ( 'NONE',  ( 194.3562588153086779, 294.0120802933159325, 14.11474987148825200 ) ) ;
#23551 = CARTESIAN_POINT ( 'NONE',  ( 184.5123196318015459, 277.1383014161853566, -17.82024832176989904 ) ) ;
#23552 = AXIS2_PLACEMENT_3D ( 'NONE', #29794, #21699, #392 ) ;
#23553 = LINE ( 'NONE', #76302, #20881 ) ;
#23554 = CARTESIAN_POINT ( 'NONE',  ( 194.2223991963907963, 294.2439319543634610, -14.97294938100067441 ) ) ;
#23555 = CARTESIAN_POINT ( 'NONE',  ( 73.42390341037517487, 68.98804980449470747, 10.73942965338376254 ) ) ;
#23556 = CARTESIAN_POINT ( 'NONE',  ( 163.2645943797325572, 249.2862317762373436, -10.33311602661124518 ) ) ;
#23557 = CYLINDRICAL_SURFACE ( 'NONE', #5456, 10.00000000000010658 ) ;
#23558 = CARTESIAN_POINT ( 'NONE',  ( 69.95749256914241698, 70.12926228225454395, 4.955899210846575365 ) ) ;
#23559 = LINE ( 'NONE', #31659, #58179 ) ;
#23560 = LINE ( 'NONE', #54452, #5941 ) ;
#23561 = ORIENTED_EDGE ( 'NONE', *, *, #68907, .F. ) ;
#23562 = AXIS2_PLACEMENT_3D ( 'NONE', #39220, #40225, #78261 ) ;
#23563 = DIRECTION ( 'NONE',  ( -1.000000000000000000, 0.000000000000000000, 0.000000000000000000 ) ) ;
#23564 = CARTESIAN_POINT ( 'NONE',  ( 182.1962218731464134, 268.3183306110546482, 15.02138923653300218 ) ) ;
#23565 = CARTESIAN_POINT ( 'NONE',  ( 121.5276403787286483, 228.7202760586659736, -5.415160957724236172E-17 ) ) ;
#23566 = CARTESIAN_POINT ( 'NONE',  ( 11.61057445305848823, 22.10171378149917842, 9.188101187500008038 ) ) ;
#23567 = ORIENTED_EDGE ( 'NONE', *, *, #20031, .F. ) ;
#23568 = CARTESIAN_POINT ( 'NONE',  ( 150.6655900823359389, 269.6865383554857090, 15.31288044136207205 ) ) ;
#23569 = CARTESIAN_POINT ( 'NONE',  ( 74.14070847040734691, 58.91510108708826721, -16.21268320586513667 ) ) ;
#23570 = CARTESIAN_POINT ( 'NONE',  ( 195.6627736265002682, 278.3332898145053491, 16.90917068752747809 ) ) ;
#23571 = CARTESIAN_POINT ( 'NONE',  ( 150.7162572431468561, 269.5987802586857924, -13.73098793484843405 ) ) ;
#23572 = B_SPLINE_CURVE_WITH_KNOTS ( 'NONE', 3,
 ( #50770, #36562, #6674, #97894, #44649, #89820, #28987, #20395, #89346, #90326, #75584, #20900, #51265, #5185, #44158, #21867, #81721, #51789, #6170, #37067, #12297, #67971, #98892, #93297, #16759, #7156, #70459, #22366, #86223, #62343, #69462, #45647, #76575, #24370, #84218, #93810, #38043, #99879, #15245, #69951, #77, #7666, #40043, #60843, #78078, #9169 ),
 .UNSPECIFIED., .F., .F.,
 ( 4, 1, 1, 1, 2, 2, 1, 1, 1, 2, 2, 1, 1, 2, 2, 1, 1, 2, 2, 1, 1, 2, 2, 1, 2, 2, 1, 2, 2, 4 ),
 ( 0.000000000000000000, 0.06250000000000936751, 0.09375000000001323941, 0.1093750000000151545, 0.1171875000000152933, 0.1250000000000154321, 0.1875000000000056899, 0.2187500000000019706, 0.2343749999999997224, 0.2421874999999978628, 0.2499999999999960032, 0.3124999999999953371, 0.3437499999999956701, 0.3593749999999965028, 0.3749999999999973355, 0.4375000000000029976, 0.4687500000000058842, 0.4843750000000073275, 0.5000000000000087708, 0.5625000000000085487, 0.5937500000000077716, 0.6093750000000073275, 0.6250000000000068834, 0.6875000000000107692, 0.7187500000000114353, 0.7500000000000121014, 0.8125000000000128786, 0.8437500000000117684, 0.8750000000000106581, 1.000000000000000000 ),
 .UNSPECIFIED. ) ;
#23573 = CARTESIAN_POINT ( 'NONE',  ( 150.7691137448031213, 269.5072301123068428, -15.63821625702598084 ) ) ;
#23574 = DIRECTION ( 'NONE',  ( -0.000000000000000000, -0.000000000000000000, -1.000000000000000000 ) ) ;
#23575 = EDGE_CURVE ( 'NONE', #100024, #69721, #74779, .T. ) ;
#23576 = CARTESIAN_POINT ( 'NONE',  ( 175.0296968597178306, 264.6864531019056699, -16.70299667166197466 ) ) ;
#23577 = CARTESIAN_POINT ( 'NONE',  ( 146.9422184197532317, 276.1356072505412840, -5.063317562214876943 ) ) ;
#23578 = CARTESIAN_POINT ( 'NONE',  ( 66.89668164680340112, 69.73571018825775525, 0.6674377462804911287 ) ) ;
#23579 = ORIENTED_EDGE ( 'NONE', *, *, #52802, .F. ) ;
#23580 = CARTESIAN_POINT ( 'NONE',  ( 164.3645038749433525, 256.7011479335206445, -14.91022226314676402 ) ) ;
#23581 = DIRECTION ( 'NONE',  ( -0.8660254037844357100, -0.5000000000000049960, -0.000000000000000000 ) ) ;
#23582 = CARTESIAN_POINT ( 'NONE',  ( 81.22341047923954704, 48.06708024569342541, 13.74252432062430529 ) ) ;
#23583 = CARTESIAN_POINT ( 'NONE',  ( 196.9976074755333286, 289.4371302133026802, -16.79549473444794216 ) ) ;
#23584 = ORIENTED_EDGE ( 'NONE', *, *, #47287, .F. ) ;
#23585 = CARTESIAN_POINT ( 'NONE',  ( 75.84116199970137018, 65.13315491392486933, -14.47742810051069284 ) ) ;
#23587 = EDGE_CURVE ( 'NONE', #58638, #23003, #66650, .T. ) ;
#23586 = CARTESIAN_POINT ( 'NONE',  ( 180.1160312531098668, 262.9874791413300272, -12.84058704759554992 ) ) ;
#23588 = CARTESIAN_POINT ( 'NONE',  ( 72.40022343535652283, 71.86297034063233014, -5.456689119915505870 ) ) ;
#23589 = CARTESIAN_POINT ( 'NONE',  ( 74.95434044882874502, 53.24670644474785064, -16.03982845221052855 ) ) ;
#23590 = LINE ( 'NONE', #45885, #19393 ) ;
#23591 = VERTEX_POINT ( 'NONE', #68631 ) ;
#23592 = CARTESIAN_POINT ( 'NONE',  ( 73.33758058659837786, 69.90254644623917102, 9.645949167502998023 ) ) ;
#23593 = CARTESIAN_POINT ( 'NONE',  ( 38.84587710395076954, 34.37878583063844218, 9.188101187500006262 ) ) ;
#23594 = VERTEX_POINT ( 'NONE', #98067 ) ;
#23595 = CARTESIAN_POINT ( 'NONE',  ( 167.5863728346707830, 249.8758218121444656, 6.940154622966127285 ) ) ;
#23596 = EDGE_CURVE ( 'NONE', #28763, #15906, #51953, .T. ) ;
#23597 = LINE ( 'NONE', #47405, #51537 ) ;
#23598 = VERTEX_POINT ( 'NONE', #75265 ) ;
#23599 = CARTESIAN_POINT ( 'NONE',  ( 86.12135434523639788, 46.98046262810482432, -10.13131473785488268 ) ) ;
#23600 = CARTESIAN_POINT ( 'NONE',  ( 205.9050707304272407, 274.0089512892737389, 12.32231322111777772 ) ) ;
#23601 = CARTESIAN_POINT ( 'NONE',  ( 192.5381442786905666, 297.1611470447178363, -13.11433798472783074 ) ) ;
#23602 = PLANE ( 'NONE',  #67693 ) ;
#23603 = AXIS2_PLACEMENT_3D ( 'NONE', #71300, #81300, #73666 ) ;
#23604 = CARTESIAN_POINT ( 'NONE',  ( 119.0825757350898755, 232.8927522451418213, 10.00000000000009948 ) ) ;
#23605 = CARTESIAN_POINT ( 'NONE',  ( 81.35996782917339942, 56.22057934968196946, -16.44131086233301176 ) ) ;
#23606 = ORIENTED_EDGE ( 'NONE', *, *, #2141, .F. ) ;
#23607 = CARTESIAN_POINT ( 'NONE',  ( 195.7233648222712930, 290.9602864498907593, 16.00646756461187437 ) ) ;
#23608 = EDGE_LOOP ( 'NONE', ( #8809, #13794, #86714, #37581, #78724, #9406, #80355, #86475, #67151, #79423, #31254, #86823, #5923, #41180, #92068, #80132 ) ) ;
#23609 = CARTESIAN_POINT ( 'NONE',  ( 77.16544646929735052, 49.29022895602057019, -14.87484003624337880 ) ) ;
#23610 = VERTEX_POINT ( 'NONE', #35753 ) ;
#23611 = CARTESIAN_POINT ( 'NONE',  ( 87.17617632782311432, 45.93339551703158463, -8.679440343565334004 ) ) ;
#23612 = CARTESIAN_POINT ( 'NONE',  ( 79.83401254395657531, 57.87045807247318407, 16.26439772172797404 ) ) ;
#23613 = ORIENTED_EDGE ( 'NONE', *, *, #85332, .F. ) ;
#23614 = CARTESIAN_POINT ( 'NONE',  ( 165.4869498693733760, 275.0640536683063146, -15.87538405248356810 ) ) ;
#23615 = CARTESIAN_POINT ( 'NONE',  ( 26.40327033588000560, 37.01751292744058475, 6.180339887498949913 ) ) ;
#23616 = CARTESIAN_POINT ( 'NONE',  ( 190.1364579050488430, 301.3209898677110345, 2.002245206357507357 ) ) ;
#23617 = CARTESIAN_POINT ( 'NONE',  ( -57.77801984846012573, 31.16909059156539996, 10.00000000000000178 ) ) ;
#23618 = CARTESIAN_POINT ( 'NONE',  ( 192.7705129102570822, 296.7586727687594816, -13.39629674907774692 ) ) ;
#23619 = CARTESIAN_POINT ( 'NONE',  ( 167.7877716316831425, 248.9074273214486368, -5.048719896133492036 ) ) ;
#23620 = CARTESIAN_POINT ( 'NONE',  ( 77.00353437484392316, 62.91037619732002639, -15.26141501223570707 ) ) ;
#23621 = CARTESIAN_POINT ( 'NONE',  ( 183.5171238009618264, 284.3872251382956620, -15.26397248544439122 ) ) ;
#23622 = CARTESIAN_POINT ( 'NONE',  ( 124.3418758452630613, 242.5958772461660544, -9.188101187500095079 ) ) ;
#23623 = CARTESIAN_POINT ( 'NONE',  ( 70.52897103333525308, 60.84962709411536252, -15.02099117819446761 ) ) ;
#23624 = CARTESIAN_POINT ( 'NONE',  ( 160.1642720190261855, 283.6550828934768447, 2.228402901662201341 ) ) ;
#23625 = CARTESIAN_POINT ( 'NONE',  ( 180.4686939987674918, 291.6062955413669329, -9.874166343425045511 ) ) ;
#23626 = ORIENTED_EDGE ( 'NONE', *, *, #30863, .F. ) ;
#23627 = VERTEX_POINT ( 'NONE', #89514 ) ;
#23628 = VECTOR ( 'NONE', #50344, 1000.000000000000227 ) ;
#23629 = CARTESIAN_POINT ( 'NONE',  ( 62.50798602660126591, 180.9153022007868685, 4.041334437186263538E-16 ) ) ;
#23630 = ADVANCED_FACE ( 'NONE', ( #81896 ), #12473, .F. ) ;
#23631 = CARTESIAN_POINT ( 'NONE',  ( 175.8027662909930484, 284.8719843250962072, 14.11304877541382119 ) ) ;
#23632 = CARTESIAN_POINT ( 'NONE',  ( 174.1370939159656643, 290.5918216138747425, -4.894811010708814081 ) ) ;
#23633 = CARTESIAN_POINT ( 'NONE',  ( 49.83874514172083536, 101.4840343560033915, -10.00000000000000000 ) ) ;
#23634 = CARTESIAN_POINT ( 'NONE',  ( 71.83446468542571495, 61.06084060420133852, 14.73407088629796746 ) ) ;
#23635 = CARTESIAN_POINT ( 'NONE',  ( 200.9445292274600092, 282.6008612054670266, -16.62830946367346741 ) ) ;
#23636 = CARTESIAN_POINT ( 'NONE',  ( 78.25402821438737533, 51.50098827152044834, 15.87605948207779605 ) ) ;
#23637 = ORIENTED_EDGE ( 'NONE', *, *, #46067, .T. ) ;
#23638 = VECTOR ( 'NONE', #94140, 1000.000000000000000 ) ;
#23639 = CARTESIAN_POINT ( 'NONE',  ( 148.0129410789982103, 274.2810612039135094, 10.14596848016967279 ) ) ;
#23640 = CARTESIAN_POINT ( 'NONE',  ( 174.0965047066266038, 253.2374073076369427, -7.700682943850493345 ) ) ;
#23641 = VERTEX_POINT ( 'NONE', #67642 ) ;
#23642 = FACE_OUTER_BOUND ( 'NONE', #23084, .T. ) ;
#23643 = CARTESIAN_POINT ( 'NONE',  ( 65.80085019850238837, 69.11466268455660611, -0.2884749532225020507 ) ) ;
#23644 = VERTEX_POINT ( 'NONE', #98574 ) ;
#23645 = ADVANCED_FACE ( 'NONE', ( #83383 ), #13949, .F. ) ;
#23646 = CARTESIAN_POINT ( 'NONE',  ( 188.4786970353986248, 265.2655723350032986, -11.77073285016548354 ) ) ;
#23647 = ADVANCED_FACE ( 'NONE', ( #6351 ), #18878, .F. ) ;
#23648 = CARTESIAN_POINT ( 'NONE',  ( 194.4506751305639796, 264.6470882917897711, 4.421188665544642404 ) ) ;
#23649 = CARTESIAN_POINT ( 'NONE',  ( 149.6896757981861583, 271.3768714794653647, 12.49809796062302603 ) ) ;
#23650 = CARTESIAN_POINT ( 'NONE',  ( 8.086986483384254853, 182.1427522451419350, -10.00000000000009592 ) ) ;
#23652 = FACE_OUTER_BOUND ( 'NONE', #31248, .T. ) ;
#23651 = CARTESIAN_POINT ( 'NONE',  ( 164.2700632124239633, 284.1926600866962644, -7.004898476152563447 ) ) ;
#23653 = DIRECTION ( 'NONE',  ( 0.4999999999999998890, -0.8660254037844385966, 0.000000000000000000 ) ) ;
#23654 = ORIENTED_EDGE ( 'NONE', *, *, #79298, .T. ) ;
#23655 = CARTESIAN_POINT ( 'NONE',  ( 147.3984236761635884, 275.3454365677582700, 5.108566646342994844 ) ) ;
#23656 = CARTESIAN_POINT ( 'NONE',  ( 71.68455251971286657, 63.38995168949250569, 13.60462078634210670 ) ) ;
#23657 = CARTESIAN_POINT ( 'NONE',  ( 186.7529496275546421, 262.6979624853421456, -8.915494530226171221 ) ) ;
#23658 = LINE ( 'NONE', #67406, #99171 ) ;
#23659 = DIRECTION ( 'NONE',  ( 0.4999999999999992784, -0.8660254037844390407, 0.000000000000000000 ) ) ;
#23660 = CARTESIAN_POINT ( 'NONE',  ( 186.0996347449242307, 297.2146404166695675, -4.282800944430866785 ) ) ;
#23661 = CARTESIAN_POINT ( 'NONE',  ( 152.9920137376499838, 265.6570543845515431, 16.15798175643282164 ) ) ;
#23662 = CARTESIAN_POINT ( 'NONE',  ( 37.60401899570393880, 182.5177522451417929, 5.000000000000051514 ) ) ;
#23663 = CARTESIAN_POINT ( 'NONE',  ( 193.9844289374573520, 294.6561085335266625, 15.49818881749970245 ) ) ;
#23664 = CARTESIAN_POINT ( 'NONE',  ( 191.4011393215214412, 282.8345302558525987, -17.71497175083820608 ) ) ;
#23665 = CARTESIAN_POINT ( 'NONE',  ( 69.48347394385132247, 66.66933067140242031, -10.76623218384503744 ) ) ;
#23666 = CARTESIAN_POINT ( 'NONE',  ( 69.78227540684341079, 211.0958772461660544, -9.188101187500095079 ) ) ;
#23667 = CARTESIAN_POINT ( 'NONE',  ( 178.6317619811870259, 253.9327355832967612, -4.167451725846189170 ) ) ;
#23668 = CARTESIAN_POINT ( 'NONE',  ( 147.5118896528469179, 275.1489077312122049, -3.975523961781759930 ) ) ;
#23669 = CARTESIAN_POINT ( 'NONE',  ( 58.19016453504443831, 197.7365022471902307, 10.00000000000009948 ) ) ;
#23670 = CARTESIAN_POINT ( 'NONE',  ( 202.7973612924478743, 279.3916619310153919, -15.54732529288344089 ) ) ;
#23671 = VECTOR ( 'NONE', #92123, 1000.000000000000114 ) ;
#23672 = CARTESIAN_POINT ( 'NONE',  ( 78.61102955532449243, 58.84556920875776598, 16.19509477467131831 ) ) ;
#23673 = CARTESIAN_POINT ( 'NONE',  ( 84.57213519662508361, 49.80120436375268156, -13.19968558455237861 ) ) ;
#23674 = VECTOR ( 'NONE', #30968, 1000.000000000000000 ) ;
#23675 = CARTESIAN_POINT ( 'NONE',  ( 78.22442621354822734, 61.78027394037003006, 15.74819469288706664 ) ) ;
#23676 = CARTESIAN_POINT ( 'NONE',  ( 73.34339640511194602, 69.67785411864186074, -9.916893174164222557 ) ) ;
#23677 = CARTESIAN_POINT ( 'NONE',  ( 70.72288414528865985, 60.52409755963705607, -14.67628891625416898 ) ) ;
#23678 = CARTESIAN_POINT ( 'NONE',  ( 72.22334018239831721, 71.90115885523906059, -3.839516039074286180 ) ) ;
#23679 = CARTESIAN_POINT ( 'NONE',  ( -0.3647194387874375665, 159.0494855054051868, -2.679491924311248496 ) ) ;
#23680 = CARTESIAN_POINT ( 'NONE',  ( 164.6737691338994978, 245.4236605166554739, -4.507742726242741860 ) ) ;
#23681 = CARTESIAN_POINT ( 'NONE',  ( 195.9920715006079490, 291.1787696107118677, 15.99608784761372071 ) ) ;
#23682 = FACE_OUTER_BOUND ( 'NONE', #65080, .T. ) ;
#23683 = CARTESIAN_POINT ( 'NONE',  ( 159.9040744856012850, 255.4269131533854420, 16.38690128260775936 ) ) ;
#23684 = CARTESIAN_POINT ( 'NONE',  ( 43.58535403812915376, 183.7202760586659736, -5.415160957724236172E-17 ) ) ;
#23685 = CARTESIAN_POINT ( 'NONE',  ( 58.14488549560751807, 210.5024278399160949, 9.188101187500095079 ) ) ;
#23686 = CARTESIAN_POINT ( 'NONE',  ( 192.4619825937016060, 278.6107209869106214, -17.59187769095188969 ) ) ;
#23687 = CARTESIAN_POINT ( 'NONE',  ( 88.28323348104321155, 43.74655523625713016, 0.1991997974169889829 ) ) ;
#23688 = CARTESIAN_POINT ( 'NONE',  ( 6.499975723459110455, 22.49103043416547010, -8.090169943749479842 ) ) ;
#23689 = CARTESIAN_POINT ( 'NONE',  ( -11.16403655135938955, 164.3615022471902591, -10.00000000000009592 ) ) ;
#23690 = CARTESIAN_POINT ( 'NONE',  ( 35.19727222974664471, 74.38379681254539832, 59.99999999999999289 ) ) ;
#23691 = CARTESIAN_POINT ( 'NONE',  ( 200.0860664192757952, 270.7206606627561882, -11.57593477606718224 ) ) ;
#23692 = EDGE_CURVE ( 'NONE', #70225, #8187, #26965, .T. ) ;
#23693 = CARTESIAN_POINT ( 'NONE',  ( 28.62558104116610380, 25.03085787977764198, 9.188101187500006262 ) ) ;
#23694 = AXIS2_PLACEMENT_3D ( 'NONE', #31775, #15577, #100219 ) ;
#23695 = CARTESIAN_POINT ( 'NONE',  ( 137.2172943591538967, 238.4824982072973967, 3.021315404115420679E-15 ) ) ;
#23696 = CARTESIAN_POINT ( 'NONE',  ( 149.0203866098534888, 272.5361143586139860, -12.73049804737905255 ) ) ;
#23697 = CARTESIAN_POINT ( 'NONE',  ( 10.75418485208671981, 27.18502408145590010, 5.678558825948277544 ) ) ;
#23698 = CARTESIAN_POINT ( 'NONE',  ( 64.74832919946385346, 214.3149278399160949, -9.188101187500095079 ) ) ;
#23699 = FACE_OUTER_BOUND ( 'NONE', #71889, .T. ) ;
#23700 = CARTESIAN_POINT ( 'NONE',  ( 82.83132155253177586, 53.79349055486937203, -15.41265137785383921 ) ) ;
#23701 = CARTESIAN_POINT ( 'NONE',  ( 159.2511875226268216, 254.8158473755685520, 15.75855490706745599 ) ) ;
#23702 = CARTESIAN_POINT ( 'NONE',  ( 74.05718643579534444, 66.92064597331267350, 12.30401845754858137 ) ) ;
#23703 = CARTESIAN_POINT ( 'NONE',  ( 201.4964414552794949, 281.6449211855650674, 17.70651170561034249 ) ) ;
#23704 = EDGE_CURVE ( 'NONE', #52768, #48577, #26514, .T. ) ;
#23705 = CIRCLE ( 'NONE', #46335, 45.00000000000000000 ) ;
#23706 = CARTESIAN_POINT ( 'NONE',  ( 198.2505066714982149, 285.2670451491296149, 0.000000000000000000 ) ) ;
#23707 = CARTESIAN_POINT ( 'NONE',  ( 110.1516887621107514, 227.7365022471902023, 10.00000000000009592 ) ) ;
#23708 = CARTESIAN_POINT ( 'NONE',  ( 188.0361769804965206, 281.7550819701144746, -17.70093714309158983 ) ) ;
#23709 = CARTESIAN_POINT ( 'NONE',  ( 164.5867587387928950, 245.5743669417666126, -3.022048486790635202 ) ) ;
#23710 = VERTEX_POINT ( 'NONE', #70118 ) ;
#23711 = CARTESIAN_POINT ( 'NONE',  ( 77.08943580307069965, 49.61595851756826647, 15.51385819011977674 ) ) ;
#23712 = CARTESIAN_POINT ( 'NONE',  ( 185.8344414862758640, 272.0246830691658602, 15.77586892895689985 ) ) ;
#23713 = ORIENTED_EDGE ( 'NONE', *, *, #25496, .F. ) ;
#23714 = CARTESIAN_POINT ( 'NONE',  ( 206.4640281786353171, 273.0408085897082060, -10.81921452789957883 ) ) ;
#23715 = CARTESIAN_POINT ( 'NONE',  ( 190.3815443110626404, 278.8296166914984155, -16.52682052525312884 ) ) ;
#23716 = EDGE_CURVE ( 'NONE', #98890, #41308, #74788, .T. ) ;
#23717 = DIRECTION ( 'NONE',  ( 0.4999999999999998890, -0.8660254037844385966, 0.000000000000000000 ) ) ;
#23718 = ORIENTED_EDGE ( 'NONE', *, *, #76046, .F. ) ;
#23719 = CARTESIAN_POINT ( 'NONE',  ( 176.6558404752379090, 252.2237374370411942, -0.2705739152901737166 ) ) ;
#23720 = ORIENTED_EDGE ( 'NONE', *, *, #97626, .T. ) ;
#23721 = CARTESIAN_POINT ( 'NONE',  ( 66.00797677831485544, 69.09111565677241629, -2.045358714672447231 ) ) ;
#23722 = CARTESIAN_POINT ( 'NONE',  ( 147.8163551302855296, 274.6215580551378821, -9.286329195885331345 ) ) ;
#23723 = CARTESIAN_POINT ( 'NONE',  ( 148.5476103079700749, 274.7756356193531246, 7.667830427786927139 ) ) ;
#23724 = ORIENTED_EDGE ( 'NONE', *, *, #25496, .T. ) ;
#23725 = EDGE_CURVE ( 'NONE', #90439, #32720, #21662, .T. ) ;
#23726 = CARTESIAN_POINT ( 'NONE',  ( 31.32709252658613508, 23.80170272979928114, 7.433330006724137462 ) ) ;
#23727 = CARTESIAN_POINT ( 'NONE',  ( 79.96799371511821164, 44.53225917763541020, 11.71816028160813161 ) ) ;
#23728 = DIRECTION ( 'NONE',  ( -0.8098206029991054100, 0.5866775868892259993, 0.000000000000000000 ) ) ;
#23729 = CARTESIAN_POINT ( 'NONE',  ( 75.02238714290075450, 66.92454316053134278, -13.18498694845918884 ) ) ;
#23730 = EDGE_CURVE ( 'NONE', #54490, #83325, #34909, .T. ) ;
#23731 = VERTEX_POINT ( 'NONE', #28463 ) ;
#23732 = CARTESIAN_POINT ( 'NONE',  ( 154.8192283419015212, 273.5986471974344454, 13.52555164010807864 ) ) ;
#23733 = ADVANCED_FACE ( 'NONE', ( #5667 ), #5178, .T. ) ;
#23734 = CARTESIAN_POINT ( 'NONE',  ( -69.94229046795800286, 43.99946344738946635, 10.00000000000000000 ) ) ;
#23735 = ORIENTED_EDGE ( 'NONE', *, *, #44819, .T. ) ;
#23736 = CARTESIAN_POINT ( 'NONE',  ( 174.3933856302132028, 286.8564427156816237, 11.77909119299353691 ) ) ;
#23738 = CARTESIAN_POINT ( 'NONE',  ( 68.16602257681624621, 65.65656189039059143, -10.28278815586033623 ) ) ;
#23737 = CARTESIAN_POINT ( 'NONE',  ( 162.8327449136414771, 284.5743273734687477, -2.483999256947636347 ) ) ;
#23739 = B_SPLINE_CURVE_WITH_KNOTS ( 'NONE', 3,
 ( #37290, #82467, #14002, #14503, #13028, #44881, #75821, #91041, #60574, #76316, #29697, #90555, #52002, #20120, #44386, #75321, #6408, #97151, #91530, #52991, #83940, #6890, #66212, #27717, #58585, #50991, #81941, #12519, #43391, #77813, #92529, #93530, #8396 ),
 .UNSPECIFIED., .F., .F.,
 ( 4, 2, 2, 2, 1, 2, 2, 1, 1, 2, 2, 2, 2, 1, 1, 2, 2, 2, 4 ),
 ( 0.000000000000000000, 0.09685993190008025666, 0.1210749148751011778, 0.1452898978501221128, 0.1937198638001665085, 0.2421498297502108765, 0.2542573212377213232, 0.2663648127252317699, 0.2905797957002522747, 0.3390097616502959488, 0.3874397276003396229, 0.4842996595004269156, 0.5085146424754509731, 0.5327296254504749751, 0.5811595914005229790, 0.6053745743755458708, 0.6295895573505686516, 0.6780195233006141020, 0.7748794552007052250 ),
 .UNSPECIFIED. ) ;
#23740 = CARTESIAN_POINT ( 'NONE',  ( 163.4084407101100851, 247.6152736349200438, -10.68829614238923931 ) ) ;
#23741 = CARTESIAN_POINT ( 'NONE',  ( 204.9427641582406636, 275.6757151647582305, 14.40446820030680897 ) ) ;
#23742 = CARTESIAN_POINT ( 'NONE',  ( -69.42519150082246426, 45.64199051378594874, -10.00000000000000000 ) ) ;
#23743 = CARTESIAN_POINT ( 'NONE',  ( 157.1002372043759010, 258.5414026113353430, -17.73553732786789539 ) ) ;
#23744 = CARTESIAN_POINT ( 'NONE',  ( 130.4037065759891334, 258.3464784336661637, 1.353441290958777525E-15 ) ) ;
#23745 = CARTESIAN_POINT ( 'NONE',  ( 38.34592905085143855, 84.17966526993892273, 59.99999999999999289 ) ) ;
#23746 = CARTESIAN_POINT ( 'NONE',  ( 181.7753553325198368, 260.2882442932133813, 9.488355369979771581 ) ) ;
#23747 = CARTESIAN_POINT ( 'NONE',  ( 74.46396492422927338, 222.9869531367911293, 4.594050593750046652 ) ) ;
#23748 = ORIENTED_EDGE ( 'NONE', *, *, #77498, .T. ) ;
#23749 = CARTESIAN_POINT ( 'NONE',  ( 191.5694344253287511, 298.8390017285333897, 8.250976118904059575 ) ) ;
#23750 = CARTESIAN_POINT ( 'NONE',  ( 77.94354854059760385, 61.39700473696555605, -16.15480247637162847 ) ) ;
#23751 = VECTOR ( 'NONE', #64020, 1000.000000000000000 ) ;
#23752 = EDGE_LOOP ( 'NONE', ( #88368, #82259, #78232, #14028 ) ) ;
#23753 = CARTESIAN_POINT ( 'NONE',  ( 157.3508622362421647, 258.1073073224944778, -17.04076575304558361 ) ) ;
#23754 = AXIS2_PLACEMENT_3D ( 'NONE', #88227, #65363, #57751 ) ;
#23755 = VERTEX_POINT ( 'NONE', #14758 ) ;
#23756 = ORIENTED_EDGE ( 'NONE', *, *, #49860, .F. ) ;
#23757 = ADVANCED_FACE ( 'NONE', ( #30458 ), #20389, .T. ) ;
#23758 = CARTESIAN_POINT ( 'NONE',  ( 66.64069086730589220, 67.52642362728826697, 6.398950582977087187 ) ) ;
#23759 = CARTESIAN_POINT ( 'NONE',  ( 190.9474291326297930, 266.7645650087163745, -12.82661358031884546 ) ) ;
#23761 = B_SPLINE_SURFACE_WITH_KNOTS ( 'NONE', 3, 1, ( 
 ( #48476, #17569 ),
 ( #16066, #79418 ),
 ( #86037, #78893 ),
 ( #70258, #47461 ),
 ( #9479, #39837 ),
 ( #54539, #40350 ),
 ( #71287, #10477 ),
 ( #16565, #9984 ),
 ( #95119, #46968 ),
 ( #2388, #78386 ),
 ( #85522, #31745 ),
 ( #77887, #25684 ),
 ( #32761, #70767 ),
 ( #31259, #63667 ),
 ( #94606, #40843 ),
 ( #56564, #25161 ),
 ( #1383, #62146 ),
 ( #32263, #71790 ),
 ( #48978, #41354 ),
 ( #72296, #23649 ),
 ( #58552, #11499 ),
 ( #57556, #18586 ),
 ( #50955, #89523 ),
 ( #20578, #4882 ),
 ( #88533, #19600 ),
 ( #49973, #19094 ),
 ( #80930, #27179 ),
 ( #26671, #97591 ),
 ( #35764, #65165 ),
 ( #43850, #49465 ),
 ( #57056, #80420 ),
 ( #66169, #33796 ),
 ( #95630, #72807 ),
 ( #58067, #59032 ) ),
 .UNSPECIFIED., .T., .F., .F.,
 ( 4, 2, 2, 2, 2, 2, 2, 2, 2, 2, 2, 2, 2, 2, 2, 2, 4 ),
 ( 2, 2 ),
 ( 0.000000000000000000, 0.06250000000000000000, 0.1250000000000000000, 0.1875000000000000000, 0.2500000000000000000, 0.3125000000000000000, 0.3750000000000000000, 0.4375000000000000000, 0.5000000000000000000, 0.5625000000000000000, 0.6250000000000000000, 0.6875000000000000000, 0.7500000000000000000, 0.8125000000000000000, 0.8750000000000000000, 0.9375000000000000000, 1.000000000000000000 ),
 ( 0.000000000000000000, 1.000000000000000000 ),
 .UNSPECIFIED. ) ;
#23760 = CARTESIAN_POINT ( 'NONE',  ( 191.1687199697037443, 299.5330595250031820, -8.491751560014430211 ) ) ;
#23762 = CARTESIAN_POINT ( 'NONE',  ( 81.27629932712225980, 55.76935796986149541, 16.38776540150240990 ) ) ;
#23763 = CARTESIAN_POINT ( 'NONE',  ( 85.51568253422234989, 47.12103425145187430, -10.62146421753836201 ) ) ;
#23764 = CARTESIAN_POINT ( 'NONE',  ( 80.66154599400290692, 223.5024278399160949, -9.188101187500093303 ) ) ;
#23765 = EDGE_LOOP ( 'NONE', ( #97777, #89302, #86612, #95111 ) ) ;
#23766 = EDGE_CURVE ( 'NONE', #46169, #1959, #38036, .T. ) ;
#23767 = CIRCLE ( 'NONE', #36717, 60.00000000000001421 ) ;
#23768 = ORIENTED_EDGE ( 'NONE', *, *, #55653, .F. ) ;
#23769 = CARTESIAN_POINT ( 'NONE',  ( 21.79139015901366250, 20.78052372038640527, -10.00000000000000355 ) ) ;
#23770 = AXIS2_PLACEMENT_3D ( 'NONE', #58577, #59061, #28187 ) ;
#23771 = CARTESIAN_POINT ( 'NONE',  ( 162.0504616076140678, 249.9673624360595454, -13.49018830579758266 ) ) ;
#23772 = ORIENTED_EDGE ( 'NONE', *, *, #19558, .F. ) ;
#23773 = CARTESIAN_POINT ( 'NONE',  ( 88.06269261788008862, 43.61796610520790551, 0.05835779599787207367 ) ) ;
#23774 = EDGE_CURVE ( 'NONE', #11960, #25891, #53045, .T. ) ;
#23775 = B_SPLINE_CURVE_WITH_KNOTS ( 'NONE', 3,
 ( #77035, #7641, #25863, #81958, #56230, #2055, #26353, #32448, #66710, #86203 ),
 .UNSPECIFIED., .F., .F.,
 ( 4, 2, 2, 2, 4 ),
 ( 0.000000000000000000, 0.2500000000000000000, 0.5000000000000000000, 0.7500000000000000000, 1.000000000000000000 ),
 .UNSPECIFIED. ) ;
#23776 = CARTESIAN_POINT ( 'NONE',  ( 76.27001746108665259, 64.92218695046919663, -14.30664744964449753 ) ) ;
#23777 = CARTESIAN_POINT ( 'NONE',  ( 206.5280879940269756, 272.9298537347264642, 11.21709153681466731 ) ) ;
#23778 = EDGE_CURVE ( 'NONE', #14203, #15032, #29183, .T. ) ;
#23779 = CARTESIAN_POINT ( 'NONE',  ( -31.34720201560244845, 93.26289111443594493, 44.07321716645989085 ) ) ;
#23780 = CARTESIAN_POINT ( 'NONE',  ( 147.1270795744234476, 264.4111747905818675, -1.822351119449947324E-15 ) ) ;
#23781 = CARTESIAN_POINT ( 'NONE',  ( -70.00000000000000000, 15.00000000000000000, 59.99999999999999289 ) ) ;
#23782 = ORIENTED_EDGE ( 'NONE', *, *, #2012, .F. ) ;
#23783 = VECTOR ( 'NONE', #31728, 1000.000000000000000 ) ;
#23784 = CARTESIAN_POINT ( 'NONE',  ( 188.6651695142899143, 294.9748060149505591, 11.65985380162412710 ) ) ;
#23785 = ADVANCED_FACE ( 'NONE', ( #23252 ), #45563, .F. ) ;
#23786 = CARTESIAN_POINT ( 'NONE',  ( 34.73240388683179702, 38.79103043416552765, 8.090169943749478065 ) ) ;
#23787 = CARTESIAN_POINT ( 'NONE',  ( 196.6610909444931679, 276.7880959174222539, 16.58182079090270733 ) ) ;
#23788 = CARTESIAN_POINT ( 'NONE',  ( 201.0844796915553161, 282.3584598911111812, -16.59562674965125950 ) ) ;
#23789 = CARTESIAN_POINT ( 'NONE',  ( 102.4195449475128470, 241.4860189848785126, -2.679491924311252493 ) ) ;
#23790 = CARTESIAN_POINT ( 'NONE',  ( 70.49967271327585649, 67.34638213932271356, -9.999908609504970514 ) ) ;
#23791 = ORIENTED_EDGE ( 'NONE', *, *, #70279, .F. ) ;
#23792 = CARTESIAN_POINT ( 'NONE',  ( -22.42236680055709641, 157.8615022471902591, 0.000000000000000000 ) ) ;
#23793 = DIRECTION ( 'NONE',  ( 1.000000000000000000, 8.921435019309292501E-15, 0.000000000000000000 ) ) ;
#23794 = CARTESIAN_POINT ( 'NONE',  ( 27.87927540258908365, 180.2365022471902023, -10.00000000000009237 ) ) ;
#23795 = CARTESIAN_POINT ( 'NONE',  ( 58.97569090598253183, 178.8759306620404175, -18.47570218321542868 ) ) ;
#23796 = CARTESIAN_POINT ( 'NONE',  ( 83.58408646423136190, 52.36411970034374974, 14.77742527876824141 ) ) ;
#23797 = CARTESIAN_POINT ( 'NONE',  ( 153.4175160819171708, 270.2815289807249997, 14.02256376582253061 ) ) ;
#23798 = ORIENTED_EDGE ( 'NONE', *, *, #41862, .T. ) ;
#23799 = CARTESIAN_POINT ( 'NONE',  ( 202.2712651538608668, 280.3028871727136675, 16.13191389836473988 ) ) ;
#23800 = DIRECTION ( 'NONE',  ( 0.000000000000000000, 0.000000000000000000, -1.000000000000000000 ) ) ;
#23802 = FACE_BOUND ( 'NONE', #91325, .T. ) ;
#23801 = CARTESIAN_POINT ( 'NONE',  ( 155.1376601545389917, 261.9406857754215707, 18.55063430030667959 ) ) ;
#23803 = CARTESIAN_POINT ( 'NONE',  ( 178.6256486530057259, 287.8356261986529034, -12.96677738169596061 ) ) ;
#23804 = B_SPLINE_CURVE_WITH_KNOTS ( 'NONE', 3,
 ( #41356, #97117, #72809, #57559 ),
 .UNSPECIFIED., .F., .F.,
 ( 4, 4 ),
 ( 0.009127121522214379570, 0.01427955626753199883 ),
 .UNSPECIFIED. ) ;
#23805 = CARTESIAN_POINT ( 'NONE',  ( 26.65225264301594166, 37.16126292948896293, -6.180339887498951690 ) ) ;
#23806 = CARTESIAN_POINT ( 'NONE',  ( 171.6010233849675330, 274.8379305346047659, 17.12104339205637871 ) ) ;
#23807 = CARTESIAN_POINT ( 'NONE',  ( 166.3787229958576859, 286.5602776898857087, -3.288044247041284507 ) ) ;
#23808 = CARTESIAN_POINT ( 'NONE',  ( 47.83996289752661113, 111.6306699247848826, 177.5919119679930134 ) ) ;
#23809 = CARTESIAN_POINT ( 'NONE',  ( 192.1608772079249263, 261.8654286030369462, 3.048632953649568655 ) ) ;
#23810 = CARTESIAN_POINT ( 'NONE',  ( 187.9196281127333918, 297.0021197407985483, -9.095446553628486086 ) ) ;
#23811 = CARTESIAN_POINT ( 'NONE',  ( 4.207654042216683266, 182.4244531367911293, -4.594050593750046652 ) ) ;
#23812 = CARTESIAN_POINT ( 'NONE',  ( -2.330697855141256269, 26.52822386297705393, 10.00000000000000000 ) ) ;
#23813 = ORIENTED_EDGE ( 'NONE', *, *, #75108, .F. ) ;
#23814 = CARTESIAN_POINT ( 'NONE',  ( 174.8837099083871180, 255.2975024955725303, 8.373857793136043171 ) ) ;
#23815 = CARTESIAN_POINT ( 'NONE',  ( -18.45562326176555956, 23.07528527759725989, -10.00000000000000000 ) ) ;
#23816 = CARTESIAN_POINT ( 'NONE',  ( 25.10051690851626560, 194.4869531367911293, 4.594050593750046652 ) ) ;
#23817 = CIRCLE ( 'NONE', #72394, 5.000000000000023981 ) ;
#23818 = CARTESIAN_POINT ( 'NONE',  ( 69.44849478424214340, 204.2365022471902023, -10.00000000000009237 ) ) ;
#23819 = CARTESIAN_POINT ( 'NONE',  ( 26.40327033588000205, 37.01751292744058475, 6.180339887498949913 ) ) ;
#23820 = CARTESIAN_POINT ( 'NONE',  ( 78.25846697678839803, 59.65309229871257202, 16.47561015943145435 ) ) ;
#23821 = CARTESIAN_POINT ( 'NONE',  ( 191.2111338740054975, 299.4595964878050154, -9.718193530796334301 ) ) ;
#23822 = CARTESIAN_POINT ( 'NONE',  ( 5.154066788520982101, 185.3297689869269504, -2.679491924311252493 ) ) ;
#23823 = CARTESIAN_POINT ( 'NONE',  ( 189.9097473895767507, 298.3003973193997354, -7.968993835093706402 ) ) ;
#23824 = LINE ( 'NONE', #86198, #29058 ) ;
#23825 = VECTOR ( 'NONE', #59776, 1000.000000000000341 ) ;
#23827 =( BOUNDED_CURVE ( )  B_SPLINE_CURVE ( 2, ( #90174, #34920, #20244, #12652, #51119, #50616, #65816, #19268, #72964 ),
 .UNSPECIFIED., .F., .T. ) 
 B_SPLINE_CURVE_WITH_KNOTS ( ( 3, 2, 2, 2, 3 ),
 ( 0.6250000000000000000, 0.6263440860215053752, 0.6290322580645161255, 0.6317204301075268758, 0.6330645161290322509 ),
 .UNSPECIFIED. ) 
 CURVE ( )  GEOMETRIC_REPRESENTATION_ITEM ( )  RATIONAL_B_SPLINE_CURVE ( ( 0.9330127018922194093, 0.9330127018922194093, 1.000000000000000000, 0.8660254037844387076, 1.000000000000000000, 0.8660254037844387076, 1.000000000000000000, 0.9330127018922194093, 0.9330127018922194093 ) ) 
 REPRESENTATION_ITEM ( '' )  );
#23826 = CARTESIAN_POINT ( 'NONE',  ( 73.77862180316432728, 206.7365022471902023, 10.00000000000009592 ) ) ;
#23828 = CARTESIAN_POINT ( 'NONE',  ( 5.871984111234073822, 29.22396284167520619, 10.00000000000000000 ) ) ;
#23829 = CARTESIAN_POINT ( 'NONE',  ( 175.4967466201937611, 291.2628096033125189, 6.560984766252938805 ) ) ;
#23830 = CARTESIAN_POINT ( 'NONE',  ( 31.32559514186443295, 179.7048013555409796, 4.594050593750051981 ) ) ;
#23831 = CARTESIAN_POINT ( 'NONE',  ( 72.69903869004953378, 70.24355232890721368, -8.744048261473219341 ) ) ;
#23832 = CARTESIAN_POINT ( 'NONE',  ( 27.81076257310190769, 39.55466486950702176, 7.012934429366973338E-14 ) ) ;
#23833 = CARTESIAN_POINT ( 'NONE',  ( 203.0120883329668970, 270.0550711529738237, -6.419258576597377974 ) ) ;
#23834 = CARTESIAN_POINT ( 'NONE',  ( 151.4188942279983223, 268.3817773016460251, -14.77302265413830895 ) ) ;
#23835 = EDGE_CURVE ( 'NONE', #23520, #68063, #72392, .T. ) ;
#23836 = LINE ( 'NONE', #55225, #12721 ) ;
#23837 = CARTESIAN_POINT ( 'NONE',  ( -48.34856483818852979, 28.93234566034054822, -10.00000000000000000 ) ) ;
#23838 = CARTESIAN_POINT ( 'NONE',  ( 159.8915935406342612, 278.4112977589962838, -10.47619785574662998 ) ) ;
#23839 = CARTESIAN_POINT ( 'NONE',  ( 205.8099205723994203, 269.1131406545866298, -1.356034389334280776 ) ) ;
#23840 = CARTESIAN_POINT ( 'NONE',  ( 21.52536902826200915, 24.37878583063841376, 9.188101187500006262 ) ) ;
#23841 = DIRECTION ( 'NONE',  ( 0.000000000000000000, 0.000000000000000000, 1.000000000000000000 ) ) ;
#23842 = CARTESIAN_POINT ( 'NONE',  ( 174.5885488454506174, 256.4458599265808516, 12.05082362884263425 ) ) ;
#23843 = VERTEX_POINT ( 'NONE', #88132 ) ;
#23844 = CARTESIAN_POINT ( 'NONE',  ( 6.244247187202517146, 25.64646525600388216, -2.839279412974133887 ) ) ;
#23845 = B_SPLINE_CURVE_WITH_KNOTS ( 'NONE', 3,
 ( #4214, #57915, #43195, #95973 ),
 .UNSPECIFIED., .F., .F.,
 ( 4, 4 ),
 ( 0.009376484201431983107, 0.01501325678996159353 ),
 .UNSPECIFIED. ) ;
#23846 = B_SPLINE_CURVE_WITH_KNOTS ( 'NONE', 3,
 ( #92207, #13667, #91194, #44540 ),
 .UNSPECIFIED., .F., .F.,
 ( 4, 4 ),
 ( 0.01730275677769292988, 0.02623041320600179305 ),
 .UNSPECIFIED. ) ;
#23847 = CARTESIAN_POINT ( 'NONE',  ( 75.31289280903088468, 53.62176160569084260, -16.53289957306499858 ) ) ;
#23848 = CARTESIAN_POINT ( 'NONE',  ( 71.22567098774472072, 60.39832601874510942, -14.84358665764284524 ) ) ;
#23849 = CARTESIAN_POINT ( 'NONE',  ( -2.305318362029009638, 176.1427522451419350, -10.00000000000009592 ) ) ;
#23850 = EDGE_CURVE ( 'NONE', #11388, #62487, #84490, .T. ) ;
#23851 = ORIENTED_EDGE ( 'NONE', *, *, #23012, .T. ) ;
#23852 = CARTESIAN_POINT ( 'NONE',  ( 186.7554075434758545, 282.3000898601083577, 17.53539547572453827 ) ) ;
#23853 = LINE ( 'NONE', #46657, #38446 ) ;
#23854 = CARTESIAN_POINT ( 'NONE',  ( 85.62087432442550039, 48.96184342359305219, 12.19155329030992618 ) ) ;
#23855 = EDGE_CURVE ( 'NONE', #61495, #11375, #26769, .T. ) ;
#23856 = CARTESIAN_POINT ( 'NONE',  ( -51.48155258352917230, 83.50091703386740960, -10.00000000000000000 ) ) ;
#23857 = ORIENTED_EDGE ( 'NONE', *, *, #19286, .F. ) ;
#23858 = ORIENTED_EDGE ( 'NONE', *, *, #50367, .T. ) ;
#23859 = VECTOR ( 'NONE', #57361, 1000.000000000000227 ) ;
#23861 = CARTESIAN_POINT ( 'NONE',  ( 84.33518316974296170, 42.63392823952606392, -4.290652948369976905 ) ) ;
#23860 = CARTESIAN_POINT ( 'NONE',  ( 68.78996647874213011, 70.77593301599395659, 1.606320726995938530 ) ) ;
#23862 = ORIENTED_EDGE ( 'NONE', *, *, #59293, .F. ) ;
#23863 = CARTESIAN_POINT ( 'NONE',  ( 201.4617167010348737, 281.7050662241970826, -17.43131506460443703 ) ) ;
#23864 = CARTESIAN_POINT ( 'NONE',  ( 71.87942950353104266, 72.15877716270880171, -3.647418342425857052 ) ) ;
#23865 = CARTESIAN_POINT ( 'NONE',  ( 72.76771589847461996, 57.00350618467320629, -16.39718444356080695 ) ) ;
#23866 = CARTESIAN_POINT ( 'NONE',  ( 76.65872121159138430, 63.56238613867309795, 15.33801735844474834 ) ) ;
#23867 = CARTESIAN_POINT ( 'NONE',  ( 190.4750160083620472, 300.7345900314585947, -1.159659205620361400 ) ) ;
#23868 = CARTESIAN_POINT ( 'NONE',  ( 201.9133243980324153, 266.9637997000594396, 2.242576533087043966 ) ) ;
#23869 = ORIENTED_EDGE ( 'NONE', *, *, #71711, .F. ) ;
#23870 = LINE ( 'NONE', #39553, #25598 ) ;
#23871 = CARTESIAN_POINT ( 'NONE',  ( 162.1260167985288376, 266.6785162637209510, 17.71249957499354366 ) ) ;
#23872 = EDGE_LOOP ( 'NONE', ( #31116, #87243, #82229 ) ) ;
#23873 = CARTESIAN_POINT ( 'NONE',  ( 29.59504171901726366, 22.80170272979927759, 7.433330006724137462 ) ) ;
#23874 = CARTESIAN_POINT ( 'NONE',  ( 157.6466783816650832, 259.5949387289228412, 17.71616314254395519 ) ) ;
#23875 = PLANE ( 'NONE',  #15866 ) ;
#23876 = ORIENTED_EDGE ( 'NONE', *, *, #91364, .F. ) ;
#23877 = DIRECTION ( 'NONE',  ( -0.7300871660154544251, -0.6833540297821638632, 0.000000000000000000 ) ) ;
#23878 = CARTESIAN_POINT ( 'NONE',  ( 26.66754231763712824, 34.13478043621389446, 8.090169943749478065 ) ) ;
#23879 = CARTESIAN_POINT ( 'NONE',  ( 97.35977185683022128, 217.0177522451417929, 5.000000000000051514 ) ) ;
#23880 = CARTESIAN_POINT ( 'NONE',  ( 83.82827945288542537, 51.88092520783234818, 14.50189114860043205 ) ) ;
#23881 = ORIENTED_EDGE ( 'NONE', *, *, #69149, .T. ) ;
#23882 = EDGE_LOOP ( 'NONE', ( #61354, #502, #52545, #5231 ) ) ;
#23883 = ADVANCED_FACE ( 'NONE', ( #97202 ), #3965, .F. ) ;
#23884 = CARTESIAN_POINT ( 'NONE',  ( 190.9492596519850451, 299.5322795678457624, 5.766969289918903563 ) ) ;
#23885 = CARTESIAN_POINT ( 'NONE',  ( 146.8000281410530192, 276.3818880375922049, 4.652863924796177386 ) ) ;
#23886 = CARTESIAN_POINT ( 'NONE',  ( 148.3837145175834280, 273.6388627701866767, 8.841971351370922605 ) ) ;
#23887 = VECTOR ( 'NONE', #98622, 1000.000000000000114 ) ;
#23888 = ORIENTED_EDGE ( 'NONE', *, *, #23271, .F. ) ;
#23889 = CARTESIAN_POINT ( 'NONE',  ( 149.7162292714551199, 271.3308795146458010, 12.12826134257344357 ) ) ;
#23890 = CARTESIAN_POINT ( 'NONE',  ( 157.2720021843916243, 259.7600564740663458, -17.50627268554094940 ) ) ;
#23891 = PLANE ( 'NONE',  #28908 ) ;
#23892 = CARTESIAN_POINT ( 'NONE',  ( 192.4172326059820648, 297.3705722050773943, -12.52563289807247848 ) ) ;
#23893 = ADVANCED_FACE ( 'NONE', ( #19195 ), #66267, .T. ) ;
#23894 = CARTESIAN_POINT ( 'NONE',  ( 148.9694607950094394, 272.6243204573405592, 11.81236034532910573 ) ) ;
#23895 = AXIS2_PLACEMENT_3D ( 'NONE', #23296, #62286, #46592 ) ;
#23896 = DIRECTION ( 'NONE',  ( -0.8660254037844385966, -0.4999999999999999445, 0.000000000000000000 ) ) ;
#23897 = CARTESIAN_POINT ( 'NONE',  ( 164.8537203408104972, 245.1119758834023230, 2.926011033004258355 ) ) ;
#23898 = DIRECTION ( 'NONE',  ( -0.5000000000000001110, 0.8660254037844384856, 2.775557561562890427E-17 ) ) ;
#23899 = CARTESIAN_POINT ( 'NONE',  ( 69.39138836530793242, 65.59840692806227480, -11.05004714553397704 ) ) ;
#23900 = CARTESIAN_POINT ( 'NONE',  ( 78.75297625648194355, 47.66336229242892131, 14.29739783554173727 ) ) ;
#23901 = CARTESIAN_POINT ( 'NONE',  ( 116.8724067376222706, 238.2833772461660544, -9.188101187500095079 ) ) ;
#23902 = VERTEX_POINT ( 'NONE', #89617 ) ;
#23903 = CARTESIAN_POINT ( 'NONE',  ( 147.2937583206075942, 275.5267222813735088, 0.1877253132609109920 ) ) ;
#23904 = CARTESIAN_POINT ( 'NONE',  ( 70.04767293653641502, 64.67844632371958369, 12.15646808155997860 ) ) ;
#23905 = EDGE_CURVE ( 'NONE', #41771, #55869, #20178, .T. ) ;
#23906 = CARTESIAN_POINT ( 'NONE',  ( 87.43197870664040749, 44.84778077074484770, -6.629285647492168643 ) ) ;
#23907 = EDGE_CURVE ( 'NONE', #13902, #96030, #50526, .T. ) ;
#23908 = CARTESIAN_POINT ( 'NONE',  ( 203.4682009197399566, 278.2297336128146412, -15.36039508894693206 ) ) ;
#23909 = CARTESIAN_POINT ( 'NONE',  ( 204.8523313866422484, 275.8323493198358847, 14.65426965484541100 ) ) ;
#23910 = CARTESIAN_POINT ( 'NONE',  ( 83.51092623577891061, 51.50185674319119045, -14.43088262691037293 ) ) ;
#23911 = CARTESIAN_POINT ( 'NONE',  ( 87.53583079710631409, 45.45925790797146249, -6.823327534849023657 ) ) ;
#23912 = VERTEX_POINT ( 'NONE', #80007 ) ;
#23913 = CARTESIAN_POINT ( 'NONE',  ( 207.6555576926778883, 270.9770189326688410, -1.235081510489080436 ) ) ;
#23914 = VECTOR ( 'NONE', #49644, 1000.000000000000000 ) ;
#23915 = DIRECTION ( 'NONE',  ( 0.5000000000000013323, -0.8660254037844378194, 0.000000000000000000 ) ) ;
#23916 = CARTESIAN_POINT ( 'NONE',  ( 74.65263117529048031, 66.98225998262294922, 13.00178404275292721 ) ) ;
#23917 = CARTESIAN_POINT ( 'NONE',  ( 127.4544149619371609, 235.2048013555409796, 4.594050593750051981 ) ) ;
#23918 = CARTESIAN_POINT ( 'NONE',  ( 150.6815632051821581, 269.6588720951601772, -14.68790257316217307 ) ) ;
#23919 = CARTESIAN_POINT ( 'NONE',  ( 185.8154782850418769, 296.8462876573850053, 4.389817180861387058 ) ) ;
#23920 = CARTESIAN_POINT ( 'NONE',  ( 157.3025066944120454, 258.1910615777721887, 18.21299529665260053 ) ) ;
#23921 = FACE_OUTER_BOUND ( 'NONE', #33378, .T. ) ;
#23922 = CARTESIAN_POINT ( 'NONE',  ( 51.75794814269728050, 206.8149278399160949, -9.188101187500095079 ) ) ;
#23923 = CARTESIAN_POINT ( 'NONE',  ( 85.48848937474792820, 48.32878387211594884, -12.22513733614604270 ) ) ;
#23924 = ORIENTED_EDGE ( 'NONE', *, *, #47540, .F. ) ;
#23925 = CARTESIAN_POINT ( 'NONE',  ( 72.31093312958903141, 67.42550271943373730, 11.03266209124485897 ) ) ;
#23926 = CARTESIAN_POINT ( 'NONE',  ( 27.58098951138967436, 43.10352854649765675, -10.00000000000000000 ) ) ;
#23927 = CARTESIAN_POINT ( 'NONE',  ( 72.73869357531808078, 58.37704337636537133, 16.17108310384250203 ) ) ;
#23928 = CARTESIAN_POINT ( 'NONE',  ( 175.0126904547745994, 261.3741942827071512, 14.53273751430707428 ) ) ;
#23929 = CARTESIAN_POINT ( 'NONE',  ( 82.29666020798650550, 41.51490518991582945, -5.842944381793243380 ) ) ;
#23930 = CARTESIAN_POINT ( 'NONE',  ( 202.8535267948003593, 279.2943804273081696, -15.36804658072946062 ) ) ;
#23931 = CARTESIAN_POINT ( 'NONE',  ( 153.6154705056581520, 269.2265720717915087, -15.53643265229117887 ) ) ;
#23932 =( GEOMETRIC_REPRESENTATION_CONTEXT ( 3 ) GLOBAL_UNCERTAINTY_ASSIGNED_CONTEXT ( ( #64563 ) ) GLOBAL_UNIT_ASSIGNED_CONTEXT ( ( #13615, #67806, #83544 ) ) REPRESENTATION_CONTEXT ( 'NONE', 'WORKASPACE' ) );
#23933 = CARTESIAN_POINT ( 'NONE',  ( 112.0100349375169912, 222.1427522451417644, 1.119607411625061291E-15 ) ) ;
#23934 = CARTESIAN_POINT ( 'NONE',  ( 171.1380476607806429, 267.8866146403163384, -17.76239963503928010 ) ) ;
#23935 = EDGE_LOOP ( 'NONE', ( #13557, #26546, #36423, #46437 ) ) ;
#23936 = EDGE_CURVE ( 'NONE', #6163, #47559, #49559, .T. ) ;
#23937 = CARTESIAN_POINT ( 'NONE',  ( 202.4323889586180201, 280.0238125565655878, 15.69595176008160919 ) ) ;
#23938 = FACE_OUTER_BOUND ( 'NONE', #43572, .T. ) ;
#23939 = CARTESIAN_POINT ( 'NONE',  ( 24.64070123457955219, 185.0333772461660544, 9.188101187500095079 ) ) ;
#23940 = CARTESIAN_POINT ( 'NONE',  ( 11.86377311551791358, 18.80066082961420548, 10.00000000000000533 ) ) ;
#23941 = DIRECTION ( 'NONE',  ( 0.2033683215378999376, -0.3522442655536480172, -0.9135454576426004225 ) ) ;
#23942 = CARTESIAN_POINT ( 'NONE',  ( 71.88281838924127953, 59.56282477450883306, -15.74156321312328011 ) ) ;
#23943 = LINE ( 'NONE', #71073, #73374 ) ;
#23945 = CARTESIAN_POINT ( 'NONE',  ( 71.40607303893924040, 212.0333772461660544, 9.188101187500095079 ) ) ;
#23944 = CARTESIAN_POINT ( 'NONE',  ( 10.37514450368026786, 11.15404122711131407, 8.090169943749479842 ) ) ;
#23946 = CARTESIAN_POINT ( 'NONE',  ( 200.2690241097007799, 283.7708703901988656, 16.96680019208369927 ) ) ;
#23947 = CARTESIAN_POINT ( 'NONE',  ( 174.3922364351138867, 288.8364454784203872, 7.670429905402864179 ) ) ;
#23948 = CARTESIAN_POINT ( 'NONE',  ( 183.9122833166825615, 256.5348419210068300, 1.420446916831177298 ) ) ;
#23949 = CARTESIAN_POINT ( 'NONE',  ( 70.47412699110996925, 67.85741242599571876, 10.12516759932945476 ) ) ;
#23950 = CARTESIAN_POINT ( 'NONE',  ( 14.86318692873816083, 16.78052372038639106, -10.00000000000000355 ) ) ;
#23951 = ORIENTED_EDGE ( 'NONE', *, *, #410, .F. ) ;
#23952 = CARTESIAN_POINT ( 'NONE',  ( 27.80710661894035596, 186.8615022471902591, -10.00000000000009592 ) ) ;
#23953 = DIRECTION ( 'NONE',  ( -0.8599083858334093389, 0.5104483989331149996, 0.000000000000000000 ) ) ;
#23954 = CARTESIAN_POINT ( 'NONE',  ( 202.7041331321765938, 279.5531378413010657, 17.14708438049711248 ) ) ;
#23955 = AXIS2_PLACEMENT_3D ( 'NONE', #36270, #42364, #27697 ) ;
#23956 = CARTESIAN_POINT ( 'NONE',  ( -5.561934722402757991, 167.5958772461660544, -9.188101187500095079 ) ) ;
#23957 = CARTESIAN_POINT ( 'NONE',  ( 35.22599450741489591, 22.19860640527294393, 2.839279412974134775 ) ) ;
#23959 = CARTESIAN_POINT ( 'NONE',  ( 170.6150151926208309, 263.3591274673946145, 15.81415637510684391 ) ) ;
#23958 = CARTESIAN_POINT ( 'NONE',  ( 167.7533332108949935, 262.4447794098586542, -16.91708224468162314 ) ) ;
#23960 = CARTESIAN_POINT ( 'NONE',  ( 185.5793223466652364, 259.8320106733570469, 7.401475797627644404 ) ) ;
#23961 = CARTESIAN_POINT ( 'NONE',  ( 164.3022921857394749, 246.0670774647090582, 1.862798784958315856 ) ) ;
#23962 = EDGE_CURVE ( 'NONE', #89739, #93198, #72899, .T. ) ;
#23963 = CARTESIAN_POINT ( 'NONE',  ( 88.01292981757310940, 43.79437901572623559, 2.423352920943459665 ) ) ;
#23964 = CARTESIAN_POINT ( 'NONE',  ( 66.37106933066878867, 68.69559461379999732, 2.357535188532553505 ) ) ;
#23965 = ORIENTED_EDGE ( 'NONE', *, *, #65141, .F. ) ;
#23966 = B_SPLINE_CURVE_WITH_KNOTS ( 'NONE', 3,
 ( #69119, #70618, #100046, #1746 ),
 .UNSPECIFIED., .F., .F.,
 ( 4, 4 ),
 ( 0.002746326142393483178, 0.008136428815393210653 ),
 .UNSPECIFIED. ) ;
#23967 = LINE ( 'NONE', #1696, #84401 ) ;
#23968 = AXIS2_PLACEMENT_3D ( 'NONE', #5736, #98461, #29540 ) ;
#23969 = CARTESIAN_POINT ( 'NONE',  ( 178.3755071135885260, 285.5767383373634516, 12.93467627631818040 ) ) ;
#23970 = CARTESIAN_POINT ( 'NONE',  ( 196.7042903992237086, 289.4290128693130555, 16.50876271461077849 ) ) ;
#23971 = CARTESIAN_POINT ( 'NONE',  ( 15.97197434310064423, 12.14754757982088940, -5.678558825948275768 ) ) ;
#23972 = VERTEX_POINT ( 'NONE', #34847 ) ;
#23973 = CARTESIAN_POINT ( 'NONE',  ( 206.7416841040605391, 272.5598944198493427, 8.000062685979553834 ) ) ;
#23974 = CARTESIAN_POINT ( 'NONE',  ( 157.6921299354026189, 257.5162143285667753, -18.18720974599499840 ) ) ;
#23975 = DIRECTION ( 'NONE',  ( -0.8660254037844387076, -0.4999999999999998890, -0.000000000000000000 ) ) ;
#23976 = EDGE_CURVE ( 'NONE', #77213, #45554, #96704, .T. ) ;
#23977 = CARTESIAN_POINT ( 'NONE',  ( 23.75126848931443746, 37.21091486745861943, 7.012934429366973338E-14 ) ) ;
#23978 = DIRECTION ( 'NONE',  ( -0.9182972510888884887, 0.3958915996110436430, 0.000000000000000000 ) ) ;
#23979 = DIRECTION ( 'NONE',  ( -1.000000000000000000, 0.000000000000000000, 0.000000000000000000 ) ) ;
#23980 = ADVANCED_FACE ( 'NONE', ( #89136 ), #50549, .T. ) ;
#23981 = CARTESIAN_POINT ( 'NONE',  ( 162.6396274730868186, 248.9468972229755082, -10.26162218571527518 ) ) ;
#23982 = CARTESIAN_POINT ( 'NONE',  ( 152.8328714238065515, 265.9326969577624027, -16.29536156676786263 ) ) ;
#23983 = ORIENTED_EDGE ( 'NONE', *, *, #3580, .F. ) ;
#23984 = ORIENTED_EDGE ( 'NONE', *, *, #24872, .T. ) ;
#23985 = CARTESIAN_POINT ( 'NONE',  ( 138.6787122315880083, 239.3262482093457493, 3.021315404115420679E-15 ) ) ;
#23986 = CARTESIAN_POINT ( 'NONE',  ( 164.1412601152769639, 248.5329951649505063, 9.989603322558886944 ) ) ;
#23987 = VERTEX_POINT ( 'NONE', #4976 ) ;
#23988 = CARTESIAN_POINT ( 'NONE',  ( 26.59681983377653580, 15.75978393459164728, -1.583844403245362020 ) ) ;
#23989 = DIRECTION ( 'NONE',  ( 0.000000000000000000, 0.000000000000000000, 1.000000000000000000 ) ) ;
#23990 = ORIENTED_EDGE ( 'NONE', *, *, #66881, .T. ) ;
#23991 = CARTESIAN_POINT ( 'NONE',  ( 68.83006821756048055, 63.80255091578027304, -12.25988136761327496 ) ) ;
#23992 = CARTESIAN_POINT ( 'NONE',  ( 79.30872066878571047, 59.07782615681725957, -16.22658500882148758 ) ) ;
#23993 = CIRCLE ( 'NONE', #66022, 70.00000000000001421 ) ;
#23994 = CARTESIAN_POINT ( 'NONE',  ( 196.9431415128477170, 289.5314680279574304, -16.61413060656005669 ) ) ;
#23995 = CARTESIAN_POINT ( 'NONE',  ( 69.68564319292937626, 62.66806819657130490, 13.90549188088030164 ) ) ;
#23996 = VERTEX_POINT ( 'NONE', #67251 ) ;
#23997 = CARTESIAN_POINT ( 'NONE',  ( 161.4726291907278721, 250.9681975403669867, 14.52346149734912117 ) ) ;
#23998 = CARTESIAN_POINT ( 'NONE',  ( 150.8167050463783312, 269.4247995599803289, 14.38040671671637938 ) ) ;
#23999 = CARTESIAN_POINT ( 'NONE',  ( 71.41016749218992743, 59.45273978182970609, 15.69346469599747174 ) ) ;
#24000 = B_SPLINE_SURFACE_WITH_KNOTS ( 'NONE', 3, 1, ( 
 ( #14065, #75891 ),
 ( #90106, #82526 ),
 ( #60141, #35364 ),
 ( #96713, #91103 ),
 ( #97692, #36355 ),
 ( #43949, #27280 ),
 ( #58162, #59135 ),
 ( #36859, #21669 ),
 ( #58650, #89624 ),
 ( #52063, #52549 ),
 ( #67768, #20185 ),
 ( #83501, #19694 ),
 ( #74888, #44449 ),
 ( #83006, #5471 ),
 ( #28261, #51052 ),
 ( #34854, #65758 ),
 ( #66763, #73878 ),
 ( #81510, #4471 ),
 ( #42939, #4984 ),
 ( #82012, #66274 ),
 ( #67260, #13578 ),
 ( #35863, #98185 ),
 ( #12587, #28767 ),
 ( #59649, #43458 ),
 ( #90620, #21184 ),
 ( #75382, #98691 ),
 ( #29273, #8456 ),
 ( #22161, #69746 ),
 ( #46433, #54525 ),
 ( #38840, #31730 ),
 ( #85506, #45447 ),
 ( #30257, #61644 ),
 ( #6470, #84499 ),
 ( #77871, #77362 ) ),
 .UNSPECIFIED., .T., .F., .F.,
 ( 4, 2, 2, 2, 2, 2, 2, 2, 2, 2, 2, 2, 2, 2, 2, 2, 4 ),
 ( 2, 2 ),
 ( 0.000000000000000000, 0.06250000000000000000, 0.1250000000000000000, 0.1875000000000000000, 0.2500000000000000000, 0.3125000000000000000, 0.3750000000000000000, 0.4375000000000000000, 0.5000000000000000000, 0.5625000000000000000, 0.6250000000000000000, 0.6875000000000000000, 0.7500000000000000000, 0.8125000000000000000, 0.8750000000000000000, 0.9375000000000000000, 1.000000000000000000 ),
 ( 0.000000000000000000, 1.000000000000000000 ),
 .UNSPECIFIED. ) ;
#24001 = VERTEX_POINT ( 'NONE', #91094 ) ;
#24002 = ORIENTED_EDGE ( 'NONE', *, *, #49069, .T. ) ;
#24003 = B_SPLINE_CURVE_WITH_KNOTS ( 'NONE', 3,
 ( #85867, #18414, #77718, #32082, #48812, #2216, #47285, #33097, #8796, #94935 ),
 .UNSPECIFIED., .F., .F.,
 ( 4, 2, 2, 2, 4 ),
 ( 0.001476764202228747404, 0.001775028363004824659, 0.002073292523780901914, 0.002371556684556979169, 0.002669820845333056424 ),
 .UNSPECIFIED. ) ;
#24004 = EDGE_LOOP ( 'NONE', ( #12365, #69253, #35227, #12059 ) ) ;
#24005 = CARTESIAN_POINT ( 'NONE',  ( 160.3106292389843759, 268.8982433465296253, -16.92231543148939821 ) ) ;
#24006 = VERTEX_POINT ( 'NONE', #84002 ) ;
#24007 = CARTESIAN_POINT ( 'NONE',  ( 70.99127280270764118, 71.57001342661881438, 1.849139882998378059 ) ) ;
#24008 = ORIENTED_EDGE ( 'NONE', *, *, #6392, .T. ) ;
#24009 = CARTESIAN_POINT ( 'NONE',  ( 164.1821508476733698, 246.2751683663292397, -7.347745041495428175 ) ) ;
#24010 = CIRCLE ( 'NONE', #14250, 70.00000000000001421 ) ;
#24012 = EDGE_CURVE ( 'NONE', #44226, #41771, #13081, .T. ) ;
#24011 = B_SPLINE_CURVE_WITH_KNOTS ( 'NONE', 3,
 ( #95835, #86738, #49189, #9702 ),
 .UNSPECIFIED., .F., .F.,
 ( 4, 4 ),
 ( 0.01365957469120875761, 0.02004134161460488853 ),
 .UNSPECIFIED. ) ;
#24013 = CARTESIAN_POINT ( 'NONE',  ( 81.74295896583093679, 45.02925702631734595, 10.54780463062767915 ) ) ;
#24014 = CYLINDRICAL_SURFACE ( 'NONE', #68886, 1.449999999999993072 ) ;
#24015 = CARTESIAN_POINT ( 'NONE',  ( 148.1004780136491377, 274.1294427855589788, -7.811560775291159331 ) ) ;
#24016 = CARTESIAN_POINT ( 'NONE',  ( 175.4882053081535105, 290.1142015617031689, 6.168936154768994484 ) ) ;
#24017 = CARTESIAN_POINT ( 'NONE',  ( 197.6892542711904071, 288.2391628223323892, -17.84453492130724683 ) ) ;
#24018 = CARTESIAN_POINT ( 'NONE',  ( 81.01234624326276901, 54.88323349113267113, -16.28327499330496053 ) ) ;
#24019 = CARTESIAN_POINT ( 'NONE',  ( 19.25324864145614612, 26.51421378149919761, -9.188101187500004485 ) ) ;
#24020 = AXIS2_PLACEMENT_3D ( 'NONE', #89650, #90652, #44981 ) ;
#24021 = CARTESIAN_POINT ( 'NONE',  ( 163.8627344909259307, 282.1053904094392237, 8.484041907820431661 ) ) ;
#24022 = CARTESIAN_POINT ( 'NONE',  ( 80.17048798456011127, 57.79824262504150312, 16.60278798193532879 ) ) ;
#24024 = ORIENTED_EDGE ( 'NONE', *, *, #21767, .F. ) ;
#24023 = CARTESIAN_POINT ( 'NONE',  ( 207.0213404229716900, 271.3941896262130626, 5.057553085821338001 ) ) ;
#24025 = CARTESIAN_POINT ( 'NONE',  ( 176.4901148274036586, 293.1746585049929763, 1.855142305940338465 ) ) ;
#24026 = CARTESIAN_POINT ( 'NONE',  ( 206.0930919633010774, 273.6832889610345774, -9.866500005465628220 ) ) ;
#24027 = DIRECTION ( 'NONE',  ( -1.000000000000000000, -9.785293164110366372E-14, 0.000000000000000000 ) ) ;
#24028 = CARTESIAN_POINT ( 'NONE',  ( 84.71308721041314982, 45.64921926619080494, -9.416152049834934701 ) ) ;
#24029 = CARTESIAN_POINT ( 'NONE',  ( 161.5431944097339851, 250.8459749958011287, 14.52339846942414603 ) ) ;
#24030 = CARTESIAN_POINT ( 'NONE',  ( 191.5383557437975242, 262.3965109955362891, -0.7496224257124077806 ) ) ;
#24031 = ORIENTED_EDGE ( 'NONE', *, *, #42814, .F. ) ;
#24032 = CARTESIAN_POINT ( 'NONE',  ( 155.3230890646803175, 261.6195134818649422, -18.58700029486878691 ) ) ;
#24033 = CARTESIAN_POINT ( 'NONE',  ( 74.67000616351420206, 66.81477949400924388, -13.12245706047550797 ) ) ;
#24034 = VECTOR ( 'NONE', #97969, 1000.000000000000000 ) ;
#24036 = CARTESIAN_POINT ( 'NONE',  ( -17.42236680055705023, 149.2012482093457777, 0.000000000000000000 ) ) ;
#24035 = B_SPLINE_CURVE_WITH_KNOTS ( 'NONE', 3,
 ( #90223, #26887, #73991, #66375 ),
 .UNSPECIFIED., .F., .F.,
 ( 4, 4 ),
 ( 0.003196948845168229043, 0.006410911750259561115 ),
 .UNSPECIFIED. ) ;
#24037 = CARTESIAN_POINT ( 'NONE',  ( 15.15952728095722435, 172.8927522451418213, 10.00000000000009592 ) ) ;
#24038 = CARTESIAN_POINT ( 'NONE',  ( 84.42325706775034178, 228.7369531367911293, -4.594050593750048428 ) ) ;
#24039 = CARTESIAN_POINT ( 'NONE',  ( 82.41720788485099547, 40.42146991629093833, -1.345722392452352034 ) ) ;
#24040 = VECTOR ( 'NONE', #48662, 1000.000000000000114 ) ;
#24041 = CARTESIAN_POINT ( 'NONE',  ( 175.0387250457744983, 253.3993311541219953, -7.863511161993287146 ) ) ;
#24042 = CARTESIAN_POINT ( 'NONE',  ( 166.8803400540483324, 278.2769978431516051, -14.68497553134216460 ) ) ;
#24044 = EDGE_CURVE ( 'NONE', #66029, #42203, #47999, .T. ) ;
#24043 = VECTOR ( 'NONE', #57147, 999.9999999999998863 ) ;
#24045 = CARTESIAN_POINT ( 'NONE',  ( 0.5273063997304934247, 181.1115022471903444, -5.000000000000047962 ) ) ;
#24047 = CARTESIAN_POINT ( 'NONE',  ( 75.75395351785276432, 65.60989001837319279, 13.81304751500886496 ) ) ;
#24046 = CARTESIAN_POINT ( 'NONE',  ( 11.05475416482865114, 183.3149278399160664, 9.188101187500093303 ) ) ;
#24048 = CARTESIAN_POINT ( 'NONE',  ( 161.4469036912142599, 251.0127554125742222, 12.93933463576739307 ) ) ;
#24049 = ORIENTED_EDGE ( 'NONE', *, *, #26198, .F. ) ;
#24050 = VECTOR ( 'NONE', #44044, 1000.000000000000000 ) ;
#24051 = ORIENTED_EDGE ( 'NONE', *, *, #98837, .T. ) ;
#24052 = DIRECTION ( 'NONE',  ( 0.8944271909999157444, 0.000000000000000000, -0.4472135954999582608 ) ) ;
#24053 = CARTESIAN_POINT ( 'NONE',  ( 200.8652091308636614, 267.7637384965461251, -2.870084330802582073 ) ) ;
#24054 = CARTESIAN_POINT ( 'NONE',  ( 85.12840156634364064, 46.10501368961206481, -9.731286439397152321 ) ) ;
#24055 = CARTESIAN_POINT ( 'NONE',  ( 84.72382484348065645, 44.74833322614003350, 8.228402119231732925 ) ) ;
#24056 = CARTESIAN_POINT ( 'NONE',  ( 207.1285138014047504, 271.8898857301724661, -5.752177443817618752 ) ) ;
#24057 = AXIS2_PLACEMENT_3D ( 'NONE', #100119, #61584, #39762 ) ;
#24058 = CARTESIAN_POINT ( 'NONE',  ( 83.20066689603021359, 44.07261036406099919, 8.458864577965798048 ) ) ;
#24059 = CARTESIAN_POINT ( 'NONE',  ( 74.44819773037836796, 68.07767128628745468, -11.61919445340353185 ) ) ;
#24060 = CARTESIAN_POINT ( 'NONE',  ( 36.33204418566946714, 191.7833772461660544, -9.188101187500095079 ) ) ;
#24061 = CARTESIAN_POINT ( 'NONE',  ( 199.9817534399692818, 276.6790051391964766, 15.46620920969797019 ) ) ;
#24062 = ORIENTED_EDGE ( 'NONE', *, *, #82016, .F. ) ;
#24063 = CARTESIAN_POINT ( 'NONE',  ( 74.62401959271109320, 66.89443057110611335, 13.05059976691391199 ) ) ;
#24064 = CARTESIAN_POINT ( 'NONE',  ( 182.4076066396311546, 260.8566311360108898, -10.64103732181219009 ) ) ;
#24065 = VECTOR ( 'NONE', #67923, 1000.000000000000000 ) ;
#24066 = CARTESIAN_POINT ( 'NONE',  ( 32.57180473799247977, 34.50829794293882458, -10.00000000000000355 ) ) ;
#24067 = FACE_OUTER_BOUND ( 'NONE', #55863, .T. ) ;
#24068 = CARTESIAN_POINT ( 'NONE',  ( 194.1153812227096864, 294.4292925221022870, 15.54001482840963710 ) ) ;
#24069 = CARTESIAN_POINT ( 'NONE',  ( 172.8210543149999978, 253.0650713199155177, -9.347212986753337560 ) ) ;
#24070 = CYLINDRICAL_SURFACE ( 'NONE', #17612, 10.00000000000010658 ) ;
#24071 = CARTESIAN_POINT ( 'NONE',  ( 148.1004780136491377, 274.1294427855589788, -7.811560775291159331 ) ) ;
#24072 = CARTESIAN_POINT ( 'NONE',  ( 71.43227217437114973, 62.73058494111581496, 14.40807302911904486 ) ) ;
#24073 = CARTESIAN_POINT ( 'NONE',  ( 165.0517352912010267, 249.7231812837857490, -10.72255941265194679 ) ) ;
#24074 = CARTESIAN_POINT ( 'NONE',  ( 35.87562414229657293, 44.21091486745863364, 7.012934429366973338E-14 ) ) ;
#24075 = CARTESIAN_POINT ( 'NONE',  ( 191.3610003135137276, 299.2000202002271294, -9.855749861282104618 ) ) ;
#24076 = CARTESIAN_POINT ( 'NONE',  ( 189.9462859318020946, 301.6503773875500087, -1.164147598593831656 ) ) ;
#24077 = CARTESIAN_POINT ( 'NONE',  ( 181.2024310249855148, 267.1550630910596738, -14.76750588113328355 ) ) ;
#24078 = ORIENTED_EDGE ( 'NONE', *, *, #77782, .T. ) ;
#24079 = CARTESIAN_POINT ( 'NONE',  ( 152.4356527347738108, 268.2593731114180287, -15.63005607008648923 ) ) ;
#24080 = CARTESIAN_POINT ( 'NONE',  ( 161.3788871511642071, 251.6867952676170148, -13.38168142625398005 ) ) ;
#24081 = CARTESIAN_POINT ( 'NONE',  ( 103.3675627755349353, 239.6744531367911577, 4.594050593750047540 ) ) ;
#24082 = CARTESIAN_POINT ( 'NONE',  ( 19.63753723929501760, 13.19860640527291551, 2.839279412974134775 ) ) ;
#24083 = CARTESIAN_POINT ( 'NONE',  ( 151.4159295687746294, 268.3869122420484814, 14.78076517566594106 ) ) ;
#24084 = CARTESIAN_POINT ( 'NONE',  ( 78.91767422429964540, 57.25042157409582444, -16.60633881229267672 ) ) ;
#24086 = CARTESIAN_POINT ( 'NONE',  ( 191.9527409762319223, 277.0321975987304768, 17.27471776080598076 ) ) ;
#24085 = CARTESIAN_POINT ( 'NONE',  ( 137.9907970510500377, 257.1427522451419350, -10.00000000000009592 ) ) ;
#24087 = CARTESIAN_POINT ( 'NONE',  ( 151.0375045328015631, 269.0423636312102076, -14.70054264444876857 ) ) ;
#24088 = CARTESIAN_POINT ( 'NONE',  ( 193.3455484147415859, 263.1264988859362006, -5.347548703547762905 ) ) ;
#24089 = CARTESIAN_POINT ( 'NONE',  ( 44.08135397534552169, 118.8355609772188188, -10.00000000000000000 ) ) ;
#24090 = DIRECTION ( 'NONE',  ( 0.3371987438498062484, -0.9414334852479556703, 0.000000000000000000 ) ) ;
#24091 = CARTESIAN_POINT ( 'NONE',  ( -76.86719868626529717, 52.73452925779879763, 177.5919119679930134 ) ) ;
#24092 = LINE ( 'NONE', #54988, #96033 ) ;
#24093 = ORIENTED_EDGE ( 'NONE', *, *, #65244, .F. ) ;
#24094 = CARTESIAN_POINT ( 'NONE',  ( -25.89332989531674301, 24.59406508915897760, -10.00000000000000000 ) ) ;
#24095 = CARTESIAN_POINT ( 'NONE',  ( 179.0584195722606751, 280.7836316943931365, 16.10768272107902277 ) ) ;
#24096 = CARTESIAN_POINT ( 'NONE',  ( 199.5392375079602232, 269.9326292274725461, 9.248178193193567154 ) ) ;
#24097 = ORIENTED_EDGE ( 'NONE', *, *, #50313, .T. ) ;
#24098 = EDGE_CURVE ( 'NONE', #30721, #23251, #4324, .T. ) ;
#24099 = CARTESIAN_POINT ( 'NONE',  ( 75.79167905567804553, 65.12415201610325255, -14.46789148266619485 ) ) ;
#24100 = CARTESIAN_POINT ( 'NONE',  ( 180.3398332753912712, 261.9433912727897109, -12.86148952795812228 ) ) ;
#24101 = EDGE_CURVE ( 'NONE', #38684, #32988, #68243, .T. ) ;
#24102 = DIRECTION ( 'NONE',  ( 0.5000000000000013323, -0.8660254037844378194, 0.000000000000000000 ) ) ;
#24103 = CARTESIAN_POINT ( 'NONE',  ( 75.03965799331250253, 52.98571459348521273, -16.01149241364986153 ) ) ;
#24104 = CARTESIAN_POINT ( 'NONE',  ( 48.23560136428437772, 110.1272893647940379, 10.00000000000000000 ) ) ;
#24105 = ORIENTED_EDGE ( 'NONE', *, *, #63047, .F. ) ;
#24106 = CARTESIAN_POINT ( 'NONE',  ( 183.4553195968295256, 297.0403188216897661, -2.838562726794640056 ) ) ;
#24107 = ADVANCED_FACE ( 'NONE', ( #98179 ), #91581, .F. ) ;
#24108 = VECTOR ( 'NONE', #71284, 1000.000000000000000 ) ;
#24109 = CARTESIAN_POINT ( 'NONE',  ( 33.58239374649102871, 42.49540643055189548, 3.479690158560446702E-15 ) ) ;
#24110 = ORIENTED_EDGE ( 'NONE', *, *, #3534, .T. ) ;
#24111 = CARTESIAN_POINT ( 'NONE',  ( 164.4590282730455044, 247.3987909035931523, 7.224049096378683643 ) ) ;
#24112 = EDGE_CURVE ( 'NONE', #23472, #43827, #12443, .T. ) ;
#24113 = CARTESIAN_POINT ( 'NONE',  ( 40.70814378237798081, 60.14496435084704018, -10.00000000000000000 ) ) ;
#24114 = CARTESIAN_POINT ( 'NONE',  ( 165.4408316472307376, 245.8969016233029379, -1.052724153476761959 ) ) ;
#24115 = VERTEX_POINT ( 'NONE', #82520 ) ;
#24116 = AXIS2_PLACEMENT_3D ( 'NONE', #2926, #80445, #87063 ) ;
#24117 = CARTESIAN_POINT ( 'NONE',  ( 86.55657754374946933, 47.30628205130771136, -10.74852006680812089 ) ) ;
#24118 = DIRECTION ( 'NONE',  ( 0.4635919272833914917, -0.8029647720336136052, 0.3746065934159158450 ) ) ;
#24119 = DIRECTION ( 'NONE',  ( 0.000000000000000000, 0.000000000000000000, -1.000000000000000000 ) ) ;
#24120 = CARTESIAN_POINT ( 'NONE',  ( 36.25628400652970384, 53.06077264917335867, -10.00000000000000000 ) ) ;
#24121 = VECTOR ( 'NONE', #40412, 1000.000000000000000 ) ;
#24122 = CARTESIAN_POINT ( 'NONE',  ( 167.5861325596884797, 256.5095974891418109, 15.03189046419509367 ) ) ;
#24123 = VECTOR ( 'NONE', #67270, 1000.000000000000114 ) ;
#24124 = CARTESIAN_POINT ( 'NONE',  ( 82.36604948993920061, 45.22791889282441957, -11.08805331368615832 ) ) ;
#24125 = CARTESIAN_POINT ( 'NONE',  ( 80.26965983545827044, 44.82647928622098021, 11.14148114410500412 ) ) ;
#24126 = CARTESIAN_POINT ( 'NONE',  ( 30.24280306353617576, 188.2677522451418497, 10.00000000000009592 ) ) ;
#24127 = ORIENTED_EDGE ( 'NONE', *, *, #18180, .F. ) ;
#24128 = ORIENTED_EDGE ( 'NONE', *, *, #9839, .T. ) ;
#24129 = CARTESIAN_POINT ( 'NONE',  ( 162.9767404783699476, 249.5334703659529794, 11.21793991045672101 ) ) ;
#24130 = EDGE_LOOP ( 'NONE', ( #45652, #88512, #19907, #28466, #14874 ) ) ;
#24131 = CARTESIAN_POINT ( 'NONE',  ( 77.31232694779509984, 49.13200894661118667, -15.30069998651773311 ) ) ;
#24132 = VERTEX_POINT ( 'NONE', #98684 ) ;
#24133 = CARTESIAN_POINT ( 'NONE',  ( 172.9470997986933583, 271.0928965516715152, 16.42712932072691956 ) ) ;
#24135 = CARTESIAN_POINT ( 'NONE',  ( 79.40743318721024480, 54.34964698095226510, 15.92978307125684445 ) ) ;
#24134 = AXIS2_PLACEMENT_3D ( 'NONE', #35210, #11932, #81362 ) ;
#24137 = VERTEX_POINT ( 'NONE', #90100 ) ;
#24136 =( BOUNDED_CURVE ( )  B_SPLINE_CURVE ( 2, ( #15163, #30884, #68869, #83629, #99797, #23769, #45078, #61770, #99303, #36979, #92717, #15670, #77500 ),
 .UNSPECIFIED., .F., .T. ) 
 B_SPLINE_CURVE_WITH_KNOTS ( ( 3, 2, 2, 2, 2, 2, 3 ),
 ( 0.3875000000000000111, 0.3900000000000000133, 0.3950000000000000178, 0.4000000000000000222, 0.4050000000000000266, 0.4099999999999999756, 0.4124999999999999778 ),
 .UNSPECIFIED. ) 
 CURVE ( )  GEOMETRIC_REPRESENTATION_ITEM ( )  RATIONAL_B_SPLINE_CURVE ( ( 0.9755282581475768211, 0.9755282581475768211, 1.000000000000000000, 0.9510565162951535312, 1.000000000000000000, 0.9510565162951535312, 1.000000000000000000, 0.9510565162951535312, 1.000000000000000000, 0.9510565162951535312, 1.000000000000000000, 0.9755282581475768211, 0.9755282581475768211 ) ) 
 REPRESENTATION_ITEM ( '' )  );
#24138 = CARTESIAN_POINT ( 'NONE',  ( 164.4494270235151419, 246.2274769805200378, 2.019287977540549672 ) ) ;
#24139 = CARTESIAN_POINT ( 'NONE',  ( 205.9736828131439097, 273.8901116759951719, -10.08879389214638778 ) ) ;
#24140 = CARTESIAN_POINT ( 'NONE',  ( 190.4402228526265048, 300.7948535449484098, 3.477366254517368027 ) ) ;
#24141 = CARTESIAN_POINT ( 'NONE',  ( 148.9498507103374152, 272.6582861203333437, 11.90061892622094852 ) ) ;
#24142 = CARTESIAN_POINT ( 'NONE',  ( 82.61013673858765571, 40.49722781981445507, 0.8877010427639511203 ) ) ;
#24143 = CARTESIAN_POINT ( 'NONE',  ( 171.3423592652010257, 250.9382160742572125, -5.598082297702525523 ) ) ;
#24144 = LINE ( 'NONE', #7955, #35535 ) ;
#24145 = CARTESIAN_POINT ( 'NONE',  ( 157.9671782409957359, 280.9922174830806512, 2.188311894391224310 ) ) ;
#24146 = CARTESIAN_POINT ( 'NONE',  ( 120.7963240266967375, 249.7369531367911293, -4.594050593750048428 ) ) ;
#24147 = CARTESIAN_POINT ( 'NONE',  ( 70.55887007047591908, 60.82933938485357572, -15.03632500835287189 ) ) ;
#24148 = CARTESIAN_POINT ( 'NONE',  ( 35.68911091587340678, 42.64646525600393545, -2.839279412974133887 ) ) ;
#24149 = EDGE_LOOP ( 'NONE', ( #77602, #65354, #15268, #67250 ) ) ;
#24150 = AXIS2_PLACEMENT_3D ( 'NONE', #9392, #40765, #63584 ) ;
#24152 = ORIENTED_EDGE ( 'NONE', *, *, #5791, .F. ) ;
#24151 = CARTESIAN_POINT ( 'NONE',  ( 85.53835401965352503, 48.98340217412621911, -12.70221784291844180 ) ) ;
#24153 = CARTESIAN_POINT ( 'NONE',  ( 200.2744661981036245, 273.7070197329613848, 13.96177302380764296 ) ) ;
#24154 = CARTESIAN_POINT ( 'NONE',  ( 32.46731799634992655, 102.8122225124608633, 59.99999999999999289 ) ) ;
#24155 = CARTESIAN_POINT ( 'NONE',  ( 171.3481116032015450, 287.9154882923708669, -4.631609681352044205 ) ) ;
#24156 = CARTESIAN_POINT ( 'NONE',  ( 192.4409507480105788, 297.3294911780226357, 11.00602545404914423 ) ) ;
#24157 = PLANE ( 'NONE',  #43501 ) ;
#24158 = CARTESIAN_POINT ( 'NONE',  ( 80.74974841587442143, 43.27611110060701805, 10.01619596027649095 ) ) ;
#24159 = CARTESIAN_POINT ( 'NONE',  ( 167.2515702596184042, 262.0622343731731689, -17.21809106051008342 ) ) ;
#24160 = CARTESIAN_POINT ( 'NONE',  ( 174.3399253482853055, 282.2778084546079072, 14.88242142284587999 ) ) ;
#24161 = CARTESIAN_POINT ( 'NONE',  ( 177.2207926979908450, 256.1411382841860700, -7.659123640409692513 ) ) ;
#24162 = VERTEX_POINT ( 'NONE', #76373 ) ;
#24163 = CARTESIAN_POINT ( 'NONE',  ( 200.5575725585719056, 282.8488716230692717, -16.71982794578856968 ) ) ;
#24164 = CARTESIAN_POINT ( 'NONE',  ( 150.4165202980163087, 271.9204874465632997, 11.69410747874298018 ) ) ;
#24165 = ORIENTED_EDGE ( 'NONE', *, *, #73883, .T. ) ;
#24166 = DIRECTION ( 'NONE',  ( -0.5000000000000013323, 0.8660254037844379305, 0.000000000000000000 ) ) ;
#24167 = B_SPLINE_CURVE_WITH_KNOTS ( 'NONE', 3,
 ( #30751, #24635, #7954, #53534 ),
 .UNSPECIFIED., .F., .F.,
 ( 4, 4 ),
 ( 0.01326838758303781549, 0.01964715698747628719 ),
 .UNSPECIFIED. ) ;
#24168 = CARTESIAN_POINT ( 'NONE',  ( 191.0339685792297644, 283.3628942986244397, -16.57419516574317697 ) ) ;
#24169 = CARTESIAN_POINT ( 'NONE',  ( 191.9264930372023059, 298.2205580714880853, -10.94482840438815074 ) ) ;
#24170 = CARTESIAN_POINT ( 'NONE',  ( 30.09478592234441408, 78.87673185299470902, 59.99999999999999289 ) ) ;
#24171 = ADVANCED_FACE ( 'NONE', ( #36348 ), #99167, .T. ) ;
#24172 = CARTESIAN_POINT ( 'NONE',  ( 204.6283382085973699, 273.0595963888450797, -10.48110626936752610 ) ) ;
#24174 = CARTESIAN_POINT ( 'NONE',  ( 160.8722636754860105, 281.5937424928134760, 5.676029096099265203 ) ) ;
#24173 = CARTESIAN_POINT ( 'NONE',  ( 164.3811851369638362, 283.5116506413451702, -6.723331180138965024 ) ) ;
#24175 = CYLINDRICAL_SURFACE ( 'NONE', #70506, 17.82106496071139645 ) ;
#24176 = ORIENTED_EDGE ( 'NONE', *, *, #39691, .F. ) ;
#24177 = CARTESIAN_POINT ( 'NONE',  ( 190.7908437487391780, 300.1875603386860689, -4.317984972589949955 ) ) ;
#24178 = DIRECTION ( 'NONE',  ( 1.000000000000000000, 1.465097884282125932E-13, 0.000000000000000000 ) ) ;
#24179 = CARTESIAN_POINT ( 'NONE',  ( 164.7364331287320738, 247.3151232938002693, -7.618980141130590411 ) ) ;
#24180 = CARTESIAN_POINT ( 'NONE',  ( 129.3070403213095005, 233.9155109091896065, 2.679491924311254714 ) ) ;
#24181 = CARTESIAN_POINT ( 'NONE',  ( 28.94376495785951775, 187.5177522451418497, -10.00000000000009592 ) ) ;
#24182 = CARTESIAN_POINT ( 'NONE',  ( 167.3350697697217413, 278.0087195862697058, 15.28430507972256258 ) ) ;
#24183 = CARTESIAN_POINT ( 'NONE',  ( 204.3334868499358095, 275.8344458505681018, 13.13630129970992400 ) ) ;
#24184 = CARTESIAN_POINT ( 'NONE',  ( 73.79815732168846409, 68.46225211080071915, 11.43730676814644553 ) ) ;
#24185 = CARTESIAN_POINT ( 'NONE',  ( 74.35881753926216220, 68.47570456641908265, 11.21376435697400709 ) ) ;
#24186 = DIRECTION ( 'NONE',  ( 0.3887219701523905169, 0.9213551052231945260, 0.000000000000000000 ) ) ;
#24187 = CARTESIAN_POINT ( 'NONE',  ( -1.340060878953613477, 170.0333772461660828, 9.188101187500095079 ) ) ;
#24188 = CARTESIAN_POINT ( 'NONE',  ( 82.93486267893707975, 224.8149278399160949, -9.188101187500095079 ) ) ;
#24189 = CARTESIAN_POINT ( 'NONE',  ( 155.5322964227545413, 261.2571557083629159, -18.35853982030605280 ) ) ;
#24190 = CARTESIAN_POINT ( 'NONE',  ( 192.8011239859581849, 296.7056528303708660, -11.79847971295421694 ) ) ;
#24191 = DIRECTION ( 'NONE',  ( 0.000000000000000000, 0.000000000000000000, 1.000000000000000000 ) ) ;
#24192 = EDGE_CURVE ( 'NONE', #41961, #36501, #6944, .T. ) ;
#24193 = CARTESIAN_POINT ( 'NONE',  ( 78.12501046422360673, 47.63414727997927400, 14.46436878840962059 ) ) ;
#24194 = AXIS2_PLACEMENT_3D ( 'NONE', #85164, #8627, #31413 ) ;
#24195 = CARTESIAN_POINT ( 'NONE',  ( 77.86187795391879263, 53.88640785478639117, 15.96271232416930630 ) ) ;
#24196 = B_SPLINE_CURVE_WITH_KNOTS ( 'NONE', 3,
 ( #87248, #80113, #64367, #96812 ),
 .UNSPECIFIED., .F., .F.,
 ( 4, 4 ),
 ( 0.01106257217117561677, 0.01948240598213658858 ),
 .UNSPECIFIED. ) ;
#24197 = CARTESIAN_POINT ( 'NONE',  ( 78.30955769916531040, 61.43963167811126169, 15.82323565659766373 ) ) ;
#24199 = CARTESIAN_POINT ( 'NONE',  ( 76.32610495235408621, 51.38149014994888830, 15.62204473798428239 ) ) ;
#24198 = DIRECTION ( 'NONE',  ( 0.000000000000000000, 0.000000000000000000, -1.000000000000000000 ) ) ;
#24200 = CARTESIAN_POINT ( 'NONE',  ( 179.4642332055343843, 290.3349191133465865, 9.386686624933396672 ) ) ;
#24201 = CARTESIAN_POINT ( 'NONE',  ( 169.0248750959679001, 251.9473120095521210, -8.780057449798482239 ) ) ;
#24202 = CARTESIAN_POINT ( 'NONE',  ( 163.9989516851529174, 246.5924786237186197, -4.702898507341187084 ) ) ;
#24204 = CARTESIAN_POINT ( 'NONE',  ( 157.3363371328520088, 258.1324655395517311, 18.24585617226787093 ) ) ;
#24203 = B_SPLINE_CURVE_WITH_KNOTS ( 'NONE', 3,
 ( #25627, #2334, #33735, #55006, #72240, #87984, #48926, #86478, #55493, #72752, #40295, #64626, #1328, #62598, #93552, #17006 ),
 .UNSPECIFIED., .F., .F.,
 ( 4, 1, 2, 2, 2, 1, 2, 2, 4 ),
 ( 0.000000000000000000, 0.1250000000000016653, 0.1875000000000024980, 0.2500000000000033307, 0.5000000000000043299, 0.6250000000000048850, 0.6875000000000051070, 0.7500000000000054401, 1.000000000000000000 ),
 .UNSPECIFIED. ) ;
#24205 = FACE_OUTER_BOUND ( 'NONE', #93163, .T. ) ;
#24206 = CARTESIAN_POINT ( 'NONE',  ( 72.69815669700709293, 57.09302316489889506, -15.89630389596367799 ) ) ;
#24207 = VECTOR ( 'NONE', #58149, 1000.000000000000114 ) ;
#24208 = CARTESIAN_POINT ( 'NONE',  ( 38.76791418169571557, 187.0643266524159856, -9.188101187500093303 ) ) ;
#24209 = CARTESIAN_POINT ( 'NONE',  ( 69.56611615166231388, 198.7202760586659736, -5.415160957724236172E-17 ) ) ;
#24210 = CARTESIAN_POINT ( 'NONE',  ( 194.0787454455293641, 279.1516233421318702, -17.53274283404612888 ) ) ;
#24211 = FACE_OUTER_BOUND ( 'NONE', #31251, .T. ) ;
#24212 = CARTESIAN_POINT ( 'NONE',  ( 166.9400527077043819, 259.7355344238575867, 15.86299304177872926 ) ) ;
#24213 = CARTESIAN_POINT ( 'NONE',  ( 144.0982539169780523, 247.8768266524160140, 9.188101187500098632 ) ) ;
#24215 = CARTESIAN_POINT ( 'NONE',  ( 77.08943580299947484, 49.61595851769168064, 15.51385818994994459 ) ) ;
#24214 = CARTESIAN_POINT ( 'NONE',  ( 71.80779569229208903, 72.11915028389421423, -3.640749997624285417 ) ) ;
#24217 = VECTOR ( 'NONE', #16502, 1000.000000000000114 ) ;
#24216 = CARTESIAN_POINT ( 'NONE',  ( 200.1771779054008960, 271.0770489275255386, -11.35077613890620185 ) ) ;
#24218 = CARTESIAN_POINT ( 'NONE',  ( 21.78279761992806129, 35.68290643055188838, 3.479690158560446702E-15 ) ) ;
#24219 = CARTESIAN_POINT ( 'NONE',  ( 198.8570476668614049, 286.2164853282868080, -17.01721544293231858 ) ) ;
#24220 = CARTESIAN_POINT ( 'NONE',  ( 149.1004267900891307, 272.3974806997987343, -12.86882154300063341 ) ) ;
#24221 = CARTESIAN_POINT ( 'NONE',  ( 18.45335787429653607, 11.44966523072493558, -2.296566073217252530E-15 ) ) ;
#24222 = CARTESIAN_POINT ( 'NONE',  ( 71.35211999908520397, 205.8768266524160424, 9.188101187500096856 ) ) ;
#24223 = CARTESIAN_POINT ( 'NONE',  ( 76.81877415327811320, 63.87294231776800757, 14.88723717811692282 ) ) ;
#24224 = CARTESIAN_POINT ( 'NONE',  ( 202.7973612924478743, 279.3916619310153919, -15.54732529288344089 ) ) ;
#24225 = CARTESIAN_POINT ( 'NONE',  ( 159.5284711081640125, 254.3355781173132755, 15.34104435652608522 ) ) ;
#24226 = DIRECTION ( 'NONE',  ( -0.7845058662180028897, -0.6201213960746241316, 0.000000000000000000 ) ) ;
#24227 = CARTESIAN_POINT ( 'NONE',  ( 7.225231395932164347, 28.43104314603599647, 177.5919119679930134 ) ) ;
#24228 = EDGE_CURVE ( 'NONE', #31200, #93443, #9454, .T. ) ;
#24229 = CARTESIAN_POINT ( 'NONE',  ( -19.65312891409030271, 93.06504152958497400, 45.00000000000000711 ) ) ;
#24230 = CARTESIAN_POINT ( 'NONE',  ( 114.8426596992765099, 227.1115022471901739, -5.000000000000041744 ) ) ;
#24231 = CARTESIAN_POINT ( 'NONE',  ( -65.00000000000000000, 10.00000000000000000, -54.99999999999999289 ) ) ;
#24232 = CARTESIAN_POINT ( 'NONE',  ( 206.9026071836525205, 272.2811674698855313, 7.240992997279449561 ) ) ;
#24233 = ORIENTED_EDGE ( 'NONE', *, *, #40702, .T. ) ;
#24234 = CARTESIAN_POINT ( 'NONE',  ( 77.58396476582734635, 49.27429002014808646, 15.29533474293770823 ) ) ;
#24235 = CARTESIAN_POINT ( 'NONE',  ( 186.1070094314815719, 272.1961740520177955, 15.73899880559026876 ) ) ;
#24236 = ORIENTED_EDGE ( 'NONE', *, *, #93715, .T. ) ;
#24237 = CARTESIAN_POINT ( 'NONE',  ( 206.6298919378964740, 272.7535241315335384, -9.267551915974392429 ) ) ;
#24238 = CARTESIAN_POINT ( 'NONE',  ( 193.8280528473190998, 294.2408607629556059, 13.96266529814797330 ) ) ;
#24239 = CARTESIAN_POINT ( 'NONE',  ( 70.34943318750055141, 68.90035037863729883, -7.849331805225474135 ) ) ;
#24240 = ADVANCED_FACE ( 'NONE', ( #69738 ), #32699, .T. ) ;
#24241 = ORIENTED_EDGE ( 'NONE', *, *, #91067, .T. ) ;
#24242 = CARTESIAN_POINT ( 'NONE',  ( 173.7443271944094647, 250.8610699240076940, 0.5123999366559217616 ) ) ;
#24243 = ORIENTED_EDGE ( 'NONE', *, *, #66320, .T. ) ;
#24244 = CARTESIAN_POINT ( 'NONE',  ( 66.15980552222140432, 69.17909379384724389, -2.043126084711875734 ) ) ;
#24245 = CARTESIAN_POINT ( 'NONE',  ( 194.3708539535661259, 293.9868007723104029, -16.01585187499628304 ) ) ;
#24246 = PLANE ( 'NONE',  #7824 ) ;
#24247 = ORIENTED_EDGE ( 'NONE', *, *, #75542, .T. ) ;
#24248 = CARTESIAN_POINT ( 'NONE',  ( 31.84670776885679899, 24.10170272979928541, -7.433330006724141015 ) ) ;
#24249 = CARTESIAN_POINT ( 'NONE',  ( 86.71718800452170228, 209.3262482093457777, 3.021315404115420679E-15 ) ) ;
#24250 = FACE_OUTER_BOUND ( 'NONE', #78576, .T. ) ;
#24251 = ORIENTED_EDGE ( 'NONE', *, *, #18119, .F. ) ;
#24252 = ADVANCED_FACE ( 'NONE', ( #87530 ), #40822, .F. ) ;
#24253 = CARTESIAN_POINT ( 'NONE',  ( 176.4997286254413780, 263.1504487394882972, -15.79179489836881167 ) ) ;
#24254 = CARTESIAN_POINT ( 'NONE',  ( 159.9770824720811220, 253.5585604421560788, -16.42166711341322483 ) ) ;
#24255 = EDGE_LOOP ( 'NONE', ( #22823, #64375, #78127, #25294 ) ) ;
#24256 = DIRECTION ( 'NONE',  ( -0.000000000000000000, -0.000000000000000000, -1.000000000000000000 ) ) ;
#24258 = CARTESIAN_POINT ( 'NONE',  ( 67.99955159661209336, 66.07893017027207350, -10.48801018483890068 ) ) ;
#24257 = CARTESIAN_POINT ( 'NONE',  ( 67.94506607690384214, 65.68283619601920975, 10.86420754080536355 ) ) ;
#24259 = CARTESIAN_POINT ( 'NONE',  ( 165.0528804069804494, 264.4852527057752241, -17.76608744198970768 ) ) ;
#24260 = CARTESIAN_POINT ( 'NONE',  ( 194.4904290197884507, 293.7796906822950973, 14.50206953321744940 ) ) ;
#24261 = CARTESIAN_POINT ( 'NONE',  ( 185.2685622359955744, 292.7380640902246682, -11.87166941586229996 ) ) ;
#24262 = CARTESIAN_POINT ( 'NONE',  ( 157.3198323354746435, 258.1610526871778006, -16.77630483474704093 ) ) ;
#24263 = CARTESIAN_POINT ( 'NONE',  ( 207.9186838572135514, 270.5212710468924229, -3.653080245775895740 ) ) ;
#24264 = AXIS2_PLACEMENT_3D ( 'NONE', #10450, #41324, #18559 ) ;
#24265 = LINE ( 'NONE', #78995, #17692 ) ;
#24266 = CARTESIAN_POINT ( 'NONE',  ( 182.7174818772467120, 259.2068321934141295, 9.747744062958584976 ) ) ;
#24267 = CARTESIAN_POINT ( 'NONE',  ( 85.91165145656356117, 232.6589784336661637, -6.496448406907675876E-16 ) ) ;
#24268 = ORIENTED_EDGE ( 'NONE', *, *, #19007, .F. ) ;
#24269 = CARTESIAN_POINT ( 'NONE',  ( 151.2455280670316711, 268.6820563007532314, 14.35914944935941229 ) ) ;
#24270 = CARTESIAN_POINT ( 'NONE',  ( 19.31801425620940194, 115.5650415295850451, 60.00000000000000000 ) ) ;
#24271 = FACE_OUTER_BOUND ( 'NONE', #69584, .T. ) ;
#24272 = ORIENTED_EDGE ( 'NONE', *, *, #86416, .F. ) ;
#24273 = LINE ( 'NONE', #77487, #8978 ) ;
#24274 = ORIENTED_EDGE ( 'NONE', *, *, #50941, .F. ) ;
#24275 = ORIENTED_EDGE ( 'NONE', *, *, #35995, .F. ) ;
#24276 = CARTESIAN_POINT ( 'NONE',  ( 79.92051602943618605, 44.51830849947365465, -11.04832637642992132 ) ) ;
#24277 = DIRECTION ( 'NONE',  ( -0.000000000000000000, -0.000000000000000000, -1.000000000000000000 ) ) ;
#24278 = CARTESIAN_POINT ( 'NONE',  ( -52.52455383977511616, 97.96304663431351401, -10.00000000000000000 ) ) ;
#24279 = CARTESIAN_POINT ( 'NONE',  ( 80.97096062864531518, 55.95811706980097000, 16.09172280808637012 ) ) ;
#24280 = CARTESIAN_POINT ( 'NONE',  ( 79.30706684625435798, 48.64070561785491265, -14.10287111613649635 ) ) ;
#24281 = CARTESIAN_POINT ( 'NONE',  ( 207.8616498235123231, 270.6200568910230118, 3.132900500943239130 ) ) ;
#24282 = CARTESIAN_POINT ( 'NONE',  ( 77.73905735199544154, 209.5643266524159571, -9.188101187500093303 ) ) ;
#24283 = ORIENTED_EDGE ( 'NONE', *, *, #68646, .F. ) ;
#24284 = VECTOR ( 'NONE', #22076, 1000.000000000000114 ) ;
#24285 = VERTEX_POINT ( 'NONE', #79891 ) ;
#24286 = B_SPLINE_SURFACE_WITH_KNOTS ( 'NONE', 3, 1, ( 
 ( #52836, #21941 ),
 ( #68537, #82799 ),
 ( #21451, #13368 ),
 ( #44232, #44725 ),
 ( #83280, #6243 ),
 ( #98471, #5257 ),
 ( #91889, #75170 ),
 ( #29064, #99460 ),
 ( #89893, #30038 ),
 ( #52339, #74683 ),
 ( #59931, #83786 ),
 ( #36139, #90901 ),
 ( #82309, #45723 ),
 ( #53335, #68043 ),
 ( #22441, #98965 ),
 ( #60925, #45236 ),
 ( #29548, #14348 ),
 ( #35654, #66553 ),
 ( #51343, #67041 ),
 ( #97965, #28541 ),
 ( #90402, #20977 ),
 ( #51859, #39114 ),
 ( #31523, #61921 ),
 ( #69538, #84780 ),
 ( #8740, #39611 ),
 ( #62416, #146 ),
 ( #55319, #86798 ),
 ( #1659, #92870 ),
 ( #99960, #93377 ),
 ( #23929, #8249 ),
 ( #55805, #24931 ) ),
 .UNSPECIFIED., .F., .F., .F.,
 ( 4, 3, 3, 3, 3, 3, 3, 3, 3, 3, 4 ),
 ( 2, 2 ),
 ( 0.000000000000000000, 0.1122669598086838000, 0.2243161639709725652, 0.3396355846219227259, 0.4553962076585201801, 0.5677860799922432866, 0.6749047109689664259, 0.7773884377078287278, 0.8775581155834328850, 0.9782364162377897854, 1.000000000000000000 ),
 ( 0.000000000000000000, 1.000000000000000000 ),
 .UNSPECIFIED. ) ;
#24287 = CARTESIAN_POINT ( 'NONE',  ( 161.9258069053378222, 250.1832707138045180, -14.03928993546631254 ) ) ;
#24288 = VERTEX_POINT ( 'NONE', #65145 ) ;
#24289 = CARTESIAN_POINT ( 'NONE',  ( 105.0000000000000000, 0.000000000000000000, 59.99999999999999289 ) ) ;
#24290 = CARTESIAN_POINT ( 'NONE',  ( 184.0509685884657642, 275.1883516303099668, 16.37021283893107793 ) ) ;
#24291 = CARTESIAN_POINT ( 'NONE',  ( 19.19489604512981984, 34.58029201028041655, 1.583844403245397769 ) ) ;
#24292 = EDGE_CURVE ( 'NONE', #35343, #31579, #39550, .T. ) ;
#24293 = CARTESIAN_POINT ( 'NONE',  ( 161.7341544900357064, 283.8969558588514133, 0.5209753697341674705 ) ) ;
#24294 = CARTESIAN_POINT ( 'NONE',  ( 207.1502663293453281, 270.3057540939174714, -2.562904251084027418 ) ) ;
#24295 = CARTESIAN_POINT ( 'NONE',  ( 87.86895504114028199, 44.78688104239807188, 4.940966480777958303 ) ) ;
#24296 = ORIENTED_EDGE ( 'NONE', *, *, #84274, .T. ) ;
#24297 = CARTESIAN_POINT ( 'NONE',  ( 188.6621308970854898, 295.0522997026344569, 11.72041705296824965 ) ) ;
#24298 = CARTESIAN_POINT ( 'NONE',  ( 156.8942407771241108, 274.4291350306359618, 13.75659550080370508 ) ) ;
#24299 = CARTESIAN_POINT ( 'NONE',  ( 206.1408608592916494, 273.6005508061571732, -10.42739367433323494 ) ) ;
#24300 = EDGE_CURVE ( 'NONE', #63648, #25248, #50437, .T. ) ;
#24301 = DIRECTION ( 'NONE',  ( -0.2774202615135436534, 0.9607486656258009683, 0.000000000000000000 ) ) ;
#24302 = CARTESIAN_POINT ( 'NONE',  ( -19.65312891409030271, 5.000000000000004441, 54.99999999999999289 ) ) ;
#24303 = CARTESIAN_POINT ( 'NONE',  ( 72.50911665321707744, 70.64777112744620524, 7.215784761677396908 ) ) ;
#24304 = DIRECTION ( 'NONE',  ( -0.8660254037844387076, -0.4999999999999998890, -0.000000000000000000 ) ) ;
#24305 = ORIENTED_EDGE ( 'NONE', *, *, #15980, .T. ) ;
#24306 = DIRECTION ( 'NONE',  ( -0.7893155279419928894, -0.6139877827364751406, 0.000000000000000000 ) ) ;
#24307 = CARTESIAN_POINT ( 'NONE',  ( 200.7583183585857967, 282.9233878912788214, 16.96937806979494212 ) ) ;
#24308 = DIRECTION ( 'NONE',  ( 0.5000000000000013323, -0.8660254037844378194, 0.000000000000000000 ) ) ;
#24309 = CARTESIAN_POINT ( 'NONE',  ( 171.3764566354917633, 251.6546961497424491, 7.121511699425036923 ) ) ;
#24310 = CARTESIAN_POINT ( 'NONE',  ( 83.85749844460281111, 51.92724282576335071, 14.91256361652490092 ) ) ;
#24311 = EDGE_CURVE ( 'NONE', #11459, #71854, #40821, .T. ) ;
#24312 = CARTESIAN_POINT ( 'NONE',  ( -22.42236680055709641, 157.8615022471902591, 0.000000000000000000 ) ) ;
#24313 = ORIENTED_EDGE ( 'NONE', *, *, #53158, .F. ) ;
#24314 = CARTESIAN_POINT ( 'NONE',  ( -17.31098718113245027, 103.3584764561434639, 44.62636701040934639 ) ) ;
#24315 = CARTESIAN_POINT ( 'NONE',  ( 164.3774690880109119, 245.9368672504194819, -2.805681983503304000 ) ) ;
#24317 = CARTESIAN_POINT ( 'NONE',  ( 73.67565831133079257, 55.36794421709517167, 16.58968170789317398 ) ) ;
#24316 = CARTESIAN_POINT ( 'NONE',  ( 48.05801951159151031, 75.31115804243518141, 177.5919119679930134 ) ) ;
#24318 = CARTESIAN_POINT ( 'NONE',  ( 176.1441259402330672, 285.2298478058193041, -12.99515216835783882 ) ) ;
#24319 = CARTESIAN_POINT ( 'NONE',  ( 32.00589586780220941, 18.28848085856232331, 1.475505719884397138E-15 ) ) ;
#24320 = EDGE_CURVE ( 'NONE', #166, #47151, #27660, .T. ) ;
#24321 = CARTESIAN_POINT ( 'NONE',  ( 166.5889384249973091, 286.4434954512080935, -3.248033821752349226 ) ) ;
#24322 = CARTESIAN_POINT ( 'NONE',  ( 124.6655725107735435, 254.3297689869269504, -2.679491924311252493 ) ) ;
#24323 = FACE_OUTER_BOUND ( 'NONE', #35145, .T. ) ;
#24324 = DIRECTION ( 'NONE',  ( 1.000000000000000000, 0.000000000000000000, 0.000000000000000000 ) ) ;
#24325 = CARTESIAN_POINT ( 'NONE',  ( -8.349714312657674498, 175.1744531367911293, 4.594050593750047540 ) ) ;
#24326 = DIRECTION ( 'NONE',  ( 0.5000000000000000000, -0.8660254037844387076, 0.000000000000000000 ) ) ;
#24327 = ORIENTED_EDGE ( 'NONE', *, *, #6733, .F. ) ;
#24328 = VECTOR ( 'NONE', #53982, 1000.000000000000114 ) ;
#24329 = CARTESIAN_POINT ( 'NONE',  ( 176.4535474755452356, 256.1020709052521056, 8.255247991639031113 ) ) ;
#24330 = CARTESIAN_POINT ( 'NONE',  ( 185.2609771608511835, 270.5205629937861431, -16.69046129513680299 ) ) ;
#24331 = CARTESIAN_POINT ( 'NONE',  ( -0.2492734796364604877, 27.10516647459197515, -10.00000000000000000 ) ) ;
#24332 = CARTESIAN_POINT ( 'NONE',  ( 19.47135178391741661, 191.2369531367911293, -4.594050593750048428 ) ) ;
#24333 = DIRECTION ( 'NONE',  ( -0.07193265315672570104, 0.9974094913373514615, 0.000000000000000000 ) ) ;
#24334 = CARTESIAN_POINT ( 'NONE',  ( 24.67121952831112353, 36.01751292744057764, 6.180339887498949913 ) ) ;
#24335 = CARTESIAN_POINT ( 'NONE',  ( 82.28514220754047415, 41.58448466926779474, -4.581006405137011406 ) ) ;
#24336 = CARTESIAN_POINT ( 'NONE',  ( 191.3041230083617563, 299.2985345825480863, -9.819045872446528378 ) ) ;
#24337 = CARTESIAN_POINT ( 'NONE',  ( 81.66701081066987911, 55.79068320882007725, 16.00012122222618771 ) ) ;
#24338 = ADVANCED_FACE ( 'NONE', ( #75255 ), #47986, .T. ) ;
#24339 = EDGE_CURVE ( 'NONE', #88734, #68766, #59010, .T. ) ;
#24340 = CARTESIAN_POINT ( 'NONE',  ( 186.5727140431293378, 296.2605864597566665, -8.800404970033115504 ) ) ;
#24341 = CARTESIAN_POINT ( 'NONE',  ( 190.7335255870825108, 261.9646230305896779, -0.8058728106476181763 ) ) ;
#24342 = AXIS2_PLACEMENT_3D ( 'NONE', #8603, #95251, #39469 ) ;
#24343 = EDGE_CURVE ( 'NONE', #99018, #33772, #46945, .T. ) ;
#24344 = CARTESIAN_POINT ( 'NONE',  ( 60.28305926085675992, 215.6115022471903160, -5.000000000000047962 ) ) ;
#24345 = CARTESIAN_POINT ( 'NONE',  ( 71.57492018021982005, 66.57275065399230130, -11.35834070733682744 ) ) ;
#24346 = CARTESIAN_POINT ( 'NONE',  ( 203.4603280001158794, 270.1122314455482183, 6.026633026702996609 ) ) ;
#24347 = CARTESIAN_POINT ( 'NONE',  ( 38.44315465527655107, 186.8768266524159856, -9.188101187500091527 ) ) ;
#24348 = CARTESIAN_POINT ( 'NONE',  ( 193.0405099973349081, 283.7233392346411165, 17.77886865111357295 ) ) ;
#24349 = LINE ( 'NONE', #69440, #61370 ) ;
#24350 = CARTESIAN_POINT ( 'NONE',  ( 203.4761922537706482, 269.1684635965042958, -5.985248603416074786 ) ) ;
#24351 = B_SPLINE_CURVE_WITH_KNOTS ( 'NONE', 3,
 ( #96363, #74035, #34043, #33530, #72554, #35516, #27435, #64427, #95389, #10736, #81659, #95877, #42113, #3158, #26929, #64933 ),
 .UNSPECIFIED., .F., .F.,
 ( 4, 2, 2, 2, 2, 2, 2, 4 ),
 ( 0.000000000000000000, 0.0004989544299106570078, 0.0007484316448658957397, 0.0009979088598211346885, 0.001247386074776373312, 0.001496863289731612152, 0.001746340504686851426, 0.001995817719642090267 ),
 .UNSPECIFIED. ) ;
#24352 = CARTESIAN_POINT ( 'NONE',  ( 198.9225589249066957, 286.1030165008847916, -17.03502353404871883 ) ) ;
#24353 = DIRECTION ( 'NONE',  ( 0.1378186779084994706, -0.2387089523694924387, -0.9612616959383186721 ) ) ;
#24354 = EDGE_CURVE ( 'NONE', #71770, #8790, #65069, .T. ) ;
#24355 = CARTESIAN_POINT ( 'NONE',  ( 179.7389585068036979, 283.2694176073634935, 16.15404047216739514 ) ) ;
#24356 = CARTESIAN_POINT ( 'NONE',  ( 202.4119438311506940, 279.2703662523446155, -15.60349858348900476 ) ) ;
#24357 = CARTESIAN_POINT ( 'NONE',  ( 205.7858960462819766, 269.5612804690865687, -1.325532578154042351 ) ) ;
#24358 = CARTESIAN_POINT ( 'NONE',  ( 26.03951966209473312, 17.96004757982090538, -5.678558825948276656 ) ) ;
#24359 = CARTESIAN_POINT ( 'NONE',  ( 163.3854574543125580, 247.6550818016845597, 10.82482370245618775 ) ) ;
#24360 = CARTESIAN_POINT ( 'NONE',  ( 149.5390997184345281, 271.6376768999995761, -11.52989534384373016 ) ) ;
#24361 = CARTESIAN_POINT ( 'NONE',  ( 175.3141911485210187, 257.2753051901946719, 11.72392066680403744 ) ) ;
#24362 = ORIENTED_EDGE ( 'NONE', *, *, #84952, .F. ) ;
#24363 = CARTESIAN_POINT ( 'NONE',  ( 13.40518456965460281, 16.24335787977761925, -9.188101187500008038 ) ) ;
#24364 = ADVANCED_FACE ( 'NONE', ( #12459 ), #98562, .T. ) ;
#24365 = CARTESIAN_POINT ( 'NONE',  ( 47.32807415326522715, 108.5480133836684900, -10.00000000000000000 ) ) ;
#24366 = LINE ( 'NONE', #72493, #98645 ) ;
#24367 = CARTESIAN_POINT ( 'NONE',  ( 71.81881128194709163, 72.53313204687133009, -1.300380427722385823 ) ) ;
#24368 = ORIENTED_EDGE ( 'NONE', *, *, #55451, .F. ) ;
#24369 = CARTESIAN_POINT ( 'NONE',  ( 175.8132799389368017, 292.7022098518745565, -2.441052075075039518 ) ) ;
#24370 = CARTESIAN_POINT ( 'NONE',  ( 70.36952472774478906, 71.02280663496645730, -2.695929215683882774 ) ) ;
#24371 = CARTESIAN_POINT ( 'NONE',  ( 150.6533415055477008, 269.7077535128032082, 14.84621632544246062 ) ) ;
#24372 = CARTESIAN_POINT ( 'NONE',  ( 179.7438496854340997, 257.3540159337386513, -7.334582191190184730 ) ) ;
#24373 = ORIENTED_EDGE ( 'NONE', *, *, #40599, .F. ) ;
#24374 = ORIENTED_EDGE ( 'NONE', *, *, #42172, .F. ) ;
#24376 = CARTESIAN_POINT ( 'NONE',  ( 86.68781752468889579, 43.33485113087137819, -1.416241137521898619 ) ) ;
#24375 = CARTESIAN_POINT ( 'NONE',  ( 187.4378393846737367, 272.8763525007090607, -15.77460183161252516 ) ) ;
#24377 = EDGE_LOOP ( 'NONE', ( #83250, #26653, #88115, #62861 ) ) ;
#24378 = CARTESIAN_POINT ( 'NONE',  ( 66.10978050773523762, 68.50388961278160593, -2.614487067079704907 ) ) ;
#24379 = DIRECTION ( 'NONE',  ( 0.5000000000000002220, -0.8660254037844387076, -0.000000000000000000 ) ) ;
#24380 = CARTESIAN_POINT ( 'NONE',  ( 80.12283971196008281, 57.76720862780119603, 16.60271659255639776 ) ) ;
#24381 = CARTESIAN_POINT ( 'NONE',  ( 7.533646096595723485, 16.30066082961419482, -10.00000000000000533 ) ) ;
#24382 = CARTESIAN_POINT ( 'NONE',  ( 190.6036479972031259, 300.5117928913073797, -0.6824572005520307405 ) ) ;
#24383 = DIRECTION ( 'NONE',  ( -1.000000000000000000, 0.000000000000000000, 0.000000000000000000 ) ) ;
#24384 = VERTEX_POINT ( 'NONE', #37227 ) ;
#24385 = CYLINDRICAL_SURFACE ( 'NONE', #61155, 16.60714546451156792 ) ;
#24386 = CARTESIAN_POINT ( 'NONE',  ( 162.1978965794471890, 266.5548187812856895, 17.22461409982334501 ) ) ;
#24387 = ORIENTED_EDGE ( 'NONE', *, *, #93373, .F. ) ;
#24388 = CARTESIAN_POINT ( 'NONE',  ( 25.67147243227365294, 35.79752408145593989, -5.678558825948271327 ) ) ;
#24389 = CARTESIAN_POINT ( 'NONE',  ( 159.5284711081640125, 254.3355781173132755, 15.34104435652608522 ) ) ;
#24390 = CARTESIAN_POINT ( 'NONE',  ( -19.65312891409030271, 93.06504152958497400, 10.00000000000000888 ) ) ;
#24391 = CARTESIAN_POINT ( 'NONE',  ( 51.40603854846860798, 209.6744531367911293, 4.594050593750047540 ) ) ;
#24392 = ORIENTED_EDGE ( 'NONE', *, *, #59171, .F. ) ;
#24393 = CARTESIAN_POINT ( 'NONE',  ( 74.38015889281619764, 68.44084013566667579, 11.25477996513194867 ) ) ;
#24394 = CARTESIAN_POINT ( 'NONE',  ( 70.22199747613832699, 222.8967562850346837, -4.648177544792955347E-16 ) ) ;
#24395 = CARTESIAN_POINT ( 'NONE',  ( 87.83349241520130590, 231.5177522451419350, 5.000000000000046185 ) ) ;
#24396 = CARTESIAN_POINT ( 'NONE',  ( 80.93613592869992601, 42.95327845849681836, -9.503115154567232992 ) ) ;
#24397 = ORIENTED_EDGE ( 'NONE', *, *, #32916, .T. ) ;
#24398 = CARTESIAN_POINT ( 'NONE',  ( 87.09272086398131307, 46.41253043617862062, 8.753911316151357980 ) ) ;
#24399 = CARTESIAN_POINT ( 'NONE',  ( 146.8881680668833951, 276.2292252078784145, 4.973452195244782104 ) ) ;
#24400 = CARTESIAN_POINT ( 'NONE',  ( 78.02511763684471191, 53.60668594641142448, 16.35104529020703623 ) ) ;
#24401 = ORIENTED_EDGE ( 'NONE', *, *, #33686, .T. ) ;
#24402 = CARTESIAN_POINT ( 'NONE',  ( 174.4278075863048230, 260.9700190746071371, -14.02905432283994536 ) ) ;
#24403 = CARTESIAN_POINT ( 'NONE',  ( 170.7059362337859056, 275.4258791682946139, -16.58347944357980452 ) ) ;
#24404 = CARTESIAN_POINT ( 'NONE',  ( 161.8150574665248200, 250.3750943687383881, -13.25074899737357903 ) ) ;
#24405 = CARTESIAN_POINT ( 'NONE',  ( 147.3715240516018810, 275.3920280842035595, -3.728968767617475866 ) ) ;
#24406 = CARTESIAN_POINT ( 'NONE',  ( 148.9228818358559749, 272.7049975811580680, 12.13823097167056275 ) ) ;
#24407 = CARTESIAN_POINT ( 'NONE',  ( 83.67416965427615594, 41.61942911856458949, 0.1873010706438003881 ) ) ;
#24408 = EDGE_CURVE ( 'NONE', #33333, #79838, #86384, .T. ) ;
#24409 = CARTESIAN_POINT ( 'NONE',  ( 206.0041637419966776, 273.8373171585603814, 11.66586596407113596 ) ) ;
#24410 = CARTESIAN_POINT ( 'NONE',  ( 67.51011536099680654, 66.65123204117807632, 8.646292631228400083 ) ) ;
#24411 = DIRECTION ( 'NONE',  ( -0.8660254037844359321, -0.5000000000000051070, -0.000000000000000000 ) ) ;
#24412 = CARTESIAN_POINT ( 'NONE',  ( 163.7587049410067266, 247.0085981909329576, -6.137518685179130351 ) ) ;
#24413 = CARTESIAN_POINT ( 'NONE',  ( 115.3025621453804490, 243.5024278399160949, 9.188101187500095079 ) ) ;
#24414 = ORIENTED_EDGE ( 'NONE', *, *, #31289, .T. ) ;
#24415 = CARTESIAN_POINT ( 'NONE',  ( 148.9845638001402506, 272.5981612851071532, -12.53752629571579291 ) ) ;
#24416 = CARTESIAN_POINT ( 'NONE',  ( 69.82278528426677155, 64.04957407583405882, 12.51083613146919227 ) ) ;
#24417 = EDGE_CURVE ( 'NONE', #39680, #39791, #44422, .T. ) ;
#24418 = CARTESIAN_POINT ( 'NONE',  ( 154.8786460229866577, 262.3893114111486398, -18.06164891362396929 ) ) ;
#24419 = CARTESIAN_POINT ( 'NONE',  ( 204.7986527064648214, 275.9253235211867263, 14.74587861556245905 ) ) ;
#24420 = CARTESIAN_POINT ( 'NONE',  ( 83.63562430374231838, 51.63275018564552710, -14.84107497619760174 ) ) ;
#24421 = CIRCLE ( 'NONE', #14722, 70.00000000000001421 ) ;
#24422 = CARTESIAN_POINT ( 'NONE',  ( 174.8210708869210350, 252.8123362264541640, 5.084827073808857456 ) ) ;
#24423 = ORIENTED_EDGE ( 'NONE', *, *, #55203, .T. ) ;
#24424 = CARTESIAN_POINT ( 'NONE',  ( 80.42443749358989180, 57.88788176714987799, -16.24735605553297191 ) ) ;
#24425 = CARTESIAN_POINT ( 'NONE',  ( 32.31598214102135103, 82.54078291444118065, 59.99999999999999289 ) ) ;
#24426 = CARTESIAN_POINT ( 'NONE',  ( 182.3683164725543691, 259.8255612630188693, 10.74697378040428752 ) ) ;
#24427 = CARTESIAN_POINT ( 'NONE',  ( 206.3869432407897193, 272.3943931181467519, 8.042875945707256946 ) ) ;
#24428 = CARTESIAN_POINT ( 'NONE',  ( 129.0235653626489238, 254.4869531367911577, 4.594050593750046652 ) ) ;
#24429 = ADVANCED_FACE ( 'NONE', ( #55399 ), #46823, .F. ) ;
#24430 = CARTESIAN_POINT ( 'NONE',  ( 189.7153962340875637, 294.7489371240931746, -12.64634207402519550 ) ) ;
#24431 = CARTESIAN_POINT ( 'NONE',  ( 189.1446688698201513, 299.4652302210857329, 4.877423590139457588 ) ) ;
#24432 = CARTESIAN_POINT ( 'NONE',  ( 187.3746306850530914, 281.3025677867038326, -17.17837978889408745 ) ) ;
#24433 = LINE ( 'NONE', #8731, #22382 ) ;
#24434 = CARTESIAN_POINT ( 'NONE',  ( 47.69862761034023180, 198.3458772461660544, 9.188101187500095079 ) ) ;
#24435 = CARTESIAN_POINT ( 'NONE',  ( 85.64890296506385425, 48.36409154393287224, -11.71277604259690541 ) ) ;
#24436 = ORIENTED_EDGE ( 'NONE', *, *, #6261, .F. ) ;
#24437 = CARTESIAN_POINT ( 'NONE',  ( 72.06403648541707696, 66.67572987517343108, 11.55341923834466833 ) ) ;
#24438 = DIRECTION ( 'NONE',  ( 0.000000000000000000, 0.000000000000000000, 1.000000000000000000 ) ) ;
#24439 = EDGE_CURVE ( 'NONE', #35211, #2161, #62523, .T. ) ;
#24440 = ADVANCED_FACE ( 'NONE', ( #15917 ), #77225, .F. ) ;
#24441 = FACE_OUTER_BOUND ( 'NONE', #50304, .T. ) ;
#24442 = DIRECTION ( 'NONE',  ( -1.000000000000000000, 0.000000000000000000, 0.000000000000000000 ) ) ;
#24443 = CARTESIAN_POINT ( 'NONE',  ( -4.170157060006060235, 26.08383846222962177, -10.00000000000000000 ) ) ;
#24444 = CARTESIAN_POINT ( 'NONE',  ( 178.4695799393319078, 261.1737003364913221, 12.23121311639275888 ) ) ;
#24445 = CARTESIAN_POINT ( 'NONE',  ( 118.5773942495489166, 239.2677522451418497, 10.00000000000009592 ) ) ;
#24446 = CARTESIAN_POINT ( 'NONE',  ( 45.44687632901609931, 27.20801979619932709, -3.090169943749474069 ) ) ;
#24447 = EDGE_LOOP ( 'NONE', ( #93056, #65035 ) ) ;
#24448 = CARTESIAN_POINT ( 'NONE',  ( 190.0515794655415789, 301.4680036374047063, -1.296825456579539626 ) ) ;
#24449 = CARTESIAN_POINT ( 'NONE',  ( 37.27951979288245354, 183.1423013555409796, -4.594050593750043987 ) ) ;
#24450 = CARTESIAN_POINT ( 'NONE',  ( 16.96546585850747491, 10.76426979415088603, 3.090169943749476733 ) ) ;
#24451 = CARTESIAN_POINT ( 'NONE',  ( 77.13473189285724629, 50.76288165847083178, -15.86405702230585213 ) ) ;
#24452 = FACE_OUTER_BOUND ( 'NONE', #64344, .T. ) ;
#24453 = CARTESIAN_POINT ( 'NONE',  ( 71.81468377527440339, 71.89775840070207380, 2.890995686414929544 ) ) ;
#24455 = CARTESIAN_POINT ( 'NONE',  ( 62.64658692180388755, 213.6427522451419065, -10.00000000000009415 ) ) ;
#24454 = CARTESIAN_POINT ( 'NONE',  ( 193.8354046899084153, 268.4885937380259406, 12.87375928640720524 ) ) ;
#24456 = CARTESIAN_POINT ( 'NONE',  ( 5.363317384539951327, 21.83478043621385822, -8.090169943749479842 ) ) ;
#24457 = CARTESIAN_POINT ( 'NONE',  ( 184.6285283030370863, 257.2480713052503916, 1.399339441625289560 ) ) ;
#24458 = CARTESIAN_POINT ( 'NONE',  ( 175.1378461883211912, 279.3152656845848583, 16.63146252814350134 ) ) ;
#24459 = CARTESIAN_POINT ( 'NONE',  ( 162.1895243271695790, 251.7827224420559560, -12.96073478808974144 ) ) ;
#24460 = ORIENTED_EDGE ( 'NONE', *, *, #34805, .F. ) ;
#24461 = EDGE_CURVE ( 'NONE', #32812, #56545, #11791, .T. ) ;
#24462 = CARTESIAN_POINT ( 'NONE',  ( 161.7897299554012136, 267.2878364038729160, 16.48459245643600113 ) ) ;
#24463 = CARTESIAN_POINT ( 'NONE',  ( 34.30229714732369217, 180.6115022471902023, -5.000000000000041744 ) ) ;
#24464 = CARTESIAN_POINT ( 'NONE',  ( 152.3797953885492973, 246.5327760586659451, 1.948934522072303157E-15 ) ) ;
#24465 = CARTESIAN_POINT ( 'NONE',  ( 202.2773826701151165, 280.2922913237452462, 16.62862787739668846 ) ) ;
#24466 = CARTESIAN_POINT ( 'NONE',  ( -10.59588092978231266, 170.8149278399160949, -9.188101187500095079 ) ) ;
#24467 = CARTESIAN_POINT ( 'NONE',  ( 29.36891313204580456, 35.14336893147757479, 7.433330006724141015 ) ) ;
#24468 = CARTESIAN_POINT ( 'NONE',  ( 170.3726117846000534, 263.6551374743509655, 15.82174270005026706 ) ) ;
#24469 = CARTESIAN_POINT ( 'NONE',  ( 185.3682712903229515, 260.2001122261074784, 7.152103282995272870 ) ) ;
#24470 = CARTESIAN_POINT ( 'NONE',  ( 164.3493441216711517, 245.9855811210807417, 1.722120810491653664 ) ) ;
#24471 = CARTESIAN_POINT ( 'NONE',  ( 183.6513914873445117, 258.0677590912166579, -2.301000200388038763 ) ) ;
#24472 = ADVANCED_FACE ( 'NONE', ( #16419 ), #32112, .T. ) ;
#24473 = CARTESIAN_POINT ( 'NONE',  ( 66.23268198520062811, 69.13923810758623745, 2.551101940990796901 ) ) ;
#24474 = ORIENTED_EDGE ( 'NONE', *, *, #26705, .F. ) ;
#24475 = CARTESIAN_POINT ( 'NONE',  ( 174.6066048939933921, 262.0940252294753918, 15.79829227059981278 ) ) ;
#24476 = CARTESIAN_POINT ( 'NONE',  ( 3.154811933878272523, 22.79752408145590081, -5.678558825948271327 ) ) ;
#24477 = CARTESIAN_POINT ( 'NONE',  ( 153.1483233301889015, 277.9035912389402938, -6.076691557333878002 ) ) ;
#24478 = CARTESIAN_POINT ( 'NONE',  ( 13.18987451683679524, 19.56628583063839244, 9.188101187500006262 ) ) ;
#24479 = CARTESIAN_POINT ( 'NONE',  ( -19.65312891409030271, 93.06504152958497400, 177.5919119679930134 ) ) ;
#24480 = EDGE_CURVE ( 'NONE', #73115, #39719, #23966, .T. ) ;
#24481 = CARTESIAN_POINT ( 'NONE',  ( 206.0870578475358172, 273.6937403561189512, -10.07771901274806581 ) ) ;
#24482 = DIRECTION ( 'NONE',  ( -0.8660254037844387076, -0.4999999999999998890, -0.000000000000000000 ) ) ;
#24483 = DIRECTION ( 'NONE',  ( -0.000000000000000000, -0.000000000000000000, -1.000000000000000000 ) ) ;
#24484 = CARTESIAN_POINT ( 'NONE',  ( 191.5950718126193806, 298.2341233548021933, 8.974193154413244500 ) ) ;
#24485 = LINE ( 'NONE', #71611, #58200 ) ;
#24486 = AXIS2_PLACEMENT_3D ( 'NONE', #99117, #29699, #45388 ) ;
#24487 = CARTESIAN_POINT ( 'NONE',  ( 155.2098048002210930, 261.8157275836062468, 16.98811268941991059 ) ) ;
#24488 = ORIENTED_EDGE ( 'NONE', *, *, #67135, .T. ) ;
#24489 = VERTEX_POINT ( 'NONE', #7321 ) ;
#24490 = CARTESIAN_POINT ( 'NONE',  ( -54.45295541630240166, 33.76759809053437067, -10.00000000000000000 ) ) ;
#24491 = CARTESIAN_POINT ( 'NONE',  ( 72.83836408177631938, 70.83590621374696639, 7.219044590757257573 ) ) ;
#24492 = ORIENTED_EDGE ( 'NONE', *, *, #63979, .F. ) ;
#24493 = CARTESIAN_POINT ( 'NONE',  ( 162.7200750364849284, 284.8437062156138495, 3.896873972031206446 ) ) ;
#24494 = DIRECTION ( 'NONE',  ( -1.000000000000000000, 0.000000000000000000, 0.000000000000000000 ) ) ;
#24495 = ORIENTED_EDGE ( 'NONE', *, *, #91136, .F. ) ;
#24496 = FACE_OUTER_BOUND ( 'NONE', #78488, .T. ) ;
#24497 = CARTESIAN_POINT ( 'NONE',  ( 79.28302063466352934, 59.54490948036853126, -16.53220260971269795 ) ) ;
#24498 = CARTESIAN_POINT ( 'NONE',  ( 196.5114383562724072, 290.2791998289336561, -17.87308875047256862 ) ) ;
#24499 = CARTESIAN_POINT ( 'NONE',  ( 10.53464200728543254, 29.58029201028040944, 1.583844403245363353 ) ) ;
#24500 = ORIENTED_EDGE ( 'NONE', *, *, #68305, .F. ) ;
#24501 = CARTESIAN_POINT ( 'NONE',  ( 161.1611771195837548, 251.5076483517112536, 14.17749514252127163 ) ) ;
#24502 = LINE ( 'NONE', #54896, #7367 ) ;
#24503 = CARTESIAN_POINT ( 'NONE',  ( 151.4327733764141612, 268.3577379114237829, 14.90862905801242100 ) ) ;
#24504 = LINE ( 'NONE', #24998, #38015 ) ;
#24505 = ORIENTED_EDGE ( 'NONE', *, *, #37368, .F. ) ;
#24506 = VERTEX_POINT ( 'NONE', #18443 ) ;
#24507 = VERTEX_POINT ( 'NONE', #2749 ) ;
#24508 = CARTESIAN_POINT ( 'NONE',  ( 80.05911005159690319, 45.70205177477036074, 12.00129917442164285 ) ) ;
#24509 = VERTEX_POINT ( 'NONE', #64026 ) ;
#24510 = DIRECTION ( 'NONE',  ( 0.000000000000000000, -0.6050222638427519284, -0.7962085532412920275 ) ) ;
#24511 = ORIENTED_EDGE ( 'NONE', *, *, #79150, .T. ) ;
#24512 = CARTESIAN_POINT ( 'NONE',  ( 208.3152833949211526, 269.8343404973242059, 2.763633873278860342 ) ) ;
#24513 = CARTESIAN_POINT ( 'NONE',  ( 81.98024531596684028, 45.55728866792462384, 10.93523696988690830 ) ) ;
#24514 = CARTESIAN_POINT ( 'NONE',  ( 168.8557204221072539, 272.7203768975772959, 16.03607575273253971 ) ) ;
#24516 = EDGE_CURVE ( 'NONE', #7077, #82637, #57919, .T. ) ;
#24515 = CARTESIAN_POINT ( 'NONE',  ( 205.8889072768004951, 273.5716727396786041, -9.812782715980612025 ) ) ;
#24517 = CARTESIAN_POINT ( 'NONE',  ( 194.8598199529639317, 293.1398868181796615, -15.91766051364927570 ) ) ;
#24518 = CARTESIAN_POINT ( 'NONE',  ( 82.66149664020484522, 53.53843108144140928, -15.73363621927587097 ) ) ;
#24519 = LINE ( 'NONE', #70108, #78996 ) ;
#24520 = CARTESIAN_POINT ( 'NONE',  ( 167.1168391014803376, 246.9550111041327796, 1.953063234077585086 ) ) ;
#24521 = CARTESIAN_POINT ( 'NONE',  ( 21.52536902826200915, 24.37878583063841376, 9.188101187500006262 ) ) ;
#24522 = CARTESIAN_POINT ( 'NONE',  ( 189.6768609436964539, 274.4077930505946483, -17.07046811116321550 ) ) ;
#24523 = CARTESIAN_POINT ( 'NONE',  ( -22.42236680055709641, 157.8615022471902591, 0.000000000000000000 ) ) ;
#24525 = EDGE_LOOP ( 'NONE', ( #67490, #27853, #71668, #70362, #19219, #27737, #75345, #85335 ) ) ;
#24524 = CARTESIAN_POINT ( 'NONE',  ( 207.0336018875206605, 271.6198296197399031, 5.247267533735946898 ) ) ;
#24526 = DIRECTION ( 'NONE',  ( -0.8660254037844387076, -0.4999999999999998890, -0.000000000000000000 ) ) ;
#24527 = CARTESIAN_POINT ( 'NONE',  ( 168.2539250261779955, 257.0764780862120347, -14.46934504387492559 ) ) ;
#24528 = CARTESIAN_POINT ( 'NONE',  ( 159.8946522441011382, 253.7013337850969492, -16.68230890105693121 ) ) ;
#24529 = CARTESIAN_POINT ( 'NONE',  ( 45.19716250472275476, 70.24742367233086782, -10.00000000000000000 ) ) ;
#24530 = CARTESIAN_POINT ( 'NONE',  ( 45.19716250472276187, 70.24742367233086782, -10.00000000000000000 ) ) ;
#24531 = CYLINDRICAL_SURFACE ( 'NONE', #45029, 10.00000000000001066 ) ;
#24532 = ORIENTED_EDGE ( 'NONE', *, *, #97966, .F. ) ;
#24533 = CARTESIAN_POINT ( 'NONE',  ( 193.8431759644069530, 294.9007658595700150, -14.61944437866594093 ) ) ;
#24534 = CARTESIAN_POINT ( 'NONE',  ( 74.98927683103343611, 66.88159155676943612, -13.20077067326868381 ) ) ;
#24535 = CARTESIAN_POINT ( 'NONE',  ( 164.9779129355220562, 244.8968679994381148, -1.771286574179712803 ) ) ;
#24536 = CARTESIAN_POINT ( 'NONE',  ( 19.41748551623073027, 172.0177522451417929, 5.000000000000051514 ) ) ;
#24537 = CARTESIAN_POINT ( 'NONE',  ( 83.80088808272149947, 225.3149278399160949, 9.188101187500093303 ) ) ;
#24538 = EDGE_CURVE ( 'NONE', #65750, #14428, #33640, .T. ) ;
#24539 = CARTESIAN_POINT ( 'NONE',  ( 82.14417565007086353, 40.79354657814926099, -1.097195410270651816 ) ) ;
#24540 = CARTESIAN_POINT ( 'NONE',  ( 167.9211111253673323, 249.4040118433879627, 8.061254949035708606 ) ) ;
#24541 = CARTESIAN_POINT ( 'NONE',  ( 166.9589859915207626, 278.2346298421052779, -13.39139289067553307 ) ) ;
#24543 = CARTESIAN_POINT ( 'NONE',  ( 75.52144112198921277, 65.39696173216708530, 13.85314077474386707 ) ) ;
#24542 = CARTESIAN_POINT ( 'NONE',  ( 3.882894515797516988, 182.2369531367911009, -4.594050593750048428 ) ) ;
#24544 = CARTESIAN_POINT ( 'NONE',  ( 161.1089126327036354, 251.5981730984191529, 13.95161017039218976 ) ) ;
#24545 = EDGE_LOOP ( 'NONE', ( #81624, #4991, #12423, #59377 ) ) ;
#24546 = ORIENTED_EDGE ( 'NONE', *, *, #90879, .F. ) ;
#24547 = DIRECTION ( 'NONE',  ( -0.000000000000000000, -0.000000000000000000, 1.000000000000000000 ) ) ;
#24548 = DIRECTION ( 'NONE',  ( 0.8660254037844387076, 0.4999999999999998890, 0.000000000000000000 ) ) ;
#24549 = EDGE_CURVE ( 'NONE', #83565, #44311, #88898, .T. ) ;
#24550 = CARTESIAN_POINT ( 'NONE',  ( -57.46197106626857476, 34.15416430719361784, 177.5919119679930134 ) ) ;
#24551 = EDGE_CURVE ( 'NONE', #47570, #53490, #11842, .T. ) ;
#24552 = CARTESIAN_POINT ( 'NONE',  ( 84.86883313302882925, 45.02243900927756215, 8.511842229617958111 ) ) ;
#24553 = LINE ( 'NONE', #64570, #99677 ) ;
#24554 = DIRECTION ( 'NONE',  ( 0.000000000000000000, 0.000000000000000000, 1.000000000000000000 ) ) ;
#24555 = CARTESIAN_POINT ( 'NONE',  ( 74.34754423757576092, 68.44411287762122242, -11.23027362005041319 ) ) ;
#24556 = CARTESIAN_POINT ( 'NONE',  ( 27.23877744593285755, 186.5333772461660544, 9.188101187500095079 ) ) ;
#24557 = CARTESIAN_POINT ( 'NONE',  ( 75.70913676221920241, 214.5177522451418497, -10.00000000000009592 ) ) ;
#24558 = CARTESIAN_POINT ( 'NONE',  ( 74.81832046901195099, 67.48663194201290594, -12.71244991431774984 ) ) ;
#24559 = ORIENTED_EDGE ( 'NONE', *, *, #83954, .F. ) ;
#24560 = CARTESIAN_POINT ( 'NONE',  ( 81.52469153597657225, 59.51941083166271795, 0.2499999999999960032 ) ) ;
#24561 = DIRECTION ( 'NONE',  ( 0.5000000000000048850, -0.8660254037844358210, 0.000000000000000000 ) ) ;
#24562 = CYLINDRICAL_SURFACE ( 'NONE', #86341, 14.21260523776213347 ) ;
#24563 = CARTESIAN_POINT ( 'NONE',  ( 199.0805333989439134, 267.9591265660101271, 8.967019654618759716 ) ) ;
#24564 = CARTESIAN_POINT ( 'NONE',  ( 194.4889937320412230, 293.7821766735966662, 14.99892588346621380 ) ) ;
#24565 = CARTESIAN_POINT ( 'NONE',  ( 161.3145230519951951, 251.2420454056404822, -14.44869077440025151 ) ) ;
#24566 = CARTESIAN_POINT ( 'NONE',  ( 186.1229685699691458, 283.4085544576373081, 17.19819074553363336 ) ) ;
#24567 = CARTESIAN_POINT ( 'NONE',  ( 147.9791529310278122, 274.3395839928920168, -7.789432462804474433 ) ) ;
#24568 = CARTESIAN_POINT ( 'NONE',  ( 192.0985965716629096, 264.9293924627144747, 7.771810996922307702 ) ) ;
#24569 = CARTESIAN_POINT ( 'NONE',  ( 171.7318633942313681, 279.6244332910715116, 14.38819572014175030 ) ) ;
#24570 = CARTESIAN_POINT ( 'NONE',  ( 176.1037769756363218, 256.5739391985542852, -11.09083365203573379 ) ) ;
#24571 = CARTESIAN_POINT ( 'NONE',  ( 147.3047606266276546, 275.5076657283461827, -0.02269072295920609994 ) ) ;
#24572 = CARTESIAN_POINT ( 'NONE',  ( 189.8480911035503880, 301.8204558191226283, -0.8992086515915015399 ) ) ;
#24573 = VERTEX_POINT ( 'NONE', #72660 ) ;
#24574 = B_SPLINE_CURVE_WITH_KNOTS ( 'NONE', 3,
 ( #19769, #58241, #65351, #20766, #5547, #96290, #42533, #13169, #96800, #89702, #50152, #26859, #34939, #20262, #5058, #66841, #35447, #51136, #35938, #4049, #82098, #51654, #89221, #88715, #36432, #4546, #88215, #57735, #44023, #73466, #12671, #73961, #28338, #97282, #66349, #11671, #19284, #67339, #72981, #81104, #43022, #82603, #27359, #97768, #65834, #18767, #59216, #90190, #50638, #27849 ),
 .UNSPECIFIED., .F., .F.,
 ( 4, 2, 2, 2, 2, 2, 2, 2, 2, 2, 2, 2, 2, 2, 2, 2, 2, 2, 2, 2, 2, 2, 2, 2, 4 ),
 ( 0.0005972733594740094231, 0.001599206768350971541, 0.001849690120570192473, 0.002100173472789413406, 0.002225415148898984841, 0.002350656825008556276, 0.002475898501118127711, 0.002601140177227699146, 0.002851623529446945665, 0.003102106881666191751, 0.003603073586104625376, 0.004605006994981492192, 0.005606940403858359442, 0.006107907108296836869, 0.006358390460515996219, 0.006608873812735157303, 0.006671494650789984437, 0.006734115488844811571, 0.006796736326899638705, 0.006859357164954464972, 0.007109840517173513300, 0.007610807221611471177, 0.008111773926049430788, 0.008362257278268407992, 0.008612740630487385196 ),
 .UNSPECIFIED. ) ;
#24575 = CARTESIAN_POINT ( 'NONE',  ( 153.1538868596604175, 267.0205913518451553, -16.30221171337800712 ) ) ;
#24576 = EDGE_CURVE ( 'NONE', #99135, #45081, #1014, .T. ) ;
#24577 = DIRECTION ( 'NONE',  ( 0.5000000000000012212, -0.8660254037844380415, 0.000000000000000000 ) ) ;
#24578 = CARTESIAN_POINT ( 'NONE',  ( 111.6762543149156386, 235.2833772461660544, -9.188101187500095079 ) ) ;
#24579 = CARTESIAN_POINT ( 'NONE',  ( 10.40777469057294091, 26.98502408145591502, -5.678558825948271327 ) ) ;
#24580 = CARTESIAN_POINT ( 'NONE',  ( 151.4384131719918685, 268.3479694989391078, 14.98299707687648841 ) ) ;
#24581 = CYLINDRICAL_SURFACE ( 'NONE', #24150, 10.00000000000010658 ) ;
#24582 = CARTESIAN_POINT ( 'NONE',  ( 157.8360072705708603, 257.2670114739976839, 17.12122855844125269 ) ) ;
#24583 = CARTESIAN_POINT ( 'NONE',  ( 150.8312752086160344, 269.3995632987097224, -13.81131374255177491 ) ) ;
#24584 = CARTESIAN_POINT ( 'NONE',  ( 23.91155070014810136, 29.50829794293881392, -10.00000000000000355 ) ) ;
#24585 = CARTESIAN_POINT ( 'NONE',  ( 149.3629284598386278, 271.9428144707212027, -12.99253781774931049 ) ) ;
#24586 = DIRECTION ( 'NONE',  ( -1.000000000000000000, 4.892646582057217816E-14, 0.000000000000000000 ) ) ;
#24587 = CARTESIAN_POINT ( 'NONE',  ( 203.7562161628329420, 276.6852326455151569, 14.03846531369241646 ) ) ;
#24588 = CARTESIAN_POINT ( 'NONE',  ( 86.13417129343109480, 47.68469467925804395, 10.84946945994417611 ) ) ;
#24589 = ORIENTED_EDGE ( 'NONE', *, *, #50395, .T. ) ;
#24590 = CYLINDRICAL_SURFACE ( 'NONE', #55378, 17.82106496071139645 ) ;
#24591 = AXIS2_PLACEMENT_3D ( 'NONE', #35947, #34945, #66357 ) ;
#24592 = CARTESIAN_POINT ( 'NONE',  ( 179.0770803138376550, 280.8245948471085285, 16.18081609326188897 ) ) ;
#24593 = CARTESIAN_POINT ( 'NONE',  ( 159.3184698695538657, 279.9366817407362191, 9.858215026386687896 ) ) ;
#24594 = EDGE_CURVE ( 'NONE', #49426, #89848, #95977, .T. ) ;
#24595 = VERTEX_POINT ( 'NONE', #33125 ) ;
#24596 = B_SPLINE_SURFACE_WITH_KNOTS ( 'NONE', 3, 1, ( 
 ( #69130, #100059 ),
 ( #30644, #60523 ),
 ( #61531, #23021 ),
 ( #53914, #84875 ),
 ( #732, #68633 ),
 ( #21555, #13950 ),
 ( #15416, #44832 ),
 ( #75765, #38726 ),
 ( #69630, #17957 ),
 ( #25028, #86901 ),
 ( #63532, #80284 ),
 ( #33138, #94474 ),
 ( #54928, #9340 ),
 ( #94983, #17436 ),
 ( #95504, #64038 ),
 ( #49344, #48343 ),
 ( #85906, #62512 ),
 ( #1242, #16432 ),
 ( #40212, #2765 ),
 ( #2256, #47815 ),
 ( #79290, #8833 ),
 ( #9862, #40721 ),
 ( #25544, #63034 ),
 ( #56432, #71666 ),
 ( #55907, #41727 ),
 ( #87427, #39702 ),
 ( #71158, #41219 ),
 ( #1757, #78753 ),
 ( #32636, #48854 ),
 ( #33655, #78253 ),
 ( #93477, #70632 ),
 ( #32125, #24029 ),
 ( #93978, #55411 ),
 ( #79787, #10352 ) ),
 .UNSPECIFIED., .T., .F., .F.,
 ( 4, 2, 2, 2, 2, 2, 2, 2, 2, 2, 2, 2, 2, 2, 2, 2, 4 ),
 ( 2, 2 ),
 ( 0.000000000000000000, 0.06250000000000000000, 0.1250000000000000000, 0.1875000000000000000, 0.2500000000000000000, 0.3125000000000000000, 0.3750000000000000000, 0.4375000000000000000, 0.5000000000000000000, 0.5625000000000000000, 0.6250000000000000000, 0.6875000000000000000, 0.7500000000000000000, 0.8125000000000000000, 0.8750000000000000000, 0.9375000000000000000, 1.000000000000000000 ),
 ( 0.000000000000000000, 1.000000000000000000 ),
 .UNSPECIFIED. ) ;
#24597 = B_SPLINE_CURVE_WITH_KNOTS ( 'NONE', 3,
 ( #97648, #73829, #80474, #35315 ),
 .UNSPECIFIED., .F., .F.,
 ( 4, 4 ),
 ( 0.005858324926681961892, 0.01085025600539994174 ),
 .UNSPECIFIED. ) ;
#24598 = CARTESIAN_POINT ( 'NONE',  ( 78.63094854509681397, 48.18467340716805580, 14.04610061905436424 ) ) ;
#24599 = CARTESIAN_POINT ( 'NONE',  ( 188.8764293144468240, 259.6972905960182061, 3.583694637520717041 ) ) ;
#24600 = DIRECTION ( 'NONE',  ( -0.3213938048432640748, 0.5566703992264119272, -0.7660444431189857850 ) ) ;
#24601 = CARTESIAN_POINT ( 'NONE',  ( 74.97683113034595692, 53.08780515268223610, -16.02469623271439048 ) ) ;
#24602 = CARTESIAN_POINT ( 'NONE',  ( 148.0649146996763363, 274.8219941347795157, 6.013499275595850513 ) ) ;
#24603 = ORIENTED_EDGE ( 'NONE', *, *, #41738, .F. ) ;
#24605 = AXIS2_PLACEMENT_3D ( 'NONE', #83807, #52856, #78173 ) ;
#24604 = DIRECTION ( 'NONE',  ( 0.7162481363636747922, 0.000000000000000000, 0.6978456900745053648 ) ) ;
#24606 = CARTESIAN_POINT ( 'NONE',  ( 40.42517716772906056, 31.84335787977767041, 9.188101187500006262 ) ) ;
#24607 = CARTESIAN_POINT ( 'NONE',  ( 83.33965292895494770, 40.89095863664473995, 0.2909840089494764581 ) ) ;
#24608 = EDGE_LOOP ( 'NONE', ( #45041, #87929, #73483, #10983 ) ) ;
#24609 = CARTESIAN_POINT ( 'NONE',  ( 164.0406800301222461, 279.3727068695090452, 12.06992682371145698 ) ) ;
#24610 = FACE_OUTER_BOUND ( 'NONE', #36574, .T. ) ;
#24611 = CARTESIAN_POINT ( 'NONE',  ( 11.35262394703597977, 187.3615022471903160, 5.000000000000046185 ) ) ;
#24612 = EDGE_LOOP ( 'NONE', ( #70760, #34447, #66251, #63305 ) ) ;
#24613 = CARTESIAN_POINT ( 'NONE',  ( 86.26706070573375484, 46.98025876953199287, -10.04304018679821731 ) ) ;
#24614 = CARTESIAN_POINT ( 'NONE',  ( 188.7896788447123697, 293.5392900447417333, 12.71403846335633503 ) ) ;
#24615 = CARTESIAN_POINT ( 'NONE',  ( 60.96635096964421763, 217.5530062829863027, -4.648177544792955347E-16 ) ) ;
#24616 = CARTESIAN_POINT ( 'NONE',  ( 165.3469776539213001, 255.6859576650746817, 15.29061740545938619 ) ) ;
#24617 = CARTESIAN_POINT ( 'NONE',  ( 121.5128116872495525, 229.4155109091896065, 2.679491924311254714 ) ) ;
#24618 = LINE ( 'NONE', #10433, #75386 ) ;
#24619 = ORIENTED_EDGE ( 'NONE', *, *, #10268, .T. ) ;
#24620 = VERTEX_POINT ( 'NONE', #81268 ) ;
#24621 = CARTESIAN_POINT ( 'NONE',  ( 175.2353567823311948, 258.4903666904938859, 12.97297848141165666 ) ) ;
#24622 = ORIENTED_EDGE ( 'NONE', *, *, #29227, .T. ) ;
#24623 = CARTESIAN_POINT ( 'NONE',  ( 77.25192996872536355, 49.17366000481920452, -15.32849534080991916 ) ) ;
#24625 = ORIENTED_EDGE ( 'NONE', *, *, #20531, .T. ) ;
#24624 = EDGE_CURVE ( 'NONE', #33264, #38319, #4604, .T. ) ;
#24626 = CARTESIAN_POINT ( 'NONE',  ( 74.95592743341377684, 58.52978105962555588, 15.90320610924748301 ) ) ;
#24627 = CARTESIAN_POINT ( 'NONE',  ( 78.35439122558771885, 49.50317310883020383, 14.71240697276643239 ) ) ;
#24628 = ORIENTED_EDGE ( 'NONE', *, *, #51184, .T. ) ;
#24629 = CARTESIAN_POINT ( 'NONE',  ( 182.7519487852241582, 280.2897188732222844, -16.10892874468358116 ) ) ;
#24630 = B_SPLINE_CURVE_WITH_KNOTS ( 'NONE', 3,
 ( #23759, #16174, #20560, #89505 ),
 .UNSPECIFIED., .F., .F.,
 ( 4, 4 ),
 ( 0.03306110125414005868, 0.04197919891026069550 ),
 .UNSPECIFIED. ) ;
#24631 = CARTESIAN_POINT ( 'NONE',  ( 206.1142978005191821, 273.6465593735555899, -11.17423994621995753 ) ) ;
#24632 = CARTESIAN_POINT ( 'NONE',  ( 190.2843330081942099, 301.0648626758887758, 1.921572748488094229 ) ) ;
#24633 = CARTESIAN_POINT ( 'NONE',  ( 196.2637273998480794, 284.5407699133422170, -17.38889955844871338 ) ) ;
#24634 = CARTESIAN_POINT ( 'NONE',  ( 78.87932154437264387, 46.39673357570728029, 12.96173668562228620 ) ) ;
#24636 = ADVANCED_FACE ( 'NONE', ( #95490 ), #17944, .F. ) ;
#24635 = CARTESIAN_POINT ( 'NONE',  ( 180.3459549195497118, 261.9372799863696741, 13.82492882169983872 ) ) ;
#24637 = FACE_OUTER_BOUND ( 'NONE', #90339, .T. ) ;
#24638 = CARTESIAN_POINT ( 'NONE',  ( 153.9013169898294962, 279.6173177660232341, 2.183373660223292934 ) ) ;
#24639 = CARTESIAN_POINT ( 'NONE',  ( 119.6866422041566693, 252.1589784336661637, -6.496448406907675876E-16 ) ) ;
#24640 = CARTESIAN_POINT ( 'NONE',  ( 185.8243919191459099, 262.2525832573476237, -9.042311947975223418 ) ) ;
#24641 = ORIENTED_EDGE ( 'NONE', *, *, #45507, .T. ) ;
#24643 = ORIENTED_EDGE ( 'NONE', *, *, #61740, .F. ) ;
#24642 = CARTESIAN_POINT ( 'NONE',  ( 20.33155438404897808, 35.23654200823202132, 1.583844403245397769 ) ) ;
#24644 = CARTESIAN_POINT ( 'NONE',  ( 74.56414817410228579, 187.8759306620403322, -17.47570218321536473 ) ) ;
#24645 = CARTESIAN_POINT ( 'NONE',  ( -29.31672308591111431, 23.47304723416778316, 10.00000000000000000 ) ) ;
#24646 = FACE_OUTER_BOUND ( 'NONE', #87543, .T. ) ;
#24647 = CARTESIAN_POINT ( 'NONE',  ( 190.4718661473337136, 300.2809275374601725, 2.324064312516258557 ) ) ;
#24648 = CARTESIAN_POINT ( 'NONE',  ( 71.74471703213781382, 60.72069063942237221, 14.83967380431143823 ) ) ;
#24649 = CARTESIAN_POINT ( 'NONE',  ( 159.8822213732012756, 255.7228646850775533, -16.63148941946954196 ) ) ;
#24650 = CARTESIAN_POINT ( 'NONE',  ( 173.6948184163663313, 287.1953014397127504, -9.575283291849126854 ) ) ;
#24652 = CARTESIAN_POINT ( 'NONE',  ( 174.9664910165346328, 282.3800467726322836, 14.52565441293174864 ) ) ;
#24651 = B_SPLINE_CURVE_WITH_KNOTS ( 'NONE', 3,
 ( #72776, #13795, #89019, #34731, #19065, #48949, #65138, #41829, #72264, #10958, #49938, #81386, #2870, #27152, #3368, #33759, #80899, #64650, #58037, #5696, #64139, #11470, #42324, #50431, #11954, #3847, #95600, #90852, #26147, #98421, #56533, #21406, #73253, #52289, #57025, #65630, #42812, #44674, #75120, #88007, #34242, #6195, #96086, #67491, #29014, #59886, #75607, #95089 ),
 .UNSPECIFIED., .F., .F.,
 ( 4, 2, 2, 2, 2, 2, 2, 2, 2, 2, 2, 2, 2, 2, 2, 2, 2, 2, 2, 2, 2, 2, 2, 4 ),
 ( 0.001944024153977080144, 0.002388868632841927454, 0.002611290872274335713, 0.002833713111706743538, 0.002944924231422909287, 0.003056135351139075904, 0.003167346470855241652, 0.003278557590571408269, 0.003500979830003698133, 0.003723402069435987997, 0.004613091027165332203, 0.005502779984894675541, 0.006392468942624018879, 0.006837313421488733049, 0.007282157900353448086, 0.007393369020069691898, 0.007448974579927781711, 0.007504580139785870657, 0.007615791259502062427, 0.007727002379218254197, 0.008171846858083097603, 0.008394269097515514103, 0.008616691336947932336, 0.009061535815812862479 ),
 .UNSPECIFIED. ) ;
#24653 = CARTESIAN_POINT ( 'NONE',  ( 194.7312017232699475, 291.7187946681755761, 16.04046780675849604 ) ) ;
#24654 = VERTEX_POINT ( 'NONE', #96469 ) ;
#24655 = CARTESIAN_POINT ( 'NONE',  ( 148.2670916631250861, 273.8408594794321971, -7.980554973576580835 ) ) ;
#24656 = CARTESIAN_POINT ( 'NONE',  ( 149.8083888948594335, 271.5779462620446338, 11.70101749353969645 ) ) ;
#24657 = VERTEX_POINT ( 'NONE', #41206 ) ;
#24658 = CARTESIAN_POINT ( 'NONE',  ( 189.1549977934801632, 266.7951475240158175, -11.86923019693644576 ) ) ;
#24659 = B_SPLINE_CURVE_WITH_KNOTS ( 'NONE', 3,
 ( #22303, #38487, #47094, #68398, #37489, #84158, #30401, #85144, #38987, #21805, #14704, #15690 ),
 .UNSPECIFIED., .F., .F.,
 ( 4, 2, 2, 2, 2, 4 ),
 ( 0.001501127264142293862, 0.001572989943943600049, 0.001644852623744906019, 0.001788577983347369423, 0.002076028702552448237, 0.002650930140962551654 ),
 .UNSPECIFIED. ) ;
#24660 = CARTESIAN_POINT ( 'NONE',  ( 160.0256511895230460, 279.1764180042833345, 10.79622904626536695 ) ) ;
#24661 = CARTESIAN_POINT ( 'NONE',  ( 152.2282464967177873, 266.9799380510025912, -15.44817667187453658 ) ) ;
#24662 = CARTESIAN_POINT ( 'NONE',  ( -40.42249077443059235, 27.53003111760058630, 10.00000000000000000 ) ) ;
#24663 = CARTESIAN_POINT ( 'NONE',  ( 81.13608137687064925, 42.60696278352305200, 7.988320930663086905 ) ) ;
#24665 = CARTESIAN_POINT ( 'NONE',  ( 151.5210055037418613, 275.0213185945912642, -8.640155065745233287 ) ) ;
#24664 = CARTESIAN_POINT ( 'NONE',  ( 164.6777298217157579, 283.8828607077460333, -6.799046367663557966 ) ) ;
#24666 = AXIS2_PLACEMENT_3D ( 'NONE', #89703, #20263, #66842 ) ;
#24667 = CARTESIAN_POINT ( 'NONE',  ( 48.87252615048947035, 107.3561085985703016, -10.00000000000000000 ) ) ;
#24668 = VERTEX_POINT ( 'NONE', #25015 ) ;
#24669 = CARTESIAN_POINT ( 'NONE',  ( 204.6823371430232896, 272.9704135290961062, -9.754921121218281144 ) ) ;
#24670 = CARTESIAN_POINT ( 'NONE',  ( 187.5160213568918834, 263.2186159667169818, -9.042077419483060652 ) ) ;
#24671 = PLANE ( 'NONE',  #81412 ) ;
#24672 = CARTESIAN_POINT ( 'NONE',  ( 87.85430303351097336, 43.89859490532884223, 0.3596698246726173775 ) ) ;
#24673 = EDGE_CURVE ( 'NONE', #80596, #84236, #55354, .T. ) ;
#24674 = CARTESIAN_POINT ( 'NONE',  ( 4.695053651895191749, 183.5177522451419350, 5.000000000000046185 ) ) ;
#24675 = CARTESIAN_POINT ( 'NONE',  ( 152.6845319923753834, 266.1896283897672220, 17.20844521882669653 ) ) ;
#24676 = EDGE_CURVE ( 'NONE', #70726, #2112, #90128, .T. ) ;
#24677 = CARTESIAN_POINT ( 'NONE',  ( 74.01669459151050035, 68.61891074470059948, 11.40943161386742233 ) ) ;
#24678 = CARTESIAN_POINT ( 'NONE',  ( 69.47607923203149483, 70.76119968013694006, -0.4672567883698480751 ) ) ;
#24679 = CARTESIAN_POINT ( 'NONE',  ( -4.289699588770600869, 159.1423013555410080, -4.594050593750043987 ) ) ;
#24680 = EDGE_CURVE ( 'NONE', #81902, #49338, #33019, .T. ) ;
#24681 = CARTESIAN_POINT ( 'NONE',  ( 91.10780387927019319, 235.6589784336661353, -6.496448406907675876E-16 ) ) ;
#24682 = CARTESIAN_POINT ( 'NONE',  ( 41.54267820409027223, 208.0707943907112565, 17.97570218321537538 ) ) ;
#24683 = CARTESIAN_POINT ( 'NONE',  ( 88.14071703455390150, 44.55363679567808788, -5.002659464432036351 ) ) ;
#24684 = CARTESIAN_POINT ( 'NONE',  ( 182.9336300665386830, 294.1347523882549808, -7.906671405285472076 ) ) ;
#24685 = EDGE_CURVE ( 'NONE', #67744, #41262, #18947, .T. ) ;
#24686 = CARTESIAN_POINT ( 'NONE',  ( 78.42360325331485171, 47.41383149739777281, 14.26703730024508054 ) ) ;
#24687 = DIRECTION ( 'NONE',  ( 0.06415622980647761597, -0.9979398670145503969, 0.000000000000000000 ) ) ;
#24688 = CARTESIAN_POINT ( 'NONE',  ( 38.47004439948830168, 203.0177522451419350, 5.000000000000046185 ) ) ;
#24690 = CARTESIAN_POINT ( 'NONE',  ( 76.35458056077806077, 51.11712984296273277, 16.05186526122436064 ) ) ;
#24689 = CARTESIAN_POINT ( 'NONE',  ( -110.0000000000000142, -8.000000000000000000, 9.212605237762145904 ) ) ;
#24691 = CARTESIAN_POINT ( 'NONE',  ( 161.3809022727548950, 251.1270732227178826, 12.88239761679595219 ) ) ;
#24692 = CARTESIAN_POINT ( 'NONE',  ( -7.501470784735642106, 173.1427522451419350, -10.00000000000009592 ) ) ;
#24693 = SURFACE_STYLE_USAGE ( .BOTH. , #87581 ) ;
#24694 = CARTESIAN_POINT ( 'NONE',  ( 196.4677102463732012, 290.3549391369982686, 16.45225250689336249 ) ) ;
#24695 = DIRECTION ( 'NONE',  ( 0.000000000000000000, 0.000000000000000000, 1.000000000000000000 ) ) ;
#24696 = CARTESIAN_POINT ( 'NONE',  ( 72.73719086776743836, 57.26489226207078787, -15.87218763176317537 ) ) ;
#24697 = B_SPLINE_CURVE_WITH_KNOTS ( 'NONE', 3,
 ( #63210, #23691, #76902, #61697, #24705, #39883, #70819, #55097, #7500, #24216, #75062, #46493, #54588, #55588, #100232, #98365, #67434, #77429, #44619, #93652, #92649, #93141, #38900, #54090, #47012, #1427, #8027, #28953, #69311, #85570, #5639, #36532, #86084, #86571, #16608, #32308, #21349, #47504, #52234, #69804, #83178, #31303, #78431, #9011, #94152, #30817, #31793, #62191, #72340, #9532, #2946, #58105 ),
 .UNSPECIFIED., .F., .F.,
 ( 4, 2, 2, 2, 2, 2, 2, 2, 2, 2, 2, 2, 2, 2, 2, 2, 2, 2, 2, 2, 2, 2, 2, 2, 2, 4 ),
 ( 0.0007535677484271811411, 0.0009585266667888987444, 0.001061006125969736784, 0.001163485585150574823, 0.001265965044331413079, 0.001368444503512250901, 0.001573403421873828534, 0.001983321258597046249, 0.002393239095320263531, 0.003213074768766698095, 0.004032910442213133093, 0.004852746115659568524, 0.005262663952382786239, 0.005467622870744357801, 0.005570102329925144015, 0.005621342059515537122, 0.005672581789105929362, 0.005723821518696322469, 0.005775061248286715576, 0.005877540707467618884, 0.006082499625829548666, 0.006287458544191479315, 0.006492417462553409097, 0.006697376380915339746, 0.006902335299277270395, 0.007312253136001233174 ),
 .UNSPECIFIED. ) ;
#24698 = CARTESIAN_POINT ( 'NONE',  ( 41.69040282370318096, 201.0024278399160664, -9.188101187500093303 ) ) ;
#24699 = CARTESIAN_POINT ( 'NONE',  ( 58.76725448063633195, 213.9244531367911577, -4.594050593750046652 ) ) ;
#24700 = CARTESIAN_POINT ( 'NONE',  ( -89.11465314115665137, 93.37593066204027537, 37.50000000000002132 ) ) ;
#24701 = CARTESIAN_POINT ( 'NONE',  ( 88.26944586016423955, 44.13856730148188490, 0.4509010169863623685 ) ) ;
#24702 = CARTESIAN_POINT ( 'NONE',  ( 167.2670237296246114, 259.8210226229481350, 16.08327144298513289 ) ) ;
#24704 = CARTESIAN_POINT ( 'NONE',  ( 67.65279290918169863, 70.10559244845448745, -1.558233695405924601 ) ) ;
#24703 = CARTESIAN_POINT ( 'NONE',  ( 198.5718581478091096, 286.2919326846333661, -17.01494721233840934 ) ) ;
#24705 = CARTESIAN_POINT ( 'NONE',  ( 200.1987971015728078, 270.8785103762743915, -11.50719176782677522 ) ) ;
#24706 = CARTESIAN_POINT ( 'NONE',  ( 32.17146729527596705, 24.28920272979928541, -7.433330006724141015 ) ) ;
#24707 = CARTESIAN_POINT ( 'NONE',  ( 198.5954523381739989, 286.6695817285962562, -18.45134152028667174 ) ) ;
#24708 = CARTESIAN_POINT ( 'NONE',  ( 82.49298411987194868, 47.17765150883158753, -12.09122284588559992 ) ) ;
#24709 = CARTESIAN_POINT ( 'NONE',  ( 7.290083236948966317, 25.18502408145589655, 5.678558825948277544 ) ) ;
#24710 = CARTESIAN_POINT ( 'NONE',  ( 64.04520420253652446, 195.5327760586659451, 1.948934522072302763E-15 ) ) ;
#24711 = DIRECTION ( 'NONE',  ( 0.8660254037844377084, 0.5000000000000015543, -0.000000000000000000 ) ) ;
#24712 = FACE_OUTER_BOUND ( 'NONE', #57399, .T. ) ;
#24713 = CARTESIAN_POINT ( 'NONE',  ( 159.3767386493506137, 254.5983864451355032, 15.47015898230477760 ) ) ;
#24714 = CARTESIAN_POINT ( 'NONE',  ( -50.03504209260853486, 51.19473430114911139, 59.99999999999999289 ) ) ;
#24715 = CARTESIAN_POINT ( 'NONE',  ( 153.7598317759031374, 264.3271545313291426, 16.52601577908147235 ) ) ;
#24716 = CARTESIAN_POINT ( 'NONE',  ( 81.85713351507602908, 54.37717625304360070, -15.69185593827182856 ) ) ;
#24718 =( BOUNDED_CURVE ( )  B_SPLINE_CURVE ( 2, ( #11723, #35500, #65895, #27418, #80656, #34993, #80154, #73032, #43076 ),
 .UNSPECIFIED., .F., .T. ) 
 B_SPLINE_CURVE_WITH_KNOTS ( ( 3, 2, 2, 2, 3 ),
 ( 0.8830645161290322509, 0.8844086021505376261, 0.8870967741935483764, 0.8897849462365591267, 0.8911290322580645018 ),
 .UNSPECIFIED. ) 
 CURVE ( )  GEOMETRIC_REPRESENTATION_ITEM ( )  RATIONAL_B_SPLINE_CURVE ( ( 0.9330127018922194093, 0.9330127018922194093, 1.000000000000000000, 0.8660254037844387076, 1.000000000000000000, 0.8660254037844387076, 1.000000000000000000, 0.9330127018922194093, 0.9330127018922194093 ) ) 
 REPRESENTATION_ITEM ( '' )  );
#24717 = CARTESIAN_POINT ( 'NONE',  ( 113.5436215935997808, 236.3615022471902307, -10.00000000000009592 ) ) ;
#24719 = LINE ( 'NONE', #39403, #52287 ) ;
#24720 = CARTESIAN_POINT ( 'NONE',  ( 164.8251969117060298, 245.1613799118173063, -1.508678420156898348 ) ) ;
#24721 = ORIENTED_EDGE ( 'NONE', *, *, #8927, .F. ) ;
#24722 = CARTESIAN_POINT ( 'NONE',  ( 77.45085267822321384, 49.21833083662652086, 15.30297809502122952 ) ) ;
#24723 = CARTESIAN_POINT ( 'NONE',  ( 187.7017978076716815, 273.1500586230484373, 15.64325622808618732 ) ) ;
#24724 = ORIENTED_EDGE ( 'NONE', *, *, #70913, .T. ) ;
#24725 = CARTESIAN_POINT ( 'NONE',  ( 159.2536436069973718, 254.8115933126508992, -15.76697951715411250 ) ) ;
#24726 = CARTESIAN_POINT ( 'NONE',  ( 186.9535536427556508, 276.6359796364028512, -17.38156364443241841 ) ) ;
#24727 = CARTESIAN_POINT ( 'NONE',  ( 70.42716005707438853, 68.90180154463854478, -7.919248421219340806 ) ) ;
#24728 = ORIENTED_EDGE ( 'NONE', *, *, #90732, .F. ) ;
#24729 = CARTESIAN_POINT ( 'NONE',  ( 177.2873494991416408, 253.1734583796121854, -0.2633482349297172065 ) ) ;
#24730 = VERTEX_POINT ( 'NONE', #73147 ) ;
#24731 = CARTESIAN_POINT ( 'NONE',  ( 65.86957007823072274, 68.92796865271058948, -2.560965087547883989 ) ) ;
#24732 = CARTESIAN_POINT ( 'NONE',  ( 194.3177355571849318, 294.0788045336591381, -15.93712594727561616 ) ) ;
#24733 = CARTESIAN_POINT ( 'NONE',  ( 164.3625597711517230, 265.6729452914248668, -17.82104740451561753 ) ) ;
#24734 = EDGE_CURVE ( 'NONE', #29494, #87383, #3743, .T. ) ;
#24735 = CIRCLE ( 'NONE', #53782, 7.499999999999996447 ) ;
#24736 = ORIENTED_EDGE ( 'NONE', *, *, #44896, .T. ) ;
#24737 = CARTESIAN_POINT ( 'NONE',  ( 21.59633513308047270, 30.65586893147756697, -7.433330006724137462 ) ) ;
#24738 = CARTESIAN_POINT ( 'NONE',  ( 79.85812127980112507, 44.70746904388536791, 11.25005473392974054 ) ) ;
#24739 = CARTESIAN_POINT ( 'NONE',  ( 30.81219509745235285, 177.0494855054051584, -2.679491924311248496 ) ) ;
#24740 = CARTESIAN_POINT ( 'NONE',  ( 74.98927683103342190, 66.88159155676945034, -13.20077067326868558 ) ) ;
#24741 = CARTESIAN_POINT ( 'NONE',  ( 80.92877085092437994, 48.89368045554081021, -13.76466174163450340 ) ) ;
#24742 = VECTOR ( 'NONE', #49001, 1000.000000000000000 ) ;
#24743 = VERTEX_POINT ( 'NONE', #19460 ) ;
#24744 = LINE ( 'NONE', #86608, #2922 ) ;
#24745 = CARTESIAN_POINT ( 'NONE',  ( -11.66375754446418611, 175.6199935810941213, 2.679491924311258266 ) ) ;
#24746 = ORIENTED_EDGE ( 'NONE', *, *, #10004, .F. ) ;
#24747 = CARTESIAN_POINT ( 'NONE',  ( 171.0749840207226384, 284.6259473909062194, 10.82415887584089020 ) ) ;
#24749 = CARTESIAN_POINT ( 'NONE',  ( 68.33938886113043054, 65.68960829769598320, -10.35387598406562226 ) ) ;
#24748 = CARTESIAN_POINT ( 'NONE',  ( 67.77383089997810828, 65.57049627815092663, 10.14032301746840403 ) ) ;
#24750 = CARTESIAN_POINT ( 'NONE',  ( 81.71195745382044606, 55.24878511337072950, -15.91731695540261171 ) ) ;
#24751 = CARTESIAN_POINT ( 'NONE',  ( 154.8679462054080318, 262.4078440388265676, 17.98338675682672871 ) ) ;
#24752 = CARTESIAN_POINT ( 'NONE',  ( 185.3899931942047772, 292.5462500827383110, -10.78127527295067800 ) ) ;
#24753 = CARTESIAN_POINT ( 'NONE',  ( 157.8696211474012330, 257.2087905314882619, -17.27527248276125604 ) ) ;
#24754 = CARTESIAN_POINT ( 'NONE',  ( 143.8006444583684242, 244.6423013555409796, -4.594050593750043987 ) ) ;
#24755 = CARTESIAN_POINT ( 'NONE',  ( 206.4640281649579947, 270.6250285429839550, 2.495114648528401258 ) ) ;
#24756 = VECTOR ( 'NONE', #47897, 1000.000000000000114 ) ;
#24757 = CARTESIAN_POINT ( 'NONE',  ( 79.01330593081745235, 59.80254073573071594, 16.49416071572547793 ) ) ;
#24758 = CARTESIAN_POINT ( 'NONE',  ( 83.80088808272151368, 225.3149278399160949, 9.188101187500093303 ) ) ;
#24759 = VERTEX_POINT ( 'NONE', #50316 ) ;
#24760 = CARTESIAN_POINT ( 'NONE',  ( 151.0778907302193943, 268.9724126853576536, 15.84769371787143832 ) ) ;
#24761 = CARTESIAN_POINT ( 'NONE',  ( 78.15719359349522222, 61.55473184547404486, -16.14768920957587284 ) ) ;
#24762 = ORIENTED_EDGE ( 'NONE', *, *, #50252, .T. ) ;
#24763 = CARTESIAN_POINT ( 'NONE',  ( 156.7217004655723258, 259.1970474754747897, -17.29079717987055886 ) ) ;
#24764 = VERTEX_POINT ( 'NONE', #29512 ) ;
#24765 = EDGE_LOOP ( 'NONE', ( #5711, #41744, #78602 ) ) ;
#24766 = PLANE ( 'NONE',  #43274 ) ;
#24767 = CARTESIAN_POINT ( 'NONE',  ( 46.43574122514301195, 74.10519008736565638, 10.00000000000000000 ) ) ;
#24768 = CARTESIAN_POINT ( 'NONE',  ( 191.0862225170008628, 299.6759493045793192, -9.402218231374108726 ) ) ;
#24769 = CARTESIAN_POINT ( 'NONE',  ( 29.53625146412516500, 35.79103043416551344, 8.090169943749478065 ) ) ;
#24770 = CYLINDRICAL_SURFACE ( 'NONE', #33853, 17.82106496071139645 ) ;
#24771 = CARTESIAN_POINT ( 'NONE',  ( 207.7117873102786518, 270.8796263780940308, 1.712754233133884085 ) ) ;
#24772 = CARTESIAN_POINT ( 'NONE',  ( 74.78872445064843077, 223.1744531367911293, 4.594050593750047540 ) ) ;
#24773 = VERTEX_POINT ( 'NONE', #4217 ) ;
#24774 = ORIENTED_EDGE ( 'NONE', *, *, #53512, .T. ) ;
#24775 = CARTESIAN_POINT ( 'NONE',  ( 200.6420049547404005, 283.1248486163401594, -18.32425536722374915 ) ) ;
#24776 = VERTEX_POINT ( 'NONE', #36601 ) ;
#24777 = CARTESIAN_POINT ( 'NONE',  ( 75.65276086696347591, 65.13941327059393416, -14.42100060933655570 ) ) ;
#24778 = CARTESIAN_POINT ( 'NONE',  ( -32.32800653043278061, 93.66491217184130846, 43.92044614505844891 ) ) ;
#24779 = CARTESIAN_POINT ( 'NONE',  ( -71.61465314115659453, 63.06504152958490295, 203.6502102582797420 ) ) ;
#24780 = CARTESIAN_POINT ( 'NONE',  ( 88.05889915941182267, 44.40447472371889148, 4.714184461739163723 ) ) ;
#24781 = ORIENTED_EDGE ( 'NONE', *, *, #4908, .F. ) ;
#24782 = CARTESIAN_POINT ( 'NONE',  ( 71.12873073640183463, 200.3262482093457777, 3.021315404115420679E-15 ) ) ;
#24783 = CARTESIAN_POINT ( 'NONE',  ( 185.2393081206536181, 260.2620773806470424, 6.297851702954142539 ) ) ;
#24784 = CARTESIAN_POINT ( 'NONE',  ( 159.9788992190088948, 253.5554137441726255, -15.81862932303382330 ) ) ;
#24785 = LINE ( 'NONE', #9618, #9248 ) ;
#24786 = CARTESIAN_POINT ( 'NONE',  ( 186.0776724513669080, 289.8818082167753118, 14.70292991719237818 ) ) ;
#24787 = CARTESIAN_POINT ( 'NONE',  ( 198.9243589141082396, 285.7204137842527985, -17.01128707248632566 ) ) ;
#24788 = FACE_OUTER_BOUND ( 'NONE', #97273, .T. ) ;
#24789 = ORIENTED_EDGE ( 'NONE', *, *, #75799, .T. ) ;
#24790 = EDGE_CURVE ( 'NONE', #64236, #8542, #67006, .T. ) ;
#24791 = CARTESIAN_POINT ( 'NONE',  ( -26.59607535340072104, 23.41021043553327630, -10.00000000000000000 ) ) ;
#24792 = CARTESIAN_POINT ( 'NONE',  ( 200.3134965941964651, 283.6938417875134064, 18.29802468362849766 ) ) ;
#24793 = DIRECTION ( 'NONE',  ( 1.000000000000000000, 0.000000000000000000, 0.000000000000000000 ) ) ;
#24794 = CARTESIAN_POINT ( 'NONE',  ( 187.9029328552566369, 266.2162208350674746, -11.92715153469220368 ) ) ;
#24795 = CARTESIAN_POINT ( 'NONE',  ( 83.63860429472313740, 52.00081728452852303, 14.99618877770985037 ) ) ;
#24796 = DIRECTION ( 'NONE',  ( 0.9576970189910596343, 0.2877784213863818774, 0.000000000000000000 ) ) ;
#24797 = CARTESIAN_POINT ( 'NONE',  ( 153.3543035181429559, 270.2748555357131295, 14.00895239929496583 ) ) ;
#24798 = EDGE_CURVE ( 'NONE', #7307, #75846, #51826, .T. ) ;
#24799 = ORIENTED_EDGE ( 'NONE', *, *, #56103, .F. ) ;
#24800 = CARTESIAN_POINT ( 'NONE',  ( 67.16256804578091533, 66.80979783321161847, 8.146902435796070208 ) ) ;
#24801 = DIRECTION ( 'NONE',  ( -0.8660254037844378194, -0.5000000000000014433, -0.000000000000000000 ) ) ;
#24802 = CLOSED_SHELL ( 'NONE', ( #44072, #70329, #13512, #58361, #36264, #30283, #2153, #33384, #62783, #10148, #50741, #27320, #88941, #90056, #92383, #45445, #31717, #19360, #47972, #1467, #94142, #53696, #50072, #81296, #21561, #40783, #22081, #4261, #75599, #95085, #39849, #81578, #17033, #35198, #73899, #11966, #96794, #10744, #85595, #80758, #98733, #40668, #64116, #70402, #7763, #29939, #25576, #90216, #11417, #10013, #17707, #14397, #90584, #97304, #76019, #43495, #39867, #95667, #37345, #58441, #39820, #5632, #73292, #58752, #95308, #2514, #74916, #89504, #51217, #66679, #95778, #55335, #85990, #17302, #65176, #88950, #92674, #64250, #33169, #18398, #36209, #17966, #34250, #88780, #94515, #52684, #1240, #77757, #87326, #77417, #52249, #3541, #32675, #69027, #62346, #76785, #82619, #30088, #39816, #13099, #86640, #52125, #9704, #99595, #18358, #77290, #28559, #13958, #18747, #44563, #72074, #77609, #26962, #100091, #62717, #14709, #36823, #8420, #2856, #59940, #54853, #17737, #6894, #54322, #4012, #92204, #44066, #58265, #44229, #32802, #56152, #70417, #62780, #86412, #71365, #25746, #6495, #57096, #44879, #38631, #32801, #69278, #1739, #71043, #96904, #64248, #59801, #40986, #60226, #25765, #50126, #24240, #60177, #2859, #73654, #79652, #43221, #23282, #59043, #80769, #11623, #12546, #17956, #48248, #49696, #83796, #85712, #60493, #5271, #51077, #85794, #45707, #2910, #844, #35940, #78057, #28440, #42292, #32904, #40673, #83381, #8429, #35675, #1823, #88448, #70028, #8482, #78246, #62911, #12584, #81009, #27589, #88742, #39896, #82642, #2348, #32360, #49191, #42055, #72339, #12266, #42241, #39879, #69408, #44237, #72403, #46732, #88947, #97958, #59876, #14472, #6950, #67070, #94374, #18717, #5234, #32371, #67870, #18851, #91171, #42519, #8747, #71490, #22022, #44114, #27779, #78623, #66723, #97336, #76915, #89715, #58077, #75348, #30183, #52458, #55852, #68203, #2983, #4707, #11775, #5846, #48241, #75725, #96477, #90282, #95503, #95657, #43683, #9892, #4075, #45470, #52420, #608, #32975, #14614, #13218, #8006, #80922, #10057, #34879, #20465, #66768, #36901, #96859, #32466, #36642, #34254, #26309, #58186, #52386, #72598, #94089, #95492, #43135, #36768, #45252, #35264, #49943, #47898, #94506, #70537, #67084, #70085, #20344, #38636, #18891, #15225, #89987, #7658, #768, #27093, #24338 ) ) ;
#24803 = CARTESIAN_POINT ( 'NONE',  ( 74.01887009131820605, 64.01258356010848161, -14.05577849739043650 ) ) ;
#24804 = CARTESIAN_POINT ( 'NONE',  ( 13.67211979723576931, 32.92651376809308772, -10.00000000000000000 ) ) ;
#24805 = CARTESIAN_POINT ( 'NONE',  ( 199.1489080723098084, 281.8162475621487033, -16.58710646079551054 ) ) ;
#24806 = VECTOR ( 'NONE', #51240, 1000.000000000000227 ) ;
#24807 = CARTESIAN_POINT ( 'NONE',  ( 29.77967365985639248, 29.14441083166262203, 10.00000000000000533 ) ) ;
#24808 = CARTESIAN_POINT ( 'NONE',  ( 171.8134125096551372, 274.9389237379870679, 17.04720683530305791 ) ) ;
#24809 = FACE_OUTER_BOUND ( 'NONE', #78852, .T. ) ;
#24810 = DIRECTION ( 'NONE',  ( 0.000000000000000000, -0.000000000000000000, 1.000000000000000000 ) ) ;
#24811 = CARTESIAN_POINT ( 'NONE',  ( 192.0630564889537482, 261.7319799974739567, 3.060561036580589978 ) ) ;
#24812 = CARTESIAN_POINT ( 'NONE',  ( 195.4097585203640222, 265.1988717782938920, -7.668974602499345039 ) ) ;
#24813 = CARTESIAN_POINT ( 'NONE',  ( -0.04102277327696322862, 170.7833772461660828, -9.188101187500095079 ) ) ;
#24814 = CIRCLE ( 'NONE', #89607, 16.60714546451156792 ) ;
#24815 = CARTESIAN_POINT ( 'NONE',  ( 81.46622351318225697, 45.77194399688346493, 11.40994803060552520 ) ) ;
#24816 = ORIENTED_EDGE ( 'NONE', *, *, #60291, .T. ) ;
#24818 = CARTESIAN_POINT ( 'NONE',  ( 174.8770607290546764, 255.3075393699999438, 8.411851435852767622 ) ) ;
#24817 = AXIS2_PLACEMENT_3D ( 'NONE', #48692, #18295, #64381 ) ;
#24819 = CARTESIAN_POINT ( 'NONE',  ( 19.98788723728717898, 104.4047874917408336, 22.50000000000002132 ) ) ;
#24820 = DIRECTION ( 'NONE',  ( 0.6758705274779430727, 0.2489746672676115269, -0.6936934806855756808 ) ) ;
#24821 = FACE_OUTER_BOUND ( 'NONE', #97431, .T. ) ;
#24822 = CARTESIAN_POINT ( 'NONE',  ( 29.16053163240333745, 178.4548013555409796, -4.594050593750042211 ) ) ;
#24823 = CARTESIAN_POINT ( 'NONE',  ( 22.35053764064823767, 35.83705186507754803, 3.090169943749475401 ) ) ;
#24824 = CARTESIAN_POINT ( 'NONE',  ( 30.93718178480143877, 33.56454794089042792, 10.00000000000000355 ) ) ;
#24825 = CARTESIAN_POINT ( 'NONE',  ( 181.6112919552439848, 294.4992701536799586, 6.459004801064330614 ) ) ;
#24826 = CARTESIAN_POINT ( 'NONE',  ( 173.5136117908628535, 272.6171107484045137, -16.35964596981252939 ) ) ;
#24827 = CARTESIAN_POINT ( 'NONE',  ( 73.55923329020097867, 67.59775090522703067, 12.07291635799731999 ) ) ;
#24828 = CARTESIAN_POINT ( 'NONE',  ( 81.89930626873778863, 42.21375885382297355, 7.647715624843501203 ) ) ;
#24829 = B_SPLINE_SURFACE_WITH_KNOTS ( 'NONE', 3, 1, ( 
 ( #1852, #45918 ),
 ( #22648, #53533 ),
 ( #100164, #92582 ),
 ( #84974, #46421 ),
 ( #69733, #93063 ),
 ( #23618, #54511 ),
 ( #5698, #72265 ),
 ( #2357, #36588 ),
 ( #48950, #66992 ),
 ( #64140, #57528 ),
 ( #88504, #26645 ),
 ( #5209, #72777 ),
 ( #59374, #19066 ),
 ( #18557, #97918 ),
 ( #33760, #94575 ),
 ( #34243, #25131 ),
 ( #57026, #96087 ),
 ( #3369, #49939 ),
 ( #13322, #80900 ),
 ( #11471, #28493 ),
 ( #88008, #65139 ),
 ( #56013, #90351 ),
 ( #42325, #20931 ),
 ( #2871, #41321 ),
 ( #79885, #49436 ),
 ( #48444, #74634 ),
 ( #10448, #87009 ),
 ( #64651, #26148 ),
 ( #17536, #79390 ),
 ( #36091, #80389 ),
 ( #51813, #95601 ),
 ( #33236, #10959 ),
 ( #82755, #9956 ),
 ( #41830, #44185 ) ),
 .UNSPECIFIED., .T., .F., .F.,
 ( 4, 2, 2, 2, 2, 2, 2, 2, 2, 2, 2, 2, 2, 2, 2, 2, 4 ),
 ( 2, 2 ),
 ( 0.000000000000000000, 0.06250000000000000000, 0.1250000000000000000, 0.1875000000000000000, 0.2500000000000000000, 0.3125000000000000000, 0.3750000000000000000, 0.4375000000000000000, 0.5000000000000000000, 0.5625000000000000000, 0.6250000000000000000, 0.6875000000000000000, 0.7500000000000000000, 0.8125000000000000000, 0.8750000000000000000, 0.9375000000000000000, 1.000000000000000000 ),
 ( 0.000000000000000000, 1.000000000000000000 ),
 .UNSPECIFIED. ) ;
#24830 = CARTESIAN_POINT ( 'NONE',  ( 186.6285282465448745, 296.1616521089468392, -8.750901477337695411 ) ) ;
#24831 = CARTESIAN_POINT ( 'NONE',  ( 91.45997379709665154, 213.6115022471902023, -5.000000000000041744 ) ) ;
#24832 = CARTESIAN_POINT ( 'NONE',  ( 70.24235140437789937, 201.3615022471901739, 5.000000000000051514 ) ) ;
#24833 = CARTESIAN_POINT ( 'NONE',  ( 68.12436787710551300, 66.83910121369015656, -8.880904761776434952 ) ) ;
#24834 = CARTESIAN_POINT ( 'NONE',  ( 185.6462244317068553, 277.7986853771898268, -17.33779381876608028 ) ) ;
#24835 = CARTESIAN_POINT ( 'NONE',  ( 203.4613517861610603, 269.9235832942454749, 6.857405767031560018 ) ) ;
#24836 = CARTESIAN_POINT ( 'NONE',  ( 43.26059451170998216, 183.5327760586659451, 1.948934522072303157E-15 ) ) ;
#24837 = CARTESIAN_POINT ( 'NONE',  ( 159.3169041484411537, 254.7020228407560580, 16.67170756419672628 ) ) ;
#24838 = CARTESIAN_POINT ( 'NONE',  ( 203.1085490052368243, 270.1107938249242579, -6.431837059875057605 ) ) ;
#24839 = LINE ( 'NONE', #70965, #77272 ) ;
#24840 = CARTESIAN_POINT ( 'NONE',  ( 17.38248943320504836, 35.13769309531819829, 10.00000000000000000 ) ) ;
#24841 = VERTEX_POINT ( 'NONE', #12846 ) ;
#24842 = FACE_OUTER_BOUND ( 'NONE', #53761, .T. ) ;
#24843 = CARTESIAN_POINT ( 'NONE',  ( 168.0045135618281904, 281.9156128332120943, -11.93384029740529684 ) ) ;
#24844 = B_SPLINE_CURVE_WITH_KNOTS ( 'NONE', 3,
 ( #44568, #22283, #21785, #75503 ),
 .UNSPECIFIED., .F., .F.,
 ( 4, 4 ),
 ( 0.005429109838488062507, 0.01103906108590186654 ),
 .UNSPECIFIED. ) ;
#24845 = DIRECTION ( 'NONE',  ( 0.8660254037844383745, 0.5000000000000003331, -0.000000000000000000 ) ) ;
#24846 = CARTESIAN_POINT ( 'NONE',  ( 169.5608527833963421, 251.6396950762901952, -9.960993533446050208 ) ) ;
#24847 = CARTESIAN_POINT ( 'NONE',  ( 23.32838594064934767, 31.65586893147757408, -7.433330006724137462 ) ) ;
#24848 = CARTESIAN_POINT ( 'NONE',  ( 162.6264071486809542, 248.9697954965390920, 10.36322805486644683 ) ) ;
#24849 = CARTESIAN_POINT ( 'NONE',  ( 149.5796913320911870, 271.5673701627850960, -12.80793412251569841 ) ) ;
#24850 = EDGE_CURVE ( 'NONE', #36314, #92132, #83751, .T. ) ;
#24851 = CARTESIAN_POINT ( 'NONE',  ( 188.8949863289861071, 270.0988553178502798, -14.15076922796234982 ) ) ;
#24852 = ORIENTED_EDGE ( 'NONE', *, *, #10502, .F. ) ;
#24853 = CARTESIAN_POINT ( 'NONE',  ( 4.685401460390529849, 24.74646525600388003, 2.839279412974139660 ) ) ;
#24854 = CARTESIAN_POINT ( 'NONE',  ( 72.21948760849898008, 60.12913787482489880, -15.14087808330432594 ) ) ;
#24855 = CARTESIAN_POINT ( 'NONE',  ( 71.77363275119753894, 72.50400781664164640, -1.333432854898964681 ) ) ;
#24856 = VERTEX_POINT ( 'NONE', #68008 ) ;
#24857 = FACE_OUTER_BOUND ( 'NONE', #97107, .T. ) ;
#24858 = CARTESIAN_POINT ( 'NONE',  ( 179.0008080442136418, 282.3876334254374001, 15.30776276532570712 ) ) ;
#24859 = CARTESIAN_POINT ( 'NONE',  ( 85.45686282584428284, 49.07624996843039611, 12.35599031532369452 ) ) ;
#24860 = CARTESIAN_POINT ( 'NONE',  ( 177.7787795431753466, 256.3680583258327488, -7.267765067160797621 ) ) ;
#24861 = CARTESIAN_POINT ( 'NONE',  ( 190.2389970918280540, 301.1433867864428748, 4.601241515604689525 ) ) ;
#24862 = EDGE_CURVE ( 'NONE', #11364, #20041, #95265, .T. ) ;
#24863 = EDGE_LOOP ( 'NONE', ( #78095, #16435, #36978, #72162 ) ) ;
#24864 = ORIENTED_EDGE ( 'NONE', *, *, #92511, .F. ) ;
#24866 = CARTESIAN_POINT ( 'NONE',  ( 83.42425903942064735, 42.46362989694333834, -5.239620355152831976 ) ) ;
#24865 = CARTESIAN_POINT ( 'NONE',  ( 194.6820509838467785, 270.8910309865917156, -14.27696746312268239 ) ) ;
#24867 = ORIENTED_EDGE ( 'NONE', *, *, #80337, .T. ) ;
#24868 = CARTESIAN_POINT ( 'NONE',  ( 200.9812045408918380, 282.5373376992193926, -16.61165062382494284 ) ) ;
#24869 = CARTESIAN_POINT ( 'NONE',  ( 71.90245059369782155, 72.17364547496468674, -3.641340926847324244 ) ) ;
#24870 = CARTESIAN_POINT ( 'NONE',  ( 72.71113525135035616, 57.05229220753940211, -15.90378019451816094 ) ) ;
#24871 = CARTESIAN_POINT ( 'NONE',  ( -32.30932376655839988, 25.48519649537502119, -10.00000000000000000 ) ) ;
#24872 = EDGE_CURVE ( 'NONE', #20250, #93322, #81760, .T. ) ;
#24873 = CARTESIAN_POINT ( 'NONE',  ( 204.6713671561005299, 276.1457885614869951, -12.94307097876490431 ) ) ;
#24874 = CARTESIAN_POINT ( 'NONE',  ( 105.4518702730975122, 225.5643266524160140, 9.188101187500095079 ) ) ;
#24875 = CARTESIAN_POINT ( 'NONE',  ( 149.0164813726494799, 272.5428784278667536, -11.67305721329070423 ) ) ;
#24876 = VECTOR ( 'NONE', #71965, 1000.000000000000227 ) ;
#24877 = ORIENTED_EDGE ( 'NONE', *, *, #20789, .T. ) ;
#24878 = CARTESIAN_POINT ( 'NONE',  ( 208.2777459429579210, 269.8993572713111462, 3.129643751043610589 ) ) ;
#24879 = VERTEX_POINT ( 'NONE', #70498 ) ;
#24880 = CARTESIAN_POINT ( 'NONE',  ( 30.88926192328758447, 20.76004757982090609, 5.678558825948272215 ) ) ;
#24881 = CARTESIAN_POINT ( 'NONE',  ( 159.4889735931715222, 254.4039898200529706, 16.88104032092801887 ) ) ;
#24882 = CARTESIAN_POINT ( 'NONE',  ( 58.41569198217266035, 204.5333772461660544, 9.188101187500095079 ) ) ;
#24883 = CARTESIAN_POINT ( 'NONE',  ( 74.20995892610953604, 68.60058487300136676, 11.52733404855582755 ) ) ;
#24884 = CARTESIAN_POINT ( 'NONE',  ( 160.2827339360533188, 254.1851989922621726, 15.48500462334072658 ) ) ;
#24885 = CARTESIAN_POINT ( 'NONE',  ( 150.2678036912315349, 270.3755245954375823, 14.25047800729520375 ) ) ;
#24886 = CARTESIAN_POINT ( 'NONE',  ( 175.4173451253388407, 272.5932200924088420, 17.76602235907715510 ) ) ;
#24887 = ORIENTED_EDGE ( 'NONE', *, *, #41478, .F. ) ;
#24888 = B_SPLINE_CURVE_WITH_KNOTS ( 'NONE', 3,
 ( #43003, #58708, #4526, #83063 ),
 .UNSPECIFIED., .F., .F.,
 ( 4, 4 ),
 ( 0.000000000000000000, 0.002003342248209785594 ),
 .UNSPECIFIED. ) ;
#24889 = CARTESIAN_POINT ( 'NONE',  ( 190.2629546459234859, 273.4080951500121159, -16.67925241984795903 ) ) ;
#24890 = AXIS2_PLACEMENT_3D ( 'NONE', #38383, #13126, #36393 ) ;
#24891 = CARTESIAN_POINT ( 'NONE',  ( 167.6146168596400514, 252.8497314824998909, -12.44459218179994231 ) ) ;
#24892 = DIRECTION ( 'NONE',  ( 0.5000000000000048850, -0.8660254037844358210, 0.000000000000000000 ) ) ;
#24893 = ORIENTED_EDGE ( 'NONE', *, *, #98347, .T. ) ;
#24894 = CARTESIAN_POINT ( 'NONE',  ( 103.0791479645378104, 236.9865022471902876, -10.00000000000009592 ) ) ;
#24895 = CARTESIAN_POINT ( 'NONE',  ( 69.87205324732853740, 69.72719669029187628, -5.804370611097000143 ) ) ;
#24896 = CARTESIAN_POINT ( 'NONE',  ( 207.4218731373931632, 271.3817724553659332, -5.249531240730909154 ) ) ;
#24897 = CARTESIAN_POINT ( 'NONE',  ( 193.1649355862271591, 296.0755126543221536, -12.21556774862162698 ) ) ;
#24898 = VECTOR ( 'NONE', #85987, 1000.000000000000227 ) ;
#24899 = CARTESIAN_POINT ( 'NONE',  ( -19.65312891409030271, 93.06504152958497400, 10.00000000000000888 ) ) ;
#24900 = CARTESIAN_POINT ( 'NONE',  ( 42.54989241151534429, 183.8262482093457493, 3.021315404115420679E-15 ) ) ;
#24901 = CARTESIAN_POINT ( 'NONE',  ( 86.23513880351241312, 43.01419119376065936, -3.607706737359228644 ) ) ;
#24902 = CARTESIAN_POINT ( 'NONE',  ( 67.34941845850391928, 66.92956724091470733, 9.029314852957725179 ) ) ;
#24903 = CARTESIAN_POINT ( 'NONE',  ( 75.79750337254498049, 64.14884731463476442, -14.49056795948485110 ) ) ;
#24904 = DIRECTION ( 'NONE',  ( -0.000000000000000000, 0.000000000000000000, -1.000000000000000000 ) ) ;
#24905 = CARTESIAN_POINT ( 'NONE',  ( 106.4801018922090066, 232.2833772461660544, -9.188101187500095079 ) ) ;
#24906 = VERTEX_POINT ( 'NONE', #14802 ) ;
#24907 = CARTESIAN_POINT ( 'NONE',  ( 147.0276296945837373, 275.9876705829954062, 0.7617065417431535534 ) ) ;
#24908 = ADVANCED_FACE ( 'NONE', ( #68994 ), #55283, .T. ) ;
#24909 = CARTESIAN_POINT ( 'NONE',  ( 84.12544262676013318, 41.86299551560625076, -0.4765227021652564954 ) ) ;
#24910 = EDGE_CURVE ( 'NONE', #86838, #81759, #80224, .T. ) ;
#24911 = CARTESIAN_POINT ( 'NONE',  ( 203.0862352702880003, 278.8913175244117610, -15.09542727681365015 ) ) ;
#24912 = CARTESIAN_POINT ( 'NONE',  ( 183.1065844243434242, 285.0799303997669654, -14.93148665631748351 ) ) ;
#24913 = DIRECTION ( 'NONE',  ( -0.1710100716628374096, 0.2961981327260301833, 0.9396926207859057634 ) ) ;
#24914 = CARTESIAN_POINT ( 'NONE',  ( 178.1205181064416081, 255.2832539585039342, 4.586525146579208290 ) ) ;
#24915 = VERTEX_POINT ( 'NONE', #85249 ) ;
#24916 = CARTESIAN_POINT ( 'NONE',  ( 80.55623134086874870, 57.74356886441330516, -16.24537044847425804 ) ) ;
#24917 = CARTESIAN_POINT ( 'NONE',  ( 158.4671134108900787, 274.9587530538368583, -12.53151093071063471 ) ) ;
#24918 = LINE ( 'NONE', #73048, #1499 ) ;
#24919 = CARTESIAN_POINT ( 'NONE',  ( 164.7680996532798474, 245.2602752643843189, -0.9068639473870550027 ) ) ;
#24920 = CARTESIAN_POINT ( 'NONE',  ( 129.5380282679697075, 245.5958772461660544, -9.188101187500095079 ) ) ;
#24921 = CARTESIAN_POINT ( 'NONE',  ( 198.4860348845112981, 286.8590983175747056, -18.20461732983060088 ) ) ;
#24922 = EDGE_CURVE ( 'NONE', #30618, #84862, #3374, .T. ) ;
#24923 = CARTESIAN_POINT ( 'NONE',  ( 185.3925434965363763, 297.5756078945317427, 4.115160971246430321 ) ) ;
#24924 = CARTESIAN_POINT ( 'NONE',  ( 188.1708508464760712, 281.7058697880425484, -16.75825131916482391 ) ) ;
#24925 = CARTESIAN_POINT ( 'NONE',  ( 147.1270795744234476, 264.4111747905818675, -1.822351119449947324E-15 ) ) ;
#24926 = CARTESIAN_POINT ( 'NONE',  ( 44.82974491242176640, 202.8149278399160664, 9.188101187500093303 ) ) ;
#24927 = CARTESIAN_POINT ( 'NONE',  ( 85.35443477132466228, 48.30880629543902671, -11.80360700664791018 ) ) ;
#24928 = CARTESIAN_POINT ( 'NONE',  ( 87.78619429942361307, 44.41240826577528367, -3.951812172081524022 ) ) ;
#24929 = ADVANCED_FACE ( 'NONE', ( #60885 ), #39949, .F. ) ;
#24930 = CARTESIAN_POINT ( 'NONE',  ( 174.3443330002151583, 262.1300491651107905, 14.35593273800351533 ) ) ;
#24931 = CARTESIAN_POINT ( 'NONE',  ( 82.10523990517462778, 41.85707133252697076, -5.529865280922466653 ) ) ;
#24932 = CARTESIAN_POINT ( 'NONE',  ( 182.0894599482799094, 294.4148934881073956, -6.407201795530185429 ) ) ;
#24933 = DIRECTION ( 'NONE',  ( -1.000000000000000000, 0.000000000000000000, 0.000000000000000000 ) ) ;
#24934 = CARTESIAN_POINT ( 'NONE',  ( 178.3097623879434934, 261.2848360722642838, 12.47870625538927669 ) ) ;
#24935 = CARTESIAN_POINT ( 'NONE',  ( 117.2061873602235238, 245.1427522451419065, -10.00000000000009415 ) ) ;
#24936 = CARTESIAN_POINT ( 'NONE',  ( 76.58844930818931118, 53.16667539083663030, -15.92936049379509456 ) ) ;
#24937 = VERTEX_POINT ( 'NONE', #94344 ) ;
#24938 = CARTESIAN_POINT ( 'NONE',  ( 202.9972156839127990, 279.0455039708822937, 16.77197898838388213 ) ) ;
#24939 = CARTESIAN_POINT ( 'NONE',  ( 88.00125901251291793, 44.79538816511593069, 4.736495928124922372 ) ) ;
#24940 = CARTESIAN_POINT ( 'NONE',  ( 30.97368554763575688, 182.5643266524159856, -9.188101187500093303 ) ) ;
#24941 = CARTESIAN_POINT ( 'NONE',  ( 9.082762260191241666, 27.01751292744054567, 6.180339887498949913 ) ) ;
#24942 = CARTESIAN_POINT ( 'NONE',  ( 188.8280684177597664, 290.6827677694134309, -15.06566886457551568 ) ) ;
#24943 = DIRECTION ( 'NONE',  ( -0.000000000000000000, 0.000000000000000000, 1.000000000000000000 ) ) ;
#24944 = LINE ( 'NONE', #40133, #10311 ) ;
#24946 = CARTESIAN_POINT ( 'NONE',  ( 63.58478110923711313, 197.5177522451417929, 5.000000000000051514 ) ) ;
#24945 = PLANE ( 'NONE',  #26710 ) ;
#24947 = CARTESIAN_POINT ( 'NONE',  ( 171.7935577790372861, 286.8752040708455411, 7.461994811497778102 ) ) ;
#24948 = CARTESIAN_POINT ( 'NONE',  ( -62.83817737799399339, 37.97373922903765475, 177.5919119679930134 ) ) ;
#24949 = CARTESIAN_POINT ( 'NONE',  ( -13.11024591527734628, 6.000000000000000000, 32.50000000000000000 ) ) ;
#24950 = CARTESIAN_POINT ( 'NONE',  ( 17.93656579593215028, 10.75978393459163307, -1.583844403245362020 ) ) ;
#24951 = ORIENTED_EDGE ( 'NONE', *, *, #25964, .T. ) ;
#24952 = B_SPLINE_CURVE_WITH_KNOTS ( 'NONE', 3,
 ( #73612, #99282, #38445, #91697, #4193, #76479, #96952, #61248, #89361, #19917, #50788, #81740, #92217, #86128, #31355, #9066, #39435, #87642, #33361, #56657, #39933, #1478, #94201, #966, #8569, #85618, #17670, #64261, #93702, #1969, #62238, #32361, #24755, #40935, #77973, #70354, #16162, #16657, #38948, #69853, #31843, #63763, #2479, #70871 ),
 .UNSPECIFIED., .F., .F.,
 ( 4, 2, 2, 2, 2, 2, 2, 2, 2, 2, 2, 2, 2, 2, 2, 2, 2, 2, 2, 2, 2, 4 ),
 ( 0.003392636941779382433, 0.003583394314189582066, 0.003678773000394681449, 0.003774151686599781265, 0.003869530372804881081, 0.003964909059009980030, 0.004155666431420030477, 0.004537181176240082797, 0.004918695921060133383, 0.005681725410700300474, 0.006444754900340467565, 0.007970813879620801748, 0.008161571252030822704, 0.008185415923582036943, 0.008209260595133251182, 0.008233105266684463686, 0.008256949938235677924, 0.008352328624440510593, 0.008543085996850172462, 0.008733843369259834330, 0.009115358114079230925, 0.009496872858898627520 ),
 .UNSPECIFIED. ) ;
#24953 = AXIS2_PLACEMENT_3D ( 'NONE', #53707, #61314, #37025 ) ;
#24954 = CARTESIAN_POINT ( 'NONE',  ( 27.01324999880465683, 179.7365022471902307, 10.00000000000009592 ) ) ;
#24955 = CARTESIAN_POINT ( 'NONE',  ( 36.73799359191946934, 192.0177522451418781, -10.00000000000009592 ) ) ;
#24956 = CARTESIAN_POINT ( 'NONE',  ( 162.8789161433191452, 248.5324370884573568, 9.731756914259689140 ) ) ;
#24957 = CARTESIAN_POINT ( 'NONE',  ( -6.102853504003019403, 155.0327760586659451, 1.948934522072303157E-15 ) ) ;
#24958 = CARTESIAN_POINT ( 'NONE',  ( 31.10096393961467598, 36.14336893147757479, 7.433330006724141015 ) ) ;
#24959 = CARTESIAN_POINT ( 'NONE',  ( 200.3625978841952531, 283.1932893211792361, 16.78850222475318432 ) ) ;
#24960 = CARTESIAN_POINT ( 'NONE',  ( -19.65312891409030271, 93.06504152958497400, 10.00000000000000888 ) ) ;
#24961 = CARTESIAN_POINT ( 'NONE',  ( 25.46698091360950045, 30.10171378149919974, 9.188101187500008038 ) ) ;
#24962 = CARTESIAN_POINT ( 'NONE',  ( 164.6241018286200699, 245.5096868128744632, 3.031483545445131433 ) ) ;
#24963 = VECTOR ( 'NONE', #64253, 1000.000000000000227 ) ;
#24964 = CARTESIAN_POINT ( 'NONE',  ( 183.6116158731336441, 256.9743117497176854, -1.628339465941822661 ) ) ;
#24965 = CARTESIAN_POINT ( 'NONE',  ( 66.04563933824955768, 68.55708310873542644, 2.069072683234986609 ) ) ;
#24966 = ORIENTED_EDGE ( 'NONE', *, *, #61819, .T. ) ;
#24967 = CARTESIAN_POINT ( 'NONE',  ( 80.33508072308801218, 44.92307697338561212, 11.19555900290710326 ) ) ;
#24968 = DIRECTION ( 'NONE',  ( 1.000000000000000000, 0.000000000000000000, 0.000000000000000000 ) ) ;
#24969 = CARTESIAN_POINT ( 'NONE',  ( 152.8894687064977234, 278.3516875449029158, -6.243347624783317507 ) ) ;
#24970 = CARTESIAN_POINT ( 'NONE',  ( 16.34664070491415444, 11.29860640527290983, -2.839279412974138328 ) ) ;
#24971 = CARTESIAN_POINT ( 'NONE',  ( 207.0170762168093859, 272.0829012885643579, 9.497721717913687911 ) ) ;
#24972 = EDGE_CURVE ( 'NONE', #50442, #17777, #44575, .T. ) ;
#24973 = CARTESIAN_POINT ( 'NONE',  ( -52.32156893544651410, 31.15564784356141814, 10.00000000000000000 ) ) ;
#24974 = CARTESIAN_POINT ( 'NONE',  ( 159.2651917302844993, 254.7915913763855258, -16.53922207549818424 ) ) ;
#24975 = CARTESIAN_POINT ( 'NONE',  ( -38.61298035630893111, 26.97617139035147460, -10.00000000000000000 ) ) ;
#24976 = EDGE_CURVE ( 'NONE', #24906, #37352, #63901, .T. ) ;
#24977 = CARTESIAN_POINT ( 'NONE',  ( 192.2431834237441706, 297.6720342317289578, 11.07782187406058938 ) ) ;
#24978 = CYLINDRICAL_SURFACE ( 'NONE', #28775, 17.82106496071139645 ) ;
#24979 = CARTESIAN_POINT ( 'NONE',  ( 163.3409975114459485, 247.7320886816312111, -10.96358124877083640 ) ) ;
#24980 = DIRECTION ( 'NONE',  ( -0.8660254037844380415, -0.5000000000000011102, 0.000000000000000000 ) ) ;
#24981 = ORIENTED_EDGE ( 'NONE', *, *, #55264, .T. ) ;
#24982 = ORIENTED_EDGE ( 'NONE', *, *, #29271, .F. ) ;
#24983 = LINE ( 'NONE', #55369, #13092 ) ;
#24984 = CARTESIAN_POINT ( 'NONE',  ( 86.26094451566392252, 47.67890430677171310, 10.76907119421248460 ) ) ;
#24985 = ORIENTED_EDGE ( 'NONE', *, *, #75425, .F. ) ;
#24986 = CARTESIAN_POINT ( 'NONE',  ( 24.75116620650193866, 19.45404122711133965, -8.090169943749478065 ) ) ;
#24987 = CARTESIAN_POINT ( 'NONE',  ( 171.2741013746033332, 249.3936815359432728, 2.927055546763141169 ) ) ;
#24989 = EDGE_CURVE ( 'NONE', #48406, #89111, #49882, .T. ) ;
#24988 = ORIENTED_EDGE ( 'NONE', *, *, #4114, .T. ) ;
#24990 = CARTESIAN_POINT ( 'NONE',  ( 191.0481192767711036, 299.7419460525905492, -9.103377665618040737 ) ) ;
#24991 = CARTESIAN_POINT ( 'NONE',  ( 84.71672111353214518, 48.50487602508921725, -12.22989703533773032 ) ) ;
#24992 = CARTESIAN_POINT ( 'NONE',  ( 80.73512995292455230, 43.24773137545005142, 9.993358235750852359 ) ) ;
#24993 = VERTEX_POINT ( 'NONE', #27897 ) ;
#24994 = CARTESIAN_POINT ( 'NONE',  ( 161.5431944097339851, 250.8459749958011287, 14.52339846942414603 ) ) ;
#24995 = DIRECTION ( 'NONE',  ( -0.8278489937552474531, 0.5609510170580175314, 0.000000000000000000 ) ) ;
#24996 = B_SPLINE_CURVE_WITH_KNOTS ( 'NONE', 3,
 ( #27908, #58305, #13233, #59793 ),
 .UNSPECIFIED., .F., .F.,
 ( 4, 4 ),
 ( 0.01565730217348996339, 0.02445820785911252682 ),
 .UNSPECIFIED. ) ;
#24997 = CARTESIAN_POINT ( 'NONE',  ( 151.3883635558152321, 268.4346579770563608, 15.44343517165679103 ) ) ;
#24998 = CARTESIAN_POINT ( 'NONE',  ( 9.830230629461709668, 30.95267373526312227, -10.00000000000000000 ) ) ;
#24999 = ORIENTED_EDGE ( 'NONE', *, *, #52211, .F. ) ;
#25000 = FACE_OUTER_BOUND ( 'NONE', #67758, .T. ) ;
#25001 = EDGE_CURVE ( 'NONE', #14695, #24162, #15049, .T. ) ;
#25002 = EDGE_LOOP ( 'NONE', ( #281, #84149, #10325 ) ) ;
#25003 = EDGE_CURVE ( 'NONE', #86003, #77450, #89748, .T. ) ;
#25004 = ORIENTED_EDGE ( 'NONE', *, *, #65731, .T. ) ;
#25005 = CARTESIAN_POINT ( 'NONE',  ( 72.97982471419457795, 59.59981046274725003, 15.43291100737614663 ) ) ;
#25006 = VERTEX_POINT ( 'NONE', #73515 ) ;
#25007 = CARTESIAN_POINT ( 'NONE',  ( 165.5093369583051128, 275.0219039653110258, -16.16693748275729803 ) ) ;
#25008 = ORIENTED_EDGE ( 'NONE', *, *, #43057, .F. ) ;
#25009 = CARTESIAN_POINT ( 'NONE',  ( 83.23886772428572556, 49.12744029586829697, 13.18137976536933031 ) ) ;
#25010 = CARTESIAN_POINT ( 'NONE',  ( 69.98658646620340562, 66.36472102019232011, 10.66432767654794311 ) ) ;
#25011 = CARTESIAN_POINT ( 'NONE',  ( 148.3253847707240141, 273.7398928553401447, -9.074433450356286457 ) ) ;
#25012 = DIRECTION ( 'NONE',  ( -1.000000000000000000, 0.000000000000000000, 0.000000000000000000 ) ) ;
#25013 = CARTESIAN_POINT ( 'NONE',  ( 187.0083344850037008, 268.0836409071914090, -15.22627500120235133 ) ) ;
#25014 = ORIENTED_EDGE ( 'NONE', *, *, #41013, .F. ) ;
#25015 = CARTESIAN_POINT ( 'NONE',  ( 78.44203751522358914, 61.21016990572090322, 16.24725970467587643 ) ) ;
#25016 = CARTESIAN_POINT ( 'NONE',  ( 18.54180792094154029, 32.74646525600390135, 2.839279412974139660 ) ) ;
#25017 = CARTESIAN_POINT ( 'NONE',  ( 206.4943150373521803, 272.9883502116088039, 11.34100825923693101 ) ) ;
#25018 = DIRECTION ( 'NONE',  ( -0.8660254037844387076, -0.4999999999999998890, -0.000000000000000000 ) ) ;
#25020 = ORIENTED_EDGE ( 'NONE', *, *, #13353, .T. ) ;
#25019 = CARTESIAN_POINT ( 'NONE',  ( 159.4574711498080433, 254.4585536525209477, 16.86100557095418395 ) ) ;
#25021 = CARTESIAN_POINT ( 'NONE',  ( 146.7443032962641212, 276.4784063000103060, -3.845166261074166147 ) ) ;
#25022 = EDGE_CURVE ( 'NONE', #19465, #70901, #98317, .T. ) ;
#25023 = CARTESIAN_POINT ( 'NONE',  ( 63.58478110923711313, 197.5177522451417929, 5.000000000000051514 ) ) ;
#25024 = CARTESIAN_POINT ( 'NONE',  ( 206.0870578475358172, 273.6937403561189512, -10.07771901274806581 ) ) ;
#25025 = FACE_OUTER_BOUND ( 'NONE', #51032, .T. ) ;
#25026 =( BOUNDED_CURVE ( )  B_SPLINE_CURVE ( 2, ( #52267, #43156, #5673, #66477, #68459, #66965, #90826, #36066, #74097 ),
 .UNSPECIFIED., .F., .T. ) 
 B_SPLINE_CURVE_WITH_KNOTS ( ( 3, 2, 2, 2, 3 ),
 ( 0.5524193548387096309, 0.5537634408602150060, 0.5564516129032257563, 0.5591397849462365066, 0.5604838709677418818 ),
 .UNSPECIFIED. ) 
 CURVE ( )  GEOMETRIC_REPRESENTATION_ITEM ( )  RATIONAL_B_SPLINE_CURVE ( ( 0.9330127018922194093, 0.9330127018922194093, 1.000000000000000000, 0.8660254037844387076, 1.000000000000000000, 0.8660254037844387076, 1.000000000000000000, 0.9330127018922194093, 0.9330127018922194093 ) ) 
 REPRESENTATION_ITEM ( '' )  );
#25027 = VECTOR ( 'NONE', #26544, 1000.000000000000227 ) ;
#25028 = CARTESIAN_POINT ( 'NONE',  ( 200.1103929410127762, 284.0456276340304953, 17.67835211026828901 ) ) ;
#25029 = PLANE ( 'NONE',  #83921 ) ;
#25030 = ORIENTED_EDGE ( 'NONE', *, *, #44451, .T. ) ;
#25032 = EDGE_CURVE ( 'NONE', #44171, #79518, #63616, .T. ) ;
#25031 = CARTESIAN_POINT ( 'NONE',  ( 155.1093231057254229, 261.9897669837033618, -17.23289009958756068 ) ) ;
#25033 = DIRECTION ( 'NONE',  ( -0.8660254037844387076, -0.4999999999999998890, -0.000000000000000000 ) ) ;
#25034 = DIRECTION ( 'NONE',  ( 0.3715724127386967335, -0.6435822975543782354, -0.6691306063588567943 ) ) ;
#25035 = CARTESIAN_POINT ( 'NONE',  ( 12.48928228595513801, 188.0177522451419065, 5.000000000000046185 ) ) ;
#25036 = CARTESIAN_POINT ( 'NONE',  ( 96.27750042569734035, 217.2048013555409796, 4.594050593750051981 ) ) ;
#25037 = CONICAL_SURFACE ( 'NONE', #86567, 11.00000000000002842, 0.7853981633974557175 ) ;
#25038 = CARTESIAN_POINT ( 'NONE',  ( 82.26726714915119487, 40.87605626266926606, -1.219143652196071459 ) ) ;
#25039 = EDGE_CURVE ( 'NONE', #48736, #6194, #5106, .T. ) ;
#25040 = B_SPLINE_CURVE_WITH_KNOTS ( 'NONE', 3,
 ( #34990, #67388, #74526, #66891 ),
 .UNSPECIFIED., .F., .F.,
 ( 4, 4 ),
 ( 0.008405187511566250894, 0.01662358261992283662 ),
 .UNSPECIFIED. ) ;
#25041 = CARTESIAN_POINT ( 'NONE',  ( 174.7267715799268615, 282.0933535004488135, -14.14109511867729729 ) ) ;
#25042 = CARTESIAN_POINT ( 'NONE',  ( 208.0964157306580375, 270.2134304119617809, 3.093366075300640894 ) ) ;
#25043 = B_SPLINE_CURVE_WITH_KNOTS ( 'NONE', 3,
 ( #13756, #52252, #99373, #68940, #53250, #51774, #75078, #99866, #59849, #64, #98382, #45149, #22849, #29952, #44144, #59333, #38540, #61340, #92299, #28971, #53732, #68445, #90812, #90313, #98879, #15232, #67959, #36547, #75569, #76088, #46128, #20885, #60333, #83194, #60828, #82715, #13283, #21856, #6158, #37052, #52737, #83700, #14259, #6662, #91788, #1057, #77568, #8156, #56240, #15736 ),
 .UNSPECIFIED., .F., .F.,
 ( 4, 2, 2, 2, 2, 2, 2, 2, 2, 2, 2, 2, 2, 2, 2, 2, 2, 2, 2, 2, 2, 2, 2, 2, 4 ),
 ( 0.0003491678432873779694, 0.0008189001457873160399, 0.001288632448287254165, 0.001523498599537288821, 0.001640931675162307342, 0.001758364750787326297, 0.001993230902037290263, 0.002228097053287254013, 0.002697829355787181513, 0.003167561658287109446, 0.004107026263287102789, 0.005046490868287095699, 0.005516223170787129884, 0.005751089322037109680, 0.005868522397662098711, 0.005927238935474593226, 0.005985955473287089476, 0.006044672011099583991, 0.006103388548912078507, 0.006220821624537024169, 0.006455687775786910290, 0.006925420078286675593, 0.007395152380786440896, 0.007630018532036412886, 0.007864884683286383141 ),
 .UNSPECIFIED. ) ;
#25045 = CARTESIAN_POINT ( 'NONE',  ( 75.53874658597716518, 65.44746306994376539, 13.83256553230837760 ) ) ;
#25044 = CARTESIAN_POINT ( 'NONE',  ( 7.590652549690899420, 181.3149278399161233, -9.188101187500095079 ) ) ;
#25046 = EDGE_CURVE ( 'NONE', #65825, #96856, #81643, .T. ) ;
#25047 = CARTESIAN_POINT ( 'NONE',  ( 161.8811854682448939, 250.2605573099562264, 13.51112293479948789 ) ) ;
#25048 = VERTEX_POINT ( 'NONE', #97821 ) ;
#25050 = ORIENTED_EDGE ( 'NONE', *, *, #65196, .T. ) ;
#25049 = PRODUCT_DEFINITION_CONTEXT ( 'detailed design', #54587, 'design' ) ;
#25051 = ADVANCED_FACE ( 'NONE', ( #84505 ), #76858, .F. ) ;
#25052 = CARTESIAN_POINT ( 'NONE',  ( 188.6230325960351024, 261.4887198759634543, -5.970139219065332625 ) ) ;
#25053 = CARTESIAN_POINT ( 'NONE',  ( 67.33690759333875064, 68.97606460400891137, 3.668405113326242084 ) ) ;
#25054 = CARTESIAN_POINT ( 'NONE',  ( 83.83342451037863441, 43.32515297521197084, 6.643328278011193078 ) ) ;
#25055 = CARTESIAN_POINT ( 'NONE',  ( 161.8668411317136986, 250.2854024296290447, -13.43522912998426655 ) ) ;
#25056 = CARTESIAN_POINT ( 'NONE',  ( 74.17344901341724039, 68.45477986254626046, -11.63824756869785659 ) ) ;
#25057 = CARTESIAN_POINT ( 'NONE',  ( 44.64073572505018461, 187.3923013555410080, 4.594050593750050204 ) ) ;
#25058 = CARTESIAN_POINT ( 'NONE',  ( 78.23504418992378362, 222.6427522451418781, -10.00000000000009415 ) ) ;
#25059 = CARTESIAN_POINT ( 'NONE',  ( -19.65312891409030271, 93.06504152958497400, 177.5919119679930134 ) ) ;
#25060 = ORIENTED_EDGE ( 'NONE', *, *, #61515, .F. ) ;
#25061 = CARTESIAN_POINT ( 'NONE',  ( 82.12214578622800332, 43.36728084772444447, 8.278842856071861434 ) ) ;
#25062 = CARTESIAN_POINT ( 'NONE',  ( -3.153128914090298274, 64.48620320469859735, 0.000000000000000000 ) ) ;
#25063 = VECTOR ( 'NONE', #100244, 1000.000000000000000 ) ;
#25064 = CARTESIAN_POINT ( 'NONE',  ( -13.54586673536430830, 172.1744531367911293, 4.594050593750047540 ) ) ;
#25065 = CARTESIAN_POINT ( 'NONE',  ( 69.04169954231571182, 64.33839118639518517, -11.93766638194810703 ) ) ;
#25066 = CARTESIAN_POINT ( 'NONE',  ( 161.6923300915171922, 250.5876644177310482, -14.43081872899884566 ) ) ;
#25067 = CARTESIAN_POINT ( 'NONE',  ( 187.0955991096881519, 282.9188776676083421, 16.20459510219963661 ) ) ;
#25068 = CARTESIAN_POINT ( 'NONE',  ( 147.6884207308302450, 274.8431469350302336, -8.096293592099874203 ) ) ;
#25069 = CARTESIAN_POINT ( 'NONE',  ( 72.79105583609376140, 67.08523038410258721, 12.12250871139724318 ) ) ;
#25070 = CARTESIAN_POINT ( 'NONE',  ( 171.6803261575313968, 279.7085677115863973, 14.16212843711857516 ) ) ;
#25071 = CARTESIAN_POINT ( 'NONE',  ( 147.0276296945837373, 275.9876705829954062, 0.7617065417431535534 ) ) ;
#25072 = DIRECTION ( 'NONE',  ( -0.8660254037844387076, -0.4999999999999998890, -0.000000000000000000 ) ) ;
#25073 = ORIENTED_EDGE ( 'NONE', *, *, #22460, .T. ) ;
#25074 = CARTESIAN_POINT ( 'NONE',  ( 181.1647404240839023, 268.1795203863183588, 15.36725951381329480 ) ) ;
#25075 = CARTESIAN_POINT ( 'NONE',  ( 109.6190968851625911, 246.3464784336661353, 1.353441290958777327E-15 ) ) ;
#25076 = CARTESIAN_POINT ( 'NONE',  ( 15.51250667149479590, 27.14336893147754992, 7.433330006724141015 ) ) ;
#25077 = CARTESIAN_POINT ( 'NONE',  ( 75.03548522729336412, 67.17073137636660363, 12.58381819018166325 ) ) ;
#25078 = CYLINDRICAL_SURFACE ( 'NONE', #64581, 10.00000000000001066 ) ;
#25080 = CARTESIAN_POINT ( 'NONE',  ( -4.429217378738782962, 26.01694505731172313, -10.00000000000000000 ) ) ;
#25079 = CARTESIAN_POINT ( 'NONE',  ( 157.1338510812060747, 258.4831816688264325, 17.88958125218800888 ) ) ;
#25081 = CARTESIAN_POINT ( 'NONE',  ( 191.1456801727256618, 299.5729656239652741, -6.514204219820171282 ) ) ;
#25082 = CARTESIAN_POINT ( 'NONE',  ( 28.21526782163968861, 21.45404122711134320, -8.090169943749478065 ) ) ;
#25083 = CARTESIAN_POINT ( 'NONE',  ( 196.4783028304046013, 290.3365922432724346, -16.37291435488387492 ) ) ;
#25084 = CARTESIAN_POINT ( 'NONE',  ( 46.83931157395847578, 209.3967562850346837, 1.101618078115930403E-13 ) ) ;
#25085 = CARTESIAN_POINT ( 'NONE',  ( 174.8696466734779449, 292.3029143586743430, -1.153856708368909967 ) ) ;
#25086 = LINE ( 'NONE', #92536, #63661 ) ;
#25087 = ORIENTED_EDGE ( 'NONE', *, *, #53881, .T. ) ;
#25088 = CARTESIAN_POINT ( 'NONE',  ( 189.0480903703354727, 265.6948563348121866, 10.88985011883314513 ) ) ;
#25089 = CARTESIAN_POINT ( 'NONE',  ( 179.4583960273904211, 270.4090523040318885, 17.47970616590194837 ) ) ;
#25090 = CARTESIAN_POINT ( 'NONE',  ( 165.5845925187108492, 269.2586473770181783, -17.52824664516929332 ) ) ;
#25091 = ORIENTED_EDGE ( 'NONE', *, *, #4562, .F. ) ;
#25092 = B_SPLINE_CURVE_WITH_KNOTS ( 'NONE', 3,
 ( #40916, #49049, #79985, #39914 ),
 .UNSPECIFIED., .F., .F.,
 ( 4, 4 ),
 ( 0.008247362098805164840, 0.01450959442545752057 ),
 .UNSPECIFIED. ) ;
#25093 = CARTESIAN_POINT ( 'NONE',  ( 75.69558293296576323, 65.12864963431647425, -14.43849588152979813 ) ) ;
#25094 = CARTESIAN_POINT ( 'NONE',  ( 155.7144456569324973, 261.3779154106480291, 17.02946396951419672 ) ) ;
#25095 = CARTESIAN_POINT ( 'NONE',  ( 75.37843707191279918, 53.50823561223473490, 16.04097401286667335 ) ) ;
#25096 = CARTESIAN_POINT ( 'NONE',  ( 74.90335404720867984, 53.25525787180524873, -16.52187237106487672 ) ) ;
#25097 = CARTESIAN_POINT ( 'NONE',  ( 153.4289928607825573, 264.9001843414388873, 17.27358709529985958 ) ) ;
#25098 = EDGE_LOOP ( 'NONE', ( #94829, #22881, #63781, #6594, #96321, #29263, #94655, #16292, #15495, #50331, #29491, #59142, #40676, #77957, #68519, #4410, #85342, #32624, #89637, #4424, #91206, #28102, #89823, #6929, #14941, #72500, #6679, #88496, #26409, #4537, #23888, #85149, #57303, #94489, #42620, #93421, #75702, #16025 ) ) ;
#25099 = CARTESIAN_POINT ( 'NONE',  ( 165.1263583288683492, 286.0211790206518003, 4.421035561736735175 ) ) ;
#25100 = B_SPLINE_SURFACE_WITH_KNOTS ( 'NONE', 3, 1, ( 
 ( #77709, #70580 ),
 ( #55857, #86852 ),
 ( #55365, #47767 ),
 ( #78706, #9292 ),
 ( #40167, #71108 ),
 ( #17384, #48295 ),
 ( #9813, #65483 ),
 ( #2711, #3221 ),
 ( #34583, #34106 ),
 ( #94928, #11319 ),
 ( #11807, #4178 ),
 ( #95454, #49785 ),
 ( #18912, #72108 ),
 ( #73597, #19901 ),
 ( #10297, #73112 ),
 ( #33598, #79737 ),
 ( #80747, #80235 ),
 ( #96935, #50772 ),
 ( #42177, #64493 ),
 ( #19424, #87377 ),
 ( #64997, #26006 ),
 ( #56379, #41170 ),
 ( #48803, #81723 ),
 ( #57379, #56876 ),
 ( #25488, #17906 ),
 ( #27502, #65982 ),
 ( #58372, #88858 ),
 ( #50280, #89348 ),
 ( #87860, #88352 ),
 ( #18404, #81232 ),
 ( #35078, #12300 ) ),
 .UNSPECIFIED., .F., .F., .F.,
 ( 4, 3, 3, 3, 3, 3, 3, 3, 3, 3, 4 ),
 ( 2, 2 ),
 ( 0.000000000000000000, 0.1333490885032321271, 0.3007194338854310423, 0.4699862290245110930, 0.5844252810809297261, 0.6686540514502729016, 0.7354980260655470392, 0.8028463152565559202, 0.8633854507757028340, 0.9437142632666930542, 1.000000000000000000 ),
 ( 0.000000000000000000, 1.000000000000000000 ),
 .UNSPECIFIED. ) ;
#25101 = CARTESIAN_POINT ( 'NONE',  ( 43.01361757626971638, 27.76004757982093452, 5.678558825948272215 ) ) ;
#25102 = CYLINDRICAL_SURFACE ( 'NONE', #52983, 70.00000000000002842 ) ;
#25103 = ORIENTED_EDGE ( 'NONE', *, *, #86286, .F. ) ;
#25104 = CARTESIAN_POINT ( 'NONE',  ( 167.7541779101917712, 280.9156681186656215, 11.77209881610279574 ) ) ;
#25105 = B_SPLINE_CURVE_WITH_KNOTS ( 'NONE', 3,
 ( #42725, #79801, #19962, #3765 ),
 .UNSPECIFIED., .F., .F.,
 ( 4, 4 ),
 ( 0.008408023062891595290, 0.01478712368365756036 ),
 .UNSPECIFIED. ) ;
#25106 = CARTESIAN_POINT ( 'NONE',  ( -18.31116180715439512, 22.81812098060338911, 10.00000000000000000 ) ) ;
#25107 = CARTESIAN_POINT ( 'NONE',  ( 19.21902136474470524, 175.2365022471902307, 10.00000000000009948 ) ) ;
#25109 = EDGE_CURVE ( 'NONE', #40944, #329, #816, .T. ) ;
#25108 = ORIENTED_EDGE ( 'NONE', *, *, #97124, .F. ) ;
#25110 = CARTESIAN_POINT ( 'NONE',  ( 86.44808582675112518, 47.03435218195901513, -10.53111747673478860 ) ) ;
#25111 = CARTESIAN_POINT ( 'NONE',  ( 164.7495643159037684, 251.3192192419287494, 12.55862708640273695 ) ) ;
#25112 = CARTESIAN_POINT ( 'NONE',  ( 82.43803718576400286, 44.54370618503160983, -10.34432007801551912 ) ) ;
#25113 = CARTESIAN_POINT ( 'NONE',  ( -22.42236680055709641, 157.8615022471902591, 0.000000000000000000 ) ) ;
#25114 = CARTESIAN_POINT ( 'NONE',  ( 80.31207982290658265, 44.87798361127789093, 11.16639872694695867 ) ) ;
#25115 = CARTESIAN_POINT ( 'NONE',  ( 203.0498946958275326, 278.9542612457532869, -15.11479947333269003 ) ) ;
#25116 = B_SPLINE_CURVE_WITH_KNOTS ( 'NONE', 3,
 ( #58887, #11353, #42208, #73143, #50312, #73628, #3739, #72656, #51297, #65516, #27031, #34134 ),
 .UNSPECIFIED., .F., .F.,
 ( 4, 2, 2, 2, 2, 4 ),
 ( 0.000000000000000000, 0.1516647414800683380, 0.2274971122201024931, 0.2654132975901196123, 0.2843713902751267564, 0.3033294829601337894 ),
 .UNSPECIFIED. ) ;
#25117 = ORIENTED_EDGE ( 'NONE', *, *, #47205, .T. ) ;
#25118 = EDGE_CURVE ( 'NONE', #20654, #29718, #25040, .T. ) ;
#25119 = VERTEX_POINT ( 'NONE', #42581 ) ;
#25120 = CYLINDRICAL_SURFACE ( 'NONE', #90195, 17.82106496071139645 ) ;
#25121 = EDGE_CURVE ( 'NONE', #28762, #483, #84295, .T. ) ;
#25122 = ORIENTED_EDGE ( 'NONE', *, *, #38764, .T. ) ;
#25123 = CARTESIAN_POINT ( 'NONE',  ( 77.32958686580666097, 49.14630502970322112, -14.78873007407067419 ) ) ;
#25124 = EDGE_LOOP ( 'NONE', ( #8412, #17290, #37946, #24762, #72113, #14987 ) ) ;
#25125 = CARTESIAN_POINT ( 'NONE',  ( -44.30466402961320682, 27.54938068083718505, 177.5919119679930134 ) ) ;
#25126 = CARTESIAN_POINT ( 'NONE',  ( 155.6569868912636991, 261.0411854816857158, -17.75433477650897984 ) ) ;
#25127 = ORIENTED_EDGE ( 'NONE', *, *, #32566, .T. ) ;
#25128 = CARTESIAN_POINT ( 'NONE',  ( 164.4118148411678817, 245.8773786609274623, -1.109947685176164045 ) ) ;
#25129 = CARTESIAN_POINT ( 'NONE',  ( 190.1558484012587371, 301.2874045430920091, 3.461433172287052606 ) ) ;
#25130 = CARTESIAN_POINT ( 'NONE',  ( 48.98810889288134263, 89.24608170897542436, -10.00000000000000000 ) ) ;
#25131 = CARTESIAN_POINT ( 'NONE',  ( 147.4563929227680603, 275.2450308873625886, -3.847749617713808412 ) ) ;
#25132 = CARTESIAN_POINT ( 'NONE',  ( 153.0927037754837556, 265.4826541232073964, -16.15085267704102634 ) ) ;
#25133 = DIRECTION ( 'NONE',  ( -0.2649596321165964552, 0.4589235447807054058, -0.8480480961564325071 ) ) ;
#25134 = CARTESIAN_POINT ( 'NONE',  ( 165.5752708168755305, 245.8622137986321832, -1.085626278946311585 ) ) ;
#25135 = CARTESIAN_POINT ( 'NONE',  ( 126.4254891512956220, 252.9869531367911009, 4.594050593750046652 ) ) ;
#25136 = CARTESIAN_POINT ( 'NONE',  ( 70.60504524851407382, 60.65317718845415129, -14.59496475064744914 ) ) ;
#25137 = CARTESIAN_POINT ( 'NONE',  ( 44.29582294825809896, 31.28920272979930672, -7.433330006724141015 ) ) ;
#25138 = EDGE_LOOP ( 'NONE', ( #76927, #5817, #36821, #58986, #27494 ) ) ;
#25139 = VECTOR ( 'NONE', #96483, 1000.000000000000000 ) ;
#25141 = ORIENTED_EDGE ( 'NONE', *, *, #92878, .F. ) ;
#25140 = CARTESIAN_POINT ( 'NONE',  ( 86.73551935668791657, 43.70951659908644160, -4.914342582248948155 ) ) ;
#25142 = CARTESIAN_POINT ( 'NONE',  ( 203.6293652163894023, 276.2782967254192954, 13.37813849736390814 ) ) ;
#25143 = CARTESIAN_POINT ( 'NONE',  ( 174.2000522056604837, 283.5616462974032288, 14.37013614557462837 ) ) ;
#25144 = DIRECTION ( 'NONE',  ( -0.000000000000000000, -0.000000000000000000, -1.000000000000000000 ) ) ;
#25145 = CARTESIAN_POINT ( 'NONE',  ( 146.9870408876112151, 276.0579724588903332, 4.160141643933214617 ) ) ;
#25146 = CARTESIAN_POINT ( 'NONE',  ( 72.32316037510372553, 62.91300431845684926, 14.06911090390365082 ) ) ;
#25147 = CARTESIAN_POINT ( 'NONE',  ( 200.2093391412865060, 269.7417714514684803, 10.46510648850140157 ) ) ;
#25148 = CARTESIAN_POINT ( 'NONE',  ( 176.5581593771217399, 288.4200715899070246, -9.318063636782698111 ) ) ;
#25149 = VECTOR ( 'NONE', #64171, 1000.000000000000000 ) ;
#25150 = CARTESIAN_POINT ( 'NONE',  ( 33.22292548896825082, 27.38052372038642801, 10.00000000000000533 ) ) ;
#25151 = CARTESIAN_POINT ( 'NONE',  ( 194.9138646879852104, 291.7602453613734497, 15.86905368594769605 ) ) ;
#25152 = ORIENTED_EDGE ( 'NONE', *, *, #4714, .T. ) ;
#25154 = EDGE_CURVE ( 'NONE', #37549, #36202, #9978, .T. ) ;
#25153 = CARTESIAN_POINT ( 'NONE',  ( 194.3011251241114508, 294.1075746476782342, -14.76047579547631905 ) ) ;
#25155 = DIRECTION ( 'NONE',  ( -0.9756173257765569096, -0.2194785493951510180, 0.000000000000000000 ) ) ;
#25156 = ORIENTED_EDGE ( 'NONE', *, *, #57718, .F. ) ;
#25157 = CARTESIAN_POINT ( 'NONE',  ( 49.42830306794132866, 81.76213237698443947, 10.00000000000000000 ) ) ;
#25158 = ADVANCED_FACE ( 'NONE', ( #23642 ), #14831, .F. ) ;
#25159 = DIRECTION ( 'NONE',  ( 0.2938926261462335709, -0.5090369604551240323, 0.8090169943749504489 ) ) ;
#25160 = CARTESIAN_POINT ( 'NONE',  ( 152.1919794413566080, 267.0427544335294670, -15.42826099493241365 ) ) ;
#25161 = CARTESIAN_POINT ( 'NONE',  ( 149.7119746935222793, 271.3382486597900538, 12.05352563709836922 ) ) ;
#25162 = CARTESIAN_POINT ( 'NONE',  ( 202.4323889586180201, 280.0238125565655878, 15.69595176008160919 ) ) ;
#25164 = CARTESIAN_POINT ( 'NONE',  ( 154.8827976570641169, 277.6426042987627625, -8.977273693884303185 ) ) ;
#25163 = CARTESIAN_POINT ( 'NONE',  ( 153.2732530772018151, 270.1937817606684575, 14.03420799374948480 ) ) ;
#25165 = LINE ( 'NONE', #70262, #39736 ) ;
#25166 = ORIENTED_EDGE ( 'NONE', *, *, #70341, .T. ) ;
#25167 = CARTESIAN_POINT ( 'NONE',  ( 165.0952264510788154, 281.4963861521250124, -11.84807672454148886 ) ) ;
#25168 = AXIS2_PLACEMENT_3D ( 'NONE', #13063, #37318, #81978 ) ;
#25169 = CARTESIAN_POINT ( 'NONE',  ( 164.6244273547873718, 247.3313301143314789, -7.559144047185251125 ) ) ;
#25170 = EDGE_CURVE ( 'NONE', #53015, #43292, #29980, .T. ) ;
#25171 = CARTESIAN_POINT ( 'NONE',  ( 198.2505066714982149, 285.2670451491296149, 0.000000000000000000 ) ) ;
#25172 = CARTESIAN_POINT ( 'NONE',  ( 84.36939080006362701, 209.5177522451417929, 5.000000000000051514 ) ) ;
#25173 = CARTESIAN_POINT ( 'NONE',  ( 184.6056068049121563, 296.8943211797820823, -4.405390306300510872 ) ) ;
#25174 = AXIS2_PLACEMENT_3D ( 'NONE', #63247, #82500, #43924 ) ;
#25175 = CARTESIAN_POINT ( 'NONE',  ( 160.8891438268352374, 281.0495864612497599, 9.578199528566821996 ) ) ;
#25176 = CARTESIAN_POINT ( 'NONE',  ( 73.96424987833113107, 68.60250435897062005, 11.39670188853132160 ) ) ;
#25177 = CARTESIAN_POINT ( 'NONE',  ( -12.46307465703608841, 173.6115022471903160, -5.000000000000047962 ) ) ;
#25178 = CARTESIAN_POINT ( 'NONE',  ( 67.72630526519628802, 69.57018049443510677, 1.992863756904409867 ) ) ;
#25179 = CARTESIAN_POINT ( 'NONE',  ( -6.536213301660246167, 167.0333772461660828, 9.188101187500095079 ) ) ;
#25180 = CARTESIAN_POINT ( 'NONE',  ( 91.51436070488293240, 214.4548013555409796, -4.594050593750042211 ) ) ;
#25181 = CARTESIAN_POINT ( 'NONE',  ( 166.1309782654906257, 249.2029336093187339, -9.347746458946922132 ) ) ;
#25182 = CARTESIAN_POINT ( 'NONE',  ( 87.95730997019668962, 44.52059963167226186, -3.981301762289743085 ) ) ;
#25183 = CARTESIAN_POINT ( 'NONE',  ( 183.1207986101861138, 294.8225010653632694, -8.165837621905515320 ) ) ;
#25184 = CARTESIAN_POINT ( 'NONE',  ( 78.66865037864833710, 47.51313895851910729, 14.24506864829981190 ) ) ;
#25185 = CARTESIAN_POINT ( 'NONE',  ( 78.37684991480820429, 56.91902664479916041, 16.21588224672203538 ) ) ;
#25186 = DIRECTION ( 'NONE',  ( 0.4999999999999998890, -0.8660254037844385966, 0.000000000000000000 ) ) ;
#25187 = CARTESIAN_POINT ( 'NONE',  ( 77.70381431022140362, 61.98645263265593286, 15.63931947556489099 ) ) ;
#25189 = CARTESIAN_POINT ( 'NONE',  ( 77.54361356138011274, 49.75803992512373952, -14.96129575302290249 ) ) ;
#25188 = FACE_OUTER_BOUND ( 'NONE', #60642, .T. ) ;
#25190 = CARTESIAN_POINT ( 'NONE',  ( 207.8741656103030664, 270.5983789124053374, 5.135401317816507216 ) ) ;
#25191 = CARTESIAN_POINT ( 'NONE',  ( 165.9806062298373774, 249.4185370747466948, -9.186238584016363617 ) ) ;
#25192 = CARTESIAN_POINT ( 'NONE',  ( 76.22048776404022874, 55.73695481322819489, -16.16703596060795078 ) ) ;
#25193 = LINE ( 'NONE', #87070, #54430 ) ;
#25194 = CARTESIAN_POINT ( 'NONE',  ( 161.8882824960653579, 250.2482648971885340, -13.83574485983625557 ) ) ;
#25195 = CARTESIAN_POINT ( 'NONE',  ( 73.66914651274929327, 69.65765408683024873, 9.569081530089540877 ) ) ;
#25196 = CARTESIAN_POINT ( 'NONE',  ( 45.69611741197122257, 191.0643266524160140, 9.188101187500095079 ) ) ;
#25197 = DIRECTION ( 'NONE',  ( -0.8660254037844387076, -0.4999999999999998890, -0.000000000000000000 ) ) ;
#25198 = ADVANCED_FACE ( 'NONE', ( #3868 ), #65653, .T. ) ;
#25199 = CARTESIAN_POINT ( 'NONE',  ( 63.61184440487929947, 207.5333772461660544, 9.188101187500095079 ) ) ;
#25200 = CARTESIAN_POINT ( 'NONE',  ( 47.43014843991451102, 113.9519901285712251, -10.00000000000000000 ) ) ;
#25201 = CARTESIAN_POINT ( 'NONE',  ( 88.45958475239287111, 43.85926912372239883, -0.5941283661710237141 ) ) ;
#25202 = CARTESIAN_POINT ( 'NONE',  ( 104.9555363394041336, 224.7365022471902307, 10.00000000000009948 ) ) ;
#25204 = CARTESIAN_POINT ( 'NONE',  ( 200.1613715040462864, 283.9573301727594981, 16.94951437046174192 ) ) ;
#25203 = CARTESIAN_POINT ( 'NONE',  ( 197.9294784878310907, 286.6389924893580883, -17.36088744678619378 ) ) ;
#25205 = CARTESIAN_POINT ( 'NONE',  ( 22.90194105960797089, 172.4824982072973967, 3.021315404115420679E-15 ) ) ;
#25206 = VECTOR ( 'NONE', #15145, 1000.000000000000000 ) ;
#25207 = CARTESIAN_POINT ( 'NONE',  ( 23.65314546706850862, 31.84336893147757408, -7.433330006724137462 ) ) ;
#25208 = CARTESIAN_POINT ( 'NONE',  ( 81.13754030168745146, 45.92056744364227683, 12.30823813837155001 ) ) ;
#25209 = CARTESIAN_POINT ( 'NONE',  ( 79.57385746726255604, 47.78104568962750420, -13.55650246241271439 ) ) ;
#25210 = ORIENTED_EDGE ( 'NONE', *, *, #51662, .T. ) ;
#25211 = CARTESIAN_POINT ( 'NONE',  ( 21.16812676580727270, 15.14754757982089650, -5.678558825948276656 ) ) ;
#25212 = CARTESIAN_POINT ( 'NONE',  ( 71.86588871287597158, 221.4869531367911293, 4.594050593750046652 ) ) ;
#25213 = CARTESIAN_POINT ( 'NONE',  ( 99.70756906128829655, 216.8262482093457493, 3.021315404115420679E-15 ) ) ;
#25214 = LINE ( 'NONE', #93149, #65597 ) ;
#25215 = CARTESIAN_POINT ( 'NONE',  ( 170.0644797785468540, 289.4723839078269521, -1.148982712589306843 ) ) ;
#25216 = CARTESIAN_POINT ( 'NONE',  ( 73.85305739393403712, 66.14698956378720140, 12.75270311107614774 ) ) ;
#25217 = CARTESIAN_POINT ( 'NONE',  ( 153.6005803596509054, 264.6029860754553056, 18.07864614867099462 ) ) ;
#25218 = VECTOR ( 'NONE', #74544, 1000.000000000000000 ) ;
#25219 = CARTESIAN_POINT ( 'NONE',  ( -97.59541525468981149, 48.06504152958505216, 36.50000000000000000 ) ) ;
#25220 = CARTESIAN_POINT ( 'NONE',  ( 189.8039450987227781, 286.5139521920973493, 16.53692407126337116 ) ) ;
#25221 = CARTESIAN_POINT ( 'NONE',  ( 130.9362984529373080, 239.7365022471902307, 10.00000000000009592 ) ) ;
#25222 = CARTESIAN_POINT ( 'NONE',  ( 161.8873598795597388, 250.2498629158519350, 13.90822209621415873 ) ) ;
#25223 = CARTESIAN_POINT ( 'NONE',  ( 164.9404048476745004, 244.9618339132846074, -2.801285734921658666 ) ) ;
#25224 = ORIENTED_EDGE ( 'NONE', *, *, #54389, .F. ) ;
#25225 = CARTESIAN_POINT ( 'NONE',  ( 185.1115058749157072, 271.5392633888741898, 15.95323373308776738 ) ) ;
#25226 = VERTEX_POINT ( 'NONE', #95623 ) ;
#25227 = CARTESIAN_POINT ( 'NONE',  ( 202.7041331321765938, 279.5531378413010657, 17.14708438049711248 ) ) ;
#25228 = LINE ( 'NONE', #56115, #40089 ) ;
#25229 = CARTESIAN_POINT ( 'NONE',  ( 71.17702396458545877, 68.89634176143304956, -8.584545784728861761 ) ) ;
#25230 = ORIENTED_EDGE ( 'NONE', *, *, #82821, .F. ) ;
#25231 = CARTESIAN_POINT ( 'NONE',  ( 176.4056758504748359, 253.1994894479077800, -0.2561444540333105979 ) ) ;
#25233 = EDGE_CURVE ( 'NONE', #65090, #25284, #85371, .T. ) ;
#25232 = ORIENTED_EDGE ( 'NONE', *, *, #59302, .F. ) ;
#25234 = CARTESIAN_POINT ( 'NONE',  ( 72.32137329212656596, 71.76143927211870732, 5.594163357809725845 ) ) ;
#25235 = CARTESIAN_POINT ( 'NONE',  ( 167.5593980844118391, 247.9703659007788303, 3.535947377295492799 ) ) ;
#25236 = CARTESIAN_POINT ( 'NONE',  ( -56.29836151245349640, 34.88994676555962116, -10.00000000000000000 ) ) ;
#25237 = ORIENTED_EDGE ( 'NONE', *, *, #58367, .T. ) ;
#25238 = CARTESIAN_POINT ( 'NONE',  ( 24.12344523961532161, 25.87878583063842086, -9.188101187500006262 ) ) ;
#25239 = AXIS2_PLACEMENT_3D ( 'NONE', #18087, #79919, #70772 ) ;
#25240 = CARTESIAN_POINT ( 'NONE',  ( 84.69667606500864565, 50.48814749939704427, -13.55077694746726280 ) ) ;
#25241 = DIRECTION ( 'NONE',  ( -0.9682419296822714072, -0.2500151307524236532, 0.000000000000000000 ) ) ;
#25243 = EDGE_CURVE ( 'NONE', #53811, #15709, #25677, .T. ) ;
#25242 = DIRECTION ( 'NONE',  ( -0.8660254037844387076, -0.4999999999999998890, -0.000000000000000000 ) ) ;
#25244 = DIRECTION ( 'NONE',  ( 0.4999999999999998890, -0.8660254037844385966, 0.000000000000000000 ) ) ;
#25245 = CIRCLE ( 'NONE', #20422, 0.1418229129680828593 ) ;
#25246 = EDGE_CURVE ( 'NONE', #43827, #39443, #79906, .T. ) ;
#25247 = EDGE_LOOP ( 'NONE', ( #78005, #90715, #46808, #82389 ) ) ;
#25248 = VERTEX_POINT ( 'NONE', #26172 ) ;
#25249 = CARTESIAN_POINT ( 'NONE',  ( 186.3701877112573300, 298.6212407368254276, 1.067666278078492459 ) ) ;
#25251 = CARTESIAN_POINT ( 'NONE',  ( 194.3442947553755005, 294.0328026529847421, -15.97648891113594871 ) ) ;
#25250 = CARTESIAN_POINT ( 'NONE',  ( 163.2399645767092693, 283.8610605660015267, -2.803462861407186590 ) ) ;
#25252 = CARTESIAN_POINT ( 'NONE',  ( 81.77850890590235622, 55.52106599324014269, -15.95406647289506985 ) ) ;
#25253 = CARTESIAN_POINT ( 'NONE',  ( 154.8596847415876994, 262.4221533139083817, 17.65401077761399762 ) ) ;
#25254 = CARTESIAN_POINT ( 'NONE',  ( 36.97850982526662023, 33.30066082961424456, -10.00000000000000533 ) ) ;
#25255 = CARTESIAN_POINT ( 'NONE',  ( 204.6470611188870521, 276.1878878528713130, -13.02652554726987866 ) ) ;
#25256 = CARTESIAN_POINT ( 'NONE',  ( 163.9797515130013892, 246.6257342973991626, 4.819337769813046179 ) ) ;
#25257 = CARTESIAN_POINT ( 'NONE',  ( 76.05587244885492737, 61.43040213351050483, -15.89239421180067069 ) ) ;
#25258 = LINE ( 'NONE', #41959, #24043 ) ;
#25259 = CARTESIAN_POINT ( 'NONE',  ( 82.93486267893707975, 224.8149278399160949, -9.188101187500095079 ) ) ;
#25260 = EDGE_LOOP ( 'NONE', ( #98465, #89446, #43307, #62489 ) ) ;
#25261 = CARTESIAN_POINT ( 'NONE',  ( 191.2645787786270262, 299.3670271975948367, 7.309947121636420242 ) ) ;
#25262 = CARTESIAN_POINT ( 'NONE',  ( 78.06822720212770150, 61.43946511097403373, -16.16087495820213960 ) ) ;
#25263 = VERTEX_POINT ( 'NONE', #95113 ) ;
#25264 = B_SPLINE_CURVE_WITH_KNOTS ( 'NONE', 3,
 ( #41129, #17868, #81196, #34546 ),
 .UNSPECIFIED., .F., .F.,
 ( 4, 4 ),
 ( 0.008201218458928592747, 0.01437332038716656810 ),
 .UNSPECIFIED. ) ;
#25265 = CARTESIAN_POINT ( 'NONE',  ( 195.4001060159568510, 292.2040839064547413, -16.96545459487308705 ) ) ;
#25266 = ORIENTED_EDGE ( 'NONE', *, *, #47982, .T. ) ;
#25267 = CARTESIAN_POINT ( 'NONE',  ( 80.03413267745405335, 44.49255549320951530, -11.65001753154222186 ) ) ;
#25268 = CARTESIAN_POINT ( 'NONE',  ( 66.90444770391341933, 67.53953207032016337, 6.664260923135624459 ) ) ;
#25269 = FACE_OUTER_BOUND ( 'NONE', #77497, .T. ) ;
#25270 = CARTESIAN_POINT ( 'NONE',  ( 38.08139550823666042, 22.39040679176985904, -6.890680421881970419E-14 ) ) ;
#25271 = DIRECTION ( 'NONE',  ( 0.4999999999999998890, -0.8660254037844385966, 0.000000000000000000 ) ) ;
#25272 = CARTESIAN_POINT ( 'NONE',  ( 208.1583869480885483, 270.1060931147653719, 3.025867354224990979 ) ) ;
#25273 = CARTESIAN_POINT ( 'NONE',  ( 94.78875894111908451, 225.5333772461660544, 9.188101187500095079 ) ) ;
#25274 = ORIENTED_EDGE ( 'NONE', *, *, #56796, .T. ) ;
#25275 = ORIENTED_EDGE ( 'NONE', *, *, #94948, .F. ) ;
#25276 = EDGE_CURVE ( 'NONE', #73478, #69482, #13857, .T. ) ;
#25277 = CARTESIAN_POINT ( 'NONE',  ( 207.8136982414359579, 270.7031114674828700, -0.9536989003868096004 ) ) ;
#25278 = ORIENTED_EDGE ( 'NONE', *, *, #48586, .F. ) ;
#25279 = DIRECTION ( 'NONE',  ( -0.8660254037844387076, -0.4999999999999998890, -0.000000000000000000 ) ) ;
#25280 = CIRCLE ( 'NONE', #2664, 0.1418229129681557177 ) ;
#25281 = CARTESIAN_POINT ( 'NONE',  ( 69.89261943739826677, 69.35781508005003104, -6.634928327201882858 ) ) ;
#25282 = CARTESIAN_POINT ( 'NONE',  ( -19.65312891409030271, 93.06504152958497400, 177.5919119679930134 ) ) ;
#25283 = DIRECTION ( 'NONE',  ( -0.7763215174174805666, 0.6303371332823576312, 0.000000000000000000 ) ) ;
#25284 = VERTEX_POINT ( 'NONE', #27677 ) ;
#25285 = CARTESIAN_POINT ( 'NONE',  ( 191.9006881710348864, 296.3094005088366885, 11.25170506121845726 ) ) ;
#25286 = CARTESIAN_POINT ( 'NONE',  ( 80.76394201868582456, 45.93450986988883500, 11.85631275749819835 ) ) ;
#25287 = CARTESIAN_POINT ( 'NONE',  ( 159.2102594322688844, 254.8867369075254885, -16.13039487917589199 ) ) ;
#25288 = CARTESIAN_POINT ( 'NONE',  ( 155.6205867397425777, 262.5964510888063614, -17.36443500069399093 ) ) ;
#25289 = LINE ( 'NONE', #33918, #38202 ) ;
#25290 = B_SPLINE_CURVE_WITH_KNOTS ( 'NONE', 3,
 ( #60490, #98034, #51416, #76239, #14423, #59496, #30111, #75234, #75732, #13919, #5815, #45789, #36703, #6317, #37208, #68109, #99033, #29617, #29130, #28612, #91448, #22010, #82865, #6813, #99528, #83857, #52906, #53403, #84352, #36206, #90474, #14899, #98540, #37694, #68605, #22509, #67109, #44797, #38185, #76709, #7304, #69101, #28115, #58989, #67610, #20537, #21524, #82377, #12947, #43808 ),
 .UNSPECIFIED., .F., .F.,
 ( 4, 2, 2, 2, 2, 2, 2, 2, 2, 2, 2, 2, 2, 2, 2, 2, 2, 2, 2, 2, 2, 2, 2, 2, 4 ),
 ( 0.0002547070572390182255, 0.001273486803321399090, 0.001782876676362517721, 0.002037571612883104250, 0.002164919081143416597, 0.002292266549403729377, 0.002419614017664041723, 0.002546961485924354503, 0.002801656422445068968, 0.003311046295486411595, 0.004329826041568941158, 0.005348605787651470288, 0.005857995660692657224, 0.006112690597213250691, 0.006367385533733843292, 0.006431059267864082732, 0.006494733001994320437, 0.006558406736124559010, 0.006622080470254797582, 0.006876775406775844680, 0.007386165279818052501, 0.007640860216339145569, 0.007895555152860238637, 0.008150250089381331706, 0.008404945025902424774 ),
 .UNSPECIFIED. ) ;
#25291 = VECTOR ( 'NONE', #7972, 1000.000000000000000 ) ;
#25292 = CARTESIAN_POINT ( 'NONE',  ( 81.19656099875513178, 43.43094936621162105, -9.896970666190501476 ) ) ;
#25293 = CARTESIAN_POINT ( 'NONE',  ( 195.4175937697542338, 279.6204996462902272, -17.14456379506867023 ) ) ;
#25294 = ORIENTED_EDGE ( 'NONE', *, *, #67322, .T. ) ;
#25295 = CARTESIAN_POINT ( 'NONE',  ( -37.33262083840143930, 163.6868197944959036, -37.49999999999995737 ) ) ;
#25296 = CARTESIAN_POINT ( 'NONE',  ( 161.1238074876215478, 251.5723744529297505, 13.42537408252843179 ) ) ;
#25297 = CARTESIAN_POINT ( 'NONE',  ( 152.7730629122270898, 271.2363297891400293, 14.33490734661111610 ) ) ;
#25298 = CARTESIAN_POINT ( 'NONE',  ( 187.8785148445833215, 266.1283279326300431, -11.85110462984868462 ) ) ;
#25299 = CARTESIAN_POINT ( 'NONE',  ( 83.22496320156969318, 52.34403607930074287, 14.85522145549952100 ) ) ;
#25300 = CARTESIAN_POINT ( 'NONE',  ( 175.5190374892232228, 290.1926326353742525, -6.256965731148535603 ) ) ;
#25301 = CARTESIAN_POINT ( 'NONE',  ( 152.7730629122270898, 271.2363297891400293, 14.33490734661111610 ) ) ;
#25302 = ORIENTED_EDGE ( 'NONE', *, *, #59224, .F. ) ;
#25303 = EDGE_CURVE ( 'NONE', #89390, #1098, #15430, .T. ) ;
#25304 = VECTOR ( 'NONE', #76127, 1000.000000000000114 ) ;
#25305 = CARTESIAN_POINT ( 'NONE',  ( 164.8329445879545290, 245.1479605429143760, -2.955380775890217304 ) ) ;
#25306 = CARTESIAN_POINT ( 'NONE',  ( 74.15368421650904907, 55.28562771191141678, 16.12354357782822589 ) ) ;
#25307 = CARTESIAN_POINT ( 'NONE',  ( 176.1244130302606834, 285.2676080955770885, -13.06404472828928398 ) ) ;
#25308 = CARTESIAN_POINT ( 'NONE',  ( 33.14931559527707350, 20.10801979619930435, 3.090169943749476733 ) ) ;
#25309 = CARTESIAN_POINT ( 'NONE',  ( 95.35708811412658292, 225.8615022471902591, -10.00000000000009592 ) ) ;
#25310 = CARTESIAN_POINT ( 'NONE',  ( 155.2193237801463113, 261.7992402267395846, -18.58295809893692407 ) ) ;
#25311 = CARTESIAN_POINT ( 'NONE',  ( 138.1418008908465822, 79.75620593067000641, 5.188172501216618598E-14 ) ) ;
#25312 = CARTESIAN_POINT ( 'NONE',  ( 160.3714828861807860, 272.7013802378941136, -14.85790459234098471 ) ) ;
#25313 = AXIS2_PLACEMENT_3D ( 'NONE', #56840, #38770, #774 ) ;
#25314 = CARTESIAN_POINT ( 'NONE',  ( 192.1413729726642714, 262.2891126618652606, 2.981852608854113296 ) ) ;
#25315 = CARTESIAN_POINT ( 'NONE',  ( 161.6127771116929921, 250.7254542206800352, -12.96229604595372464 ) ) ;
#25316 =( BOUNDED_CURVE ( )  B_SPLINE_CURVE ( 2, ( #79253, #24499, #40686, #55377, #86866, #86363, #71625, #65010, #40180, #1724, #10314, #10814, #2221 ),
 .UNSPECIFIED., .F., .T. ) 
 B_SPLINE_CURVE_WITH_KNOTS ( ( 3, 2, 2, 2, 2, 2, 3 ),
 ( 0.2625000000000000111, 0.2650000000000000133, 0.2700000000000000178, 0.2750000000000000222, 0.2800000000000000266, 0.2849999999999999756, 0.2874999999999999778 ),
 .UNSPECIFIED. ) 
 CURVE ( )  GEOMETRIC_REPRESENTATION_ITEM ( )  RATIONAL_B_SPLINE_CURVE ( ( 0.9755282581475768211, 0.9755282581475768211, 1.000000000000000000, 0.9510565162951535312, 1.000000000000000000, 0.9510565162951535312, 1.000000000000000000, 0.9510565162951535312, 1.000000000000000000, 0.9510565162951535312, 1.000000000000000000, 0.9755282581475768211, 0.9755282581475768211 ) ) 
 REPRESENTATION_ITEM ( '' )  );
#25317 = CARTESIAN_POINT ( 'NONE',  ( 8.700681467995980967, 166.6423013555410080, -4.594050593750043987 ) ) ;
#25318 = DIRECTION ( 'NONE',  ( 1.000000000000000000, 0.000000000000000000, 0.000000000000000000 ) ) ;
#25319 = ORIENTED_EDGE ( 'NONE', *, *, #67714, .T. ) ;
#25320 = CARTESIAN_POINT ( 'NONE',  ( 174.8858495065613852, 255.2716098750472042, 8.953978856888550553 ) ) ;
#25321 = CARTESIAN_POINT ( 'NONE',  ( -17.42236680055705023, 149.2012482093457777, 0.000000000000000000 ) ) ;
#25322 = FACE_OUTER_BOUND ( 'NONE', #13067, .T. ) ;
#25323 = CARTESIAN_POINT ( 'NONE',  ( 82.35608806024791306, 41.41197313041440253, 5.516391017443479150 ) ) ;
#25324 = CARTESIAN_POINT ( 'NONE',  ( 17.82075117977708700, 181.0958772461660544, -9.188101187500095079 ) ) ;
#25325 = DIRECTION ( 'NONE',  ( -0.5000000000000002220, 0.8660254037844385966, -9.251858538542986372E-17 ) ) ;
#25326 = CARTESIAN_POINT ( 'NONE',  ( 40.95666657127031840, 28.81029122506297924, 8.090169943749479842 ) ) ;
#25327 = CARTESIAN_POINT ( 'NONE',  ( 199.6968473295422939, 267.3144708874781372, -6.730990908593314614 ) ) ;
#25328 = CARTESIAN_POINT ( 'NONE',  ( 191.1000148935602567, 299.6520602076213891, -9.462302242170249400 ) ) ;
#25329 = CARTESIAN_POINT ( 'NONE',  ( 197.0455264951692129, 289.3541320366447280, 17.54437334811087368 ) ) ;
#25330 = DIRECTION ( 'NONE',  ( -1.000000000000000000, 0.000000000000000000, 0.000000000000000000 ) ) ;
#25331 = CARTESIAN_POINT ( 'NONE',  ( 4.743097115929088226, 26.23654200823200000, 1.583844403245363353 ) ) ;
#25332 = CARTESIAN_POINT ( 'NONE',  ( 190.0885270318794937, 298.7835894469523623, -8.138652993139137592 ) ) ;
#25333 = CARTESIAN_POINT ( 'NONE',  ( 84.04820955589276821, 51.68058956114519731, 14.75728579592695588 ) ) ;
#25334 = CARTESIAN_POINT ( 'NONE',  ( 85.03695205236203947, 213.2365022471901739, -10.00000000000009059 ) ) ;
#25335 = CARTESIAN_POINT ( 'NONE',  ( 74.82470458544302971, 65.83378423986729899, -13.33277362726854776 ) ) ;
#25336 = CARTESIAN_POINT ( 'NONE',  ( 41.51553799054924099, 59.02985107750643579, 10.00000000000000000 ) ) ;
#25337 = CARTESIAN_POINT ( 'NONE',  ( 42.65610334793076674, 64.00004027534475881, 10.00000000000000000 ) ) ;
#25338 = CARTESIAN_POINT ( 'NONE',  ( 37.03551627836181126, 198.3149278399160664, 9.188101187500093303 ) ) ;
#25339 = LINE ( 'NONE', #95800, #66577 ) ;
#25340 = CARTESIAN_POINT ( 'NONE',  ( 205.7753384153419631, 271.2832105871503927, -6.565646494404037803 ) ) ;
#25341 = CARTESIAN_POINT ( 'NONE',  ( 190.8907028847385448, 300.0145992415348815, -5.421341690443150618 ) ) ;
#25342 = FACE_OUTER_BOUND ( 'NONE', #14291, .T. ) ;
#25343 = EDGE_LOOP ( 'NONE', ( #86511, #20558, #46139, #35271 ) ) ;
#25344 = CARTESIAN_POINT ( 'NONE',  ( 166.1070111784138703, 253.4115428555481344, -13.60050710122670559 ) ) ;
#25345 = DIRECTION ( 'NONE',  ( -0.000000000000000000, -0.000000000000000000, -1.000000000000000000 ) ) ;
#25346 = CARTESIAN_POINT ( 'NONE',  ( 159.5941974674867083, 278.9247971600711367, -11.03768485503293739 ) ) ;
#25347 = LINE ( 'NONE', #63353, #26168 ) ;
#25348 = CARTESIAN_POINT ( 'NONE',  ( 29.50362127723248662, 19.96004757982091604, -5.678558825948276656 ) ) ;
#25349 = CARTESIAN_POINT ( 'NONE',  ( 202.5511585997265911, 279.8180975037686835, 17.12781264818056925 ) ) ;
#25350 = CARTESIAN_POINT ( 'NONE',  ( 149.7109319212262051, 271.3400547943878109, -12.38605961032017433 ) ) ;
#25351 = CIRCLE ( 'NONE', #78812, 17.82106496071138224 ) ;
#25352 = CARTESIAN_POINT ( 'NONE',  ( 185.5654499382181655, 267.7323668493922924, -14.54006482872913253 ) ) ;
#25353 = ORIENTED_EDGE ( 'NONE', *, *, #7992, .T. ) ;
#25354 = VECTOR ( 'NONE', #17789, 1000.000000000000000 ) ;
#25355 = CARTESIAN_POINT ( 'NONE',  ( 5.869580825389008716, 26.49540643055185640, 3.479690158560446702E-15 ) ) ;
#25356 = CARTESIAN_POINT ( 'NONE',  ( 79.80752115302324512, 57.35651460586262829, -16.24722079539231956 ) ) ;
#25357 = CARTESIAN_POINT ( 'NONE',  ( 71.91886814437489761, 72.60555707853946217, -1.127020781340661193 ) ) ;
#25358 = VERTEX_POINT ( 'NONE', #57049 ) ;
#25360 = EDGE_CURVE ( 'NONE', #28922, #99839, #67195, .T. ) ;
#25359 = CARTESIAN_POINT ( 'NONE',  ( -27.62287085492247485, 60.80044415029907867, -10.00000000000000000 ) ) ;
#25361 = CARTESIAN_POINT ( 'NONE',  ( 81.93820057532437318, 58.80319216612334543, 0.3078307376628310332 ) ) ;
#25362 = CARTESIAN_POINT ( 'NONE',  ( 110.0000000000000000, -8.000000000000000000, 9.212605237762131694 ) ) ;
#25363 = CARTESIAN_POINT ( 'NONE',  ( 149.3833831332874240, 271.9073859370555510, 11.40518020539810173 ) ) ;
#25364 = EDGE_CURVE ( 'NONE', #28623, #31851, #74783, .T. ) ;
#25365 = ORIENTED_EDGE ( 'NONE', *, *, #98313, .F. ) ;
#25366 = ORIENTED_EDGE ( 'NONE', *, *, #79415, .T. ) ;
#25368 = CARTESIAN_POINT ( 'NONE',  ( 46.08672700828314106, 69.01776843458345922, 177.5919119679930134 ) ) ;
#25367 = CARTESIAN_POINT ( 'NONE',  ( -21.95578541582649379, 35.16639575222019687, 59.99999999999999289 ) ) ;
#25369 = ORIENTED_EDGE ( 'NONE', *, *, #33162, .F. ) ;
#25370 = CARTESIAN_POINT ( 'NONE',  ( 152.8651171364917900, 265.8768457450651113, -16.25664868183201861 ) ) ;
#25371 = EDGE_CURVE ( 'NONE', #19698, #15824, #13471, .T. ) ;
#25372 = CARTESIAN_POINT ( 'NONE',  ( 172.8964584746522917, 253.4886925110870664, 9.877074417240217841 ) ) ;
#25373 = CARTESIAN_POINT ( 'NONE',  ( 72.73224412574886344, 56.97554388665330549, -15.91743659082035123 ) ) ;
#25374 = CARTESIAN_POINT ( 'NONE',  ( 77.20655462988578677, 63.53086439471233859, 15.45977356242439349 ) ) ;
#25376 = EDGE_CURVE ( 'NONE', #46780, #68198, #39491, .T. ) ;
#25375 = CARTESIAN_POINT ( 'NONE',  ( 204.7237927799493775, 276.0549847173622879, -12.81020997223575364 ) ) ;
#25377 = CARTESIAN_POINT ( 'NONE',  ( 99.98491136382573075, 228.5333772461660828, 9.188101187500095079 ) ) ;
#25378 = CARTESIAN_POINT ( 'NONE',  ( 41.37327796571900507, 124.7191351846657028, -10.00000000000000000 ) ) ;
#25379 = ORIENTED_EDGE ( 'NONE', *, *, #12103, .F. ) ;
#25380 = VECTOR ( 'NONE', #14471, 1000.000000000000000 ) ;
#25381 = VECTOR ( 'NONE', #9200, 1000.000000000000000 ) ;
#25382 = CARTESIAN_POINT ( 'NONE',  ( 161.6083111375297108, 266.9942300563631647, 16.50555569288089686 ) ) ;
#25383 = EDGE_LOOP ( 'NONE', ( #25648, #39068, #40306, #36320 ) ) ;
#25384 = CARTESIAN_POINT ( 'NONE',  ( 25.58005199048888656, 32.95586893147756768, 7.433330006724141015 ) ) ;
#25385 = CARTESIAN_POINT ( 'NONE',  ( 157.2985995762109042, 259.4415387207266122, 17.34027181022534947 ) ) ;
#25386 = CARTESIAN_POINT ( 'NONE',  ( 67.59162108422654569, 69.94611594471417959, -2.429117792699152734 ) ) ;
#25387 = CARTESIAN_POINT ( 'NONE',  ( 58.76725448063633195, 213.9244531367911577, -4.594050593750046652 ) ) ;
#25388 = CARTESIAN_POINT ( 'NONE',  ( 73.98997032606590096, 68.61244119570729083, 11.40121143613689192 ) ) ;
#25389 = CARTESIAN_POINT ( 'NONE',  ( 190.9061255863007318, 299.9878863388391892, 7.497146773253707153 ) ) ;
#25390 = FACE_OUTER_BOUND ( 'NONE', #40036, .T. ) ;
#25392 = VECTOR ( 'NONE', #83347, 1000.000000000000227 ) ;
#25391 = LINE ( 'NONE', #47677, #12385 ) ;
#25393 = VERTEX_POINT ( 'NONE', #28155 ) ;
#25394 = CARTESIAN_POINT ( 'NONE',  ( 75.36396396989580637, 58.32137975822279685, -15.97037604966454438 ) ) ;
#25395 = CARTESIAN_POINT ( 'NONE',  ( 177.7443685448805581, 288.9686455644151124, 11.17637150946867841 ) ) ;
#25396 = CARTESIAN_POINT ( 'NONE',  ( 147.6088797830324779, 274.9809158978982850, 8.531536684623960198 ) ) ;
#25397 = VERTEX_POINT ( 'NONE', #59529 ) ;
#25398 = CARTESIAN_POINT ( 'NONE',  ( 171.9697486346997266, 259.6717877315294345, -13.86376714732617543 ) ) ;
#25399 = CARTESIAN_POINT ( 'NONE',  ( 174.1708078612628583, 277.4829975439923828, -15.60795485462966425 ) ) ;
#25400 = CARTESIAN_POINT ( 'NONE',  ( 207.1770866921659717, 271.8057550155037347, -5.569195235244989384 ) ) ;
#25401 = CARTESIAN_POINT ( 'NONE',  ( 193.1444937042664094, 296.1109190324805240, -12.15243020627156767 ) ) ;
#25402 = CARTESIAN_POINT ( 'NONE',  ( 180.8863484661150949, 271.3550751966830603, 16.94740090253783649 ) ) ;
#25403 = CARTESIAN_POINT ( 'NONE',  ( 189.7726967107949747, 264.4065126852114531, 11.24316165915873000 ) ) ;
#25404 = CARTESIAN_POINT ( 'NONE',  ( 75.98882072545443123, 65.54910008167897217, 13.91231000067740275 ) ) ;
#25405 = CARTESIAN_POINT ( 'NONE',  ( 167.7102881833664014, 256.2825055472106897, 13.57817267270622885 ) ) ;
#25406 = DIRECTION ( 'NONE',  ( -1.000000000000000000, 0.000000000000000000, 0.000000000000000000 ) ) ;
#25407 = CARTESIAN_POINT ( 'NONE',  ( 108.0499464844507997, 227.0643266524160424, 9.188101187500095079 ) ) ;
#25408 = ORIENTED_EDGE ( 'NONE', *, *, #69358, .F. ) ;
#25409 = CARTESIAN_POINT ( 'NONE',  ( 146.7818291168261453, 276.4134096722012828, -0.7617065417431535534 ) ) ;
#25410 = CARTESIAN_POINT ( 'NONE',  ( 84.11621381539826814, 42.22557305609230838, 3.174655551866189196 ) ) ;
#25411 = CARTESIAN_POINT ( 'NONE',  ( 202.7973612924478743, 279.3916619310153919, -15.54732529288344089 ) ) ;
#25412 = CARTESIAN_POINT ( 'NONE',  ( 204.1953342137782954, 276.9703018036655067, 13.84727111424505885 ) ) ;
#25413 = CARTESIAN_POINT ( 'NONE',  ( 83.60569444237076198, 51.47509952066116767, -14.39597358549856843 ) ) ;
#25414 = CARTESIAN_POINT ( 'NONE',  ( 175.3043775287472101, 252.5449758547659940, 5.231882537108772269 ) ) ;
#25415 = ORIENTED_EDGE ( 'NONE', *, *, #51791, .F. ) ;
#25416 = CARTESIAN_POINT ( 'NONE',  ( 80.58776074949071244, 57.68173972368585112, -16.24394003362809968 ) ) ;
#25417 = CARTESIAN_POINT ( 'NONE',  ( 154.5758520964906779, 273.3885357916005319, -13.22738657698927689 ) ) ;
#25418 = CARTESIAN_POINT ( 'NONE',  ( 181.9501482740564029, 260.5583091221847098, 9.820294706648617478 ) ) ;
#25419 = CARTESIAN_POINT ( 'NONE',  ( 206.6829130365991034, 272.6616888947074244, -10.15488415123734001 ) ) ;
#25420 = CARTESIAN_POINT ( 'NONE',  ( 134.8963869060034142, 254.8149278399160949, -9.188101187500095079 ) ) ;
#25421 = CARTESIAN_POINT ( 'NONE',  ( 191.8284704360776516, 295.3786271354495057, -12.12832068662400076 ) ) ;
#25422 = CARTESIAN_POINT ( 'NONE',  ( 189.0615291916986109, 299.2959719742789275, 4.846944731644502902 ) ) ;
#25423 = DIRECTION ( 'NONE',  ( -0.1963739994383812415, 0.9805290675673896672, 0.000000000000000000 ) ) ;
#25424 = CARTESIAN_POINT ( 'NONE',  ( 68.75404378773190217, 204.3768266524160140, 9.188101187500098632 ) ) ;
#25426 = ADVANCED_FACE ( 'NONE', ( #21081 ), #1146, .F. ) ;
#25425 = VECTOR ( 'NONE', #76179, 1000.000000000000000 ) ;
#25428 = CARTESIAN_POINT ( 'NONE',  ( 70.42029346824453739, 62.39263015420969083, -14.29769421334009749 ) ) ;
#25427 = VECTOR ( 'NONE', #30430, 1000.000000000000000 ) ;
#25429 = CARTESIAN_POINT ( 'NONE',  ( 204.9658583905037688, 275.6357147811169170, -12.57240504404813564 ) ) ;
#25430 = LINE ( 'NONE', #47230, #2781 ) ;
#25431 = B_SPLINE_SURFACE_WITH_KNOTS ( 'NONE', 3, 1, ( 
 ( #55655, #31868 ),
 ( #55163, #86643 ),
 ( #17174, #71900 ),
 ( #39454, #48075 ),
 ( #70378, #9604 ),
 ( #2500, #70895 ),
 ( #72411, #87661 ),
 ( #32876, #86150 ),
 ( #48593, #32384 ),
 ( #16680, #1498 ),
 ( #3016, #95234 ),
 ( #25277, #17689 ),
 ( #56163, #18194 ),
 ( #25800, #56677 ),
 ( #33905, #64792 ),
 ( #95737, #43955 ),
 ( #12595, #97215 ),
 ( #96219, #96721 ),
 ( #11104, #42457 ),
 ( #50566, #19701 ),
 ( #81516, #26783 ),
 ( #65279, #51574 ),
 ( #13095, #4990 ),
 ( #67266, #12085 ),
 ( #82020, #28266 ),
 ( #43463, #98191 ),
 ( #42946, #97698 ),
 ( #41975, #74404 ),
 ( #50078, #73885 ),
 ( #57664, #49573 ),
 ( #73392, #81037 ),
 ( #80526, #35369 ),
 ( #4477, #36361 ),
 ( #59141, #90111 ) ),
 .UNSPECIFIED., .T., .F., .F.,
 ( 4, 2, 2, 2, 2, 2, 2, 2, 2, 2, 2, 2, 2, 2, 2, 2, 4 ),
 ( 2, 2 ),
 ( 0.000000000000000000, 0.06250000000000000000, 0.1250000000000000000, 0.1875000000000000000, 0.2500000000000000000, 0.3125000000000000000, 0.3750000000000000000, 0.4375000000000000000, 0.5000000000000000000, 0.5625000000000000000, 0.6250000000000000000, 0.6875000000000000000, 0.7500000000000000000, 0.8125000000000000000, 0.8750000000000000000, 0.9375000000000000000, 1.000000000000000000 ),
 ( 0.000000000000000000, 1.000000000000000000 ),
 .UNSPECIFIED. ) ;
#25432 = CARTESIAN_POINT ( 'NONE',  ( 68.39600206231747848, 70.06355299527018587, -1.199260098510152028 ) ) ;
#25433 = CARTESIAN_POINT ( 'NONE',  ( 174.5900386765337657, 262.0875730750212824, 14.28570942272308741 ) ) ;
#25434 = CARTESIAN_POINT ( 'NONE',  ( 153.5001613412225936, 278.7771225056793583, -1.599187862637977187 ) ) ;
#25435 = CARTESIAN_POINT ( 'NONE',  ( 178.4254400080073424, 292.4993321051520070, -7.220885224839013183 ) ) ;
#25436 = CARTESIAN_POINT ( 'NONE',  ( 155.3513572141771704, 261.5705516107003064, -17.00592413546589299 ) ) ;
#25437 = CARTESIAN_POINT ( 'NONE',  ( 153.6088888397055143, 269.2756142106472339, -15.62050981732668475 ) ) ;
#25438 = AXIS2_PLACEMENT_3D ( 'NONE', #35755, #4874, #28153 ) ;
#25439 = CARTESIAN_POINT ( 'NONE',  ( 121.1754704609021900, 250.7677522451419065, -5.000000000000047962 ) ) ;
#25440 = CARTESIAN_POINT ( 'NONE',  ( 18.81282613181931040, 26.56454794089041371, 10.00000000000000355 ) ) ;
#25441 = VERTEX_POINT ( 'NONE', #39705 ) ;
#25442 = ADVANCED_FACE ( 'NONE', ( #70635 ), #32128, .T. ) ;
#25443 = CARTESIAN_POINT ( 'NONE',  ( 147.6088797830324779, 274.9809158978982850, 8.531536684623960198 ) ) ;
#25444 = CARTESIAN_POINT ( 'NONE',  ( 87.04122873496829982, 46.31593380912286761, -9.298662157179395038 ) ) ;
#25445 = CARTESIAN_POINT ( 'NONE',  ( 36.33204418566946714, 191.7833772461660544, -9.188101187500095079 ) ) ;
#25446 = CARTESIAN_POINT ( 'NONE',  ( 16.01096549046674511, 31.01751292744055988, 6.180339887498949913 ) ) ;
#25447 = CARTESIAN_POINT ( 'NONE',  ( 85.93470712620026575, 48.23248545518190866, 11.93606436224419198 ) ) ;
#25448 = CIRCLE ( 'NONE', #43231, 45.00000000000000000 ) ;
#25449 = CARTESIAN_POINT ( 'NONE',  ( 72.24503514708140983, 222.5177522451419065, 5.000000000000046185 ) ) ;
#25450 = CARTESIAN_POINT ( 'NONE',  ( 147.4317198359019301, 275.2877659273946733, 3.797273160043843188 ) ) ;
#25451 = FACE_OUTER_BOUND ( 'NONE', #38668, .T. ) ;
#25453 = CARTESIAN_POINT ( 'NONE',  ( 64.01779381112929457, 207.7677522451418497, 10.00000000000009592 ) ) ;
#25452 = DIRECTION ( 'NONE',  ( 0.3668518372888612822, 0.9302793824855987159, 0.000000000000000000 ) ) ;
#25454 = CARTESIAN_POINT ( 'NONE',  ( 174.3739577948688577, 289.3819840071309386, 7.916562535199481943 ) ) ;
#25455 = CARTESIAN_POINT ( 'NONE',  ( 163.1346087304468142, 255.9866270473322629, -14.93535196593188275 ) ) ;
#25456 = CARTESIAN_POINT ( 'NONE',  ( 5.723458822437210713, 164.1115022471902023, -5.000000000000041744 ) ) ;
#25457 = DIRECTION ( 'NONE',  ( 1.000000000000000000, 0.000000000000000000, 0.000000000000000000 ) ) ;
#25458 = ORIENTED_EDGE ( 'NONE', *, *, #40577, .T. ) ;
#25459 = CARTESIAN_POINT ( 'NONE',  ( 179.6160012257981862, 295.0481727651569486, 1.085779272287555663 ) ) ;
#25460 = CARTESIAN_POINT ( 'NONE',  ( 20.08504676852905746, 195.7365022471903444, 2.944929066748280225E-16 ) ) ;
#25461 = CARTESIAN_POINT ( 'NONE',  ( 142.0139464194155039, 261.9869531367911009, 4.594050593750046652 ) ) ;
#25462 = AXIS2_PLACEMENT_3D ( 'NONE', #86674, #3051, #95275 ) ;
#25463 = CARTESIAN_POINT ( 'NONE',  ( 162.9148248802443106, 248.4702413316674381, 9.709394404200100581 ) ) ;
#25464 = CARTESIAN_POINT ( 'NONE',  ( -0.9067010812963882671, 158.0327760586659451, 1.948934522072303157E-15 ) ) ;
#25465 = CARTESIAN_POINT ( 'NONE',  ( 36.29711636232130445, 39.14336893147758900, 7.433330006724141015 ) ) ;
#25467 = CARTESIAN_POINT ( 'NONE',  ( 200.4168219705828449, 282.9326697566199869, 16.82828662466668845 ) ) ;
#25466 = CARTESIAN_POINT ( 'NONE',  ( 164.0724714897467607, 247.3131831635135711, 6.957961843141012181 ) ) ;
#25468 = CARTESIAN_POINT ( 'NONE',  ( 153.1164404339926080, 265.4415410246681972, 16.15325778160653414 ) ) ;
#25469 = CARTESIAN_POINT ( 'NONE',  ( 22.53213034355506750, 33.98502408145593279, -5.678558825948271327 ) ) ;
#25470 = CARTESIAN_POINT ( 'NONE',  ( 156.0731593180878178, 261.2610882355718331, -17.28887939065674573 ) ) ;
#25471 = CARTESIAN_POINT ( 'NONE',  ( 183.7664330935276951, 256.7078052723039718, -1.761079896072507145 ) ) ;
#25472 = CARTESIAN_POINT ( 'NONE',  ( 66.18591460530085158, 68.59894752875132440, 2.300355685169377828 ) ) ;
#25473 = ORIENTED_EDGE ( 'NONE', *, *, #73261, .F. ) ;
#25474 = CARTESIAN_POINT ( 'NONE',  ( 196.2630260332681189, 290.7094625936034049, -17.43112004684450866 ) ) ;
#25475 = CARTESIAN_POINT ( 'NONE',  ( 29.41244916810467203, 42.77587997571678358, 10.00000000000000000 ) ) ;
#25476 = SHAPE_REPRESENTATION_RELATIONSHIP ( 'NONE' , 'NONE' ,  #94304, #88828 ) ;
#25477 = CARTESIAN_POINT ( 'NONE',  ( 16.02188117849498639, 11.11110640527290983, -2.839279412974138328 ) ) ;
#25478 = CARTESIAN_POINT ( 'NONE',  ( 165.8170486466665068, 285.4962505645767692, 0.4920860348752986169 ) ) ;
#25479 = CARTESIAN_POINT ( 'NONE',  ( 12.48623565965559479, 28.18502408145590721, 5.678558825948276656 ) ) ;
#25480 = DIRECTION ( 'NONE',  ( -0.9957145386939475484, -0.09248003802712848054, 0.000000000000000000 ) ) ;
#25481 = CARTESIAN_POINT ( 'NONE',  ( 153.7162572231245292, 275.1202623374771861, 10.51805260027509981 ) ) ;
#25482 = CARTESIAN_POINT ( 'NONE',  ( 87.98439851106198262, 44.06910850096573995, -1.717092390252117573 ) ) ;
#25483 = EDGE_CURVE ( 'NONE', #23533, #90262, #10521, .T. ) ;
#25484 = VERTEX_POINT ( 'NONE', #16931 ) ;
#25485 = CARTESIAN_POINT ( 'NONE',  ( 152.7618747630824885, 266.0556667813044101, 16.41480086888796919 ) ) ;
#25486 = CARTESIAN_POINT ( 'NONE',  ( 165.0532575723395041, 244.7663672603923715, -2.144843157699870773 ) ) ;
#25487 = CARTESIAN_POINT ( 'NONE',  ( 66.25644290789426805, 68.19202803638752641, 4.197190157902950247 ) ) ;
#25488 = CARTESIAN_POINT ( 'NONE',  ( 87.41847558182290356, 44.98594970355499356, 6.912341091792672643 ) ) ;
#25489 = CARTESIAN_POINT ( 'NONE',  ( 155.0898745997320134, 262.0234527842152374, 17.05457557403769542 ) ) ;
#25490 = ORIENTED_EDGE ( 'NONE', *, *, #5236, .T. ) ;
#25491 = ORIENTED_EDGE ( 'NONE', *, *, #29284, .F. ) ;
#25492 = CARTESIAN_POINT ( 'NONE',  ( 155.7871210497565642, 277.0951557919157722, -10.36611183180045082 ) ) ;
#25493 = CARTESIAN_POINT ( 'NONE',  ( 85.86500116153743534, 47.48139021253037839, 10.80080889994705906 ) ) ;
#25494 = ORIENTED_EDGE ( 'NONE', *, *, #70925, .T. ) ;
#25496 = EDGE_CURVE ( 'NONE', #24384, #39418, #87922, .T. ) ;
#25495 = CARTESIAN_POINT ( 'NONE',  ( 193.1318887679063039, 292.6717260935084255, 15.39800915952812588 ) ) ;
#25497 = LINE ( 'NONE', #8303, #95361 ) ;
#25498 = ORIENTED_EDGE ( 'NONE', *, *, #17580, .T. ) ;
#25500 = ADVANCED_FACE ( 'NONE', ( #72675 ), #49347, .T. ) ;
#25499 = CARTESIAN_POINT ( 'NONE',  ( 78.35410446158606135, 61.54825803293332598, -15.81517172436243790 ) ) ;
#25501 = CARTESIAN_POINT ( 'NONE',  ( 79.13712759260106111, 59.42437504702360940, -16.53516983581165434 ) ) ;
#25502 = CARTESIAN_POINT ( 'NONE',  ( 80.59841950988781889, 48.28954382714877624, -14.06662836619941892 ) ) ;
#25503 = AXIS2_PLACEMENT_3D ( 'NONE', #78022, #8612, #70403 ) ;
#25504 = CARTESIAN_POINT ( 'NONE',  ( 80.72615790689530968, 43.21908027699803512, 9.966345867180507412 ) ) ;
#25505 = ORIENTED_EDGE ( 'NONE', *, *, #211, .T. ) ;
#25506 = CARTESIAN_POINT ( 'NONE',  ( 200.7897860911934913, 282.8688841796032420, 18.17522996445731920 ) ) ;
#25507 = CARTESIAN_POINT ( 'NONE',  ( 168.3012556413555387, 276.0081633973304633, -16.37610827237247335 ) ) ;
#25508 = AXIS2_PLACEMENT_3D ( 'NONE', #91784, #84202, #14748 ) ;
#25509 = CARTESIAN_POINT ( 'NONE',  ( 150.7226148805041817, 269.5877685077668957, 15.52819754351937576 ) ) ;
#25510 = CARTESIAN_POINT ( 'NONE',  ( 29.58720089054306968, 40.58029201028043786, 1.583844403245363353 ) ) ;
#25511 = B_SPLINE_CURVE_WITH_KNOTS ( 'NONE', 3,
 ( #189, #60974, #61962, #23468 ),
 .UNSPECIFIED., .F., .F.,
 ( 4, 4 ),
 ( 0.01631437863335180247, 0.02516723697892677206 ),
 .UNSPECIFIED. ) ;
#25512 = ORIENTED_EDGE ( 'NONE', *, *, #46857, .T. ) ;
#25513 = CARTESIAN_POINT ( 'NONE',  ( 198.1063734369593590, 266.1900715569024669, 6.878534305327493215 ) ) ;
#25514 = CARTESIAN_POINT ( 'NONE',  ( 37.57390229391633341, 33.64441083166263979, -10.00000000000000533 ) ) ;
#25515 = VERTEX_POINT ( 'NONE', #40724 ) ;
#25516 = ORIENTED_EDGE ( 'NONE', *, *, #7280, .F. ) ;
#25517 = CARTESIAN_POINT ( 'NONE',  ( 160.3554891620578076, 268.8548341825590455, -16.71133067088820567 ) ) ;
#25518 = ORIENTED_EDGE ( 'NONE', *, *, #68711, .T. ) ;
#25519 = CARTESIAN_POINT ( 'NONE',  ( 160.4237162281696953, 273.2376347127639633, -15.66572034412998882 ) ) ;
#25520 = ORIENTED_EDGE ( 'NONE', *, *, #71507, .T. ) ;
#25521 = COLOUR_RGB ( '',0.7921568627450980005, 0.8196078431372548767, 0.9333333333333333481 ) ;
#25522 = CARTESIAN_POINT ( 'NONE',  ( 159.1510347580164648, 259.5013206209943064, 16.69515602809037347 ) ) ;
#25523 = CARTESIAN_POINT ( 'NONE',  ( 168.6746947616884711, 272.7949930551382636, 15.97852131846135038 ) ) ;
#25524 = CARTESIAN_POINT ( 'NONE',  ( 193.8013783128415639, 294.9731615157183455, 13.35591610390495632 ) ) ;
#25525 = CARTESIAN_POINT ( 'NONE',  ( 192.1943038168404314, 277.1473907896511264, 17.36549850453357635 ) ) ;
#25526 = DIRECTION ( 'NONE',  ( 1.000000000000000000, 0.000000000000000000, 0.000000000000000000 ) ) ;
#25527 = DIRECTION ( 'NONE',  ( 0.000000000000000000, 0.000000000000000000, 1.000000000000000000 ) ) ;
#25528 = CARTESIAN_POINT ( 'NONE',  ( 82.63376612087627393, 53.27330958937008631, -15.29856784112376822 ) ) ;
#25529 = CARTESIAN_POINT ( 'NONE',  ( 197.5889545809544927, 288.4128869818045473, -18.07878478781679732 ) ) ;
#25530 = VECTOR ( 'NONE', #15014, 1000.000000000000000 ) ;
#25531 = ORIENTED_EDGE ( 'NONE', *, *, #51563, .F. ) ;
#25532 = CARTESIAN_POINT ( 'NONE',  ( 162.7028393313443360, 279.7088927405546883, -12.24337270576748438 ) ) ;
#25533 = CARTESIAN_POINT ( 'NONE',  ( 16.91979795264450459, 27.95586893147755347, 7.433330006724141015 ) ) ;
#25534 = CARTESIAN_POINT ( 'NONE',  ( 164.8849641302980444, 245.0578600525887794, 2.884140591399200648 ) ) ;
#25535 = CARTESIAN_POINT ( 'NONE',  ( 191.1729615630557646, 298.6818583910219331, -8.222589559603353138 ) ) ;
#25537 = ORIENTED_EDGE ( 'NONE', *, *, #47229, .F. ) ;
#25536 = CARTESIAN_POINT ( 'NONE',  ( 198.2040940955416488, 287.3474340887963763, 16.95806375232200480 ) ) ;
#25538 = AXIS2_PLACEMENT_3D ( 'NONE', #43822, #36221, #69114 ) ;
#25539 = ORIENTED_EDGE ( 'NONE', *, *, #19700, .T. ) ;
#25540 = DIRECTION ( 'NONE',  ( 0.5000000000000014433, -0.8660254037844378194, 0.000000000000000000 ) ) ;
#25541 = CARTESIAN_POINT ( 'NONE',  ( 169.6843210851487527, 258.2382094438814875, -14.02289787536656185 ) ) ;
#25542 = CARTESIAN_POINT ( 'NONE',  ( 38.90461549961826648, 38.16454794089045066, -10.00000000000000355 ) ) ;
#25543 = FACE_OUTER_BOUND ( 'NONE', #55925, .T. ) ;
#25544 = CARTESIAN_POINT ( 'NONE',  ( 200.7583183585857967, 282.9233878912788214, 16.96937806979494212 ) ) ;
#25545 = DIRECTION ( 'NONE',  ( -0.8660254037844387076, -0.4999999999999998890, -0.000000000000000000 ) ) ;
#25546 = EDGE_LOOP ( 'NONE', ( #27525, #50120, #99775, #18172 ) ) ;
#25547 = CARTESIAN_POINT ( 'NONE',  ( 159.9882936611505500, 262.0288864495718144, -17.79556786074740415 ) ) ;
#25548 = CARTESIAN_POINT ( 'NONE',  ( 13.85453579343919905, 10.12755873383624383, -6.180339887498949025 ) ) ;
#25549 = VECTOR ( 'NONE', #27072, 1000.000000000000000 ) ;
#25550 = CARTESIAN_POINT ( 'NONE',  ( 134.6710330032098000, 241.8927522451418497, 10.00000000000009948 ) ) ;
#25551 = LINE ( 'NONE', #34154, #17608 ) ;
#25552 = CARTESIAN_POINT ( 'NONE',  ( 16.74724052122864393, 187.1427522451419065, 10.00000000000009237 ) ) ;
#25553 = CARTESIAN_POINT ( 'NONE',  ( 100.4182711614829486, 216.5327760586659451, 1.948934522072302763E-15 ) ) ;
#25554 = CARTESIAN_POINT ( 'NONE',  ( 82.09616139842204063, 40.74998018113815590, -0.9067466716294869666 ) ) ;
#25555 = B_SPLINE_CURVE_WITH_KNOTS ( 'NONE', 3,
 ( #24158, #39824, #55043, #71778, #56031, #16551, #47446, #78375, #17048, #63152 ),
 .UNSPECIFIED., .F., .F.,
 ( 4, 2, 2, 2, 4 ),
 ( 0.000000000000000000, 0.0002622400424273465310, 0.0005244800848546930620, 0.0007867201272820395930, 0.001048960169709386124 ),
 .UNSPECIFIED. ) ;
#25556 = CARTESIAN_POINT ( 'NONE',  ( 14.54318666465499632, 27.13478043621387314, 8.090169943749478065 ) ) ;
#25557 = CARTESIAN_POINT ( 'NONE',  ( 170.1875097353064916, 280.4626186455269590, -13.75171363026703730 ) ) ;
#25558 = CARTESIAN_POINT ( 'NONE',  ( 23.17910981781079727, 190.3149278399161233, -9.188101187500095079 ) ) ;
#25559 = EDGE_CURVE ( 'NONE', #80879, #54426, #33485, .T. ) ;
#25560 = CARTESIAN_POINT ( 'NONE',  ( 161.4396252346964218, 251.0253620690641299, 14.51972485405798885 ) ) ;
#25561 = ORIENTED_EDGE ( 'NONE', *, *, #35687, .F. ) ;
#25562 = VERTEX_POINT ( 'NONE', #34152 ) ;
#25563 = CARTESIAN_POINT ( 'NONE',  ( 200.1200414979239213, 267.3440445008968709, -2.849651934370048600 ) ) ;
#25564 = EDGE_CURVE ( 'NONE', #100252, #30838, #48857, .T. ) ;
#25565 = CARTESIAN_POINT ( 'NONE',  ( 67.37707244819222296, 69.01508689139724595, 3.611659466110988870 ) ) ;
#25566 = CARTESIAN_POINT ( 'NONE',  ( 29.75882387383049377, 25.38052372038642446, 10.00000000000000533 ) ) ;
#25567 = CARTESIAN_POINT ( 'NONE',  ( -22.42236680055709641, 157.8615022471902591, 0.000000000000000000 ) ) ;
#25568 = CARTESIAN_POINT ( 'NONE',  ( 192.7288556637334125, 292.1918731402626577, -15.52061534916644447 ) ) ;
#25569 = CARTESIAN_POINT ( 'NONE',  ( 69.10817959322751847, 64.24658173014449858, 12.03926405174448000 ) ) ;
#25570 = CARTESIAN_POINT ( 'NONE',  ( 74.06641568892433725, 68.90029856846140888, -11.17356148674937444 ) ) ;
#25571 = CARTESIAN_POINT ( 'NONE',  ( 29.83685365728618066, 188.0333772461660544, 9.188101187500095079 ) ) ;
#25572 = CARTESIAN_POINT ( 'NONE',  ( 80.11143256479013530, 210.3927522451417929, 10.00000000000009592 ) ) ;
#25573 = AXIS2_PLACEMENT_3D ( 'NONE', #9272, #39137, #85836 ) ;
#25574 = CARTESIAN_POINT ( 'NONE',  ( 97.79278455872238851, 227.2677522451418497, 10.00000000000009592 ) ) ;
#25575 = ORIENTED_EDGE ( 'NONE', *, *, #62756, .F. ) ;
#25576 = ADVANCED_FACE ( 'NONE', ( #41222 ), #18459, .T. ) ;
#25577 = CARTESIAN_POINT ( 'NONE',  ( 83.47332239865056636, 45.96411348524937068, 10.52733798611148508 ) ) ;
#25578 = CARTESIAN_POINT ( 'NONE',  ( 178.9086871400862719, 258.8446539160876796, -10.04105931206729529 ) ) ;
#25579 = AXIS2_PLACEMENT_3D ( 'NONE', #16824, #39104, #40112 ) ;
#25580 = CARTESIAN_POINT ( 'NONE',  ( 0.1211834420501121806, 177.0024278399160949, -9.188101187500093303 ) ) ;
#25581 = CIRCLE ( 'NONE', #38497, 60.00000000000002132 ) ;
#25582 = CARTESIAN_POINT ( 'NONE',  ( 68.94203703131894656, 64.31246542778407616, -11.91225929259457672 ) ) ;
#25583 = CARTESIAN_POINT ( 'NONE',  ( 198.9369963555428740, 286.0780101374919013, -18.58432392708837710 ) ) ;
#25584 = CARTESIAN_POINT ( 'NONE',  ( 186.6165385818496247, 282.6660768309312743, 16.17880700807253191 ) ) ;
#25585 = CARTESIAN_POINT ( 'NONE',  ( 147.6512387128590262, 274.9075480792844246, -8.209968531507987777 ) ) ;
#25586 = CARTESIAN_POINT ( 'NONE',  ( 87.98594423550160570, 43.75089820288621212, -2.253463800273092676 ) ) ;
#25587 = CARTESIAN_POINT ( 'NONE',  ( 164.4294002498235159, 245.8469198396639399, 6.098783631055905374 ) ) ;
#25588 = CARTESIAN_POINT ( 'NONE',  ( 191.5893301551938350, 298.8045413135534432, -8.323356515452589477 ) ) ;
#25589 = DIRECTION ( 'NONE',  ( 1.000000000000000000, 1.962715704248044129E-13, 0.000000000000000000 ) ) ;
#25590 = EDGE_CURVE ( 'NONE', #27771, #60705, #99864, .T. ) ;
#25591 = ORIENTED_EDGE ( 'NONE', *, *, #55712, .T. ) ;
#25592 = VECTOR ( 'NONE', #60066, 1000.000000000000000 ) ;
#25593 = CARTESIAN_POINT ( 'NONE',  ( -21.58168810074490551, 24.33735145887881757, -10.00000000000000000 ) ) ;
#25594 = CARTESIAN_POINT ( 'NONE',  ( 99.22679203974932705, 240.3464784336661637, 1.353441290958777327E-15 ) ) ;
#25595 = CARTESIAN_POINT ( 'NONE',  ( 21.54279312762077936, 14.29860640527291871, -2.839279412974138328 ) ) ;
#25596 = CARTESIAN_POINT ( 'NONE',  ( 75.18968313674336912, 67.03148441216438869, 12.73605655727703123 ) ) ;
#25597 = CARTESIAN_POINT ( 'NONE',  ( 35.87196818813498567, 201.5177522451419350, 5.000000000000046185 ) ) ;
#25598 = VECTOR ( 'NONE', #69969, 1000.000000000000114 ) ;
#25600 = CARTESIAN_POINT ( 'NONE',  ( 185.5365472822558672, 288.1719225632029406, 15.10228555286701813 ) ) ;
#25599 = LINE ( 'NONE', #54981, #51680 ) ;
#25601 = CARTESIAN_POINT ( 'NONE',  ( 191.0098866877199271, 299.8081668393321024, -6.439016407525185670 ) ) ;
#25602 = ORIENTED_EDGE ( 'NONE', *, *, #65306, .F. ) ;
#25603 = CARTESIAN_POINT ( 'NONE',  ( 190.2102363550532118, 262.0023303024768779, -4.404598936143417909 ) ) ;
#25604 = CARTESIAN_POINT ( 'NONE',  ( 149.2223635749290622, 272.1862799931444670, -12.97307652490353647 ) ) ;
#25605 = CARTESIAN_POINT ( 'NONE',  ( 192.0603001030472683, 293.3461588932823929, -14.68827779892621344 ) ) ;
#25606 = CARTESIAN_POINT ( 'NONE',  ( 173.1401207867795335, 289.7447317016536772, -1.382016094127694217 ) ) ;
#25607 = CARTESIAN_POINT ( 'NONE',  ( 81.56781671333388317, 55.98423300004855463, -16.39433532902865309 ) ) ;
#25608 = VERTEX_POINT ( 'NONE', #65044 ) ;
#25609 = CARTESIAN_POINT ( 'NONE',  ( 75.31289280905393468, 53.62176160565092431, -16.53289957284814449 ) ) ;
#25610 = CARTESIAN_POINT ( 'NONE',  ( 175.4103267356181846, 278.8476840418515508, 15.42183127757729189 ) ) ;
#25611 = CARTESIAN_POINT ( 'NONE',  ( 166.1693173614613102, 270.1811453668383933, -16.28491390599275590 ) ) ;
#25612 = EDGE_CURVE ( 'NONE', #84918, #89501, #79790, .T. ) ;
#25613 = CARTESIAN_POINT ( 'NONE',  ( 71.97456596565469056, 72.60744930783874906, 1.463844530419991852 ) ) ;
#25614 = CARTESIAN_POINT ( 'NONE',  ( 199.4244589065890523, 272.3134371430058422, 12.33418413535176761 ) ) ;
#25615 = DIRECTION ( 'NONE',  ( -0.000000000000000000, 0.000000000000000000, -1.000000000000000000 ) ) ;
#25616 = CARTESIAN_POINT ( 'NONE',  ( 72.29675234079142854, 71.91852905550483399, -5.160928375136445645 ) ) ;
#25617 = CARTESIAN_POINT ( 'NONE',  ( 148.2992785150285613, 274.6248789480700907, 6.993002833606254853 ) ) ;
#25618 = EDGE_CURVE ( 'NONE', #47527, #74125, #11376, .T. ) ;
#25619 = CIRCLE ( 'NONE', #54722, 70.00000000000001421 ) ;
#25620 = CARTESIAN_POINT ( 'NONE',  ( 191.2498569334766216, 280.2133405228250354, 17.23712193076469745 ) ) ;
#25621 = CARTESIAN_POINT ( 'NONE',  ( 36.41018743920069056, 41.99752408145594273, 5.678558825948277544 ) ) ;
#25622 = CARTESIAN_POINT ( 'NONE',  ( 192.1027933011355344, 288.1354424464720410, -15.86813138701040060 ) ) ;
#25623 = EDGE_LOOP ( 'NONE', ( #57896, #51189, #6668, #32941 ) ) ;
#25624 = CARTESIAN_POINT ( 'NONE',  ( 77.72420466810140738, 61.55156736199941037, 16.09483585134336181 ) ) ;
#25626 = ADVANCED_FACE ( 'NONE', ( #50332 ), #10855, .T. ) ;
#25625 = CARTESIAN_POINT ( 'NONE',  ( 147.9791529310278122, 274.3395839928920168, -7.789432462804474433 ) ) ;
#25627 = CARTESIAN_POINT ( 'NONE',  ( 87.74907107289486419, 44.16117455547063742, -4.521424286948807492 ) ) ;
#25628 = VERTEX_POINT ( 'NONE', #4229 ) ;
#25630 = EDGE_CURVE ( 'NONE', #74475, #14940, #41730, .T. ) ;
#25629 = CARTESIAN_POINT ( 'NONE',  ( 78.70723262944966336, 59.87900897892416197, 16.12280052229424498 ) ) ;
#25631 = CARTESIAN_POINT ( 'NONE',  ( 188.8123896052067607, 293.6903704042900358, 12.84215840511197193 ) ) ;
#25632 = B_SPLINE_CURVE_WITH_KNOTS ( 'NONE', 3,
 ( #68033, #7220, #98954, #76635, #38104, #69017, #61418, #38616, #69524, #136 ),
 .UNSPECIFIED., .F., .F.,
 ( 4, 2, 2, 2, 4 ),
 ( 0.000000000000000000, 0.2500000000000000000, 0.5000000000000000000, 0.7500000000000000000, 1.000000000000000000 ),
 .UNSPECIFIED. ) ;
#25633 = CARTESIAN_POINT ( 'NONE',  ( 17.41845772768865075, 33.55466486950699334, -1.111400068045478839E-16 ) ) ;
#25634 = CARTESIAN_POINT ( 'NONE',  ( 198.2391837281077756, 286.3575794386269422, 17.25947343406376078 ) ) ;
#25635 = CARTESIAN_POINT ( 'NONE',  ( 79.65090360336043318, 51.49598528711052836, -15.19126888219039451 ) ) ;
#25636 = CARTESIAN_POINT ( 'NONE',  ( 80.55107469691334643, 44.51596713245550063, 11.40293197512799672 ) ) ;
#25637 = CARTESIAN_POINT ( 'NONE',  ( 27.13954536664190798, 193.1427522451419065, 10.00000000000009415 ) ) ;
#25638 = ADVANCED_FACE ( 'NONE', ( #17961 ), #57428, .T. ) ;
#25639 = ORIENTED_EDGE ( 'NONE', *, *, #11296, .T. ) ;
#25640 = EDGE_CURVE ( 'NONE', #59964, #18914, #18963, .T. ) ;
#25641 = ORIENTED_EDGE ( 'NONE', *, *, #36443, .F. ) ;
#25642 = CARTESIAN_POINT ( 'NONE',  ( 178.9149458720169719, 260.2138664454146806, 12.17723821761245695 ) ) ;
#25643 = ORIENTED_EDGE ( 'NONE', *, *, #92264, .F. ) ;
#25644 = CYLINDRICAL_SURFACE ( 'NONE', #46748, 16.60714546451156792 ) ;
#25645 = ORIENTED_EDGE ( 'NONE', *, *, #88683, .T. ) ;
#25646 = CARTESIAN_POINT ( 'NONE',  ( 173.3860743566676774, 270.4884716614657805, 17.09475665396154298 ) ) ;
#25647 = CARTESIAN_POINT ( 'NONE',  ( 155.5322964227545413, 261.2571557083629159, -18.35853982030605280 ) ) ;
#25648 = ORIENTED_EDGE ( 'NONE', *, *, #37624, .T. ) ;
#25649 = CARTESIAN_POINT ( 'NONE',  ( 186.1509274190741223, 282.5035783377156804, -17.04520025225239266 ) ) ;
#25650 = CARTESIAN_POINT ( 'NONE',  ( 165.0817809681736037, 244.7169632896033136, -1.727194264083430131 ) ) ;
#25651 = CARTESIAN_POINT ( 'NONE',  ( 189.9593806053207459, 301.6276967477073754, 3.110130642237009191 ) ) ;
#25652 = DIRECTION ( 'NONE',  ( 0.8660254037844339337, 0.5000000000000081046, -0.000000000000000000 ) ) ;
#25653 = LINE ( 'NONE', #56534, #72621 ) ;
#25654 = CIRCLE ( 'NONE', #48349, 3.299999999999998934 ) ;
#25655 = CARTESIAN_POINT ( 'NONE',  ( 200.7484899876179441, 282.9404111291507888, -16.88964748465601673 ) ) ;
#25656 = PLANE ( 'NONE',  #12939 ) ;
#25658 = CARTESIAN_POINT ( 'NONE',  ( 155.9389183335434552, 280.0307964060903601, 2.100540160644290832 ) ) ;
#25657 = TOROIDAL_SURFACE ( 'NONE', #45084, 16.10714546451156437, 0.5000000000000000000 ) ;
#25659 = CARTESIAN_POINT ( 'NONE',  ( 129.7002344832967538, 251.8149278399160949, -9.188101187500095079 ) ) ;
#25660 = CARTESIAN_POINT ( 'NONE',  ( 70.64756877957057668, 61.00196420740825687, -14.45602737464827392 ) ) ;
#25661 = CARTESIAN_POINT ( 'NONE',  ( 44.05945362601616466, 27.29860640527295956, -2.839279412974138328 ) ) ;
#25662 = VECTOR ( 'NONE', #93464, 1000.000000000000000 ) ;
#25663 = EDGE_LOOP ( 'NONE', ( #3357, #52186, #89888, #23561 ) ) ;
#25665 = ORIENTED_EDGE ( 'NONE', *, *, #54183, .T. ) ;
#25664 = CARTESIAN_POINT ( 'NONE',  ( 88.33748333995926316, 44.07075497373335793, -2.898134731201833070 ) ) ;
#25666 = CARTESIAN_POINT ( 'NONE',  ( 203.5059372267095625, 276.4897655546087663, 14.10020651900479294 ) ) ;
#25667 = LINE ( 'NONE', #56027, #91730 ) ;
#25668 = CARTESIAN_POINT ( 'NONE',  ( 173.8869354466250456, 290.5925258257277619, -4.931910953996751168 ) ) ;
#25669 = CARTESIAN_POINT ( 'NONE',  ( -66.55019942848203129, 42.78701949053055387, 10.00000000000000000 ) ) ;
#25670 = CARTESIAN_POINT ( 'NONE',  ( 156.5044409881847685, 278.9616761084025143, 7.288134256061602478 ) ) ;
#25671 = CARTESIAN_POINT ( 'NONE',  ( 153.0790963368640689, 265.5062228982576471, -17.74594954892339160 ) ) ;
#25672 = CARTESIAN_POINT ( 'NONE',  ( 79.07351061557720584, 55.41849508022395554, 16.50442470572476594 ) ) ;
#25673 = CARTESIAN_POINT ( 'NONE',  ( 207.5270645556383329, 271.1995755744450207, 0.000000000000000000 ) ) ;
#25674 = CARTESIAN_POINT ( 'NONE',  ( 155.0568450317760494, 264.0806616740677555, 17.52241723436104337 ) ) ;
#25675 = VECTOR ( 'NONE', #99299, 999.9999999999998863 ) ;
#25676 = ORIENTED_EDGE ( 'NONE', *, *, #81062, .T. ) ;
#25677 = LINE ( 'NONE', #34751, #12215 ) ;
#25678 = CARTESIAN_POINT ( 'NONE',  ( 188.6826127332440421, 272.6057162039079458, 16.71479996418005243 ) ) ;
#25679 = EDGE_LOOP ( 'NONE', ( #23869, #36088, #48076, #42930 ) ) ;
#25680 = CARTESIAN_POINT ( 'NONE',  ( 163.6128237694224765, 277.6105145936779763, 13.01957428213605361 ) ) ;
#25681 = CARTESIAN_POINT ( 'NONE',  ( 204.0366409255401834, 269.1163672225195000, -2.920898469201972159 ) ) ;
#25682 = B_SPLINE_CURVE_WITH_KNOTS ( 'NONE', 3,
 ( #78242, #8823, #76257, #24522 ),
 .UNSPECIFIED., .F., .F.,
 ( 4, 4 ),
 ( 0.005090543101624064523, 0.01311434132611732917 ),
 .UNSPECIFIED. ) ;
#25683 = CARTESIAN_POINT ( 'NONE',  ( 191.6828115734357425, 298.6426267475946474, -9.425347171908683208 ) ) ;
#25684 = CARTESIAN_POINT ( 'NONE',  ( 149.5593209768671841, 271.6026526530012575, 11.55487339793564949 ) ) ;
#25685 = CARTESIAN_POINT ( 'NONE',  ( 202.9093905060991005, 279.1976216410395182, 16.97070083370504179 ) ) ;
#25687 = CARTESIAN_POINT ( 'NONE',  ( 160.9037366693648039, 281.5822211133703945, 5.837102615454335286 ) ) ;
#25686 = CARTESIAN_POINT ( 'NONE',  ( 164.5925561631139260, 283.7481285952978283, -6.766772729352702243 ) ) ;
#25688 = AXIS2_PLACEMENT_3D ( 'NONE', #29423, #14227, #60297 ) ;
#25689 = DIRECTION ( 'NONE',  ( -0.8660254037844387076, -0.4999999999999998890, -0.000000000000000000 ) ) ;
#25690 = ORIENTED_EDGE ( 'NONE', *, *, #77199, .F. ) ;
#25691 = PRODUCT_DEFINITION_SHAPE ( 'NONE', 'NONE',  #100301 ) ;
#25692 = CARTESIAN_POINT ( 'NONE',  ( 74.39841895140679640, 68.21392270468032848, 11.95628786500076579 ) ) ;
#25693 = CARTESIAN_POINT ( 'NONE',  ( 191.5557312797294287, 275.2428672974049277, -15.79654600051574498 ) ) ;
#25694 = CARTESIAN_POINT ( 'NONE',  ( 71.74349412889739597, 65.94227022788277282, -11.98261597976729753 ) ) ;
#25695 = CARTESIAN_POINT ( 'NONE',  ( 204.2663578856130755, 276.4680603110491575, 13.28230551973123852 ) ) ;
#25696 = CARTESIAN_POINT ( 'NONE',  ( 74.38015889281619764, 68.44084013566667579, 11.75477996513195045 ) ) ;
#25697 = CARTESIAN_POINT ( 'NONE',  ( 81.19029346057565988, 43.43118860823614114, -9.901472530966298535 ) ) ;
#25698 = CARTESIAN_POINT ( 'NONE',  ( 67.18445374837708073, 69.11489579876541711, 2.756726376966783132 ) ) ;
#25699 = CARTESIAN_POINT ( 'NONE',  ( 25.96864935082050252, 154.0458036431183189, -21.50000000000001421 ) ) ;
#25700 = CARTESIAN_POINT ( 'NONE',  ( 91.08134800299070832, 214.2048013555409796, 4.594050593750051981 ) ) ;
#25701 = CARTESIAN_POINT ( 'NONE',  ( 203.5477091018662748, 278.0920214017542662, -16.09930363698006062 ) ) ;
#25702 = CARTESIAN_POINT ( 'NONE',  ( 146.7943851877206214, 276.3916619194686746, -4.608908220452185844 ) ) ;
#25703 = LINE ( 'NONE', #71812, #4265 ) ;
#25704 = EDGE_CURVE ( 'NONE', #99455, #62377, #15325, .T. ) ;
#25705 = CARTESIAN_POINT ( 'NONE',  ( -22.42236680055709641, 157.8615022471902591, 0.000000000000000000 ) ) ;
#25706 = CARTESIAN_POINT ( 'NONE',  ( 49.04287251715432205, 95.72274150194785136, -10.00000000000000000 ) ) ;
#25707 = DIRECTION ( 'NONE',  ( 0.000000000000000000, 1.000000000000000000, 0.000000000000000000 ) ) ;
#25708 = CARTESIAN_POINT ( 'NONE',  ( 161.3547410062914480, 281.8923609553542065, 5.601659783808949911 ) ) ;
#25710 = CARTESIAN_POINT ( 'NONE',  ( 76.61888230030999125, 51.35972145264445032, 16.07233720539656119 ) ) ;
#25709 = CARTESIAN_POINT ( 'NONE',  ( 5.530962353892125094, 15.14441083166257584, 0.000000000000000000 ) ) ;
#25711 = CARTESIAN_POINT ( 'NONE',  ( 207.4925036560929925, 271.2594368084131702, 4.868688772655199948 ) ) ;
#25712 = B_SPLINE_CURVE_WITH_KNOTS ( 'NONE', 3,
 ( #28348, #90202, #43032, #88725, #95821, #20776, #82615, #26374, #57251, #88225, #44035, #21267, #28864, #98277, #59742, #83094, #74976, #5557, #90711, #52145, #93409, #94406, #62965, #33068, #8771, #55348, #669, #40149, #9791, #2185, #63470, #24468, #10278, #56356, #47261, #64473, #40652, #1689, #78182, #39640, #23959, #95433, #63962, #41148, #32053, #94904, #70562, #78687 ),
 .UNSPECIFIED., .F., .F.,
 ( 4, 2, 2, 2, 2, 2, 2, 2, 2, 2, 2, 2, 2, 2, 2, 2, 2, 2, 2, 2, 2, 2, 2, 4 ),
 ( 0.0005725079143340260123, 0.001009693989615074224, 0.001228287027255563256, 0.001337583546075807664, 0.001446880064896052288, 0.001556176583716296913, 0.001665473102536541104, 0.001884066140176979612, 0.002321252215457800250, 0.003195624366019438924, 0.004069996516581078465, 0.004944368667142717139, 0.005381554742423579410, 0.005600147780063974984, 0.005709444298884176240, 0.005764092558294238271, 0.005818740817704299434, 0.005873389077114361465, 0.005928037336524423495, 0.006037333855344682865, 0.006255926892985246707, 0.006693112968266370921, 0.007130299043547496003, 0.007567485118828620218 ),
 .UNSPECIFIED. ) ;
#25713 = EDGE_CURVE ( 'NONE', #47742, #99040, #10618, .T. ) ;
#25714 = CARTESIAN_POINT ( 'NONE',  ( 205.1568691672349871, 275.3048744110253097, -13.82554525023989989 ) ) ;
#25715 = DIRECTION ( 'NONE',  ( 1.000000000000000000, 2.149074569095838299E-13, 0.000000000000000000 ) ) ;
#25716 = CARTESIAN_POINT ( 'NONE',  ( 77.47733472172021152, 54.59384519352943954, -16.52087748544757417 ) ) ;
#25717 = ADVANCED_FACE ( 'NONE', ( #97461 ), #22109, .F. ) ;
#25718 = CARTESIAN_POINT ( 'NONE',  ( 66.43953443436691941, 68.06212878376058484, -4.898982275787033380 ) ) ;
#25719 = CARTESIAN_POINT ( 'NONE',  ( 39.47103917862304456, 205.8464784336661637, 1.353441290958777327E-15 ) ) ;
#25720 = CARTESIAN_POINT ( 'NONE',  ( 76.77731254116882553, 64.09355814141257213, -15.16545583891343263 ) ) ;
#25721 = AXIS2_PLACEMENT_3D ( 'NONE', #62017, #31621, #30652 ) ;
#25722 = CARTESIAN_POINT ( 'NONE',  ( 69.07880331415105957, 204.5643266524160140, 9.188101187500095079 ) ) ;
#25723 = CARTESIAN_POINT ( 'NONE',  ( 164.6517207862732164, 247.1756023946066989, -7.101760799815486358 ) ) ;
#25724 = CARTESIAN_POINT ( 'NONE',  ( -22.42236680055709641, 157.8615022471902591, 0.000000000000000000 ) ) ;
#25725 = CARTESIAN_POINT ( 'NONE',  ( 164.1326753310708284, 258.2664819102902243, 15.54305778615748501 ) ) ;
#25727 = DIRECTION ( 'NONE',  ( 0.8660254037844379305, 0.5000000000000014433, 0.000000000000000000 ) ) ;
#25726 = DIRECTION ( 'NONE',  ( 0.000000000000000000, -0.000000000000000000, -1.000000000000000000 ) ) ;
#25728 = VECTOR ( 'NONE', #3405, 1000.000000000000114 ) ;
#25729 = DIRECTION ( 'NONE',  ( -0.8660254037844379305, -0.5000000000000016653, -3.252519625699479034E-16 ) ) ;
#25730 = CARTESIAN_POINT ( 'NONE',  ( 33.38390286057418166, 24.98920272979928470, 7.433330006724137462 ) ) ;
#25731 = CARTESIAN_POINT ( 'NONE',  ( 81.33727068537973537, 46.45028969087891824, 12.62407423705470144 ) ) ;
#25732 = CARTESIAN_POINT ( 'NONE',  ( 196.4783028304046013, 290.3365922432724346, -16.37291435488387492 ) ) ;
#25733 = ORIENTED_EDGE ( 'NONE', *, *, #65744, .T. ) ;
#25734 = CARTESIAN_POINT ( 'NONE',  ( 14.85459438965255607, 31.68290643055187061, 3.479690158560446702E-15 ) ) ;
#25735 = CARTESIAN_POINT ( 'NONE',  ( 80.68904315757745849, 208.2048013555409796, 4.594050593750051981 ) ) ;
#25736 = FACE_OUTER_BOUND ( 'NONE', #5550, .T. ) ;
#25737 = VECTOR ( 'NONE', #85524, 1000.000000000000114 ) ;
#25738 = CARTESIAN_POINT ( 'NONE',  ( 169.3079978421220630, 288.1705777629971976, -1.100478215856383279 ) ) ;
#25739 = CARTESIAN_POINT ( 'NONE',  ( -32.76508427577140736, 94.18386203199597162, 10.41389758979254587 ) ) ;
#25740 = CARTESIAN_POINT ( 'NONE',  ( 153.7968043968548386, 264.2631160733518527, 16.53979738298849611 ) ) ;
#25741 = B_SPLINE_CURVE_WITH_KNOTS ( 'NONE', 3,
 ( #52315, #74656, #6218, #75144, #59400, #7208, #36610, #37602, #91861, #14811, #90376, #30012, #53309, #51837, #90880, #82777, #98447, #67517 ),
 .UNSPECIFIED., .F., .F.,
 ( 4, 2, 2, 2, 2, 2, 2, 2, 4 ),
 ( 1.387778780781445676E-17, 0.0002767872370572536196, 0.0005535744741144933614, 0.0008303617111717331032, 0.001107148948228972845, 0.001383936185286212695, 0.001660723422343452329, 0.001937510659400691962, 0.002214297896457931812 ),
 .UNSPECIFIED. ) ;
#25742 = CARTESIAN_POINT ( 'NONE',  ( 86.47115166784590201, 47.25330420953332577, 10.74459335058070941 ) ) ;
#25743 = CARTESIAN_POINT ( 'NONE',  ( 189.8136429382303731, 286.6226720265459562, 16.81544881319448592 ) ) ;
#25744 = CARTESIAN_POINT ( 'NONE',  ( 120.0388121219830708, 240.1115022471902307, 10.00000000000009592 ) ) ;
#25745 = CARTESIAN_POINT ( 'NONE',  ( 157.6668627405778409, 257.5599783937680058, -16.78811156090270629 ) ) ;
#25746 = ADVANCED_FACE ( 'NONE', ( #78137 ), #1130, .T. ) ;
#25747 = CARTESIAN_POINT ( 'NONE',  ( 75.24899567225237718, 53.31857512432304702, 16.02918851208695017 ) ) ;
#25748 = ORIENTED_EDGE ( 'NONE', *, *, #94596, .F. ) ;
#25749 = CARTESIAN_POINT ( 'NONE',  ( 188.2088990708346614, 273.3690300468384180, 15.62809882445249876 ) ) ;
#25750 = ORIENTED_EDGE ( 'NONE', *, *, #73887, .T. ) ;
#25751 = CARTESIAN_POINT ( 'NONE',  ( 159.9770824720811220, 253.5585604421560788, -16.42166711341322483 ) ) ;
#25752 = FACE_OUTER_BOUND ( 'NONE', #69, .T. ) ;
#25753 = DIRECTION ( 'NONE',  ( -0.3978777116982054607, -0.7304723483372553838, -0.5550706935593476832 ) ) ;
#25754 = ORIENTED_EDGE ( 'NONE', *, *, #50687, .T. ) ;
#25755 = CARTESIAN_POINT ( 'NONE',  ( 174.7476935608443114, 252.4984142128707845, -0.2521487975539727922 ) ) ;
#25756 = VERTEX_POINT ( 'NONE', #9224 ) ;
#25758 = EDGE_CURVE ( 'NONE', #22001, #52344, #70516, .T. ) ;
#25757 = CARTESIAN_POINT ( 'NONE',  ( 189.3112218707861700, 290.0744326881770689, 14.37879668408311495 ) ) ;
#25759 = CARTESIAN_POINT ( 'NONE',  ( 50.59440005247052596, 190.0177522451418213, 5.000000000000051514 ) ) ;
#25760 = B_SPLINE_CURVE_WITH_KNOTS ( 'NONE', 3,
 ( #93594, #94597, #24653, #25151, #87028, #18074, #90506, #13469, #66653, #80919, #97581, #51955, #12475, #65651, #50452, #44338 ),
 .UNSPECIFIED., .F., .F.,
 ( 4, 2, 2, 2, 2, 2, 2, 4 ),
 ( 3.103167691559091397E-17, 0.0003787177898468203126, 0.0007574355796936096171, 0.001136153369540402825, 0.001514871159387196032, 0.001893588949233989023, 0.002272306739080782664, 0.003029742318774367345 ),
 .UNSPECIFIED. ) ;
#25761 = CARTESIAN_POINT ( 'NONE',  ( 81.70949458604077620, 44.04605918311328594, 10.26744876709650534 ) ) ;
#25762 = CIRCLE ( 'NONE', #53280, 0.1418229129680863287 ) ;
#25763 = VERTEX_POINT ( 'NONE', #15811 ) ;
#25764 = CARTESIAN_POINT ( 'NONE',  ( 36.79557518129325899, 43.01751292744059896, 6.180339887498949913 ) ) ;
#25765 = ADVANCED_FACE ( 'NONE', ( #46716 ), #30207, .T. ) ;
#25766 = CARTESIAN_POINT ( 'NONE',  ( 34.51575008502857855, 31.87878583063843863, -9.188101187500006262 ) ) ;
#25767 = CARTESIAN_POINT ( 'NONE',  ( 84.83932634351975821, 50.31781210311571328, -13.41000248947998941 ) ) ;
#25768 = CARTESIAN_POINT ( 'NONE',  ( 85.69676750305241342, 47.72673510730739821, -11.08893409868475821 ) ) ;
#25769 = LINE ( 'NONE', #88113, #43299 ) ;
#25770 = DIRECTION ( 'NONE',  ( -0.8660254037844387076, -0.4999999999999998890, -0.000000000000000000 ) ) ;
#25771 = ORIENTED_EDGE ( 'NONE', *, *, #21052, .F. ) ;
#25772 = EDGE_LOOP ( 'NONE', ( #29970, #94432, #75758, #615 ) ) ;
#25773 = CARTESIAN_POINT ( 'NONE',  ( 183.1259174442036510, 295.7551109177733792, 0.9378797900342676908 ) ) ;
#25775 = CARTESIAN_POINT ( 'NONE',  ( 194.9636675848471441, 292.9600174435121289, -15.57898232594655319 ) ) ;
#25774 = CARTESIAN_POINT ( 'NONE',  ( 68.22205435732229262, 65.90345407231323804, 10.80313017776371254 ) ) ;
#25776 = CARTESIAN_POINT ( 'NONE',  ( -72.30469571560091424, 48.86078274006645472, -10.00000000000000000 ) ) ;
#25777 = CARTESIAN_POINT ( 'NONE',  ( 194.2321518193436987, 294.2270399159019121, 13.98132384850917020 ) ) ;
#25778 = CARTESIAN_POINT ( 'NONE',  ( 185.3422210113485562, 292.6085084928443507, -11.74510369913683761 ) ) ;
#25779 = CARTESIAN_POINT ( 'NONE',  ( 70.88228214377448921, 60.99952434776093924, 15.04298896821893727 ) ) ;
#25780 = CARTESIAN_POINT ( 'NONE',  ( 164.0017338887578546, 246.5876597057176696, 4.694633606064320119 ) ) ;
#25781 = DIRECTION ( 'NONE',  ( 0.08498217737243618508, 0.9963824715083258177, 0.000000000000000000 ) ) ;
#25782 = CARTESIAN_POINT ( 'NONE',  ( 69.95523204135936624, 62.90150226501648234, 13.86126985460704653 ) ) ;
#25783 = CARTESIAN_POINT ( 'NONE',  ( 86.39896429407481548, 226.8149278399160664, 9.188101187500093303 ) ) ;
#25784 = ORIENTED_EDGE ( 'NONE', *, *, #88057, .F. ) ;
#25785 = CARTESIAN_POINT ( 'NONE',  ( 73.76988841918569051, 55.47430203404649518, -16.58764015103525580 ) ) ;
#25786 = CARTESIAN_POINT ( 'NONE',  ( 77.87641386972968860, 61.39850456329286743, -16.14647179981831115 ) ) ;
#25787 = ORIENTED_EDGE ( 'NONE', *, *, #5397, .T. ) ;
#25788 = CARTESIAN_POINT ( 'NONE',  ( 195.5498780363893729, 291.9446711575129711, -17.20314750324050834 ) ) ;
#25789 = ORIENTED_EDGE ( 'NONE', *, *, #29293, .F. ) ;
#25790 = CARTESIAN_POINT ( 'NONE',  ( 80.02161912385248854, 44.37003809598091664, -11.54766014928761386 ) ) ;
#25791 = DIRECTION ( 'NONE',  ( 1.000000000000000000, 0.000000000000000000, 0.000000000000000000 ) ) ;
#25792 = DIRECTION ( 'NONE',  ( -0.9634819383873028942, 0.2491829092639709919, -0.09803281150813239475 ) ) ;
#25793 = CARTESIAN_POINT ( 'NONE',  ( 35.76051414856368638, 25.81029122506296858, 8.090169943749479842 ) ) ;
#25794 = CARTESIAN_POINT ( 'NONE',  ( 206.7893622945242385, 272.4773133715531230, -10.52881283832460291 ) ) ;
#25795 = DIRECTION ( 'NONE',  ( 0.000000000000000000, -0.000000000000000000, -1.000000000000000000 ) ) ;
#25796 = CARTESIAN_POINT ( 'NONE',  ( 91.91987624320061911, 230.0024278399160949, 9.188101187500095079 ) ) ;
#25797 = ORIENTED_EDGE ( 'NONE', *, *, #79029, .T. ) ;
#25798 = VERTEX_POINT ( 'NONE', #65418 ) ;
#25799 = DIRECTION ( 'NONE',  ( -0.8660254037844384856, -0.5000000000000002220, -3.252519625699449945E-16 ) ) ;
#25800 = CARTESIAN_POINT ( 'NONE',  ( 207.6837091943624785, 270.9282591014416539, -1.156610046911421552 ) ) ;
#25801 = ORIENTED_EDGE ( 'NONE', *, *, #20412, .T. ) ;
#25802 = EDGE_CURVE ( 'NONE', #61069, #78457, #46742, .T. ) ;
#25803 = AXIS2_PLACEMENT_3D ( 'NONE', #36665, #65583, #73696 ) ;
#25804 = FACE_OUTER_BOUND ( 'NONE', #18681, .T. ) ;
#25805 = CARTESIAN_POINT ( 'NONE',  ( 21.47138989493050332, 31.13478043621388736, 8.090169943749478065 ) ) ;
#25806 = CARTESIAN_POINT ( 'NONE',  ( 67.97625722659998360, 69.06288173737418390, -4.661947418481645400 ) ) ;
#25807 = CARTESIAN_POINT ( 'NONE',  ( 87.79103035407327127, 45.19801466894013942, -6.906962003849810294 ) ) ;
#25808 = LINE ( 'NONE', #56683, #26704 ) ;
#25809 = CARTESIAN_POINT ( 'NONE',  ( 87.79117399615233808, 44.76081256804975794, 4.995967170566625093 ) ) ;
#25810 = AXIS2_PLACEMENT_3D ( 'NONE', #63820, #9128, #1542 ) ;
#25811 = VERTEX_POINT ( 'NONE', #96361 ) ;
#25812 = CARTESIAN_POINT ( 'NONE',  ( 204.3646970165318351, 276.6769568243839217, 14.33703115251539018 ) ) ;
#25813 = CARTESIAN_POINT ( 'NONE',  ( 81.33832127110852639, 47.47515066021468044, 12.76697642013896505 ) ) ;
#25814 = DIRECTION ( 'NONE',  ( -0.8660254037844387076, -0.4999999999999998890, -0.000000000000000000 ) ) ;
#25815 = CARTESIAN_POINT ( 'NONE',  ( 192.2600176540098857, 271.9115477842126438, 14.16314048194649544 ) ) ;
#25816 = CARTESIAN_POINT ( 'NONE',  ( 71.45874632471999632, 59.24191456302641257, -15.76368813740517538 ) ) ;
#25817 = CARTESIAN_POINT ( 'NONE',  ( 76.28872632190459058, 51.00282802105012081, -16.03419075268624994 ) ) ;
#25818 = FACE_OUTER_BOUND ( 'NONE', #91358, .T. ) ;
#25819 = ORIENTED_EDGE ( 'NONE', *, *, #11861, .F. ) ;
#25820 = CARTESIAN_POINT ( 'NONE',  ( 149.0764958053571263, 274.4627432579617334, 9.065804115783038242 ) ) ;
#25821 = VECTOR ( 'NONE', #100194, 1000.000000000000114 ) ;
#25822 = CARTESIAN_POINT ( 'NONE',  ( 161.1027382213887336, 251.6088674925233022, 13.55451100897754557 ) ) ;
#25823 = CARTESIAN_POINT ( 'NONE',  ( 86.54292033101232562, 46.25028892199808439, 8.970843135639702481 ) ) ;
#25824 = CARTESIAN_POINT ( 'NONE',  ( 24.48906155743269508, 15.10801979619929014, 3.090169943749476733 ) ) ;
#25825 = CARTESIAN_POINT ( 'NONE',  ( 78.38601017018802963, 61.50250219569392129, 16.18534724403903269 ) ) ;
#25826 = CARTESIAN_POINT ( 'NONE',  ( 178.3941412731578851, 291.5035416958068595, -6.132204003346442001 ) ) ;
#25827 = CARTESIAN_POINT ( 'NONE',  ( 163.1017244536801343, 248.1465217745638654, -10.44344155757014114 ) ) ;
#25828 = B_SPLINE_CURVE_WITH_KNOTS ( 'NONE', 3,
 ( #16805, #9213, #31002, #40087, #92842, #23393, #9737, #55779, #86770, #54283, #17306, #71531, #41596, #56296, #64917, #57298, #19342, #4102 ),
 .UNSPECIFIED., .F., .F.,
 ( 4, 2, 2, 2, 2, 2, 2, 2, 4 ),
 ( 0.000000000000000000, 0.0002735155329757442671, 0.0005470310659514885342, 0.0008205465989272328012, 0.001094062131902977068, 0.001367577664878721335, 0.001641093197854465602, 0.001914608730830209870, 0.002188124263805954137 ),
 .UNSPECIFIED. ) ;
#25829 = VERTEX_POINT ( 'NONE', #71542 ) ;
#25830 = ADVANCED_FACE ( 'NONE', ( #33018 ), #37001, .F. ) ;
#25831 = CARTESIAN_POINT ( 'NONE',  ( 164.9836323268835940, 244.8869617230113249, -2.696511969808454534 ) ) ;
#25832 = CARTESIAN_POINT ( 'NONE',  ( 182.3781704481015140, 264.5827396642109193, 13.45902643938770638 ) ) ;
#25833 = CARTESIAN_POINT ( 'NONE',  ( 176.0733391018527527, 285.3569424919562607, -13.18445672484209830 ) ) ;
#25834 = EDGE_CURVE ( 'NONE', #31218, #74638, #45101, .T. ) ;
#25835 = CARTESIAN_POINT ( 'NONE',  ( 29.70092825881656751, 40.08080186712595605, -3.090169943749475845 ) ) ;
#25836 = FACE_OUTER_BOUND ( 'NONE', #16784, .T. ) ;
#25837 = CARTESIAN_POINT ( 'NONE',  ( 180.4423813072727967, 272.9747474098779207, 17.19032754332442181 ) ) ;
#25838 = CARTESIAN_POINT ( 'NONE',  ( 161.0025371176779174, 273.2044621363186820, -15.07898562200838199 ) ) ;
#25839 = CARTESIAN_POINT ( 'NONE',  ( 150.5438776023515004, 278.3016033182416322, -9.804454847755098641E-05 ) ) ;
#25840 = EDGE_CURVE ( 'NONE', #75907, #58283, #44587, .T. ) ;
#25841 = CARTESIAN_POINT ( 'NONE',  ( 161.8150574665248200, 250.3750943687383881, -13.25074899737357903 ) ) ;
#25842 = CARTESIAN_POINT ( 'NONE',  ( -5.237175195983594378, 167.7833772461660828, -9.188101187500095079 ) ) ;
#25843 = CARTESIAN_POINT ( 'NONE',  ( 81.44852512392907329, 45.72822924548952273, 11.37997471554883155 ) ) ;
#25844 = ORIENTED_EDGE ( 'NONE', *, *, #32096, .F. ) ;
#25845 = CARTESIAN_POINT ( 'NONE',  ( 86.59946856559290040, 46.34450665633656996, 9.054963042594563305 ) ) ;
#25846 = CARTESIAN_POINT ( 'NONE',  ( 81.78702560211090145, 41.63811551741589767, 5.443813600127541008 ) ) ;
#25847 = CARTESIAN_POINT ( 'NONE',  ( 40.66251830035667325, 182.0327760586659451, 1.948934522072302763E-15 ) ) ;
#25848 = CARTESIAN_POINT ( 'NONE',  ( 161.4469036912142599, 251.0127554125742222, 12.93933463576739307 ) ) ;
#25849 = LINE ( 'NONE', #17743, #11900 ) ;
#25850 = CARTESIAN_POINT ( 'NONE',  ( 36.09163463545626627, 29.03677371833804344, 10.00000000000000533 ) ) ;
#25851 = LINE ( 'NONE', #57217, #44863 ) ;
#25852 = CARTESIAN_POINT ( 'NONE',  ( 107.5017976953482446, 221.3262482093458061, 3.021315404115420679E-15 ) ) ;
#25853 = CARTESIAN_POINT ( 'NONE',  ( 149.0436225622167115, 272.4958685085585444, 12.76381714291240144 ) ) ;
#25854 = CARTESIAN_POINT ( 'NONE',  ( 182.3215694434810246, 280.0626234744391923, -16.09935857771849044 ) ) ;
#25855 = DIRECTION ( 'NONE',  ( -0.000000000000000000, -0.000000000000000000, 1.000000000000000000 ) ) ;
#25856 = CARTESIAN_POINT ( 'NONE',  ( 186.8734402896601807, 295.9231036555426044, -7.697649258255485627 ) ) ;
#25857 = CARTESIAN_POINT ( 'NONE',  ( 46.30674614090290220, 112.4688969640381231, -10.00000000000000000 ) ) ;
#25858 = CARTESIAN_POINT ( 'NONE',  ( 83.23273246114447943, 208.8615022471902023, 5.000000000000051514 ) ) ;
#25859 = CARTESIAN_POINT ( 'NONE',  ( 164.9965579215539151, 246.0088170146208597, 0.8672894934246058174 ) ) ;
#25860 = EDGE_CURVE ( 'NONE', #71283, #8735, #20314, .T. ) ;
#25861 = CARTESIAN_POINT ( 'NONE',  ( 39.76905880593325548, 23.36477965099643228, 1.583844403245330712 ) ) ;
#25862 = CARTESIAN_POINT ( 'NONE',  ( 36.16949087457737733, 197.8149278399160949, -9.188101187500095079 ) ) ;
#25863 = CARTESIAN_POINT ( 'NONE',  ( 67.28998128626176367, 66.40108913371626898, -8.819887048254448914 ) ) ;
#25864 = ORIENTED_EDGE ( 'NONE', *, *, #96849, .F. ) ;
#25865 = CARTESIAN_POINT ( 'NONE',  ( -7.503431993918264098, 84.28954770299061749, 13.68879844432522219 ) ) ;
#25866 = CARTESIAN_POINT ( 'NONE',  ( 190.1693911629507738, 301.2639477917662703, -5.112716700269980485 ) ) ;
#25868 = DIRECTION ( 'NONE',  ( 0.8660254037844378194, 0.5000000000000016653, 0.000000000000000000 ) ) ;
#25867 = VECTOR ( 'NONE', #49329, 1000.000000000000000 ) ;
#25869 = ORIENTED_EDGE ( 'NONE', *, *, #53586, .T. ) ;
#25870 = CARTESIAN_POINT ( 'NONE',  ( 73.98570270871888965, 68.92876820612470112, -11.10152750440662750 ) ) ;
#25871 = CARTESIAN_POINT ( 'NONE',  ( 168.0367729244566988, 281.8922763585110260, -11.02587170619616508 ) ) ;
#25872 = FACE_OUTER_BOUND ( 'NONE', #39798, .T. ) ;
#25873 = CARTESIAN_POINT ( 'NONE',  ( 71.24283209038772213, 66.52597613840981694, 11.86082254693358173 ) ) ;
#25874 = CARTESIAN_POINT ( 'NONE',  ( 22.00590953607929023, 34.74646525600390845, 2.839279412974139660 ) ) ;
#25875 = CARTESIAN_POINT ( 'NONE',  ( 202.2603678735342214, 280.3217618159037556, 16.49712126737133744 ) ) ;
#25876 = CARTESIAN_POINT ( 'NONE',  ( 111.2365322456207224, 223.4824982072973683, 3.021315404115420679E-15 ) ) ;
#25877 = CARTESIAN_POINT ( 'NONE',  ( 204.5482460332032986, 276.3590406018296903, 14.63243279326650814 ) ) ;
#25878 = ORIENTED_EDGE ( 'NONE', *, *, #68441, .F. ) ;
#25879 = CARTESIAN_POINT ( 'NONE',  ( 6.618913549016022912, 24.79752408145590081, -5.678558825948271327 ) ) ;
#25880 = CARTESIAN_POINT ( 'NONE',  ( 172.0974426341863932, 252.4089283455955410, 8.839998632889988883 ) ) ;
#25881 = DIRECTION ( 'NONE',  ( 0.000000000000000000, 0.000000000000000000, -1.000000000000000000 ) ) ;
#25882 = EDGE_CURVE ( 'NONE', #83882, #53490, #41904, .T. ) ;
#25883 = VERTEX_POINT ( 'NONE', #98830 ) ;
#25884 = CARTESIAN_POINT ( 'NONE',  ( 178.6998812467141420, 282.4658996288984554, 15.77537290851580032 ) ) ;
#25885 = B_SPLINE_CURVE_WITH_KNOTS ( 'NONE', 3,
 ( #93527, #39263, #79338, #31668, #32182, #23569, #23074, #62066, #47380, #46365, #17487, #100112, #24084, #93014, #77294, #92527 ),
 .UNSPECIFIED., .F., .F.,
 ( 4, 1, 2, 2, 2, 1, 2, 2, 4 ),
 ( 0.000000000000000000, 0.1249999999999998057, 0.1874999999999997224, 0.2499999999999996114, 0.5000000000000031086, 0.6250000000000028866, 0.6875000000000027756, 0.7500000000000026645, 1.000000000000000000 ),
 .UNSPECIFIED. ) ;
#25886 = CARTESIAN_POINT ( 'NONE',  ( 85.17400780349038314, 49.04769795992583425, 12.45946173256488265 ) ) ;
#25887 = DIRECTION ( 'NONE',  ( 1.082076799516502080E-16, 0.000000000000000000, 1.000000000000000000 ) ) ;
#25888 = CARTESIAN_POINT ( 'NONE',  ( 71.98077362405804536, 64.91430807166688055, -13.35472713366527486 ) ) ;
#25889 = ORIENTED_EDGE ( 'NONE', *, *, #64816, .F. ) ;
#25890 = VECTOR ( 'NONE', #59550, 1000.000000000000000 ) ;
#25891 = VERTEX_POINT ( 'NONE', #29412 ) ;
#25893 = CARTESIAN_POINT ( 'NONE',  ( 150.9171781617125134, 270.0645241841637016, -13.65841583251952684 ) ) ;
#25892 = CARTESIAN_POINT ( 'NONE',  ( 69.93330931759959412, 71.50341667604121199, 8.155205941333377477E-06 ) ) ;
#25894 = CARTESIAN_POINT ( 'NONE',  ( 149.5390997184345281, 271.6376768999995761, -11.52989534384373016 ) ) ;
#25895 = ORIENTED_EDGE ( 'NONE', *, *, #5839, .F. ) ;
#25896 = CARTESIAN_POINT ( 'NONE',  ( 153.2283961777204695, 265.2476279883323400, -17.66880461074566000 ) ) ;
#25897 = DIRECTION ( 'NONE',  ( -0.8660254037844387076, -0.4999999999999998890, -0.000000000000000000 ) ) ;
#25898 = CARTESIAN_POINT ( 'NONE',  ( 70.40987744940257187, 71.50345078331645254, -2.811369489084570183 ) ) ;
#25899 = CARTESIAN_POINT ( 'NONE',  ( 78.04364300777291419, 61.42399649461658129, -16.16113552180852508 ) ) ;
#25900 = CARTESIAN_POINT ( 'NONE',  ( 204.7519188734507622, 276.0062688943993408, -12.76027478560537531 ) ) ;
#25901 = CARTESIAN_POINT ( 'NONE',  ( 122.5830220656496579, 232.3923013555409796, 4.594050593750050204 ) ) ;
#25902 = EDGE_CURVE ( 'NONE', #74173, #49930, #18973, .T. ) ;
#25903 = CARTESIAN_POINT ( 'NONE',  ( 180.4744007604609237, 287.0154873131820636, -13.59564979728018130 ) ) ;
#25904 = EDGE_LOOP ( 'NONE', ( #3245, #5070, #84950, #12086 ) ) ;
#25905 = CARTESIAN_POINT ( 'NONE',  ( 201.3171141051938378, 281.5403940053560632, 16.35011633700059974 ) ) ;
#25906 = ORIENTED_EDGE ( 'NONE', *, *, #66106, .T. ) ;
#25907 = CARTESIAN_POINT ( 'NONE',  ( 32.78369927745970358, 30.87878583063843863, -9.188101187500006262 ) ) ;
#25908 = CARTESIAN_POINT ( 'NONE',  ( 197.8822014719394531, 287.9049684674569676, 17.88172308374019792 ) ) ;
#25909 = CARTESIAN_POINT ( 'NONE',  ( 204.6350011963004647, 275.7068757420208271, -12.64342396695018245 ) ) ;
#25910 = CARTESIAN_POINT ( 'NONE',  ( 48.80796233711527776, 208.1744531367911293, 4.594050593750047540 ) ) ;
#25911 = CARTESIAN_POINT ( 'NONE',  ( 73.98997032606590096, 68.61244119570729083, 10.90121143613688304 ) ) ;
#25912 = CARTESIAN_POINT ( 'NONE',  ( 151.4159295687746294, 268.3869122420484814, 14.78076517566594106 ) ) ;
#25913 = CARTESIAN_POINT ( 'NONE',  ( 150.3996455637841621, 270.1471677736116703, 15.13740740754872327 ) ) ;
#25914 = CARTESIAN_POINT ( 'NONE',  ( 172.6297427891187795, 271.8127495741235293, 17.53455634568126698 ) ) ;
#25915 = ORIENTED_EDGE ( 'NONE', *, *, #2735, .T. ) ;
#25916 = DIRECTION ( 'NONE',  ( 0.8660254037844395958, 0.4999999999999985567, 0.000000000000000000 ) ) ;
#25917 = DIRECTION ( 'NONE',  ( -0.2113248654052032327, -0.7886751345948027625, 0.5773502691896338357 ) ) ;
#25918 = CARTESIAN_POINT ( 'NONE',  ( 189.8147415777049218, 301.8782188922952514, -0.5019643756309712934 ) ) ;
#25919 = ORIENTED_EDGE ( 'NONE', *, *, #33960, .T. ) ;
#25920 = CARTESIAN_POINT ( 'NONE',  ( 171.7130510479120744, 259.4982484653344272, -13.85566588815878752 ) ) ;
#25921 = CARTESIAN_POINT ( 'NONE',  ( 67.53901457411087961, 69.18284913860507856, -3.335900949275148353 ) ) ;
#25922 = CARTESIAN_POINT ( 'NONE',  ( 160.5099781893591455, 258.1706592185460067, -17.21824937912870013 ) ) ;
#25923 = DIRECTION ( 'NONE',  ( 0.000000000000000000, 0.000000000000000000, 1.000000000000000000 ) ) ;
#25924 = CARTESIAN_POINT ( 'NONE',  ( 149.6877696051026305, 271.3801731027346591, 11.89134584187677390 ) ) ;
#25925 = CARTESIAN_POINT ( 'NONE',  ( 41.66351307949141614, 184.8615022471902023, 5.000000000000051514 ) ) ;
#25926 = CARTESIAN_POINT ( 'NONE',  ( 84.98744680587442701, 42.71960512013303912, -5.006987873416975710 ) ) ;
#25927 =( NAMED_UNIT ( * ) PLANE_ANGLE_UNIT ( ) SI_UNIT ( $, .RADIAN. ) );
#25928 = CARTESIAN_POINT ( 'NONE',  ( 167.4563420731973338, 256.4722478396594170, 13.70524261881715589 ) ) ;
#25929 = CARTESIAN_POINT ( 'NONE',  ( -19.65312891409030271, 93.06504152958497400, 59.99999999999999289 ) ) ;
#25930 = CARTESIAN_POINT ( 'NONE',  ( 134.8967340017684080, 242.5643266524159856, -9.188101187500093303 ) ) ;
#25931 = ORIENTED_EDGE ( 'NONE', *, *, #81673, .F. ) ;
#25932 = CARTESIAN_POINT ( 'NONE',  ( 191.0604813119340690, 299.7205343796033503, -9.270812881586136811 ) ) ;
#25933 = CARTESIAN_POINT ( 'NONE',  ( 83.20693519809137229, 41.48837047502863840, 1.928222989275212740 ) ) ;
#25934 = CARTESIAN_POINT ( 'NONE',  ( 74.32283972735670829, 55.33658384534069796, 16.60204640374922036 ) ) ;
#25935 = CARTESIAN_POINT ( 'NONE',  ( 182.7869685246910194, 285.6357107071319774, -15.76494286922655874 ) ) ;
#25936 = CARTESIAN_POINT ( 'NONE',  ( -45.75347490765857117, 28.11296735934751112, 10.00000000000000000 ) ) ;
#25937 = CARTESIAN_POINT ( 'NONE',  ( 175.5249711800137220, 253.6457629656688653, 4.969749041686572610 ) ) ;
#25938 = ORIENTED_EDGE ( 'NONE', *, *, #63705, .F. ) ;
#25939 = CARTESIAN_POINT ( 'NONE',  ( 80.09948508391848065, 57.43746099958096352, -16.59413991463535964 ) ) ;
#25940 =( BOUNDED_CURVE ( )  B_SPLINE_CURVE ( 2, ( #66140, #88507, #89497, #20056, #35739, #12455, #73256, #98050, #43326, #28627, #72780, #50929, #51940 ),
 .UNSPECIFIED., .F., .F. ) 
 B_SPLINE_CURVE_WITH_KNOTS ( ( 3, 2, 2, 2, 2, 2, 3 ),
 ( 0.4625000000000000222, 0.4650000000000000244, 0.4699999999999999734, 0.4749999999999999778, 0.4799999999999999822, 0.4849999999999999867, 0.4874999999999999889 ),
 .UNSPECIFIED. ) 
 CURVE ( )  GEOMETRIC_REPRESENTATION_ITEM ( )  RATIONAL_B_SPLINE_CURVE ( ( 0.9755282581475768211, 0.9755282581475768211, 1.000000000000000000, 0.9510565162951535312, 1.000000000000000000, 0.9510565162951535312, 1.000000000000000000, 0.9510565162951535312, 1.000000000000000000, 0.9510565162951535312, 1.000000000000000000, 0.9755282581475768211, 0.9755282581475768211 ) ) 
 REPRESENTATION_ITEM ( '' )  );
#25941 = CARTESIAN_POINT ( 'NONE',  ( 158.3969645014495882, 274.9141732135112761, -12.53854624713853028 ) ) ;
#25942 = CARTESIAN_POINT ( 'NONE',  ( 185.9504045463281443, 261.9056071599655411, 9.988078213316251563 ) ) ;
#25943 = CARTESIAN_POINT ( 'NONE',  ( 165.0424088038023456, 244.7851578786982145, -1.332161216135762105 ) ) ;
#25944 = CARTESIAN_POINT ( 'NONE',  ( 145.6409484414103588, 245.7048013555409511, 4.594050593750051981 ) ) ;
#25945 = CARTESIAN_POINT ( 'NONE',  ( -27.15312891409035601, 106.0554225863516109, 0.000000000000000000 ) ) ;
#25946 = VECTOR ( 'NONE', #45354, 1000.000000000000000 ) ;
#25947 = CARTESIAN_POINT ( 'NONE',  ( 185.9561589036855764, 296.7738594392127425, 4.656816216167465328 ) ) ;
#25948 = CARTESIAN_POINT ( 'NONE',  ( 67.16327201103491973, 67.73731889023999031, 6.573435314091262249 ) ) ;
#25949 = B_SPLINE_CURVE_WITH_KNOTS ( 'NONE', 3,
 ( #86240, #23368, #55258, #70477 ),
 .UNSPECIFIED., .F., .F.,
 ( 4, 4 ),
 ( 0.01390897628007791570, 0.02024841952128482447 ),
 .UNSPECIFIED. ) ;
#25950 = CARTESIAN_POINT ( 'NONE',  ( 59.93088934303040816, 217.6589784336661637, -6.496448406907675876E-16 ) ) ;
#25951 = CARTESIAN_POINT ( 'NONE',  ( 207.6727254509676186, 270.9472835030587703, 7.315149605389819953 ) ) ;
#25952 = CARTESIAN_POINT ( 'NONE',  ( 174.2379957965557651, 251.2590728793752248, 3.639292605338433795 ) ) ;
#25953 = ADVANCED_FACE ( 'NONE', ( #23288 ), #70395, .F. ) ;
#25954 = CARTESIAN_POINT ( 'NONE',  ( 171.1110197743758476, 259.7606215877287923, 15.15264976788713902 ) ) ;
#25955 = CARTESIAN_POINT ( 'NONE',  ( 153.0048580355102672, 278.5866977936228182, -1.606994127711936615 ) ) ;
#25956 = DIRECTION ( 'NONE',  ( -0.5000000000000043299, 0.8660254037844362651, -8.973825869789965068E-15 ) ) ;
#25957 = CARTESIAN_POINT ( 'NONE',  ( 203.0862352702880003, 278.8913175244117610, -15.09542727681365015 ) ) ;
#25958 = ADVANCED_FACE ( 'NONE', ( #69891 ), #62278, .T. ) ;
#25959 = CARTESIAN_POINT ( 'NONE',  ( 156.9763224152064822, 271.9908631200777904, -15.29896765642516776 ) ) ;
#25960 = CARTESIAN_POINT ( 'NONE',  ( 131.5677753063155251, 236.7677522451417929, -5.000000000000041744 ) ) ;
#25961 = EDGE_CURVE ( 'NONE', #59643, #50800, #78159, .T. ) ;
#25962 = CARTESIAN_POINT ( 'NONE',  ( 77.14157061559578210, 52.99909543789008382, -15.86103023851207361 ) ) ;
#25963 = EDGE_LOOP ( 'NONE', ( #50817, #81719, #18063, #84939 ) ) ;
#25964 = EDGE_CURVE ( 'NONE', #84967, #31576, #85661, .T. ) ;
#25965 = CARTESIAN_POINT ( 'NONE',  ( 147.9748066657072627, 274.3471119452502762, 9.387104374042873900 ) ) ;
#25966 = CARTESIAN_POINT ( 'NONE',  ( 2.746756816977958593, 163.2048013555410080, 4.594050593750051981 ) ) ;
#25967 = CARTESIAN_POINT ( 'NONE',  ( 49.83688814775681664, 190.3923013555410080, 4.594050593750050204 ) ) ;
#25968 = CARTESIAN_POINT ( 'NONE',  ( 15.42233441037273423, 31.83705186507753382, 3.090169943749475401 ) ) ;
#25969 = CARTESIAN_POINT ( 'NONE',  ( 43.68655075043449898, 184.4824982072973967, 3.021315404115420679E-15 ) ) ;
#25970 = FACE_OUTER_BOUND ( 'NONE', #94022, .T. ) ;
#25971 = CARTESIAN_POINT ( 'NONE',  ( 72.28517652677638239, 71.97109234898169916, -3.701588698221916829 ) ) ;
#25972 = CARTESIAN_POINT ( 'NONE',  ( 190.9380839614473473, 299.9325328093580652, -5.232187664503159752 ) ) ;
#25973 = CARTESIAN_POINT ( 'NONE',  ( 71.93359151460639112, 71.98077168563673922, 2.829254084576380723 ) ) ;
#25975 = CARTESIAN_POINT ( 'NONE',  ( 67.98707691180798918, 203.3927522451418213, -10.00000000000009059 ) ) ;
#25974 = PLANE ( 'NONE',  #2428 ) ;
#25976 = CARTESIAN_POINT ( 'NONE',  ( 127.8330407560430757, 234.6115022471901739, -5.000000000000041744 ) ) ;
#25977 = CARTESIAN_POINT ( 'NONE',  ( 163.1949325260522983, 256.0357984523876098, -14.93818428935952269 ) ) ;
#25978 = CARTESIAN_POINT ( 'NONE',  ( 157.4211152037729562, 257.9856256133486454, -16.71526195140576831 ) ) ;
#25979 = DIRECTION ( 'NONE',  ( -0.000000000000000000, 0.000000000000000000, -1.000000000000000000 ) ) ;
#25980 = CARTESIAN_POINT ( 'NONE',  ( 40.72531889205828293, 180.9865022471901455, 1.119607411625061291E-15 ) ) ;
#25981 = DIRECTION ( 'NONE',  ( 0.5000000000000048850, -0.8660254037844358210, 0.000000000000000000 ) ) ;
#25982 = CARTESIAN_POINT ( 'NONE',  ( 163.1014434023538513, 248.1470085697407058, 9.692260209037655727 ) ) ;
#25983 = CARTESIAN_POINT ( 'NONE',  ( 8.998290926605619688, 169.8768266524160140, 9.188101187500098632 ) ) ;
#25984 = CARTESIAN_POINT ( 'NONE',  ( 38.48863484149602954, 25.14754757982092670, -5.678558825948276656 ) ) ;
#25986 = PLANE ( 'NONE',  #92144 ) ;
#25985 = DIRECTION ( 'NONE',  ( 0.8660254037844379305, 0.5000000000000012212, 0.000000000000000000 ) ) ;
#25987 = CARTESIAN_POINT ( 'NONE',  ( 152.6945189806187955, 266.1723304187151484, 16.62409282110771613 ) ) ;
#25988 = CARTESIAN_POINT ( 'NONE',  ( 29.08566721201706784, 38.83396525600392124, -2.839279412974133887 ) ) ;
#25989 = CARTESIAN_POINT ( 'NONE',  ( 206.5318754762992910, 272.9232936229979032, 10.63244694018452741 ) ) ;
#25990 = CARTESIAN_POINT ( 'NONE',  ( 46.99867368304095550, 76.19044720721625197, -10.00000000000000000 ) ) ;
#25991 = DIRECTION ( 'NONE',  ( 0.5076330711061761702, -0.8615733660689098850, 0.000000000000000000 ) ) ;
#25992 = FACE_OUTER_BOUND ( 'NONE', #93448, .T. ) ;
#25993 = DIRECTION ( 'NONE',  ( -0.9041295198387040433, 0.4272584830711199100, 0.000000000000000000 ) ) ;
#25994 = CARTESIAN_POINT ( 'NONE',  ( 13.40518456965460281, 16.24335787977761925, -9.188101187500008038 ) ) ;
#25995 = CARTESIAN_POINT ( 'NONE',  ( 168.8640704870188927, 288.0653526464637935, 0.5210052316872593181 ) ) ;
#25996 = CARTESIAN_POINT ( 'NONE',  ( 18.31506083472495661, 16.28920272979926054, -7.433330006724141015 ) ) ;
#25997 = CARTESIAN_POINT ( 'NONE',  ( 160.5112507838001079, 252.6333537864655057, 16.06973146617909975 ) ) ;
#25998 = DIRECTION ( 'NONE',  ( -0.7280311630581435267, -0.6855440362341479466, 0.000000000000000000 ) ) ;
#25999 = CARTESIAN_POINT ( 'NONE',  ( 84.60239308390620749, 50.60453406874029270, -14.06751209996561158 ) ) ;
#26000 = CARTESIAN_POINT ( 'NONE',  ( 206.1615484827472358, 273.5647187912443314, -9.556459874778100883 ) ) ;
#26001 = LINE ( 'NONE', #24975, #78704 ) ;
#26002 = ORIENTED_EDGE ( 'NONE', *, *, #37953, .T. ) ;
#26003 = CARTESIAN_POINT ( 'NONE',  ( 152.9489295551198893, 265.7316783776963121, 17.71675637597311237 ) ) ;
#26004 = CARTESIAN_POINT ( 'NONE',  ( 207.6826438088389750, 270.9301044032979462, 7.252082088659585146 ) ) ;
#26005 = CARTESIAN_POINT ( 'NONE',  ( 66.28155827565299774, 68.16852158415039753, 4.313148695808196820 ) ) ;
#26006 = CARTESIAN_POINT ( 'NONE',  ( 87.26772313172064344, 45.44742106685279737, 7.124560975800460660 ) ) ;
#26007 = LINE ( 'NONE', #78707, #96995 ) ;
#26008 = VERTEX_POINT ( 'NONE', #16699 ) ;
#26009 = ORIENTED_EDGE ( 'NONE', *, *, #34192, .T. ) ;
#26010 = CARTESIAN_POINT ( 'NONE',  ( 40.82928596147627331, 60.38352576601455723, 10.00000000000000000 ) ) ;
#26011 = CARTESIAN_POINT ( 'NONE',  ( 86.29568871537288999, 47.66748683144847831, 10.73674591253165822 ) ) ;
#26012 = VERTEX_POINT ( 'NONE', #55181 ) ;
#26013 = CARTESIAN_POINT ( 'NONE',  ( 78.03746721159666322, 59.28273036852866085, 16.09598523568621076 ) ) ;
#26014 = DIRECTION ( 'NONE',  ( 0.5000000000000001110, -0.8660254037844385966, 0.000000000000000000 ) ) ;
#26015 = ORIENTED_EDGE ( 'NONE', *, *, #99895, .T. ) ;
#26016 = CARTESIAN_POINT ( 'NONE',  ( 38.34546801798370552, 23.10801979619931501, 3.090169943749476733 ) ) ;
#26017 = CARTESIAN_POINT ( 'NONE',  ( 83.96860308896397385, 48.73281357008495718, -12.68925788642582297 ) ) ;
#26018 = B_SPLINE_CURVE_WITH_KNOTS ( 'NONE', 3,
 ( #6699, #21891, #82258, #67995 ),
 .UNSPECIFIED., .F., .F.,
 ( 4, 4 ),
 ( 0.000000000000000000, 2.846293438401689159E-06 ),
 .UNSPECIFIED. ) ;
#26019 = ADVANCED_FACE ( 'NONE', ( #55672 ), #79034, .T. ) ;
#26020 = DIRECTION ( 'NONE',  ( 0.5000000000000048850, -0.8660254037844358210, 0.000000000000000000 ) ) ;
#26021 = EDGE_LOOP ( 'NONE', ( #66849, #40280, #68154, #53909 ) ) ;
#26022 = CARTESIAN_POINT ( 'NONE',  ( 173.7834928849634935, 267.2296750262562455, 17.04777296020808564 ) ) ;
#26023 = CARTESIAN_POINT ( 'NONE',  ( 206.4537138826727301, 273.0586734743599209, 11.45643784582899016 ) ) ;
#26024 = CARTESIAN_POINT ( 'NONE',  ( -19.55231060296998180, 93.16478824274193471, 59.99999999999999289 ) ) ;
#26025 = ORIENTED_EDGE ( 'NONE', *, *, #15196, .F. ) ;
#26026 = CARTESIAN_POINT ( 'NONE',  ( 171.2743479101317234, 254.4242377521371736, -11.94796457435898951 ) ) ;
#26027 = CARTESIAN_POINT ( 'NONE',  ( 163.3543347837650686, 247.7089878483399730, 10.92686688779373405 ) ) ;
#26028 = ORIENTED_EDGE ( 'NONE', *, *, #40977, .F. ) ;
#26029 = EDGE_LOOP ( 'NONE', ( #10041, #83735, #90635, #29704 ) ) ;
#26030 = CARTESIAN_POINT ( 'NONE',  ( 156.8155610647694687, 266.6398381445407040, -16.21946676759114325 ) ) ;
#26031 = ORIENTED_EDGE ( 'NONE', *, *, #81804, .F. ) ;
#26032 = CARTESIAN_POINT ( 'NONE',  ( 160.3461653528465263, 270.4748347642712929, 15.77331661139888475 ) ) ;
#26033 = ORIENTED_EDGE ( 'NONE', *, *, #49173, .T. ) ;
#26034 = CARTESIAN_POINT ( 'NONE',  ( 193.4053711441870576, 295.6590660519894982, 14.70124750960288118 ) ) ;
#26035 = CARTESIAN_POINT ( 'NONE',  ( 177.4191073644459777, 288.9051419072185922, -9.334082586762583844 ) ) ;
#26037 = EDGE_CURVE ( 'NONE', #2384, #77129, #40970, .T. ) ;
#26036 = FACE_OUTER_BOUND ( 'NONE', #45175, .T. ) ;
#26038 = CARTESIAN_POINT ( 'NONE',  ( 192.0645969571214096, 297.9813550654635605, 11.46542907566974812 ) ) ;
#26039 = CARTESIAN_POINT ( 'NONE',  ( 174.7547596240474377, 290.5425714371900199, 6.460816282008575939 ) ) ;
#26040 = CARTESIAN_POINT ( 'NONE',  ( 158.5776461130937491, 255.9824553178812323, -17.58135378896025358 ) ) ;
#26041 = EDGE_LOOP ( 'NONE', ( #39544, #36261, #25537, #71489 ) ) ;
#26042 = DIRECTION ( 'NONE',  ( 0.000000000000000000, 0.000000000000000000, 1.000000000000000000 ) ) ;
#26043 = CARTESIAN_POINT ( 'NONE',  ( 20.65934362447757167, 23.87878583063841376, -9.188101187500006262 ) ) ;
#26044 = CARTESIAN_POINT ( 'NONE',  ( 164.7462163020046262, 245.2981783406326599, 1.451255823150352064 ) ) ;
#26045 = CARTESIAN_POINT ( 'NONE',  ( 77.53919650534660946, 49.73269318645782988, -15.46600695893548227 ) ) ;
#26046 = CARTESIAN_POINT ( 'NONE',  ( 159.7608930362198407, 253.9330115291272421, 15.38895778945778581 ) ) ;
#26047 = EDGE_LOOP ( 'NONE', ( #30199, #16062, #68868, #84504 ) ) ;
#26048 = CARTESIAN_POINT ( 'NONE',  ( 146.6797637568835171, 276.5901920613147809, -3.161329895305951876 ) ) ;
#26049 = CARTESIAN_POINT ( 'NONE',  ( 171.6504431596714539, 259.4514037848667272, -15.21112824701198640 ) ) ;
#26050 = CARTESIAN_POINT ( 'NONE',  ( 163.5642666985274332, 247.7300691424477179, 7.713274332594024507 ) ) ;
#26051 = CARTESIAN_POINT ( 'NONE',  ( 85.49318370521093868, 48.99722645306705715, -12.73116331006621493 ) ) ;
#26052 = CARTESIAN_POINT ( 'NONE',  ( 199.3272761551183692, 285.4020256954596562, -18.33026947811089258 ) ) ;
#26053 = CARTESIAN_POINT ( 'NONE',  ( 191.3546420016972434, 260.9821492784607244, -0.08077186525796756222 ) ) ;
#26054 = ORIENTED_EDGE ( 'NONE', *, *, #18772, .F. ) ;
#26055 = CARTESIAN_POINT ( 'NONE',  ( 152.1671311979278016, 269.0857928536317445, 15.36489295260887822 ) ) ;
#26056 = CARTESIAN_POINT ( 'NONE',  ( 51.02741275436275004, 190.2677522451418213, -5.000000000000041744 ) ) ;
#26057 = CARTESIAN_POINT ( 'NONE',  ( 207.0548180518391916, 272.0175305127218053, 7.721676452263806389 ) ) ;
#26058 = CARTESIAN_POINT ( 'NONE',  ( 25.55183212637048840, 178.8927522451418497, 10.00000000000009592 ) ) ;
#26059 = CARTESIAN_POINT ( 'NONE',  ( 99.30858933894288043, 218.9548013555409511, -4.594050593750042211 ) ) ;
#26060 = CARTESIAN_POINT ( 'NONE',  ( 82.52994871329097748, 40.49336819921385455, -1.416186232783453125 ) ) ;
#26061 = CARTESIAN_POINT ( 'NONE',  ( 12.55362526388469746, 30.18080186712592194, 3.090169943749475401 ) ) ;
#26062 = CARTESIAN_POINT ( 'NONE',  ( 162.4702972292363086, 249.2401858085828508, 11.41296778546566060 ) ) ;
#26063 = CARTESIAN_POINT ( 'NONE',  ( 27.18482440607884243, 180.3768266524160140, 9.188101187500098632 ) ) ;
#26064 = CARTESIAN_POINT ( 'NONE',  ( 154.0986224399686648, 280.1916420498395155, 2.233781007141098396 ) ) ;
#26065 = VERTEX_POINT ( 'NONE', #24791 ) ;
#26067 = ORIENTED_EDGE ( 'NONE', *, *, #70293, .T. ) ;
#26066 = PRODUCT_DEFINITION_CONTEXT ( 'detailed design', #13922, 'design' ) ;
#26068 = CARTESIAN_POINT ( 'NONE',  ( 63.31414817410234264, 207.3615022471904012, 5.155647304959626021E-14 ) ) ;
#26069 = CARTESIAN_POINT ( 'NONE',  ( 69.40068436163360843, 70.67970960180943507, 0.7597560883736370618 ) ) ;
#26070 = CARTESIAN_POINT ( 'NONE',  ( 83.97020538542169277, 43.52084701081836471, 6.873119719476476597 ) ) ;
#26071 = CARTESIAN_POINT ( 'NONE',  ( 46.50192534792603283, 74.36443251879779837, 10.00000000000000000 ) ) ;
#26072 = CARTESIAN_POINT ( 'NONE',  ( 207.6129110656513035, 271.0508850574501025, -5.265106572941297358 ) ) ;
#26073 = CARTESIAN_POINT ( 'NONE',  ( 183.4649218511410425, 284.8064977680535890, 15.00784822088543358 ) ) ;
#26074 = CARTESIAN_POINT ( 'NONE',  ( 167.2501155028055564, 251.6211038041439849, 10.31133882848387628 ) ) ;
#26075 = CARTESIAN_POINT ( 'NONE',  ( 50.62146334811270521, 200.0333772461660544, 9.188101187500095079 ) ) ;
#26076 = CARTESIAN_POINT ( 'NONE',  ( 84.80240350195585108, 209.7677522451417929, -5.000000000000041744 ) ) ;
#26077 = ORIENTED_EDGE ( 'NONE', *, *, #48776, .T. ) ;
#26078 = CARTESIAN_POINT ( 'NONE',  ( -13.11024591527723615, 27.99999999999999645, -40.00000000000016342 ) ) ;
#26079 = EDGE_CURVE ( 'NONE', #38189, #62928, #14101, .T. ) ;
#26080 = B_SPLINE_CURVE_WITH_KNOTS ( 'NONE', 3,
 ( #61778, #16688, #39963, #1506, #32388, #63285 ),
 .UNSPECIFIED., .F., .F.,
 ( 4, 2, 4 ),
 ( 0.02097825722499890508, 0.02555397795540580511, 0.03012969868581270513 ),
 .UNSPECIFIED. ) ;
#26081 = CARTESIAN_POINT ( 'NONE',  ( 178.7905889683881355, 259.2243177618232721, -10.28886766292962207 ) ) ;
#26082 = CARTESIAN_POINT ( 'NONE',  ( -1.610867365518755978, 176.0024278399160949, 9.188101187500095079 ) ) ;
#26083 = CARTESIAN_POINT ( 'NONE',  ( 69.07519263286346245, 64.34084314335252941, -11.95120022168340412 ) ) ;
#26084 = CARTESIAN_POINT ( 'NONE',  ( 198.8570476668614049, 286.2164853282868080, -17.01721544293231858 ) ) ;
#26085 = DIRECTION ( 'NONE',  ( -0.8660254037844387076, -0.4999999999999998890, -0.000000000000000000 ) ) ;
#26086 = CARTESIAN_POINT ( 'NONE',  ( 147.0314375879888757, 275.9810751181479986, -5.168577011192616588 ) ) ;
#26087 = CARTESIAN_POINT ( 'NONE',  ( 175.1183745746886871, 267.9007702990796247, 17.47926410801357022 ) ) ;
#26088 = CARTESIAN_POINT ( 'NONE',  ( 204.4781092559247782, 276.4805210635553863, 13.30606382016679490 ) ) ;
#26089 = CARTESIAN_POINT ( 'NONE',  ( 147.1731211915891322, 275.7356719181125868, 0.5879280619134324981 ) ) ;
#26090 = CARTESIAN_POINT ( 'NONE',  ( 164.7694554770609159, 245.2579269087094076, -3.003635650077957742 ) ) ;
#26091 = ORIENTED_EDGE ( 'NONE', *, *, #31023, .F. ) ;
#26092 = VECTOR ( 'NONE', #66740, 1000.000000000000114 ) ;
#26093 = CARTESIAN_POINT ( 'NONE',  ( 208.0045976720423084, 270.3724639545367836, 2.002128742561712471 ) ) ;
#26094 = CARTESIAN_POINT ( 'NONE',  ( -3.297639133650707599, 162.2365022471902023, -10.00000000000009059 ) ) ;
#26095 = CARTESIAN_POINT ( 'NONE',  ( 181.2928807913240234, 267.9761254251728815, 15.08543189990537137 ) ) ;
#26096 = CARTESIAN_POINT ( 'NONE',  ( 127.4269177983626236, 250.5024278399160949, -9.188101187500093303 ) ) ;
#26097 = CARTESIAN_POINT ( 'NONE',  ( 26.56574046957052460, 17.19860640527293327, 2.839279412974134775 ) ) ;
#26098 = CARTESIAN_POINT ( 'NONE',  ( 75.26069627141727381, 66.83174392109067696, 12.89175359686561961 ) ) ;
#26099 = CARTESIAN_POINT ( 'NONE',  ( 34.98558885611105751, 202.5530062829863027, -4.648177544792955347E-16 ) ) ;
#26101 = DIRECTION ( 'NONE',  ( 1.000000000000000000, 1.804112415015878984E-15, 0.000000000000000000 ) ) ;
#26100 = CARTESIAN_POINT ( 'NONE',  ( -19.65312891409030271, 93.06504152958497400, -10.00000000000000888 ) ) ;
#26102 = CARTESIAN_POINT ( 'NONE',  ( 150.2943746394907691, 270.3295023630476521, -14.89639308767058701 ) ) ;
#26103 = EDGE_LOOP ( 'NONE', ( #90447, #96731, #4306, #43665 ) ) ;
#26104 = CARTESIAN_POINT ( 'NONE',  ( 158.2129804214947058, 265.2348010298870236, 17.61986633405762603 ) ) ;
#26105 = CARTESIAN_POINT ( 'NONE',  ( 149.4908848037268001, 271.7211875819559737, -12.92288068979413573 ) ) ;
#26106 = LINE ( 'NONE', #3807, #8626 ) ;
#26107 = CARTESIAN_POINT ( 'NONE',  ( 175.4875483129441136, 292.5133918439943272, -1.145445019159226696 ) ) ;
#26108 = CARTESIAN_POINT ( 'NONE',  ( 81.70827727213743685, 55.24394141669957747, -15.91687133283663869 ) ) ;
#26109 = ORIENTED_EDGE ( 'NONE', *, *, #85468, .T. ) ;
#26110 = CARTESIAN_POINT ( 'NONE',  ( 189.0909386108920103, 265.6590948244866581, 10.80641681947311028 ) ) ;
#26111 = CARTESIAN_POINT ( 'NONE',  ( 184.3226795282388650, 274.5458599865910969, 17.66928848808302988 ) ) ;
#26112 = CARTESIAN_POINT ( 'NONE',  ( 168.1566130751629942, 271.3748772526728885, -16.49521172744375974 ) ) ;
#26113 = CARTESIAN_POINT ( 'NONE',  ( 198.6815419560737155, 272.0295385808636297, 12.20295816876821426 ) ) ;
#26115 = CARTESIAN_POINT ( 'NONE',  ( 155.5855974046909296, 261.5528867068662180, 16.99664480632919705 ) ) ;
#26114 = B_SPLINE_CURVE_WITH_KNOTS ( 'NONE', 3,
 ( #96980, #41215, #27549, #4744 ),
 .UNSPECIFIED., .F., .F.,
 ( 4, 4 ),
 ( 0.01048982011972383714, 0.01573329961111291642 ),
 .UNSPECIFIED. ) ;
#26116 = CARTESIAN_POINT ( 'NONE',  ( 72.38671951208186783, 71.75852817245944948, -5.691748070601700960 ) ) ;
#26117 = CARTESIAN_POINT ( 'NONE',  ( 192.4454213697443095, 297.3217478340386606, 12.58566886711101596 ) ) ;
#26118 = ORIENTED_EDGE ( 'NONE', *, *, #32475, .T. ) ;
#26119 = CARTESIAN_POINT ( 'NONE',  ( 199.5332225370696904, 272.7339375561579686, -13.62198628356192565 ) ) ;
#26120 = CARTESIAN_POINT ( 'NONE',  ( 7.095368192108828076, 22.83478043621386178, -8.090169943749479842 ) ) ;
#26121 = LINE ( 'NONE', #96556, #93457 ) ;
#26122 = VERTEX_POINT ( 'NONE', #63297 ) ;
#26123 = CARTESIAN_POINT ( 'NONE',  ( 167.6260565400901044, 280.9425530968866269, 11.66579211281432116 ) ) ;
#26124 = CARTESIAN_POINT ( 'NONE',  ( 148.4083960970861256, 273.5961130204771052, -8.574185186226726429 ) ) ;
#26125 = CARTESIAN_POINT ( 'NONE',  ( 109.4119587261635758, 240.6427522451419065, -10.00000000000009592 ) ) ;
#26126 = EDGE_LOOP ( 'NONE', ( #97833, #89627, #66610, #53277 ) ) ;
#26127 = FACE_OUTER_BOUND ( 'NONE', #42335, .T. ) ;
#26128 = LINE ( 'NONE', #18536, #13623 ) ;
#26129 = B_SPLINE_CURVE_WITH_KNOTS ( 'NONE', 3,
 ( #43010, #73948, #18754, #80590, #4534, #97270, #20249, #35434, #66337, #11167, #27837, #58714, #51124, #12658, #3561, #33444, #95304, #34441, #65340, #67838, #53615, #35926, #5536, #36420, #67328, #75964, #45515, #13642, #83071, #15109, #44515, #75446, #98758, #14134, #91663, #74466, #76446, #5046, #51641, #6030, #98252, #66828, #28326, #82590, #28841, #37414, #21244, #29830, #68320, #83573, #84571, #59203 ),
 .UNSPECIFIED., .F., .F.,
 ( 4, 2, 2, 2, 2, 2, 2, 2, 2, 2, 2, 2, 2, 2, 2, 2, 2, 2, 2, 2, 2, 2, 2, 2, 2, 4 ),
 ( 0.0006591152314301792136, 0.0008712174001076930475, 0.001083319568785206990, 0.001189370653124002721, 0.001295421737462798453, 0.001401472821801594184, 0.001507523906140389915, 0.001719626074817925867, 0.001931728243495461819, 0.002355932580850601376, 0.003204341255560809801, 0.004052749930271017792, 0.004901158604981225783, 0.005325362942336289013, 0.005537465111013899557, 0.005643516195352659727, 0.005696541737522091420, 0.005749567279691522245, 0.005855618364030549562, 0.005961669448369576879, 0.006173771617047633248, 0.006597975954403787618, 0.006810078123081869141, 0.007022180291759949795, 0.007234282460438032185, 0.007446384629116113707 ),
 .UNSPECIFIED. ) ;
#26130 = CARTESIAN_POINT ( 'NONE',  ( 88.05069107734583156, 43.77613950941169918, -2.175448891271404506 ) ) ;
#26131 = EDGE_CURVE ( 'NONE', #48830, #83821, #17710, .T. ) ;
#26132 = DIRECTION ( 'NONE',  ( -0.6386832404231596039, -0.7694697644498922351, 0.000000000000000000 ) ) ;
#26133 = CARTESIAN_POINT ( 'NONE',  ( 187.0522961678524609, 271.2721401460262882, 16.58916046916640141 ) ) ;
#26134 = CARTESIAN_POINT ( 'NONE',  ( 155.6066474290145720, 261.1283759879266881, -18.16552045242181279 ) ) ;
#26135 = ORIENTED_EDGE ( 'NONE', *, *, #1124, .T. ) ;
#26136 = ORIENTED_EDGE ( 'NONE', *, *, #86793, .T. ) ;
#26137 = CARTESIAN_POINT ( 'NONE',  ( 178.5732266955483567, 260.7996415306764106, 12.02568443977059331 ) ) ;
#26138 = ORIENTED_EDGE ( 'NONE', *, *, #37336, .F. ) ;
#26139 = CARTESIAN_POINT ( 'NONE',  ( 76.99824972205654205, 49.58236607186867673, 15.01116573833570378 ) ) ;
#26141 = EDGE_CURVE ( 'NONE', #54626, #90614, #69982, .T. ) ;
#26140 = ORIENTED_EDGE ( 'NONE', *, *, #55697, .T. ) ;
#26142 = CARTESIAN_POINT ( 'NONE',  ( 88.28592015977814356, 44.16006502160688996, -0.2344584660017056954 ) ) ;
#26143 = CARTESIAN_POINT ( 'NONE',  ( 155.5587153255869453, 261.2113968263770971, -18.30500480654006878 ) ) ;
#26144 = ORIENTED_EDGE ( 'NONE', *, *, #43687, .T. ) ;
#26145 = CARTESIAN_POINT ( 'NONE',  ( 82.58415536943712709, 40.81765542747830722, 3.215309922963823563 ) ) ;
#26146 = CARTESIAN_POINT ( 'NONE',  ( 80.67724759154341996, 43.51231060136900197, -9.541306243518663521 ) ) ;
#26147 = CARTESIAN_POINT ( 'NONE',  ( 158.8643209822442373, 275.1626068170347708, -12.53457103330068101 ) ) ;
#26148 = CARTESIAN_POINT ( 'NONE',  ( 146.7842303614460207, 276.4092505945183689, -4.491116827832889236 ) ) ;
#26150 = EDGE_CURVE ( 'NONE', #46531, #97695, #91464, .T. ) ;
#26149 = CARTESIAN_POINT ( 'NONE',  ( 201.2949053258274148, 281.9939920013367782, -18.04004790210578335 ) ) ;
#26151 = CARTESIAN_POINT ( 'NONE',  ( -71.36129514276956343, 45.88172302328153052, 10.00000000000000000 ) ) ;
#26152 = CARTESIAN_POINT ( 'NONE',  ( 183.3634088509504352, 284.6525016221286251, -16.42631288611494256 ) ) ;
#26153 = CARTESIAN_POINT ( 'NONE',  ( 137.4944631173567018, 256.3149278399160380, -9.188101187500095079 ) ) ;
#26154 = ORIENTED_EDGE ( 'NONE', *, *, #98689, .F. ) ;
#26155 = CARTESIAN_POINT ( 'NONE',  ( 70.62074857767794356, 61.40485173823782361, -14.80809279627126607 ) ) ;
#26156 = ORIENTED_EDGE ( 'NONE', *, *, #8925, .F. ) ;
#26157 = B_SPLINE_CURVE_WITH_KNOTS ( 'NONE', 3,
 ( #66808, #13134, #97737, #20732, #43992, #59702, #60683, #13624, #53106, #91642, #75943, #45982, #51617, #90159, #91147, #28817, #30311, #84062, #37396, #82572, #6519, #76429, #59183, #14617, #98740, #74934, #21712, #53595 ),
 .UNSPECIFIED., .F., .F.,
 ( 4, 2, 2, 2, 2, 2, 2, 2, 2, 2, 2, 2, 2, 4 ),
 ( 0.0004814462238576242893, 0.001666870227462020123, 0.002852294231066416011, 0.003445006232868651035, 0.003741362233769804542, 0.003778406733882429865, 0.003815451233995055189, 0.003852495734107680512, 0.003889540234220305401, 0.004037718234670611105, 0.004334074235571087202, 0.004630430236471567637, 0.004926786237372048072, 0.005223142238272528506 ),
 .UNSPECIFIED. ) ;
#26159 = VERTEX_POINT ( 'NONE', #3032 ) ;
#26158 = CARTESIAN_POINT ( 'NONE',  ( 13.90223112049948639, 33.06302660730329279, 10.00000000000000000 ) ) ;
#26160 = CARTESIAN_POINT ( 'NONE',  ( 46.30674614090290220, 112.4688969640381231, -10.00000000000000000 ) ) ;
#26161 = CARTESIAN_POINT ( 'NONE',  ( 202.6560281492536717, 279.6364581158209717, 17.15553667345918853 ) ) ;
#26162 = CARTESIAN_POINT ( 'NONE',  ( -19.65312891409030271, 93.06504152958497400, 203.6502102582797420 ) ) ;
#26163 = CARTESIAN_POINT ( 'NONE',  ( 192.4464452833618964, 297.3199743636303083, 12.61460102250842574 ) ) ;
#26164 = CARTESIAN_POINT ( 'NONE',  ( 153.3196571941631419, 276.9012595390603906, 7.065720231617055092 ) ) ;
#26165 = CARTESIAN_POINT ( 'NONE',  ( 153.0308080659177392, 265.5898606369461277, -17.74682723936668438 ) ) ;
#26166 = CARTESIAN_POINT ( 'NONE',  ( 83.90596095485256001, 41.21795184261720379, -1.108148245180562033E-06 ) ) ;
#26167 = CARTESIAN_POINT ( 'NONE',  ( 171.5764408558917182, 280.0072332633130259, 13.86250607708617899 ) ) ;
#26168 = VECTOR ( 'NONE', #48668, 1000.000000000000000 ) ;
#26169 = CARTESIAN_POINT ( 'NONE',  ( 48.77433535142598231, 99.76555324011610537, 10.00000000000000000 ) ) ;
#26170 = CARTESIAN_POINT ( 'NONE',  ( -110.0000000000000000, 0.000000000000000000, 9.212605237762156563 ) ) ;
#26171 = ORIENTED_EDGE ( 'NONE', *, *, #28447, .F. ) ;
#26172 = CARTESIAN_POINT ( 'NONE',  ( 32.30839531297598910, 123.0650415295850593, 40.00000000000000711 ) ) ;
#26173 = CARTESIAN_POINT ( 'NONE',  ( 76.19955060832064930, 61.81918726698732769, -15.41303817956920064 ) ) ;
#26174 = ORIENTED_EDGE ( 'NONE', *, *, #65257, .T. ) ;
#26175 = CARTESIAN_POINT ( 'NONE',  ( 164.0359846223783791, 278.2138621274489765, 13.39833324297733164 ) ) ;
#26176 = CARTESIAN_POINT ( 'NONE',  ( 200.9789653343762268, 267.8171911071562477, -2.834779958744446660 ) ) ;
#26177 = CARTESIAN_POINT ( 'NONE',  ( 191.4160719247997804, 299.1046333714251659, -10.38740866002593677 ) ) ;
#26178 = LINE ( 'NONE', #81410, #91565 ) ;
#26179 = CARTESIAN_POINT ( 'NONE',  ( 202.3421728196210552, 280.1800714929709670, 16.85915999540957344 ) ) ;
#26181 = CARTESIAN_POINT ( 'NONE',  ( 151.4541170308968674, 274.9972311722506220, -9.452079333234340908 ) ) ;
#26180 = PLANE ( 'NONE',  #67891 ) ;
#26182 = CARTESIAN_POINT ( 'NONE',  ( 60.04851071045058575, 212.1427522451419065, -10.00000000000009592 ) ) ;
#26183 = VERTEX_POINT ( 'NONE', #64809 ) ;
#26184 = EDGE_CURVE ( 'NONE', #3825, #63991, #85045, .T. ) ;
#26185 = CARTESIAN_POINT ( 'NONE',  ( 76.35339246177476014, 61.05343328037434247, -15.60956989098418290 ) ) ;
#26186 = CARTESIAN_POINT ( 'NONE',  ( 193.4352373529416411, 275.9703139695285472, -16.71496292338552792 ) ) ;
#26187 = ADVANCED_FACE ( 'NONE', ( #41994 ), #78519, .F. ) ;
#26188 = CARTESIAN_POINT ( 'NONE',  ( 57.31414817410225027, 217.7538070926034379, 17.97570218321539315 ) ) ;
#26189 = FACE_OUTER_BOUND ( 'NONE', #84027, .T. ) ;
#26190 = CARTESIAN_POINT ( 'NONE',  ( 80.67704869399170775, 43.49956702784530904, -9.526446727701394224 ) ) ;
#26191 = CARTESIAN_POINT ( 'NONE',  ( 67.08348705826007574, 69.02495177153369355, 2.899183874508027170 ) ) ;
#26192 = CARTESIAN_POINT ( 'NONE',  ( -4.208943576872074210, 174.5024278399160949, 9.188101187500095079 ) ) ;
#26193 = CARTESIAN_POINT ( 'NONE',  ( 95.92524373570365981, 232.3149278399160949, -9.188101187500095079 ) ) ;
#26194 = CARTESIAN_POINT ( 'NONE',  ( 203.0498946958275326, 278.9542612457532869, -15.11479947333269003 ) ) ;
#26195 = CARTESIAN_POINT ( 'NONE',  ( 88.17106782721933200, 44.41923492627702075, -4.565543248975953539 ) ) ;
#26196 = CARTESIAN_POINT ( 'NONE',  ( 147.7445507185682629, 275.1340851767408822, 4.244012899323919896 ) ) ;
#26197 = CARTESIAN_POINT ( 'NONE',  ( 176.2580550267919932, 278.7780497695933946, -16.99066290002705060 ) ) ;
#26198 = EDGE_CURVE ( 'NONE', #77230, #77384, #60688, .T. ) ;
#26199 = CARTESIAN_POINT ( 'NONE',  ( 81.54419519852100962, 59.48562949720209048, 0.3078307376628255376 ) ) ;
#26200 = CARTESIAN_POINT ( 'NONE',  ( 160.5467508819430691, 282.2240450670404357, 5.086209391429217241 ) ) ;
#26203 = CARTESIAN_POINT ( 'NONE',  ( 208.3790849386676598, 269.7238329819538762, -1.525282248498321946 ) ) ;
#26202 = B_SPLINE_CURVE_WITH_KNOTS ( 'NONE', 3,
 ( #15559, #71298, #24182, #55064 ),
 .UNSPECIFIED., .F., .F.,
 ( 4, 4 ),
 ( 0.01367696721474719219, 0.01995365678480425300 ),
 .UNSPECIFIED. ) ;
#26201 = CARTESIAN_POINT ( 'NONE',  ( 190.4356836585210431, 300.3996184492839916, -0.5836641476860114919 ) ) ;
#26204 = EDGE_CURVE ( 'NONE', #43030, #6693, #88662, .T. ) ;
#26205 = CARTESIAN_POINT ( 'NONE',  ( 178.1725702544899264, 289.8985928146129254, 9.568895312856861679 ) ) ;
#26206 = CARTESIAN_POINT ( 'NONE',  ( 50.13870555935886841, 87.67061469898740711, -10.00000000000000000 ) ) ;
#26207 = CARTESIAN_POINT ( 'NONE',  ( 7.313483791488072150, 163.4824982072973683, 3.021315404115420679E-15 ) ) ;
#26208 = CARTESIAN_POINT ( 'NONE',  ( 79.82019804487738668, 54.41907435463492959, -15.91247824403962596 ) ) ;
#26209 = CARTESIAN_POINT ( 'NONE',  ( 76.24020477147122676, 54.98903279212289164, -16.58624229681600326 ) ) ;
#26210 = CARTESIAN_POINT ( 'NONE',  ( 73.37237386183839760, 69.84228272576173424, 9.150815133132212509 ) ) ;
#26211 = CARTESIAN_POINT ( 'NONE',  ( 50.89226983467786170, 194.0643266524160424, 9.188101187500095079 ) ) ;
#26212 = CARTESIAN_POINT ( 'NONE',  ( 86.78549426258130950, 45.83013854792883990, 8.849882187839872572 ) ) ;
#26213 = CARTESIAN_POINT ( 'NONE',  ( 83.25962220535622293, 225.0024278399160664, -9.188101187500093303 ) ) ;
#26214 = CARTESIAN_POINT ( 'NONE',  ( 207.1285138014047504, 271.8898857301724661, -5.752177443817618752 ) ) ;
#26215 = CARTESIAN_POINT ( 'NONE',  ( 72.48667266402317466, 57.40015563624327655, 15.83031223551729560 ) ) ;
#26216 = CARTESIAN_POINT ( 'NONE',  ( 163.3339561395536350, 258.0835846320132418, 15.71813896107145148 ) ) ;
#26218 = CARTESIAN_POINT ( 'NONE',  ( 28.46864935082042081, 149.7156766241961066, 22.50000000000001776 ) ) ;
#26217 = DIRECTION ( 'NONE',  ( 0.000000000000000000, 0.000000000000000000, 1.000000000000000000 ) ) ;
#26219 = CARTESIAN_POINT ( 'NONE',  ( 174.4104451852509214, 268.9371725773738149, -16.32578690765196328 ) ) ;
#26220 = CARTESIAN_POINT ( 'NONE',  ( 29.25887229277395463, 38.93396525600392266, 2.839279412974139660 ) ) ;
#26221 = CARTESIAN_POINT ( 'NONE',  ( -75.14068524134967220, 52.46521621197197760, -10.00000000000000000 ) ) ;
#26222 = CARTESIAN_POINT ( 'NONE',  ( 85.56354969485944650, 46.62399995276157227, -10.02333073147364040 ) ) ;
#26223 = VERTEX_POINT ( 'NONE', #58674 ) ;
#26224 = CARTESIAN_POINT ( 'NONE',  ( 16.65397613197454518, 21.56628583063840310, 9.188101187500006262 ) ) ;
#26225 = CARTESIAN_POINT ( 'NONE',  ( 70.32319418844367931, 223.6589784336661637, -6.496448406907676862E-16 ) ) ;
#26226 = DIRECTION ( 'NONE',  ( -1.000000000000000000, -1.156482317317871133E-15, 0.000000000000000000 ) ) ;
#26227 = FACE_OUTER_BOUND ( 'NONE', #32224, .T. ) ;
#26228 = CARTESIAN_POINT ( 'NONE',  ( 192.6679047218190135, 296.9363953644068488, -13.34486378385621386 ) ) ;
#26229 = CARTESIAN_POINT ( 'NONE',  ( 41.37327796571899796, 124.7191351846657028, 10.00000000000000000 ) ) ;
#26230 = ORIENTED_EDGE ( 'NONE', *, *, #30062, .T. ) ;
#26231 =( BOUNDED_CURVE ( )  B_SPLINE_CURVE ( 2, ( #16150, #24745, #62734, #31345, #30352, #8062, #22757, #9055, #62228 ),
 .UNSPECIFIED., .F., .T. ) 
 B_SPLINE_CURVE_WITH_KNOTS ( ( 3, 2, 2, 2, 3 ),
 ( 0.03629032258064516375, 0.03763440860215053890, 0.04032258064516128920, 0.04301075268817204644, 0.04435483870967742159 ),
 .UNSPECIFIED. ) 
 CURVE ( )  GEOMETRIC_REPRESENTATION_ITEM ( )  RATIONAL_B_SPLINE_CURVE ( ( 0.9330127018922194093, 0.9330127018922195203, 1.000000000000000000, 0.8660254037844387076, 1.000000000000000000, 0.8660254037844387076, 1.000000000000000000, 0.9330127018922194093, 0.9330127018922194093 ) ) 
 REPRESENTATION_ITEM ( '' )  );
#26232 = FACE_OUTER_BOUND ( 'NONE', #81118, .T. ) ;
#26233 = DIRECTION ( 'NONE',  ( 0.000000000000000000, 0.000000000000000000, 1.000000000000000000 ) ) ;
#26234 = CARTESIAN_POINT ( 'NONE',  ( 72.06694649076332837, 71.38420282548176488, 5.126693848571997059 ) ) ;
#26235 = CARTESIAN_POINT ( 'NONE',  ( 87.30348251005597149, 44.98986743115608533, -6.196706157115566604 ) ) ;
#26236 = CARTESIAN_POINT ( 'NONE',  ( 135.6272693901030379, 239.1115022471902023, -5.000000000000041744 ) ) ;
#26237 = CARTESIAN_POINT ( 'NONE',  ( 157.4805323096970255, 257.8827121670497036, -16.70238855805511591 ) ) ;
#26238 = CARTESIAN_POINT ( 'NONE',  ( 75.00053908662732738, 53.26751709772522503, 16.03872633732851227 ) ) ;
#26239 = VERTEX_POINT ( 'NONE', #66299 ) ;
#26240 = CARTESIAN_POINT ( 'NONE',  ( 85.42093500504424242, 46.21730090332891905, 9.681390438263864695 ) ) ;
#26241 = ORIENTED_EDGE ( 'NONE', *, *, #44193, .F. ) ;
#26242 = CARTESIAN_POINT ( 'NONE',  ( 202.5511585997265911, 279.8180975037686835, 17.12781264818056925 ) ) ;
#26243 = CARTESIAN_POINT ( 'NONE',  ( 207.3023081270791295, 270.3638296917698085, -0.1999334432952042662 ) ) ;
#26244 = PLANE ( 'NONE',  #95345 ) ;
#26245 = ORIENTED_EDGE ( 'NONE', *, *, #13041, .T. ) ;
#26246 = CARTESIAN_POINT ( 'NONE',  ( 77.31150235362825640, 63.25814829948299689, -15.20253986937943935 ) ) ;
#26247 = ORIENTED_EDGE ( 'NONE', *, *, #23835, .F. ) ;
#26248 = CARTESIAN_POINT ( 'NONE',  ( 192.8660768639943797, 292.4946550107171674, 15.23525216266379090 ) ) ;
#26249 = CARTESIAN_POINT ( 'NONE',  ( 171.2207522194980811, 249.4850955738359630, 2.852778252398243453 ) ) ;
#26250 = CARTESIAN_POINT ( 'NONE',  ( 84.14312167556933275, 48.98415679381830756, 0.000000000000000000 ) ) ;
#26251 = CARTESIAN_POINT ( 'NONE',  ( 192.9359148231858967, 296.1054784705493717, -12.00501928171166455 ) ) ;
#26252 = ORIENTED_EDGE ( 'NONE', *, *, #19671, .F. ) ;
#26253 = EDGE_CURVE ( 'NONE', #92597, #80984, #21475, .T. ) ;
#26254 = CARTESIAN_POINT ( 'NONE',  ( 36.08541434599421649, 23.76004757982091675, 5.678558825948272215 ) ) ;
#26255 = CARTESIAN_POINT ( 'NONE',  ( 84.21135162255031048, 48.08253741963655159, -12.07440697007694119 ) ) ;
#26256 = ADVANCED_FACE ( 'NONE', ( #42965 ), #19719, .T. ) ;
#26257 = CARTESIAN_POINT ( 'NONE',  ( 166.7959447105422157, 276.3626885415273478, 15.91653206054683523 ) ) ;
#26258 = CARTESIAN_POINT ( 'NONE',  ( -22.42236680055709641, 157.8615022471902591, 0.000000000000000000 ) ) ;
#26259 = ORIENTED_EDGE ( 'NONE', *, *, #74231, .T. ) ;
#26260 = ORIENTED_EDGE ( 'NONE', *, *, #94144, .F. ) ;
#26261 = CARTESIAN_POINT ( 'NONE',  ( 188.4805308512120234, 298.0761574053781828, 7.892637567094712203 ) ) ;
#26263 = CARTESIAN_POINT ( 'NONE',  ( 147.8308140999695866, 274.5965143850199865, -7.866624397492971710 ) ) ;
#26262 = CARTESIAN_POINT ( 'NONE',  ( 163.9149533033796047, 246.7379680887036670, 7.273005089308705706 ) ) ;
#26264 = CARTESIAN_POINT ( 'NONE',  ( 46.80869107419874098, 110.6443039040113092, -10.00000000000000000 ) ) ;
#26265 = CARTESIAN_POINT ( 'NONE',  ( 194.3252252352508265, 294.0658320307167628, 14.07225870721148731 ) ) ;
#26266 = CARTESIAN_POINT ( 'NONE',  ( 147.4869352381265628, 275.6365489870674423, 0.2695896373555386472 ) ) ;
#26267 = DIRECTION ( 'NONE',  ( 0.000000000000000000, 1.000000000000000000, 0.000000000000000000 ) ) ;
#26269 = EDGE_CURVE ( 'NONE', #59430, #3700, #10691, .T. ) ;
#26268 = CARTESIAN_POINT ( 'NONE',  ( 164.6152412757387538, 245.5250337406482117, 4.392968637767231677 ) ) ;
#26270 = CARTESIAN_POINT ( 'NONE',  ( 166.1117962628217697, 265.5293696438469624, 16.57715453726662247 ) ) ;
#26271 = DIRECTION ( 'NONE',  ( 1.000000000000000000, 0.000000000000000000, 0.000000000000000000 ) ) ;
#26272 = CARTESIAN_POINT ( 'NONE',  ( 87.42789010471635436, 209.0327760586659451, 1.948934522072303157E-15 ) ) ;
#26273 = ORIENTED_EDGE ( 'NONE', *, *, #28633, .F. ) ;
#26274 = CARTESIAN_POINT ( 'NONE',  ( -74.97640825042664403, 52.25402898078436920, 10.00000000000000000 ) ) ;
#26275 = ORIENTED_EDGE ( 'NONE', *, *, #24311, .F. ) ;
#26276 = AXIS2_PLACEMENT_3D ( 'NONE', #19186, #41954, #35850 ) ;
#26277 = ORIENTED_EDGE ( 'NONE', *, *, #59885, .T. ) ;
#26278 = ORIENTED_EDGE ( 'NONE', *, *, #54891, .F. ) ;
#26279 = CARTESIAN_POINT ( 'NONE',  ( 80.14239153911771041, 44.91288235749343727, -11.28435394345837928 ) ) ;
#26280 = ADVANCED_FACE ( 'NONE', ( #74912 ), #74424, .T. ) ;
#26282 = B_SPLINE_SURFACE_WITH_KNOTS ( 'NONE', 3, 1, ( 
 ( #72436, #96247 ),
 ( #49111, #50592 ),
 ( #10112, #33407 ),
 ( #44361, #75294 ),
 ( #87684, #10615 ),
 ( #4005, #34891 ),
 ( #79557, #65790 ),
 ( #36761, #3040 ),
 ( #26808, #25827 ),
 ( #64307, #18219 ),
 ( #33931, #57692 ),
 ( #64815, #14475 ),
 ( #39233, #30162 ),
 ( #45356, #38238 ),
 ( #22064, #68656 ),
 ( #31638, #76288 ),
 ( #23041, #52962 ),
 ( #84897, #83406 ),
 ( #29668, #69652 ),
 ( #261, #60545 ),
 ( #21577, #53937 ),
 ( #92986, #37261 ),
 ( #13977, #22565 ),
 ( #75792, #83912 ),
 ( #6860, #91501 ),
 ( #61044, #38748 ),
 ( #68160, #37749 ),
 ( #70141, #99578 ),
 ( #6378, #31142 ),
 ( #45836, #92019 ),
 ( #753, #53451 ),
 ( #99086, #69153 ),
 ( #76759, #84402 ),
 ( #15954, #14946 ) ),
 .UNSPECIFIED., .T., .F., .F.,
 ( 4, 2, 2, 2, 2, 2, 2, 2, 2, 2, 2, 2, 2, 2, 2, 2, 4 ),
 ( 2, 2 ),
 ( 0.000000000000000000, 0.06250000000000000000, 0.1250000000000000000, 0.1875000000000000000, 0.2500000000000000000, 0.3125000000000000000, 0.3750000000000000000, 0.4375000000000000000, 0.5000000000000000000, 0.5625000000000000000, 0.6250000000000000000, 0.6875000000000000000, 0.7500000000000000000, 0.8125000000000000000, 0.8750000000000000000, 0.9375000000000000000, 1.000000000000000000 ),
 ( 0.000000000000000000, 1.000000000000000000 ),
 .UNSPECIFIED. ) ;
#26281 = CARTESIAN_POINT ( 'NONE',  ( 178.4456047009153110, 292.8474234380366852, -2.655382915061203608 ) ) ;
#26283 = CARTESIAN_POINT ( 'NONE',  ( 164.0981304475902789, 249.9383316284954333, 10.21525845096581264 ) ) ;
#26284 = CARTESIAN_POINT ( 'NONE',  ( 159.2289198208967775, 254.8544161663325838, -15.88961297684315888 ) ) ;
#26285 = CARTESIAN_POINT ( 'NONE',  ( 163.2124973040920111, 247.9546575695509887, 10.85238219581215269 ) ) ;
#26286 = EDGE_CURVE ( 'NONE', #26637, #65011, #1372, .T. ) ;
#26287 = CARTESIAN_POINT ( 'NONE',  ( 86.72372382049398709, 227.0024278399160949, 9.188101187500095079 ) ) ;
#26288 = ORIENTED_EDGE ( 'NONE', *, *, #60564, .T. ) ;
#26289 = ORIENTED_EDGE ( 'NONE', *, *, #45134, .T. ) ;
#26290 = CARTESIAN_POINT ( 'NONE',  ( 161.4688978523910805, 250.9746604079464589, -14.18458049884803529 ) ) ;
#26291 = ORIENTED_EDGE ( 'NONE', *, *, #51526, .F. ) ;
#26292 = AXIS2_PLACEMENT_3D ( 'NONE', #16429, #47325, #15927 ) ;
#26293 = CARTESIAN_POINT ( 'NONE',  ( 75.69558293296576323, 65.12864963431647425, -14.43849588152979813 ) ) ;
#26294 = DIRECTION ( 'NONE',  ( 0.4999999999999992784, -0.8660254037844390407, 0.000000000000000000 ) ) ;
#26296 = CARTESIAN_POINT ( 'NONE',  ( 188.6237917963981090, 260.2852467542186901, 5.911286565928174142 ) ) ;
#26295 = CARTESIAN_POINT ( 'NONE',  ( 126.4254891512956220, 252.9869531367911009, 4.594050593750046652 ) ) ;
#26297 = CARTESIAN_POINT ( 'NONE',  ( 73.72680694775513643, 201.8262482093457777, 3.021315404115420679E-15 ) ) ;
#26298 = CARTESIAN_POINT ( 'NONE',  ( 87.95111445425231977, 44.80020534355205797, 4.839585637743885727 ) ) ;
#26299 = ORIENTED_EDGE ( 'NONE', *, *, #84190, .F. ) ;
#26300 = CARTESIAN_POINT ( 'NONE',  ( 88.19053702688614749, 44.32527345396092500, -2.493626234014364673 ) ) ;
#26301 = CARTESIAN_POINT ( 'NONE',  ( 160.5298764916272773, 275.8772147286272229, 14.16040495044419245 ) ) ;
#26302 = EDGE_CURVE ( 'NONE', #45557, #24115, #81054, .T. ) ;
#26303 = CARTESIAN_POINT ( 'NONE',  ( 82.35140075591571929, 40.37528365890498350, -1.256860545790653205 ) ) ;
#26304 = DIRECTION ( 'NONE',  ( -1.000000000000000000, 0.000000000000000000, 0.000000000000000000 ) ) ;
#26305 = CARTESIAN_POINT ( 'NONE',  ( 71.79944583284617465, 59.58521246314043651, -15.72103291199168318 ) ) ;
#26306 = CYLINDRICAL_SURFACE ( 'NONE', #1272, 70.00000000000002842 ) ;
#26307 = DIRECTION ( 'NONE',  ( -0.8660254037844387076, -0.4999999999999998890, -0.000000000000000000 ) ) ;
#26308 = DIRECTION ( 'NONE',  ( 0.000000000000000000, 1.000000000000000000, 0.000000000000000000 ) ) ;
#26309 = ADVANCED_FACE ( 'NONE', ( #83030 ), #44474, .T. ) ;
#26310 = CARTESIAN_POINT ( 'NONE',  ( 161.4844649541891499, 250.9476973967054789, 12.93553496455142415 ) ) ;
#26311 = CARTESIAN_POINT ( 'NONE',  ( 82.98592046873434924, 41.48112914865087220, 2.708872267169455839 ) ) ;
#26312 = CARTESIAN_POINT ( 'NONE',  ( 13.99874362242318604, 31.58029201028041300, 1.583844403245363353 ) ) ;
#26313 = CARTESIAN_POINT ( 'NONE',  ( 78.31032011038168150, 61.54964048803103793, 15.80295067388503050 ) ) ;
#26314 = CARTESIAN_POINT ( 'NONE',  ( 175.5461044416861114, 291.1942812272370702, -6.598926784758673669 ) ) ;
#26315 = CARTESIAN_POINT ( 'NONE',  ( 200.9070263471402029, 275.2638490881122948, 14.76484851748618787 ) ) ;
#26316 = EDGE_CURVE ( 'NONE', #21055, #87863, #60204, .T. ) ;
#26317 = EDGE_CURVE ( 'NONE', #27838, #76006, #12615, .T. ) ;
#26318 = EDGE_CURVE ( 'NONE', #62259, #93301, #98209, .T. ) ;
#26319 = CARTESIAN_POINT ( 'NONE',  ( 207.6860335175200589, 270.9242332556395922, 6.913225035677485586 ) ) ;
#26321 = CARTESIAN_POINT ( 'NONE',  ( 74.20017517015935482, 55.33913510227883847, 16.12309036971300458 ) ) ;
#26320 = CARTESIAN_POINT ( 'NONE',  ( 180.6399068022690813, 266.9789143157389617, -16.10679502715467848 ) ) ;
#26322 = EDGE_CURVE ( 'NONE', #10212, #45167, #19229, .T. ) ;
#26323 = CARTESIAN_POINT ( 'NONE',  ( 79.00824644612984571, 51.04380436647237929, 15.61778681553768244 ) ) ;
#26324 = CARTESIAN_POINT ( 'NONE',  ( 32.37774987120970849, 30.64441083166263269, -10.00000000000000533 ) ) ;
#26325 = CARTESIAN_POINT ( 'NONE',  ( 152.9489295551198893, 265.7316783776963121, 17.71675637597311237 ) ) ;
#26326 = CARTESIAN_POINT ( 'NONE',  ( 180.6524066389949326, 273.0753924814325160, 17.36873516045730170 ) ) ;
#26327 = CARTESIAN_POINT ( 'NONE',  ( 160.6761024546964336, 273.3315593702743058, -15.58338923054105329 ) ) ;
#26328 = CARTESIAN_POINT ( 'NONE',  ( 85.47202168011459378, 43.45241828910128135, -4.867446897391397798 ) ) ;
#26329 = CARTESIAN_POINT ( 'NONE',  ( 13.89683389070260944, 169.6423013555409796, -4.594050593750043987 ) ) ;
#26330 = CARTESIAN_POINT ( 'NONE',  ( 82.54152556014342679, 49.05345396727486218, 13.38640032703253624 ) ) ;
#26331 = EDGE_LOOP ( 'NONE', ( #79882, #43733, #30131, #93736 ) ) ;
#26332 = CARTESIAN_POINT ( 'NONE',  ( 87.34667321826604791, 45.97495992385612595, 8.598559468654661586 ) ) ;
#26333 = CARTESIAN_POINT ( 'NONE',  ( 65.74726825304114186, 69.08659106095529978, 2.128305819671951817E-12 ) ) ;
#26334 = CARTESIAN_POINT ( 'NONE',  ( 82.35975313184987101, 41.41624149272713851, 5.521678208627143647 ) ) ;
#26335 = CARTESIAN_POINT ( 'NONE',  ( 42.15091268916992817, 185.9548013555409796, -4.594050593750042211 ) ) ;
#26336 = AXIS2_PLACEMENT_3D ( 'NONE', #40019, #32445, #48138 ) ;
#26337 = VECTOR ( 'NONE', #93925, 1000.000000000000000 ) ;
#26338 = CARTESIAN_POINT ( 'NONE',  ( 87.06988255670405863, 46.05766899987094831, 8.936389965629217613 ) ) ;
#26339 = CARTESIAN_POINT ( 'NONE',  ( 190.9380839614473473, 299.9325328093580652, -5.232187664503159752 ) ) ;
#26340 = CARTESIAN_POINT ( 'NONE',  ( 32.66923259237032084, 34.56454794089044213, 10.00000000000000355 ) ) ;
#26341 = CARTESIAN_POINT ( 'NONE',  ( 178.8696907613845610, 291.8157686920125684, 6.076668511113703097 ) ) ;
#26342 = CARTESIAN_POINT ( 'NONE',  ( 191.7187529716733820, 298.5803744197520473, -8.487597704798396592 ) ) ;
#26343 = CARTESIAN_POINT ( 'NONE',  ( 197.0834897501566729, 289.2883777501857594, 16.96463043134541238 ) ) ;
#26344 = CARTESIAN_POINT ( 'NONE',  ( 182.5718888600741820, 280.2395840502504143, -16.09643023696035513 ) ) ;
#26345 = CARTESIAN_POINT ( 'NONE',  ( 36.76746430747500227, 51.63176190406338151, 177.5919119679930134 ) ) ;
#26346 = CARTESIAN_POINT ( 'NONE',  ( 166.4967320654721732, 257.8000681324233483, -15.13017568244432098 ) ) ;
#26347 = VECTOR ( 'NONE', #63981, 1000.000000000000000 ) ;
#26348 = CARTESIAN_POINT ( 'NONE',  ( 83.09635312912047311, 230.3297689869269220, -2.679491924311252493 ) ) ;
#26349 = CARTESIAN_POINT ( 'NONE',  ( 76.30452923086889427, 224.8615022471903160, 5.000000000000046185 ) ) ;
#26350 = DIRECTION ( 'NONE',  ( 0.000000000000000000, 0.000000000000000000, 1.000000000000000000 ) ) ;
#26351 = DIRECTION ( 'NONE',  ( -1.000000000000000000, 4.892646582057217816E-14, 0.000000000000000000 ) ) ;
#26352 = CARTESIAN_POINT ( 'NONE',  ( 44.74898890052324418, 187.4548013555409796, -4.594050593750042211 ) ) ;
#26353 = CARTESIAN_POINT ( 'NONE',  ( 67.37944191706843355, 66.71681795993420394, -8.450929298107464405 ) ) ;
#26354 = ORIENTED_EDGE ( 'NONE', *, *, #78516, .F. ) ;
#26355 = DIRECTION ( 'NONE',  ( -0.9956898167541090583, 0.09274582908232931189, 0.000000000000000000 ) ) ;
#26356 = CARTESIAN_POINT ( 'NONE',  ( 198.5970767652345899, 286.6667681383942181, -17.17073100918929640 ) ) ;
#26357 = CARTESIAN_POINT ( 'NONE',  ( 58.13834967963523326, 192.8262482093458061, 3.021315404115420679E-15 ) ) ;
#26358 = ORIENTED_EDGE ( 'NONE', *, *, #36258, .T. ) ;
#26360 = CARTESIAN_POINT ( 'NONE',  ( 37.67364948790085322, 52.89489741671174272, 10.00000000000000000 ) ) ;
#26359 = VECTOR ( 'NONE', #56120, 999.9999999999998863 ) ;
#26361 = CARTESIAN_POINT ( 'NONE',  ( 164.3138894970802824, 246.0469903322357368, -2.642126690130961020 ) ) ;
#26362 = CARTESIAN_POINT ( 'NONE',  ( 147.1824143116938046, 275.7195757619304572, 6.276289813856542388 ) ) ;
#26363 = CARTESIAN_POINT ( 'NONE',  ( 80.96546451793241772, 46.78193962505741865, -13.01366642040773947 ) ) ;
#26364 = CARTESIAN_POINT ( 'NONE',  ( 33.16918417342686354, 21.01110640527294038, 2.839279412974134775 ) ) ;
#26365 = LINE ( 'NONE', #57240, #23914 ) ;
#26366 = CARTESIAN_POINT ( 'NONE',  ( 196.2379679265050925, 290.7528645076583871, -16.93678934971137906 ) ) ;
#26367 = CARTESIAN_POINT ( 'NONE',  ( 172.2121928603940262, 256.1155326756577892, 11.22455358908347378 ) ) ;
#26368 = ORIENTED_EDGE ( 'NONE', *, *, #65306, .T. ) ;
#26369 = CARTESIAN_POINT ( 'NONE',  ( 12.32504541118064978, 22.51421378149917985, -9.188101187500004485 ) ) ;
#26370 = CARTESIAN_POINT ( 'NONE',  ( 17.34263298987836066, 187.4865022471903444, -10.00000000000009592 ) ) ;
#26371 = LINE ( 'NONE', #20773, #42372 ) ;
#26372 = ORIENTED_EDGE ( 'NONE', *, *, #31070, .T. ) ;
#26373 = CARTESIAN_POINT ( 'NONE',  ( 72.23468229527969697, 71.59820328793978206, -5.860928441596811922 ) ) ;
#26374 = CARTESIAN_POINT ( 'NONE',  ( 166.9004453850575374, 261.3797933789293779, 16.71428553088463431 ) ) ;
#26375 = CARTESIAN_POINT ( 'NONE',  ( 177.7795532957129581, 255.1900280424794687, -6.882059445467048953 ) ) ;
#26376 = CARTESIAN_POINT ( 'NONE',  ( 201.1403430031335517, 280.2617017971787732, 16.85780947333721613 ) ) ;
#26377 = ORIENTED_EDGE ( 'NONE', *, *, #97112, .F. ) ;
#26378 = ORIENTED_EDGE ( 'NONE', *, *, #12991, .F. ) ;
#26380 = CARTESIAN_POINT ( 'NONE',  ( 46.30674614090290220, 112.4688969640381231, 10.00000000000000000 ) ) ;
#26379 = CARTESIAN_POINT ( 'NONE',  ( 207.8984236726843164, 270.5563627158673512, -6.084369154771423815 ) ) ;
#26381 = CARTESIAN_POINT ( 'NONE',  ( 196.4170778717353585, 290.4426369823788718, -17.78762421190030452 ) ) ;
#26382 = ORIENTED_EDGE ( 'NONE', *, *, #21160, .T. ) ;
#26383 = CARTESIAN_POINT ( 'NONE',  ( 201.0468719883840265, 282.4235983437597497, -16.59631526626950659 ) ) ;
#26384 = CARTESIAN_POINT ( 'NONE',  ( 198.3449891235413531, 287.1033967417670283, 16.95540786497457120 ) ) ;
#26385 = CARTESIAN_POINT ( 'NONE',  ( 72.98169074979469428, 57.62652471086132522, -16.32181584066402991 ) ) ;
#26386 = CARTESIAN_POINT ( 'NONE',  ( 78.39164420400439326, 61.24742163703882625, -15.88566992787024823 ) ) ;
#26387 = CARTESIAN_POINT ( 'NONE',  ( 157.8820657059571033, 257.1872359237914338, -17.60412210594719440 ) ) ;
#26389 = ADVANCED_FACE ( 'NONE', ( #3998 ), #34884, .F. ) ;
#26388 = CARTESIAN_POINT ( 'NONE',  ( 124.1257165900819359, 230.2202760586659736, -5.415160957724236172E-17 ) ) ;
#26390 = CARTESIAN_POINT ( 'NONE',  ( -78.71521058394759507, 57.86724000996476747, -10.00000000000000000 ) ) ;
#26391 = CARTESIAN_POINT ( 'NONE',  ( 187.4166251561426293, 263.4339899954952102, 11.64397722261905166 ) ) ;
#26392 = ORIENTED_EDGE ( 'NONE', *, *, #7187, .F. ) ;
#26393 = CARTESIAN_POINT ( 'NONE',  ( 207.6471633721571379, 270.9915583223058206, 2.196965492132801678 ) ) ;
#26394 = ORIENTED_EDGE ( 'NONE', *, *, #879, .F. ) ;
#26395 = B_SPLINE_CURVE_WITH_KNOTS ( 'NONE', 3,
 ( #16328, #54304, #39103, #15819, #47222, #78144, #16823, #8730, #39602, #24432, #92371, #53806, #1138, #47710, #9231, #24924, #32537, #94369, #63431, #55798, #1652, #86035, #9477, #78384, #85520, #63665, #94108, #78891, #24168, #1877, #55544, #39341, #40841, #77377, #71285, #92605, #8470, #30775, #38855, #40348, #70765, #32759 ),
 .UNSPECIFIED., .F., .F.,
 ( 4, 2, 2, 2, 2, 2, 2, 2, 2, 2, 2, 2, 2, 2, 2, 2, 2, 2, 2, 2, 4 ),
 ( 0.002222259514562908208, 0.002656659727101862243, 0.002873859833371299362, 0.003091059939640736914, 0.003199659992775469568, 0.003308260045910201789, 0.003525460152179574723, 0.003959860364718250335, 0.004828660789795527833, 0.005697461214872804464, 0.006566261639950082829, 0.007000661852488722012, 0.007435062065027361194, 0.007543662118161998872, 0.007597962144729316844, 0.007652262171296634816, 0.007760862224431298514, 0.007869462277565960479, 0.008303862490104212818, 0.008738262702642463423, 0.009172662915180715762 ),
 .UNSPECIFIED. ) ;
#26396 = CARTESIAN_POINT ( 'NONE',  ( 32.59967566254915994, 39.79752408145595410, -5.678558825948271327 ) ) ;
#26397 = CARTESIAN_POINT ( 'NONE',  ( 198.4772197948566372, 286.8743665007300478, 18.43646439804394532 ) ) ;
#26398 = CARTESIAN_POINT ( 'NONE',  ( 78.15916255518206412, 47.79662076820892480, -13.98612838149463755 ) ) ;
#26399 = CARTESIAN_POINT ( 'NONE',  ( 66.99449581658849695, 218.6744531367911293, 4.594050593750047540 ) ) ;
#26400 = ADVANCED_FACE ( 'NONE', ( #13113 ), #36379, .F. ) ;
#26401 = CARTESIAN_POINT ( 'NONE',  ( 73.79815732168846409, 68.46225211080071915, 11.43730676814645442 ) ) ;
#26402 = CARTESIAN_POINT ( 'NONE',  ( 190.8604783348975502, 300.0669496974951471, 7.597731640149610222 ) ) ;
#26403 = LINE ( 'NONE', #58281, #12741 ) ;
#26404 = CARTESIAN_POINT ( 'NONE',  ( 175.9016958582107293, 272.8421865953737324, 16.70581961971107887 ) ) ;
#26405 = EDGE_CURVE ( 'NONE', #53525, #82029, #1961, .T. ) ;
#26406 = ORIENTED_EDGE ( 'NONE', *, *, #18434, .F. ) ;
#26407 = CARTESIAN_POINT ( 'NONE',  ( 75.51395409436767636, 58.27241819066912853, -15.98951179309681159 ) ) ;
#26408 = CARTESIAN_POINT ( 'NONE',  ( 13.90223112049948639, 33.06302660730329279, 10.00000000000000000 ) ) ;
#26409 = ORIENTED_EDGE ( 'NONE', *, *, #11528, .F. ) ;
#26410 = CARTESIAN_POINT ( 'NONE',  ( 153.1965564441067045, 269.1488324487709178, -15.62636021046843382 ) ) ;
#26411 = CARTESIAN_POINT ( 'NONE',  ( 173.8411061959160691, 278.0589164288677466, -16.53377806444067488 ) ) ;
#26412 = CARTESIAN_POINT ( 'NONE',  ( 160.4278600671212303, 258.1933913629677591, -16.98986990419299659 ) ) ;
#26413 = CARTESIAN_POINT ( 'NONE',  ( 70.22199747613832699, 222.8967562850346837, -4.648177544792955347E-16 ) ) ;
#26414 = CARTESIAN_POINT ( 'NONE',  ( 190.6661865267473104, 300.4034729807058852, 4.523489664447863490 ) ) ;
#26415 = VECTOR ( 'NONE', #56571, 1000.000000000000114 ) ;
#26416 = CARTESIAN_POINT ( 'NONE',  ( 180.1766175091199216, 271.0712247103771801, 16.39758672572147091 ) ) ;
#26417 = CARTESIAN_POINT ( 'NONE',  ( 83.00815485991435594, 53.30142267139499523, 15.60062745561815767 ) ) ;
#26418 = LINE ( 'NONE', #18818, #12104 ) ;
#26419 = CARTESIAN_POINT ( 'NONE',  ( 164.2981700896163773, 253.9203781951923133, 14.63367134977796802 ) ) ;
#26420 = EDGE_LOOP ( 'NONE', ( #64676, #8686, #18138, #18562 ) ) ;
#26421 = CARTESIAN_POINT ( 'NONE',  ( 164.0179800784044915, 246.5595204798204065, -5.772998092557310557 ) ) ;
#26422 = CARTESIAN_POINT ( 'NONE',  ( 125.1810982770029881, 233.8923013555409796, 4.594050593750050204 ) ) ;
#26423 = ORIENTED_EDGE ( 'NONE', *, *, #91424, .F. ) ;
#26424 = CARTESIAN_POINT ( 'NONE',  ( 191.1687199697037443, 299.5330595250031820, -8.491751560014430211 ) ) ;
#26425 = CARTESIAN_POINT ( 'NONE',  ( 83.94709567845697507, 42.07943496863257593, 2.936195033694379841 ) ) ;
#26426 = AXIS2_PLACEMENT_3D ( 'NONE', #82085, #89208, #5045 ) ;
#26427 = DIRECTION ( 'NONE',  ( -0.1378186779084930869, 0.2387089523694814197, -0.9612616959383223358 ) ) ;
#26428 = DIRECTION ( 'NONE',  ( -0.3668518372888710521, -0.9302793824855948301, 0.000000000000000000 ) ) ;
#26429 = CARTESIAN_POINT ( 'NONE',  ( -14.83262083840143575, 124.7156766241961208, -21.50000000000003197 ) ) ;
#26430 = CARTESIAN_POINT ( 'NONE',  ( 176.7263968240380621, 254.5787242937214785, 4.904709157180852763 ) ) ;
#26431 = EDGE_LOOP ( 'NONE', ( #8578, #17421, #84231, #59870 ) ) ;
#26432 = CARTESIAN_POINT ( 'NONE',  ( 80.63145207929048297, 57.26919043701818879, -16.23179315233208087 ) ) ;
#26433 = EDGE_CURVE ( 'NONE', #30181, #90587, #23171, .T. ) ;
#26434 = CIRCLE ( 'NONE', #7024, 9.212605237762131694 ) ;
#26435 = CARTESIAN_POINT ( 'NONE',  ( 157.9903129722402753, 275.9952189379433776, -12.65964543032067091 ) ) ;
#26436 = CARTESIAN_POINT ( 'NONE',  ( 182.0600995000775413, 260.3591856445613644, 10.51176232977279312 ) ) ;
#26437 = CARTESIAN_POINT ( 'NONE',  ( 165.0477436618537865, 244.7759176335020186, -2.027991469056170448 ) ) ;
#26438 = CARTESIAN_POINT ( 'NONE',  ( 141.2293712190596011, 252.3458772461660260, 9.188101187500095079 ) ) ;
#26439 = DIRECTION ( 'NONE',  ( 0.8660254037844378194, 0.5000000000000013323, 0.000000000000000000 ) ) ;
#26440 = AXIS2_PLACEMENT_3D ( 'NONE', #88468, #81346, #26609 ) ;
#26441 = CARTESIAN_POINT ( 'NONE',  ( 41.47569090598247499, 209.1868197944957899, 17.47570218321535762 ) ) ;
#26442 = ADVANCED_FACE ( 'NONE', ( #882 ), #84035, .T. ) ;
#26443 = DIRECTION ( 'NONE',  ( -0.5632146860273895550, 0.8263106059122495850, 0.000000000000000000 ) ) ;
#26444 = CARTESIAN_POINT ( 'NONE',  ( 74.43750904794977430, 201.5327760586659167, 1.948934522072303157E-15 ) ) ;
#26445 = CARTESIAN_POINT ( 'NONE',  ( 205.3465787480556344, 274.9762877783610406, -13.79319041940166279 ) ) ;
#26446 = CARTESIAN_POINT ( 'NONE',  ( 174.6847557482075217, 251.9401552947160781, 3.562689555296894017 ) ) ;
#26447 = ADVANCED_FACE ( 'NONE', ( #69279 ), #93108, .F. ) ;
#26448 = CARTESIAN_POINT ( 'NONE',  ( 11.96499418379068480, 31.00034080476288878, -1.878358725466461243E-16 ) ) ;
#26449 = CARTESIAN_POINT ( 'NONE',  ( 149.7128599965862463, 271.3367152699035501, 12.33532264622322394 ) ) ;
#26450 = CARTESIAN_POINT ( 'NONE',  ( 155.3976843646185273, 279.6809108413763738, -1.548285546709123883 ) ) ;
#26451 = CARTESIAN_POINT ( 'NONE',  ( 172.0998544454759838, 287.8757577825812177, -8.507407346436933082 ) ) ;
#26452 = DIRECTION ( 'NONE',  ( -0.8660254037844387076, -0.4999999999999998890, -0.000000000000000000 ) ) ;
#26453 = CARTESIAN_POINT ( 'NONE',  ( 193.6168471018168589, 288.5492936057587485, 16.06529688929707689 ) ) ;
#26454 = CARTESIAN_POINT ( 'NONE',  ( 121.1754704609022752, 230.7677522451417929, -5.000000000000041744 ) ) ;
#26455 = CARTESIAN_POINT ( 'NONE',  ( 78.36746962641299774, 52.62081666013096992, -15.66493875128054469 ) ) ;
#26456 = VERTEX_POINT ( 'NONE', #92621 ) ;
#26457 = CARTESIAN_POINT ( 'NONE',  ( 157.8740713127050981, 257.2010826190796706, 17.31862062017425075 ) ) ;
#26458 = CARTESIAN_POINT ( 'NONE',  ( 160.2313082275607599, 258.0676731373150687, -17.23155629354643281 ) ) ;
#26459 = CARTESIAN_POINT ( 'NONE',  ( -10.21716836350912949, 177.1589784336661637, -6.496448406907676862E-16 ) ) ;
#26460 = CARTESIAN_POINT ( 'NONE',  ( 29.07873433320978052, 199.8464784336661353, 1.353441290958777327E-15 ) ) ;
#26461 = CARTESIAN_POINT ( 'NONE',  ( 175.5402865323166282, 256.4720531653651960, -10.93513971934378759 ) ) ;
#26462 = CARTESIAN_POINT ( 'NONE',  ( 14.83370333027871801, 32.65659080271450421, -1.878358725466461243E-16 ) ) ;
#26463 = CARTESIAN_POINT ( 'NONE',  ( -22.42236680055709641, 157.8615022471902591, 0.000000000000000000 ) ) ;
#26464 = CARTESIAN_POINT ( 'NONE',  ( 204.7237927799493775, 276.0549847173622879, -12.81020997223575364 ) ) ;
#26465 = CARTESIAN_POINT ( 'NONE',  ( 190.6163636546212103, 291.2123861011319832, -14.36794556205205176 ) ) ;
#26466 = CARTESIAN_POINT ( 'NONE',  ( 190.8545714895799392, 300.0771806536980648, -5.516553996882049837 ) ) ;
#26467 = CARTESIAN_POINT ( 'NONE',  ( 73.94850163436859702, 55.42609493996558001, -16.11567799753128227 ) ) ;
#26469 = CARTESIAN_POINT ( 'NONE',  ( 66.18285732059042914, 199.0177522451417929, 5.000000000000051514 ) ) ;
#26468 = CARTESIAN_POINT ( 'NONE',  ( 167.5861325596884797, 256.5095974891418109, 15.03189046419509367 ) ) ;
#26470 = CARTESIAN_POINT ( 'NONE',  ( 74.93659349595930053, 67.20166626244473207, 12.52374196637391357 ) ) ;
#26471 = CARTESIAN_POINT ( 'NONE',  ( 204.8385597977314490, 275.8562024115307167, -12.64672659107585240 ) ) ;
#26472 = CARTESIAN_POINT ( 'NONE',  ( 162.1309243477163875, 252.0648751526918261, -13.42546355478092401 ) ) ;
#26473 = EDGE_CURVE ( 'NONE', #32988, #36501, #85018, .T. ) ;
#26474 = CARTESIAN_POINT ( 'NONE',  ( 42.52953848327577191, 205.3615022471903160, 5.000000000000046185 ) ) ;
#26475 = CARTESIAN_POINT ( 'NONE',  ( 181.4638851230621981, 292.1855915779808583, 8.982959869412693976 ) ) ;
#26476 = CARTESIAN_POINT ( 'NONE',  ( 202.8499463704053198, 279.3005819042728604, 17.04674939340617001 ) ) ;
#26477 = CARTESIAN_POINT ( 'NONE',  ( 6.480970727150832111, 183.7369531367911009, -4.594050593750048428 ) ) ;
#26478 = CARTESIAN_POINT ( 'NONE',  ( 35.85928575902275384, 36.10171378149922106, 9.188101187500008038 ) ) ;
#26480 = EDGE_CURVE ( 'NONE', #7391, #19447, #21280, .T. ) ;
#26479 = CARTESIAN_POINT ( 'NONE',  ( 164.0679150660969015, 247.0361648238571490, 5.995095722802411764 ) ) ;
#26481 = DIRECTION ( 'NONE',  ( 0.5000000000000013323, -0.8660254037844378194, 0.000000000000000000 ) ) ;
#26482 = CARTESIAN_POINT ( 'NONE',  ( 35.55378427144160014, 29.03085787977765264, 9.188101187500006262 ) ) ;
#26483 = CARTESIAN_POINT ( 'NONE',  ( 16.86745276891122103, 33.23654200823202842, 1.583844403245363353 ) ) ;
#26484 = CARTESIAN_POINT ( 'NONE',  ( 179.6767793656050856, 277.0380904139387326, 16.30208254225003373 ) ) ;
#26485 = CARTESIAN_POINT ( 'NONE',  ( 81.12452645434240139, 43.43369904203282772, -9.948711836735455449 ) ) ;
#26486 = CARTESIAN_POINT ( 'NONE',  ( 48.32408078245681793, 82.80331927372955647, -10.00000000000000000 ) ) ;
#26487 = DIRECTION ( 'NONE',  ( -0.000000000000000000, 0.000000000000000000, -1.000000000000000000 ) ) ;
#26488 = CARTESIAN_POINT ( 'NONE',  ( 14.00658445089738180, 13.80170272979924917, 7.433330006724137462 ) ) ;
#26489 = CARTESIAN_POINT ( 'NONE',  ( 153.7085206060443454, 277.9268386586845736, -5.206943850374270433 ) ) ;
#26490 = CARTESIAN_POINT ( 'NONE',  ( 16.11390655273756778, 24.70171378149918340, -9.188101187500004485 ) ) ;
#26491 = CARTESIAN_POINT ( 'NONE',  ( -78.71521058394759507, 57.86724000996476747, -10.00000000000000000 ) ) ;
#26492 = CARTESIAN_POINT ( 'NONE',  ( 154.9226727788713731, 262.3130548330639726, 18.22497199616848818 ) ) ;
#26493 = LINE ( 'NONE', #57370, #3315 ) ;
#26494 = CARTESIAN_POINT ( 'NONE',  ( 88.24741913774678892, 44.24286465476006924, -1.859444097506131488 ) ) ;
#26495 = EDGE_LOOP ( 'NONE', ( #98774, #99302, #12043, #23255 ) ) ;
#26496 = CARTESIAN_POINT ( 'NONE',  ( 153.4477557824949940, 264.8676860077344486, 17.16010094972647693 ) ) ;
#26497 = CARTESIAN_POINT ( 'NONE',  ( 164.8670003495851404, 245.0889742334797177, -1.557028074864921674 ) ) ;
#26498 = CARTESIAN_POINT ( 'NONE',  ( 191.5687499534637652, 298.4314963742343139, 8.517990275034220460 ) ) ;
#26499 = CARTESIAN_POINT ( 'NONE',  ( 203.3041373168503299, 278.5139001086923827, -16.61929732091214973 ) ) ;
#26500 = AXIS2_PLACEMENT_3D ( 'NONE', #69061, #7770, #47749 ) ;
#26501 = VERTEX_POINT ( 'NONE', #21693 ) ;
#26502 = VERTEX_POINT ( 'NONE', #68279 ) ;
#26504 = CARTESIAN_POINT ( 'NONE',  ( -19.65312891409030271, 93.06504152958497400, 10.00000000000000888 ) ) ;
#26503 = FACE_OUTER_BOUND ( 'NONE', #12173, .T. ) ;
#26505 = CIRCLE ( 'NONE', #20078, 70.00000000000001421 ) ;
#26506 = CARTESIAN_POINT ( 'NONE',  ( 86.47552948348150892, 47.43782623826668043, 10.38323646570730752 ) ) ;
#26507 = ORIENTED_EDGE ( 'NONE', *, *, #98728, .T. ) ;
#26508 = CARTESIAN_POINT ( 'NONE',  ( 77.33305236775244396, 55.26159023894539501, 16.12204705925791970 ) ) ;
#26509 = CARTESIAN_POINT ( 'NONE',  ( 175.4059438627250529, 262.7554929797840941, 14.36458932732593397 ) ) ;
#26510 = ORIENTED_EDGE ( 'NONE', *, *, #55574, .T. ) ;
#26511 = LINE ( 'NONE', #71622, #71787 ) ;
#26512 = CARTESIAN_POINT ( 'NONE',  ( 82.32629372474684715, 49.22594776363517610, -13.55554168643329049 ) ) ;
#26513 = AXIS2_PLACEMENT_3D ( 'NONE', #28062, #41388, #79450 ) ;
#26514 = B_SPLINE_CURVE_WITH_KNOTS ( 'NONE', 3,
 ( #43340, #76737, #23020, #38724, #69629, #84873, #15415, #61530, #15928, #7331 ),
 .UNSPECIFIED., .F., .F.,
 ( 4, 2, 2, 2, 4 ),
 ( 0.000000000000000000, 0.0002622400424273768345, 0.0005244800848547536689, 0.0007867201272821304492, 0.001048960169709507338 ),
 .UNSPECIFIED. ) ;
#26515 = CARTESIAN_POINT ( 'NONE',  ( 80.79660903030796248, 43.04784081911883220, 9.716927669273982104 ) ) ;
#26516 = EDGE_LOOP ( 'NONE', ( #34947, #28169, #23287, #31908 ) ) ;
#26517 = CARTESIAN_POINT ( 'NONE',  ( 173.8773719162893769, 267.3830834928915010, 16.61494387878642698 ) ) ;
#26518 = CARTESIAN_POINT ( 'NONE',  ( 166.2593844326262911, 273.7376754232747658, -16.16122191897295224 ) ) ;
#26519 = CARTESIAN_POINT ( 'NONE',  ( -19.65312891409030271, 93.06504152958497400, 177.5919119679930134 ) ) ;
#26520 = PRODUCT ( 'Circular Angle Protractor Plate', 'Circular Angle Protractor Plate', '', ( #84692 ) ) ;
#26521 = VERTEX_POINT ( 'NONE', #46463 ) ;
#26522 = DIRECTION ( 'NONE',  ( 0.4813790724697852297, 0.8765125147926464688, 0.000000000000000000 ) ) ;
#26523 = CARTESIAN_POINT ( 'NONE',  ( 203.0507839702407580, 278.9527209772879814, 16.21318481136342626 ) ) ;
#26524 = ORIENTED_EDGE ( 'NONE', *, *, #81797, .T. ) ;
#26525 = EDGE_CURVE ( 'NONE', #8895, #48406, #70583, .T. ) ;
#26526 = CARTESIAN_POINT ( 'NONE',  ( 156.8716556710364500, 266.6757045202047038, -16.21603570256788629 ) ) ;
#26527 = VERTEX_POINT ( 'NONE', #16079 ) ;
#26528 = EDGE_CURVE ( 'NONE', #89390, #36862, #52575, .T. ) ;
#26529 = CARTESIAN_POINT ( 'NONE',  ( 80.09120749856197108, 44.41673742825524585, -10.86461196121644157 ) ) ;
#26530 = VERTEX_POINT ( 'NONE', #6497 ) ;
#26531 =( BOUNDED_CURVE ( )  B_SPLINE_CURVE ( 2, ( #57223, #20747, #51634, #28319, #12142, #88696, #97752, #4032, #58709 ),
 .UNSPECIFIED., .F., .T. ) 
 B_SPLINE_CURVE_WITH_KNOTS ( ( 3, 2, 2, 2, 3 ),
 ( 0.7782258064516128782, 0.7795698924731182533, 0.7822580645161290036, 0.7849462365591397539, 0.7862903225806451291 ),
 .UNSPECIFIED. ) 
 CURVE ( )  GEOMETRIC_REPRESENTATION_ITEM ( )  RATIONAL_B_SPLINE_CURVE ( ( 0.9330127018922194093, 0.9330127018922194093, 1.000000000000000000, 0.8660254037844387076, 1.000000000000000000, 0.8660254037844387076, 1.000000000000000000, 0.9330127018922194093, 0.9330127018922194093 ) ) 
 REPRESENTATION_ITEM ( '' )  );
#26532 = CARTESIAN_POINT ( 'NONE',  ( 147.1938706002993626, 275.6997328879997440, 7.009419768930110095 ) ) ;
#26533 = CARTESIAN_POINT ( 'NONE',  ( 15.67199189347853761, 32.63213790969698636, 10.00000000000000000 ) ) ;
#26534 = CARTESIAN_POINT ( 'NONE',  ( 72.56680254073344827, 71.38637538794351656, 5.777867564336608197 ) ) ;
#26535 = CARTESIAN_POINT ( 'NONE',  ( 81.89485588203808675, 55.22971306509118250, 16.24120679747552032 ) ) ;
#26536 = CARTESIAN_POINT ( 'NONE',  ( 178.0801157186545254, 291.3379508872625365, 6.079316923194516775 ) ) ;
#26537 = CARTESIAN_POINT ( 'NONE',  ( 146.6363376198206652, 276.6654083370839885, -0.5879280619134327202 ) ) ;
#26538 = ORIENTED_EDGE ( 'NONE', *, *, #12664, .F. ) ;
#26539 = DIRECTION ( 'NONE',  ( -1.850371707708595795E-16, -7.401486830834383181E-16, 1.000000000000000000 ) ) ;
#26540 = CARTESIAN_POINT ( 'NONE',  ( 28.52090319329063206, 17.26216523072495690, -2.296566073217252530E-15 ) ) ;
#26541 = CARTESIAN_POINT ( 'NONE',  ( 164.3493441216711517, 245.9855811210807417, 1.722120810491653664 ) ) ;
#26543 = CARTESIAN_POINT ( 'NONE',  ( 69.35253854976201637, 63.01665765323906498, 13.58811665770852350 ) ) ;
#26542 = CARTESIAN_POINT ( 'NONE',  ( 77.55384616172401024, 49.72970008889385696, -15.46212513759681428 ) ) ;
#26545 = VERTEX_POINT ( 'NONE', #53572 ) ;
#26544 = DIRECTION ( 'NONE',  ( -0.2805612043866616001, -0.9598361373656993933, 0.000000000000000000 ) ) ;
#26546 = ORIENTED_EDGE ( 'NONE', *, *, #70885, .T. ) ;
#26547 = CARTESIAN_POINT ( 'NONE',  ( 187.6674080789407242, 277.1453262015298264, 17.21093267091079682 ) ) ;
#26548 = CARTESIAN_POINT ( 'NONE',  ( 171.6829532011573747, 259.3958823610213358, -15.24497651433520318 ) ) ;
#26549 = CARTESIAN_POINT ( 'NONE',  ( 163.5366322716688785, 247.7755347313017467, 7.814338521876752708 ) ) ;
#26550 = CARTESIAN_POINT ( 'NONE',  ( 118.0080022156327431, 250.4860189848785126, -2.679491924311252493 ) ) ;
#26551 = CARTESIAN_POINT ( 'NONE',  ( 159.9160972866109205, 253.6641898818994889, -15.06183666839949709 ) ) ;
#26552 = CARTESIAN_POINT ( 'NONE',  ( 148.6217150854157580, 273.2266336944707632, -9.117259336374514689 ) ) ;
#26553 = ORIENTED_EDGE ( 'NONE', *, *, #77001, .T. ) ;
#26554 = CARTESIAN_POINT ( 'NONE',  ( 58.00798602660123748, 188.7095308348469018, 4.041334437186252691E-16 ) ) ;
#26555 = EDGE_CURVE ( 'NONE', #37792, #16392, #18764, .T. ) ;
#26556 = CARTESIAN_POINT ( 'NONE',  ( 42.66379208638658582, 206.9860189848785410, -2.679491924311252493 ) ) ;
#26557 = CARTESIAN_POINT ( 'NONE',  ( 164.4781197247689306, 245.7625352337404649, -1.511762618280499515 ) ) ;
#26558 = CARTESIAN_POINT ( 'NONE',  ( 32.40786657299730678, 179.5177522451417929, 5.000000000000051514 ) ) ;
#26559 = CARTESIAN_POINT ( 'NONE',  ( 101.1213961584103060, 235.3149278399160664, -9.188101187500095079 ) ) ;
#26560 = CARTESIAN_POINT ( 'NONE',  ( 183.8023311956230827, 297.0733055398724787, -2.815221220798488577 ) ) ;
#26561 = CARTESIAN_POINT ( 'NONE',  ( 100.8442274002074441, 217.4824982072973683, 3.021315404115420679E-15 ) ) ;
#26562 = CARTESIAN_POINT ( 'NONE',  ( 208.2995279947827783, 269.8616296508574237, 2.738519832864397152 ) ) ;
#26563 = CARTESIAN_POINT ( 'NONE',  ( 12.78680497239753144, 184.3149278399160949, -9.188101187500095079 ) ) ;
#26564 = FACE_OUTER_BOUND ( 'NONE', #46792, .T. ) ;
#26565 = ORIENTED_EDGE ( 'NONE', *, *, #72185, .F. ) ;
#26566 = ORIENTED_EDGE ( 'NONE', *, *, #43547, .F. ) ;
#26567 = CARTESIAN_POINT ( 'NONE',  ( 147.7140364658288263, 276.4223552458277027, -0.9273017251447416287 ) ) ;
#26568 = CARTESIAN_POINT ( 'NONE',  ( 88.14145358481059134, 44.06566488169897866, 0.5518357132556823696 ) ) ;
#26569 = DIRECTION ( 'NONE',  ( 0.2588190451025027539, 0.9659258262890731972, 6.846136862223680982E-16 ) ) ;
#26570 = LINE ( 'NONE', #73670, #83871 ) ;
#26571 = VECTOR ( 'NONE', #62547, 1000.000000000000000 ) ;
#26572 = CARTESIAN_POINT ( 'NONE',  ( 176.9878821292914211, 283.3466992399841615, -15.40003107629192769 ) ) ;
#26573 = CARTESIAN_POINT ( 'NONE',  ( 68.59280378597286187, 64.14102549347582283, 11.89188498909244629 ) ) ;
#26574 = DIRECTION ( 'NONE',  ( -1.000000000000000000, 0.000000000000000000, -2.816764622163179958E-16 ) ) ;
#26575 = CARTESIAN_POINT ( 'NONE',  ( 44.66719160132967659, 208.8464784336661637, 1.353441290958777525E-15 ) ) ;
#26576 = CARTESIAN_POINT ( 'NONE',  ( 89.99855592466249732, 212.7677522451417929, -5.000000000000041744 ) ) ;
#26577 = EDGE_CURVE ( 'NONE', #73884, #39921, #32423, .T. ) ;
#26578 = ORIENTED_EDGE ( 'NONE', *, *, #30407, .F. ) ;
#26579 = CARTESIAN_POINT ( 'NONE',  ( 84.52987419023656912, 49.02393738901606923, 12.65494964629210983 ) ) ;
#26580 = VECTOR ( 'NONE', #49419, 1000.000000000000000 ) ;
#26581 = LINE ( 'NONE', #34176, #97079 ) ;
#26582 = EDGE_CURVE ( 'NONE', #28659, #23610, #81791, .T. ) ;
#26583 = CARTESIAN_POINT ( 'NONE',  ( 0.9064528339360315989, 162.1423013555410080, -4.594050593750043987 ) ) ;
#26584 = CARTESIAN_POINT ( 'NONE',  ( 68.71429273641867042, 63.93483983531514525, -12.10708682878116527 ) ) ;
#26585 = CARTESIAN_POINT ( 'NONE',  ( 151.0801312611820890, 268.9685319718947198, -15.83903210480701240 ) ) ;
#26586 = CARTESIAN_POINT ( 'NONE',  ( 188.8764293144468240, 259.6972905960182061, 3.583694637520717041 ) ) ;
#26587 = CARTESIAN_POINT ( 'NONE',  ( 147.0456760057551833, 275.9564134551570760, -3.678503029046952033 ) ) ;
#26588 = CARTESIAN_POINT ( 'NONE',  ( 177.5337925685473408, 280.1858537220425092, 16.79564202278857721 ) ) ;
#26589 = CARTESIAN_POINT ( 'NONE',  ( 171.3751619920873281, 280.2398791927632828, 15.33202389549764888 ) ) ;
#26590 = CARTESIAN_POINT ( 'NONE',  ( 191.0604813119340690, 299.7205343796033503, -9.270812881586136811 ) ) ;
#26591 = CARTESIAN_POINT ( 'NONE',  ( 164.8670003495851404, 245.0889742334797177, -1.557028074864921674 ) ) ;
#26592 = EDGE_LOOP ( 'NONE', ( #84019, #83843, #27679, #86744, #54931, #43798, #33492, #83443 ) ) ;
#26593 = CARTESIAN_POINT ( 'NONE',  ( 3.125382611083894702, 162.6115022471902023, -5.000000000000041744 ) ) ;
#26594 = DIRECTION ( 'NONE',  ( 1.000000000000000000, 0.000000000000000000, 0.000000000000000000 ) ) ;
#26595 = CARTESIAN_POINT ( 'NONE',  ( 121.5540962550081190, 250.1744531367911009, 4.594050593750047540 ) ) ;
#26596 = CARTESIAN_POINT ( 'NONE',  ( 20.04711164229383513, 17.28920272979926764, -7.433330006724141015 ) ) ;
#26597 = CARTESIAN_POINT ( 'NONE',  ( 74.89402362195637863, 67.20670802991241999, 12.50338612930198146 ) ) ;
#26598 = CARTESIAN_POINT ( 'NONE',  ( -27.42236680055714260, 166.5217562850347406, 1.224646799147364892E-15 ) ) ;
#26600 = CARTESIAN_POINT ( 'NONE',  ( 185.5710010263521212, 288.0579674285398255, 14.90484884845676383 ) ) ;
#26599 = CARTESIAN_POINT ( 'NONE',  ( 196.4677418905696129, 290.3548843276421394, 17.08610552292358520 ) ) ;
#26601 = EDGE_LOOP ( 'NONE', ( #62988, #53371, #94476, #88483 ) ) ;
#26602 = CARTESIAN_POINT ( 'NONE',  ( 191.2056514706806070, 299.4690922889112699, 7.290007621276087590 ) ) ;
#26603 = CARTESIAN_POINT ( 'NONE',  ( 149.7109319212262051, 271.3400547943878109, -12.38605961032017433 ) ) ;
#26604 = CARTESIAN_POINT ( 'NONE',  ( 190.1308301828542824, 300.0323083375496935, 4.625340536964981375 ) ) ;
#26605 = CARTESIAN_POINT ( 'NONE',  ( 203.5963693286578007, 276.4956262415219612, 14.26529644090561710 ) ) ;
#26606 = CARTESIAN_POINT ( 'NONE',  ( 81.66708723681374238, 55.20605668156866841, -15.91457100465458474 ) ) ;
#26607 = VERTEX_POINT ( 'NONE', #16577 ) ;
#26608 = CARTESIAN_POINT ( 'NONE',  ( 189.0562362369354048, 265.6604396169832398, 11.68942508348690268 ) ) ;
#26609 = DIRECTION ( 'NONE',  ( -1.000000000000000000, 0.000000000000000000, 0.000000000000000000 ) ) ;
#26610 = CARTESIAN_POINT ( 'NONE',  ( 72.10745786146183889, 72.33289146567349803, 0.8714635118042719508 ) ) ;
#26611 = CARTESIAN_POINT ( 'NONE',  ( 77.71017327488615933, 49.43655273470124456, 15.32784876113035288 ) ) ;
#26612 = DIRECTION ( 'NONE',  ( 0.8660254037844379305, 0.5000000000000011102, 0.000000000000000000 ) ) ;
#26613 = CARTESIAN_POINT ( 'NONE',  ( 155.5527680174282068, 261.6201814834243464, 16.99819418695508588 ) ) ;
#26614 = CARTESIAN_POINT ( 'NONE',  ( 72.33760062768145360, 71.68797599686796218, -5.790821312261726916 ) ) ;
#26615 = CARTESIAN_POINT ( 'NONE',  ( 153.0070714074088016, 265.6309737354857248, 17.74442213480098474 ) ) ;
#26616 = VERTEX_POINT ( 'NONE', #50841 ) ;
#26617 = CARTESIAN_POINT ( 'NONE',  ( 198.2505066714982149, 285.2670451491296149, 0.000000000000000000 ) ) ;
#26618 = CARTESIAN_POINT ( 'NONE',  ( 7.614983434379491101, 23.13478043621386249, 8.090169943749478065 ) ) ;
#26619 = CARTESIAN_POINT ( 'NONE',  ( 191.8474946137321524, 287.8597454743107846, -15.89771325201565233 ) ) ;
#26620 = VERTEX_POINT ( 'NONE', #64182 ) ;
#26621 = CARTESIAN_POINT ( 'NONE',  ( 77.92825354283080230, 61.79113456967466789, 16.06764011202815468 ) ) ;
#26622 = CARTESIAN_POINT ( 'NONE',  ( 194.1789525331299728, 294.3191837825503967, -15.34533909744314961 ) ) ;
#26623 = CARTESIAN_POINT ( 'NONE',  ( 159.7423958009181320, 264.1536618208600657, -17.54225510600860716 ) ) ;
#26624 = ORIENTED_EDGE ( 'NONE', *, *, #94328, .T. ) ;
#26625 = CARTESIAN_POINT ( 'NONE',  ( 79.31323107047896315, 59.76145823410249136, 16.51491591541846660 ) ) ;
#26626 = CARTESIAN_POINT ( 'NONE',  ( 204.8815496696085177, 273.0746141528632620, -9.761282367569325658 ) ) ;
#26627 = VERTEX_POINT ( 'NONE', #32774 ) ;
#26628 = CARTESIAN_POINT ( 'NONE',  ( 77.74446929066526479, 52.10494957478874767, -15.63064665268012376 ) ) ;
#26629 = CARTESIAN_POINT ( 'NONE',  ( 177.4877928417686803, 293.5951873982637608, -2.837372163671336267 ) ) ;
#26630 = CARTESIAN_POINT ( 'NONE',  ( 184.4003287965598474, 259.5388931828980503, -5.814281059522229178 ) ) ;
#26631 = ORIENTED_EDGE ( 'NONE', *, *, #45997, .F. ) ;
#26632 = ORIENTED_EDGE ( 'NONE', *, *, #10255, .F. ) ;
#26633 = EDGE_CURVE ( 'NONE', #87662, #77729, #17074, .T. ) ;
#26634 = ORIENTED_EDGE ( 'NONE', *, *, #70890, .F. ) ;
#26635 = DIRECTION ( 'NONE',  ( 0.3978777116982039619, 0.7304723483372554949, 0.5550706935593484603 ) ) ;
#26636 = AXIS2_PLACEMENT_3D ( 'NONE', #993, #38975, #56167 ) ;
#26637 = VERTEX_POINT ( 'NONE', #12368 ) ;
#26638 = EDGE_CURVE ( 'NONE', #6447, #68960, #95130, .T. ) ;
#26639 = CARTESIAN_POINT ( 'NONE',  ( 88.34040369365730783, 44.17924546850527179, 0.3139463615716704958 ) ) ;
#26640 = CARTESIAN_POINT ( 'NONE',  ( 155.1398527401465230, 261.9368881057492899, -17.02245700497956449 ) ) ;
#26641 = ORIENTED_EDGE ( 'NONE', *, *, #98262, .F. ) ;
#26642 = CARTESIAN_POINT ( 'NONE',  ( 82.15513920341352616, 40.66133961728853308, 3.593347833157086502 ) ) ;
#26643 = CARTESIAN_POINT ( 'NONE',  ( 160.4314248734274031, 254.1918255350734057, -15.30701149497589064 ) ) ;
#26644 = CARTESIAN_POINT ( 'NONE',  ( 51.80235952159637236, 80.00000000000000000, -10.00000000000000178 ) ) ;
#26645 = CARTESIAN_POINT ( 'NONE',  ( 147.5749398328735822, 275.0397016159798227, -4.620786157167191099 ) ) ;
#26646 = CARTESIAN_POINT ( 'NONE',  ( 153.2906404175950854, 265.1398178023911782, -17.60231834963988007 ) ) ;
#26647 = EDGE_CURVE ( 'NONE', #76194, #15371, #13911, .T. ) ;
#26648 = CARTESIAN_POINT ( 'NONE',  ( 167.8988096083529911, 276.9559784313423165, -15.94421658709092426 ) ) ;
#26649 = AXIS2_PLACEMENT_3D ( 'NONE', #66506, #32437, #88695 ) ;
#26650 = CARTESIAN_POINT ( 'NONE',  ( 48.32408078245681793, 82.80331927372955647, 10.00000000000000000 ) ) ;
#26651 = CARTESIAN_POINT ( 'NONE',  ( 145.6409484414103588, 245.7048013555409511, 4.594050593750051981 ) ) ;
#26652 = CARTESIAN_POINT ( 'NONE',  ( 88.06269261788008862, 43.61796610520790551, 0.05835779599787207367 ) ) ;
#26653 = ORIENTED_EDGE ( 'NONE', *, *, #88749, .F. ) ;
#26655 = ORIENTED_EDGE ( 'NONE', *, *, #22761, .T. ) ;
#26654 = CARTESIAN_POINT ( 'NONE',  ( 199.9521760394648027, 270.2061738998779674, 9.324312810954292985 ) ) ;
#26656 = DIRECTION ( 'NONE',  ( 0.000000000000000000, 0.000000000000000000, 1.000000000000000000 ) ) ;
#26657 = CARTESIAN_POINT ( 'NONE',  ( -6.635445380951201066, 173.6427522451419065, 10.00000000000009415 ) ) ;
#26658 = CARTESIAN_POINT ( 'NONE',  ( 170.4623819437503016, 288.8056674672355939, -5.476885062779371260 ) ) ;
#26659 = CARTESIAN_POINT ( 'NONE',  ( 157.3440770660893975, 280.1834744503427146, -6.999751510017727441 ) ) ;
#26660 = CARTESIAN_POINT ( 'NONE',  ( 165.4921054121714121, 246.8916612925589220, -1.878118433271425136 ) ) ;
#26661 = CARTESIAN_POINT ( 'NONE',  ( 192.8319713945120668, 292.4878551455605589, -14.36409660672679856 ) ) ;
#26662 = CARTESIAN_POINT ( 'NONE',  ( 72.48661302258760486, 71.52526770760661634, -5.337229783571229014 ) ) ;
#26663 = CARTESIAN_POINT ( 'NONE',  ( 88.30455217607853058, 43.91915848855261828, -2.151936166193182398 ) ) ;
#26664 = ORIENTED_EDGE ( 'NONE', *, *, #60072, .F. ) ;
#26665 = CARTESIAN_POINT ( 'NONE',  ( 147.8819534105757043, 274.5079385007862811, -9.338341377131436971 ) ) ;
#26666 = CARTESIAN_POINT ( 'NONE',  ( 65.95405552260710635, 69.20365738631340946, 0.2585006146049920739 ) ) ;
#26667 = ORIENTED_EDGE ( 'NONE', *, *, #2048, .T. ) ;
#26668 = CARTESIAN_POINT ( 'NONE',  ( 88.33748333995926316, 44.07075497373335793, -2.898134731201826852 ) ) ;
#26669 = CARTESIAN_POINT ( 'NONE',  ( 201.1812938895721459, 267.3327365634810349, -2.234727838033611746 ) ) ;
#26670 = DIRECTION ( 'NONE',  ( 0.3595896960900372696, 0.9331105242498740626, 0.000000000000000000 ) ) ;
#26671 = CARTESIAN_POINT ( 'NONE',  ( 190.2935937139882299, 301.0488226629397559, 4.649863831023156813 ) ) ;
#26672 = CARTESIAN_POINT ( 'NONE',  ( 163.4004183463084416, 247.6291687766210146, 10.19167732382099345 ) ) ;
#26674 = CARTESIAN_POINT ( 'NONE',  ( 88.08517209305595941, 44.29913593851635767, 2.778213776158472648 ) ) ;
#26673 = DIRECTION ( 'NONE',  ( -0.3958915996110536906, -0.9182972510888841589, 0.000000000000000000 ) ) ;
#26675 = VECTOR ( 'NONE', #33205, 999.9999999999998863 ) ;
#26676 = FACE_OUTER_BOUND ( 'NONE', #56425, .T. ) ;
#26677 = ORIENTED_EDGE ( 'NONE', *, *, #24850, .T. ) ;
#26678 = CARTESIAN_POINT ( 'NONE',  ( 74.04344310693554121, 61.81268583747974077, -14.95296161341949848 ) ) ;
#26679 = CARTESIAN_POINT ( 'NONE',  ( 79.83401254395657531, 57.87045807247318407, 16.26439772172797404 ) ) ;
#26680 = DIRECTION ( 'NONE',  ( 0.000000000000000000, 0.000000000000000000, 1.000000000000000000 ) ) ;
#26681 = DIRECTION ( 'NONE',  ( -0.9331105242498700658, 0.3595896960900473172, 0.000000000000000000 ) ) ;
#26682 = CARTESIAN_POINT ( 'NONE',  ( 80.82399500712998019, 43.24504854750488647, -9.930955225068224479 ) ) ;
#26683 = LINE ( 'NONE', #80433, #80646 ) ;
#26684 = CARTESIAN_POINT ( 'NONE',  ( 163.1014434023538513, 248.1470085697407058, 9.692260209037655727 ) ) ;
#26685 = CARTESIAN_POINT ( 'NONE',  ( 0.9872088458345585904, 177.5024278399160949, 9.188101187500095079 ) ) ;
#26686 = CARTESIAN_POINT ( 'NONE',  ( 99.38934535084139554, 234.3149278399160949, 9.188101187500093303 ) ) ;
#26687 = CARTESIAN_POINT ( 'NONE',  ( 202.8535267948003593, 279.2943804273081696, -15.36804658072946062 ) ) ;
#26688 = CARTESIAN_POINT ( 'NONE',  ( 178.2543802835785698, 279.4939343734425279, -17.11033828990027672 ) ) ;
#26689 = CARTESIAN_POINT ( 'NONE',  ( 182.3427999490124307, 257.2899902172831617, -2.311323497713533737 ) ) ;
#26690 = B_SPLINE_CURVE_WITH_KNOTS ( 'NONE', 3,
 ( #20960, #58905, #91360, #19951, #59916, #44707, #90384, #82784, #36120, #28523, #29046, #20450, #5240, #97950, #12861, #75640 ),
 .UNSPECIFIED., .F., .F.,
 ( 4, 1, 2, 2, 2, 1, 2, 2, 4 ),
 ( 0.000000000000000000, 0.1249999999999992506, 0.1874999999999994449, 0.2499999999999996669, 0.4999999999999998890, 0.6250000000000001110, 0.6875000000000003331, 0.7500000000000004441, 1.000000000000000000 ),
 .UNSPECIFIED. ) ;
#26691 = DIRECTION ( 'NONE',  ( -0.9888308262251267466, 0.1490422661761856560, 0.000000000000000000 ) ) ;
#26692 = B_SPLINE_CURVE_WITH_KNOTS ( 'NONE', 3,
 ( #42480, #65301, #75408, #35392, #65786, #73910, #81056, #74915, #43481, #35889, #5010, #96243, #97717, #28285, #90649, #20709, #82550, #50101, #13115, #43974, #5498, #67285, #21207, #4001, #52087, #98212, #83033, #13603, #44477, #26804, #57687, #11619, #34887, #27307, #85020, #46987, #7999, #36886, #83532, #76410, #99204, #67794, #60166, #14096, #29790, #69282 ),
 .UNSPECIFIED., .F., .F.,
 ( 4, 1, 1, 1, 2, 2, 1, 1, 1, 2, 2, 1, 1, 2, 2, 1, 1, 2, 2, 1, 1, 2, 2, 1, 2, 2, 1, 2, 2, 4 ),
 ( 0.000000000000000000, 0.06250000000000983935, 0.09375000000001355860, 0.1093750000000154321, 0.1171875000000157513, 0.1250000000000160705, 0.1875000000000305589, 0.2187500000000371925, 0.2343750000000392741, 0.2421875000000397460, 0.2500000000000401901, 0.3125000000000500711, 0.3437500000000562883, 0.3593750000000585643, 0.3750000000000608957, 0.4375000000000651701, 0.4687500000000668909, 0.4843750000000661138, 0.5000000000000652811, 0.5625000000000554001, 0.5937500000000518474, 0.6093750000000499600, 0.6250000000000480727, 0.6875000000000401901, 0.7187500000000348610, 0.7500000000000295319, 0.8125000000000217604, 0.8437500000000176525, 0.8750000000000136557, 1.000000000000000000 ),
 .UNSPECIFIED. ) ;
#26693 = EDGE_CURVE ( 'NONE', #54647, #11375, #34892, .T. ) ;
#26694 = CARTESIAN_POINT ( 'NONE',  ( 77.15155500632977237, 50.73808484653564221, 15.35664286137126489 ) ) ;
#26695 = DIRECTION ( 'NONE',  ( 0.000000000000000000, 0.000000000000000000, 1.000000000000000000 ) ) ;
#26696 = CARTESIAN_POINT ( 'NONE',  ( 160.1795347027651815, 282.8633239002924711, 5.491715875156680582 ) ) ;
#26697 = CARTESIAN_POINT ( 'NONE',  ( 194.9455394410084921, 292.9914163096879065, -15.01116663483170655 ) ) ;
#26698 = CARTESIAN_POINT ( 'NONE',  ( 181.3660832969280250, 291.3269257893657596, 9.327634650582066200 ) ) ;
#26699 = DIRECTION ( 'NONE',  ( -0.9689225787001330970, 0.2473641778533918756, 0.000000000000000000 ) ) ;
#26700 = CARTESIAN_POINT ( 'NONE',  ( 164.4057847141585285, 245.8878231472837115, -5.819655715517686900 ) ) ;
#26701 = CARTESIAN_POINT ( 'NONE',  ( 2.963002844326352747, 172.5177522451418781, -10.00000000000009592 ) ) ;
#26702 = CARTESIAN_POINT ( 'NONE',  ( 78.04917184312711242, 55.09204980408419772, -16.10415483157210659 ) ) ;
#26703 = CARTESIAN_POINT ( 'NONE',  ( 155.8152618860606253, 260.7670451491295012, 0.000000000000000000 ) ) ;
#26704 = VECTOR ( 'NONE', #18700, 1000.000000000000114 ) ;
#26705 = EDGE_CURVE ( 'NONE', #37717, #56418, #42728, .T. ) ;
#26706 = CARTESIAN_POINT ( 'NONE',  ( 176.1555758231396567, 265.5273580598085914, -16.25916769215487889 ) ) ;
#26707 = ADVANCED_FACE ( 'NONE', ( #66055 ), #27572, .F. ) ;
#26708 = CARTESIAN_POINT ( 'NONE',  ( 77.38680066200176100, 224.6744531367911293, 4.594050593750047540 ) ) ;
#26709 = CARTESIAN_POINT ( 'NONE',  ( 207.8570869662935365, 270.6279599915536664, -5.669188455878507504 ) ) ;
#26711 = CARTESIAN_POINT ( 'NONE',  ( 82.09936887833779906, 51.48109869154082219, -15.14494387904524864 ) ) ;
#26710 = AXIS2_PLACEMENT_3D ( 'NONE', #40639, #63950, #72072 ) ;
#26712 = CARTESIAN_POINT ( 'NONE',  ( 163.3923068497962277, 257.9918827725503547, 15.63397831145243622 ) ) ;
#26714 = DIRECTION ( 'NONE',  ( 0.5076330711061762813, -0.8615733660689097739, 0.000000000000000000 ) ) ;
#26713 = CARTESIAN_POINT ( 'NONE',  ( 86.81854227949330038, 43.42264536667640584, -3.855948753652409522 ) ) ;
#26715 = CARTESIAN_POINT ( 'NONE',  ( 66.54264984482914258, 68.81226801441182772, 2.258477026830895795 ) ) ;
#26716 = CARTESIAN_POINT ( 'NONE',  ( 35.63556891041371699, 26.28920272979929607, -7.433330006724141015 ) ) ;
#26717 = CARTESIAN_POINT ( 'NONE',  ( -19.65312891409030271, 93.06504152958497400, -10.00000000000000888 ) ) ;
#26718 = CARTESIAN_POINT ( 'NONE',  ( 74.57503898873223136, 56.40329876199222525, 16.56847014829402553 ) ) ;
#26719 = VERTEX_POINT ( 'NONE', #1893 ) ;
#26720 = CARTESIAN_POINT ( 'NONE',  ( 17.19404571121151548, 18.43085787977762280, -9.188101187500008038 ) ) ;
#26721 = CARTESIAN_POINT ( 'NONE',  ( 71.08131351252005459, 211.8458772461660544, 9.188101187500095079 ) ) ;
#26722 = CARTESIAN_POINT ( 'NONE',  ( 171.5149613532572914, 288.8291111043322417, -1.065049549448901844 ) ) ;
#26723 = DIRECTION ( 'NONE',  ( -0.9506327454577400138, -0.3103181967972222788, 0.000000000000000000 ) ) ;
#26724 = CARTESIAN_POINT ( 'NONE',  ( 188.2744068810562510, 286.2937481655858960, -16.77334613339053249 ) ) ;
#26725 = CARTESIAN_POINT ( 'NONE',  ( 86.25117823697901542, 47.20812847272011226, 10.82755581481952056 ) ) ;
#26726 = CARTESIAN_POINT ( 'NONE',  ( 191.7501012462608116, 287.4658672486679052, 16.07335574080813245 ) ) ;
#26727 = CARTESIAN_POINT ( 'NONE',  ( -17.42236680055705023, 149.2012482093457777, 0.000000000000000000 ) ) ;
#26728 = CARTESIAN_POINT ( 'NONE',  ( 129.2042476453684117, 238.7365022471901739, -10.00000000000009059 ) ) ;
#26729 = DIRECTION ( 'NONE',  ( -0.000000000000000000, -1.000000000000000000, -0.000000000000000000 ) ) ;
#26730 = CARTESIAN_POINT ( 'NONE',  ( 74.96166150690207530, 53.27833328053394979, 16.04207443345645245 ) ) ;
#26731 = ORIENTED_EDGE ( 'NONE', *, *, #83987, .F. ) ;
#26732 = CARTESIAN_POINT ( 'NONE',  ( 165.6980386070991926, 247.0211899460981044, -1.865356867150344655 ) ) ;
#26733 = VERTEX_POINT ( 'NONE', #58438 ) ;
#26734 = CARTESIAN_POINT ( 'NONE',  ( 162.9796882977680639, 248.3578945969637743, 9.683801903336119565 ) ) ;
#26735 = CARTESIAN_POINT ( 'NONE',  ( 1.030962353892107330, 22.93863946572252743, 0.000000000000000000 ) ) ;
#26736 = FACE_OUTER_BOUND ( 'NONE', #85499, .T. ) ;
#26737 = ORIENTED_EDGE ( 'NONE', *, *, #77236, .F. ) ;
#26738 = CARTESIAN_POINT ( 'NONE',  ( 77.30414578634690770, 63.13278840050173812, -15.24465609931389487 ) ) ;
#26739 = ORIENTED_EDGE ( 'NONE', *, *, #63363, .T. ) ;
#26740 = CARTESIAN_POINT ( 'NONE',  ( 189.4441960630004189, 289.9932173292452262, 14.44447376131311778 ) ) ;
#26741 = CARTESIAN_POINT ( 'NONE',  ( 40.18174127881769664, 205.5530062829863027, -4.648177544792955347E-16 ) ) ;
#26742 = CARTESIAN_POINT ( 'NONE',  ( 48.83428215874786815, 87.09189275153327969, 10.00000000000000000 ) ) ;
#26743 = CARTESIAN_POINT ( 'NONE',  ( 83.13827405794465619, 47.56982798971775139, 12.68584740263780297 ) ) ;
#26744 = ORIENTED_EDGE ( 'NONE', *, *, #9835, .F. ) ;
#26745 = CARTESIAN_POINT ( 'NONE',  ( 110.1516887621107657, 227.7365022471902307, 10.00000000000009948 ) ) ;
#26746 = AXIS2_PLACEMENT_3D ( 'NONE', #88863, #4698, #88357 ) ;
#26747 = CARTESIAN_POINT ( 'NONE',  ( 28.38624132378438958, 39.49540643055189548, 3.479690158560446702E-15 ) ) ;
#26748 = CARTESIAN_POINT ( 'NONE',  ( 84.80399932964064647, 47.93957977109545254, -11.70082172808313103 ) ) ;
#26749 = ADVANCED_FACE ( 'NONE', ( #91883 ), #5253, .T. ) ;
#26750 = FACE_OUTER_BOUND ( 'NONE', #50913, .T. ) ;
#26751 = B_SPLINE_CURVE_WITH_KNOTS ( 'NONE', 3,
 ( #82963, #85327, #97650, #5429, #15872, #8288, #13048, #8782, #28217, #16381, #54873, #82485, #26494, #33083, #87855, #41669, #80229, #17901, #63978, #48290, #25482, #48798, #79729, #10797 ),
 .UNSPECIFIED., .F., .F.,
 ( 4, 2, 2, 2, 2, 2, 2, 2, 2, 2, 2, 4 ),
 ( 0.000000000000000000, 0.1249999999999956701, 0.2499999999999913403, 0.3749999999999870104, 0.4374999999999887312, 0.4999999999999900080, 0.5624999999999912292, 0.6249999999999925615, 0.6874999999999937828, 0.7499999999999951150, 0.8749999999999975575, 1.000000000000000000 ),
 .UNSPECIFIED. ) ;
#26752 = CARTESIAN_POINT ( 'NONE',  ( 53.05822266071304938, 189.8932355074535678, -2.679491924311248496 ) ) ;
#26753 = VERTEX_POINT ( 'NONE', #60417 ) ;
#26754 = VERTEX_POINT ( 'NONE', #98466 ) ;
#26755 = CARTESIAN_POINT ( 'NONE',  ( 186.3700259935355064, 298.5219211581387526, 1.062272678801966297 ) ) ;
#26757 = CARTESIAN_POINT ( 'NONE',  ( 147.7785919239399846, 274.6869658471848652, -7.924750738206837397 ) ) ;
#26756 = CARTESIAN_POINT ( 'NONE',  ( 204.2457645315488719, 276.8829539310449945, 14.53406579917280261 ) ) ;
#26758 = CARTESIAN_POINT ( 'NONE',  ( 85.51397903554266122, 48.65227260402726017, 12.46570927396283146 ) ) ;
#26759 = LINE ( 'NONE', #57642, #79750 ) ;
#26760 = CARTESIAN_POINT ( 'NONE',  ( 190.7685386727469279, 298.2261938635710976, -9.678376712886644029 ) ) ;
#26761 = CARTESIAN_POINT ( 'NONE',  ( 187.5841530998652331, 291.2525622860537169, -13.74720276183634660 ) ) ;
#26762 = EDGE_CURVE ( 'NONE', #13784, #52411, #62329, .T. ) ;
#26763 = CARTESIAN_POINT ( 'NONE',  ( 164.1886994716367383, 246.2638258169049266, 4.302100816186628762 ) ) ;
#26764 = EDGE_CURVE ( 'NONE', #8604, #65750, #36630, .T. ) ;
#26765 = DIRECTION ( 'NONE',  ( -0.2168075248790319320, -0.9762143704923770260, 0.000000000000000000 ) ) ;
#26766 = CARTESIAN_POINT ( 'NONE',  ( 79.40659458863603959, 59.69041580281565018, 16.52608132308843736 ) ) ;
#26767 = CARTESIAN_POINT ( 'NONE',  ( 103.3950599391094443, 224.3768266524160140, -9.188101187500091527 ) ) ;
#26768 = ORIENTED_EDGE ( 'NONE', *, *, #69625, .F. ) ;
#26769 = LINE ( 'NONE', #27768, #80377 ) ;
#26770 = CARTESIAN_POINT ( 'NONE',  ( 166.2786698706664765, 279.3007919285489606, -14.16120680810289301 ) ) ;
#26771 = EDGE_LOOP ( 'NONE', ( #19058, #37229, #43558, #17827 ) ) ;
#26772 = ORIENTED_EDGE ( 'NONE', *, *, #2576, .F. ) ;
#26773 = B_SPLINE_CURVE_WITH_KNOTS ( 'NONE', 3,
 ( #91545, #45882, #16501, #31195 ),
 .UNSPECIFIED., .F., .F.,
 ( 4, 4 ),
 ( 0.01063587648819574669, 0.01619468505063361569 ),
 .UNSPECIFIED. ) ;
#26774 = CARTESIAN_POINT ( 'NONE',  ( 86.97822204926990253, 45.79386009709899952, -8.643660422075560845 ) ) ;
#26775 = LINE ( 'NONE', #19693, #77048 ) ;
#26776 = CARTESIAN_POINT ( 'NONE',  ( 163.0358311274019343, 249.2395244830586307, 10.27721552788938908 ) ) ;
#26777 = CARTESIAN_POINT ( 'NONE',  ( 206.6912923161529818, 272.6471755567893638, -9.325620632947922317 ) ) ;
#26778 = CARTESIAN_POINT ( 'NONE',  ( 208.0941653616417852, 270.2173281654339689, 1.603026803260118704 ) ) ;
#26779 = CARTESIAN_POINT ( 'NONE',  ( 94.00418374076319594, 215.8923013555410080, 4.594050593750050204 ) ) ;
#26780 = ORIENTED_EDGE ( 'NONE', *, *, #5267, .T. ) ;
#26781 = AXIS2_PLACEMENT_3D ( 'NONE', #77934, #55595, #86578 ) ;
#26782 = ORIENTED_EDGE ( 'NONE', *, *, #24538, .F. ) ;
#26783 = CARTESIAN_POINT ( 'NONE',  ( 162.7007457333762090, 248.8410372908842021, -10.94671474643812914 ) ) ;
#26784 = VERTEX_POINT ( 'NONE', #28537 ) ;
#26785 =( GEOMETRIC_REPRESENTATION_CONTEXT ( 3 ) GLOBAL_UNCERTAINTY_ASSIGNED_CONTEXT ( ( #79803 ) ) GLOBAL_UNIT_ASSIGNED_CONTEXT ( ( #80219, #17894, #57364 ) ) REPRESENTATION_CONTEXT ( 'NONE', 'WORKASPACE' ) );
#26786 = CARTESIAN_POINT ( 'NONE',  ( -19.65312891409030271, 93.06504152958497400, -10.00000000000000888 ) ) ;
#26787 = CARTESIAN_POINT ( 'NONE',  ( 183.6498318386265396, 256.3252116762061519, 1.424693195823348635 ) ) ;
#26788 = CARTESIAN_POINT ( 'NONE',  ( 165.5754880998921408, 285.4032371899495502, 0.7844207949055206353 ) ) ;
#26790 = CARTESIAN_POINT ( 'NONE',  ( 69.70373566977634994, 62.70902085928403835, -13.31389724659099016 ) ) ;
#26789 = CARTESIAN_POINT ( 'NONE',  ( 137.4944631173567018, 256.3149278399160380, -9.188101187500095079 ) ) ;
#26791 = CARTESIAN_POINT ( 'NONE',  ( -6.130263895410251962, 167.2677522451418781, 10.00000000000009592 ) ) ;
#26792 = LINE ( 'NONE', #35378, #65799 ) ;
#26793 = CARTESIAN_POINT ( 'NONE',  ( 86.85456002791893582, 44.01107763648593618, -4.201576838953794635 ) ) ;
#26794 = CARTESIAN_POINT ( 'NONE',  ( 81.44373164288916200, 47.79091324518223871, 12.93866338402850147 ) ) ;
#26795 = CARTESIAN_POINT ( 'NONE',  ( 22.45462004596304695, 37.14601545153949047, 10.00000000000000000 ) ) ;
#26796 = CARTESIAN_POINT ( 'NONE',  ( -19.65312891409030271, 93.06504152958497400, 177.5919119679930134 ) ) ;
#26797 = CARTESIAN_POINT ( 'NONE',  ( 114.8426596992763962, 247.1115022471903160, -5.000000000000047962 ) ) ;
#26798 = B_SPLINE_CURVE_WITH_KNOTS ( 'NONE', 3,
 ( #55139, #10067, #86124, #17667, #16654, #95209, #38944, #69850 ),
 .UNSPECIFIED., .F., .F.,
 ( 4, 2, 2, 4 ),
 ( 0.6245648125881849699, 0.7184236094411386997, 0.8122824062940925405, 1.000000000000000000 ),
 .UNSPECIFIED. ) ;
#26799 = DIRECTION ( 'NONE',  ( -0.8660254037844384856, -0.5000000000000002220, -3.252519625699449945E-16 ) ) ;
#26800 = DIRECTION ( 'NONE',  ( 0.4999999999999992784, -0.8660254037844390407, 0.000000000000000000 ) ) ;
#26801 = DIRECTION ( 'NONE',  ( 0.000000000000000000, 0.000000000000000000, 1.000000000000000000 ) ) ;
#26802 =( BOUNDED_CURVE ( )  B_SPLINE_CURVE ( 2, ( #61404, #58300, #19826, #81651, #88779, #73039, #87298, #72030, #72545 ),
 .UNSPECIFIED., .F., .T. ) 
 B_SPLINE_CURVE_WITH_KNOTS ( ( 3, 2, 2, 2, 3 ),
 ( 0.6169354838709677491, 0.6182795698924731242, 0.6209677419354838745, 0.6236559139784946248, 0.6250000000000000000 ),
 .UNSPECIFIED. ) 
 CURVE ( )  GEOMETRIC_REPRESENTATION_ITEM ( )  RATIONAL_B_SPLINE_CURVE ( ( 0.9330127018922194093, 0.9330127018922194093, 1.000000000000000000, 0.8660254037844387076, 1.000000000000000000, 0.8660254037844387076, 1.000000000000000000, 0.9330127018922194093, 0.9330127018922194093 ) ) 
 REPRESENTATION_ITEM ( '' )  );
#26803 = CARTESIAN_POINT ( 'NONE',  ( 80.01120875526221710, 50.16365770749508357, 14.62385428340041926 ) ) ;
#26804 = CARTESIAN_POINT ( 'NONE',  ( 70.25980337983864388, 70.48501441192767913, -4.468181338594434671 ) ) ;
#26805 = CARTESIAN_POINT ( 'NONE',  ( 206.8851632406098702, 272.3113812655195716, -9.957011741946159233 ) ) ;
#26806 = CARTESIAN_POINT ( 'NONE',  ( 78.17252251050902601, 61.73722341659915713, 16.11086890919064274 ) ) ;
#26807 = CARTESIAN_POINT ( 'NONE',  ( 207.5920568422024814, 271.0870056320159165, -1.586464549033245186 ) ) ;
#26808 = CARTESIAN_POINT ( 'NONE',  ( 202.5283990184146035, 279.8575182549602118, -15.90040239656587140 ) ) ;
#26809 = CARTESIAN_POINT ( 'NONE',  ( 30.24436146177389162, 33.16454794089043645, -10.00000000000000355 ) ) ;
#26811 = EDGE_CURVE ( 'NONE', #29721, #51689, #44227, .T. ) ;
#26810 = AXIS2_PLACEMENT_3D ( 'NONE', #72163, #79295, #9865 ) ;
#26812 = CARTESIAN_POINT ( 'NONE',  ( 70.67237675181191037, 64.83686998721212547, -12.31838050195076839 ) ) ;
#26813 = CARTESIAN_POINT ( 'NONE',  ( 185.1232581413127036, 266.3925326034153613, 13.18423089168799933 ) ) ;
#26814 = CARTESIAN_POINT ( 'NONE',  ( 170.1892289429057996, 282.6882086596259001, 13.36031953422248364 ) ) ;
#26815 = EDGE_CURVE ( 'NONE', #52681, #23462, #84246, .T. ) ;
#26816 = CARTESIAN_POINT ( 'NONE',  ( 29.28550225947944341, 41.00034080476293497, -1.878358725466461243E-16 ) ) ;
#26817 = CARTESIAN_POINT ( 'NONE',  ( 90.89058176318043536, 234.8297689869269220, -2.679491924311252493 ) ) ;
#26819 = DIRECTION ( 'NONE',  ( -0.9514785060800255989, 0.3077152132536228324, 0.000000000000000000 ) ) ;
#26818 =( BOUNDED_CURVE ( )  B_SPLINE_CURVE ( 2, ( #62469, #23988, #84835, #40175, #24986, #15373, #31081, #1715, #15885, #47284, #38686, #46271, #16393 ),
 .UNSPECIFIED., .F., .T. ) 
 B_SPLINE_CURVE_WITH_KNOTS ( ( 3, 2, 2, 2, 2, 2, 3 ),
 ( 0.4375000000000000000, 0.4400000000000000022, 0.4450000000000000067, 0.4500000000000000111, 0.4550000000000000155, 0.4600000000000000200, 0.4625000000000000222 ),
 .UNSPECIFIED. ) 
 CURVE ( )  GEOMETRIC_REPRESENTATION_ITEM ( )  RATIONAL_B_SPLINE_CURVE ( ( 0.9755282581475768211, 0.9755282581475768211, 1.000000000000000000, 0.9510565162951535312, 1.000000000000000000, 0.9510565162951535312, 1.000000000000000000, 0.9510565162951535312, 1.000000000000000000, 0.9510565162951535312, 1.000000000000000000, 0.9755282581475768211, 0.9755282581475768211 ) ) 
 REPRESENTATION_ITEM ( '' )  );
#26820 = CARTESIAN_POINT ( 'NONE',  ( 158.0014590649305717, 271.2370772881457697, -14.70865708044451736 ) ) ;
#26821 = CARTESIAN_POINT ( 'NONE',  ( 83.86240323164606991, 43.27496035831070742, -6.513153732076713887 ) ) ;
#26822 = CARTESIAN_POINT ( 'NONE',  ( 161.1150691641480535, 251.5875096731584506, -13.48836942566120101 ) ) ;
#26823 = CARTESIAN_POINT ( 'NONE',  ( 15.03297158952216961, 188.6744531367911293, 4.594050593750047540 ) ) ;
#26824 = PLANE ( 'NONE',  #25810 ) ;
#26825 = ORIENTED_EDGE ( 'NONE', *, *, #64750, .T. ) ;
#26826 = EDGE_CURVE ( 'NONE', #26527, #34648, #52652, .T. ) ;
#26827 = CARTESIAN_POINT ( 'NONE',  ( 86.91463931152809153, 46.48516107814676701, 8.998642835661645023 ) ) ;
#26828 = CARTESIAN_POINT ( 'NONE',  ( 195.6664450926536460, 278.3245960621525796, 17.18455885460583232 ) ) ;
#26829 = CARTESIAN_POINT ( 'NONE',  ( 81.72551602421658856, 41.61951536209159741, 5.485699263129209413 ) ) ;
#26830 = CARTESIAN_POINT ( 'NONE',  ( 37.30632276492696064, 192.3458772461660544, 9.188101187500095079 ) ) ;
#26832 = EDGE_CURVE ( 'NONE', #55869, #70967, #75165, .T. ) ;
#26831 = CARTESIAN_POINT ( 'NONE',  ( 161.6256441450323678, 250.7031678651938762, 14.48526717260977037 ) ) ;
#26833 = CARTESIAN_POINT ( 'NONE',  ( 146.9709166616330549, 276.0859004375172390, 3.755270622130282732 ) ) ;
#26834 = CARTESIAN_POINT ( 'NONE',  ( 37.49256495613256845, 26.81029122506297568, 8.090169943749479842 ) ) ;
#26835 = CARTESIAN_POINT ( 'NONE',  ( 178.0294974782117947, 292.4800352430163457, 5.617471776230186009 ) ) ;
#26836 = LINE ( 'NONE', #35425, #28566 ) ;
#26837 = AXIS2_PLACEMENT_3D ( 'NONE', #55058, #86041, #54544 ) ;
#26838 = AXIS2_PLACEMENT_3D ( 'NONE', #56200, #41505, #2537 ) ;
#26839 = CARTESIAN_POINT ( 'NONE',  ( 179.9555032624530497, 279.0079853041619913, -17.36825822513608486 ) ) ;
#26840 = CARTESIAN_POINT ( 'NONE',  ( 35.03822396736671152, 49.37458582131907292, -10.00000000000000000 ) ) ;
#26841 = CARTESIAN_POINT ( 'NONE',  ( 164.5980941468485526, 256.8328644044750035, -14.91555327743531834 ) ) ;
#26842 = EDGE_CURVE ( 'NONE', #68153, #40206, #65933, .T. ) ;
#26843 = LINE ( 'NONE', #88697, #40153 ) ;
#26844 = ADVANCED_FACE ( 'NONE', ( #74677 ), #89889, .F. ) ;
#26845 = AXIS2_PLACEMENT_3D ( 'NONE', #67231, #19667, #98160 ) ;
#26846 = CARTESIAN_POINT ( 'NONE',  ( 83.66574516303664666, 219.1115022471902591, 10.00000000000009592 ) ) ;
#26847 = DIRECTION ( 'NONE',  ( -0.4554470513245823526, -0.8902628732232651387, 0.000000000000000000 ) ) ;
#26848 = CARTESIAN_POINT ( 'NONE',  ( 39.81344631580554250, 23.39040679176985904, -6.890680421881970419E-14 ) ) ;
#26849 = CARTESIAN_POINT ( 'NONE',  ( 49.15987193134396449, 205.3149278399160949, -9.188101187500095079 ) ) ;
#26850 = VERTEX_POINT ( 'NONE', #21936 ) ;
#26851 = CARTESIAN_POINT ( 'NONE',  ( -10.52443098933919785, 85.48226290750096723, 14.42878460834265120 ) ) ;
#26852 = CARTESIAN_POINT ( 'NONE',  ( 150.7691137448031213, 269.5072301123068428, -15.63821625702598084 ) ) ;
#26853 = CARTESIAN_POINT ( 'NONE',  ( 67.04979016446885964, 67.03861818912726278, -8.640631002729076471 ) ) ;
#26854 = VERTEX_POINT ( 'NONE', #45232 ) ;
#26855 = CARTESIAN_POINT ( 'NONE',  ( 168.3183238356223228, 286.2632724110728759, 8.085195618967237152 ) ) ;
#26856 = CARTESIAN_POINT ( 'NONE',  ( 207.1059763530604698, 271.9289217357780899, 6.370907250589925575 ) ) ;
#26857 = CARTESIAN_POINT ( 'NONE',  ( 159.8440474668410332, 278.4957488270735553, -10.68596225390687415 ) ) ;
#26858 = CARTESIAN_POINT ( 'NONE',  ( 28.45357225853751260, 28.37878583063842441, 9.188101187500006262 ) ) ;
#26859 = CARTESIAN_POINT ( 'NONE',  ( 185.7602392900914481, 263.0086591247442129, 11.24710565870787882 ) ) ;
#26860 = CARTESIAN_POINT ( 'NONE',  ( 86.50518482659130370, 47.16427830571769420, -10.09192607653805318 ) ) ;
#26861 = FACE_OUTER_BOUND ( 'NONE', #9053, .T. ) ;
#26862 = ORIENTED_EDGE ( 'NONE', *, *, #97469, .F. ) ;
#26863 = CARTESIAN_POINT ( 'NONE',  ( 13.34565549823491004, 29.74646525600389424, 2.839279412974139660 ) ) ;
#26864 = CARTESIAN_POINT ( 'NONE',  ( 76.05556955939475472, 60.28745929515056901, 15.74899105576687397 ) ) ;
#26865 = CARTESIAN_POINT ( 'NONE',  ( 174.6110402932947636, 255.0538503848414109, 8.239021665820192908 ) ) ;
#26866 = CARTESIAN_POINT ( 'NONE',  ( 12.20045371381521626, 28.81751292744055348, -6.180339887498951690 ) ) ;
#26867 = EDGE_CURVE ( 'NONE', #26719, #56559, #69525, .T. ) ;
#26868 = ORIENTED_EDGE ( 'NONE', *, *, #73876, .F. ) ;
#26869 = CARTESIAN_POINT ( 'NONE',  ( 178.6471812665516552, 282.3158997316623982, 15.55331189247123547 ) ) ;
#26870 = CARTESIAN_POINT ( 'NONE',  ( 190.8443993347725325, 300.0947993426467519, 8.522468760355437212 ) ) ;
#26871 = CARTESIAN_POINT ( 'NONE',  ( 177.4279444979247273, 255.8030325494246711, -6.933745715773924623 ) ) ;
#26872 = LINE ( 'NONE', #49658, #43120 ) ;
#26873 = VERTEX_POINT ( 'NONE', #38111 ) ;
#26874 = EDGE_LOOP ( 'NONE', ( #42200, #70648, #51099, #54822, #41274 ) ) ;
#26875 = EDGE_CURVE ( 'NONE', #67548, #11833, #7736, .T. ) ;
#26877 = LINE ( 'NONE', #26380, #63725 ) ;
#26876 = CARTESIAN_POINT ( 'NONE',  ( 207.8792014703394671, 270.5896565469619759, -5.780233892547864905 ) ) ;
#26878 = CARTESIAN_POINT ( 'NONE',  ( 196.7491951525289835, 289.8673929779723721, -16.35352603081977207 ) ) ;
#26879 = ORIENTED_EDGE ( 'NONE', *, *, #21399, .T. ) ;
#26880 = CARTESIAN_POINT ( 'NONE',  ( 66.19894089851189278, 69.19767938403377627, -2.070941327739651339 ) ) ;
#26881 = CARTESIAN_POINT ( 'NONE',  ( 198.2489255580726422, 287.2697837179150042, 18.53597557040773225 ) ) ;
#26882 = CARTESIAN_POINT ( 'NONE',  ( 68.20887950783240683, 70.50781471800318911, 6.446984873749973067E-06 ) ) ;
#26883 = CARTESIAN_POINT ( 'NONE',  ( 77.82180247422382990, 61.41261899432889493, -16.13690189282890941 ) ) ;
#26884 = CARTESIAN_POINT ( 'NONE',  ( 157.7733463334721478, 257.3755434007023268, -16.94489513499352995 ) ) ;
#26885 = CARTESIAN_POINT ( 'NONE',  ( 109.0781781035623226, 233.7833772461660544, -9.188101187500095079 ) ) ;
#26886 = EDGE_CURVE ( 'NONE', #1592, #45024, #61425, .T. ) ;
#26887 = CARTESIAN_POINT ( 'NONE',  ( 204.5621601773678719, 270.1235943821444607, 7.273613950894332270 ) ) ;
#26888 = CARTESIAN_POINT ( 'NONE',  ( 35.43895548624285396, 181.2677522451417929, -5.000000000000041744 ) ) ;
#26890 = EDGE_CURVE ( 'NONE', #96352, #23472, #92378, .T. ) ;
#26889 = VECTOR ( 'NONE', #28793, 1000.000000000000000 ) ;
#26891 = CARTESIAN_POINT ( 'NONE',  ( 208.3135187673106543, 269.8373969220020285, 2.829653198597726682 ) ) ;
#26892 = ORIENTED_EDGE ( 'NONE', *, *, #21264, .F. ) ;
#26893 = EDGE_CURVE ( 'NONE', #89775, #52670, #70527, .T. ) ;
#26894 = CARTESIAN_POINT ( 'NONE',  ( 37.65389587561885776, 30.24335787977765833, -9.188101187500008038 ) ) ;
#26895 = FACE_BOUND ( 'NONE', #33140, .T. ) ;
#26896 = CARTESIAN_POINT ( 'NONE',  ( 75.28544958660151565, 66.51564022635962203, -13.12383671828155407 ) ) ;
#26897 = CARTESIAN_POINT ( 'NONE',  ( 77.73905735199544154, 209.5643266524159856, -9.188101187500093303 ) ) ;
#26898 = FACE_OUTER_BOUND ( 'NONE', #67472, .T. ) ;
#26899 = CARTESIAN_POINT ( 'NONE',  ( 151.4361976351029000, 268.3518069213970421, 15.15218985681980612 ) ) ;
#26900 = CARTESIAN_POINT ( 'NONE',  ( 199.3352131601118344, 270.6712675723642292, 12.00403451141520250 ) ) ;
#26901 = CARTESIAN_POINT ( 'NONE',  ( 81.63706098559951840, 206.3932355074535963, -2.679491924311248496 ) ) ;
#26902 = ORIENTED_EDGE ( 'NONE', *, *, #22040, .T. ) ;
#26903 = CARTESIAN_POINT ( 'NONE',  ( 79.06560434158508599, 56.99523315522970535, -16.20124195947191126 ) ) ;
#26904 = CARTESIAN_POINT ( 'NONE',  ( 155.6066474290145720, 261.1283759879266881, -18.16552045242181279 ) ) ;
#26905 = EDGE_LOOP ( 'NONE', ( #79321, #23851, #56130, #57829 ) ) ;
#26906 = CARTESIAN_POINT ( 'NONE',  ( 91.00660716696485508, 234.8967562850347122, -4.648177544792955347E-16 ) ) ;
#26907 = CARTESIAN_POINT ( 'NONE',  ( 66.90064016111628575, 68.95865979773512322, -2.633467781610826286 ) ) ;
#26908 = CARTESIAN_POINT ( 'NONE',  ( 163.0918957739551445, 259.9684307908772212, -16.22645816865646040 ) ) ;
#26909 = CARTESIAN_POINT ( 'NONE',  ( 206.6785509007829944, 270.7286264247209715, 2.448473520048410013 ) ) ;
#26910 = CARTESIAN_POINT ( 'NONE',  ( 190.1190668544949460, 301.3511120508678118, 4.410340539513557090 ) ) ;
#26911 = CARTESIAN_POINT ( 'NONE',  ( 164.2572333502590709, 246.1451216570909253, 2.155809084027023204 ) ) ;
#26912 = CARTESIAN_POINT ( 'NONE',  ( 152.3820699219956225, 270.2311863471538800, -14.73681983046514254 ) ) ;
#26913 = CARTESIAN_POINT ( 'NONE',  ( 75.59250669426468505, 65.53249472979591417, 13.80495133635462679 ) ) ;
#26914 = CARTESIAN_POINT ( 'NONE',  ( 166.4111547595541367, 255.8261474448014781, 13.77734897554943849 ) ) ;
#26915 = CARTESIAN_POINT ( 'NONE',  ( 163.7423057141168385, 247.0370024851108610, -6.909410042141566066 ) ) ;
#26916 = CARTESIAN_POINT ( 'NONE',  ( 122.2307653756559773, 247.5024278399160949, -9.188101187500093303 ) ) ;
#26917 = ORIENTED_EDGE ( 'NONE', *, *, #19007, .T. ) ;
#26918 = VECTOR ( 'NONE', #89146, 1000.000000000000114 ) ;
#26919 = CARTESIAN_POINT ( 'NONE',  ( 86.14665820123012452, 44.21313626661029872, -5.852833583934166306 ) ) ;
#26920 = CYLINDRICAL_SURFACE ( 'NONE', #69125, 16.60714546451156792 ) ;
#26921 = DIRECTION ( 'NONE',  ( -0.1039558454088829048, 0.1800568059919617214, 0.9781476007338041345 ) ) ;
#26922 = CIRCLE ( 'NONE', #39748, 60.00000000000002132 ) ;
#26923 = CARTESIAN_POINT ( 'NONE',  ( 105.0000000000000000, 4.999999999999999112, -54.99999999999999289 ) ) ;
#26924 = CARTESIAN_POINT ( 'NONE',  ( 73.91315373279360301, 56.96484810097162210, 16.01878388499446615 ) ) ;
#26925 = FACE_OUTER_BOUND ( 'NONE', #63892, .T. ) ;
#26926 = ORIENTED_EDGE ( 'NONE', *, *, #8556, .F. ) ;
#26927 = CARTESIAN_POINT ( 'NONE',  ( 179.4722142099873565, 269.7276464518548096, -17.35046799866735157 ) ) ;
#26928 = CARTESIAN_POINT ( 'NONE',  ( 152.6809499003229860, 273.9044486092186048, 12.24870461040242553 ) ) ;
#26930 = CARTESIAN_POINT ( 'NONE',  ( 79.14312167556931854, 57.64441083166269664, 0.000000000000000000 ) ) ;
#26929 = CARTESIAN_POINT ( 'NONE',  ( 147.7177902700356071, 275.4030622120182557, 3.691961389914627745 ) ) ;
#26931 = CARTESIAN_POINT ( 'NONE',  ( 206.5431607373320730, 272.9037469775124691, -11.15649369879132102 ) ) ;
#26932 = CARTESIAN_POINT ( 'NONE',  ( 143.7012754916490280, 257.3569598644533585, -9.188101187500093303 ) ) ;
#26933 = CARTESIAN_POINT ( 'NONE',  ( 18.37649865285644779, 192.9637435831425023, 2.679491924311251605 ) ) ;
#26934 = CARTESIAN_POINT ( 'NONE',  ( -19.65312891409030271, 93.06504152958497400, 177.5919119679930134 ) ) ;
#26935 = CARTESIAN_POINT ( 'NONE',  ( -19.78992125718828277, 93.02760366756663757, 59.99999999999999289 ) ) ;
#26936 = CARTESIAN_POINT ( 'NONE',  ( 23.01911539893306013, 18.45404122711133255, -8.090169943749478065 ) ) ;
#26937 = CARTESIAN_POINT ( 'NONE',  ( 190.2389970918280540, 301.1433867864428748, 4.601241515604689525 ) ) ;
#26938 = DIRECTION ( 'NONE',  ( 0.02977611660964677234, -0.9995565931350004485, -0.000000000000000000 ) ) ;
#26939 = CARTESIAN_POINT ( 'NONE',  ( 171.4999057815707033, 286.5447579310401238, -8.034712056625934906 ) ) ;
#26940 = CARTESIAN_POINT ( 'NONE',  ( 205.0025969320384718, 269.2761223580778847, -4.589315089892217259 ) ) ;
#26941 = CARTESIAN_POINT ( 'NONE',  ( 186.1630411436486554, 296.9614825196608194, -7.488375694256206749 ) ) ;
#26942 = CARTESIAN_POINT ( 'NONE',  ( 137.9907970510500661, 257.1427522451419350, -10.00000000000009415 ) ) ;
#26943 = CARTESIAN_POINT ( 'NONE',  ( 82.42646601710040954, 51.29741023544101353, -14.55490622455238992 ) ) ;
#26944 = ORIENTED_EDGE ( 'NONE', *, *, #88894, .T. ) ;
#26945 = EDGE_CURVE ( 'NONE', #23996, #80478, #45298, .T. ) ;
#26946 = CARTESIAN_POINT ( 'NONE',  ( 157.5520850189458884, 257.7587792392113215, 16.71892742266126319 ) ) ;
#26947 = CARTESIAN_POINT ( 'NONE',  ( 148.3930300673291640, 273.6227277647267897, 8.375036249079425232 ) ) ;
#26948 = CARTESIAN_POINT ( 'NONE',  ( 0.5816933075168655431, 161.9548013555410080, -4.594050593750042211 ) ) ;
#26949 = AXIS2_PLACEMENT_3D ( 'NONE', #37848, #90625, #52068 ) ;
#26950 = CARTESIAN_POINT ( 'NONE',  ( 44.12627281972940807, 196.2833772461660828, -9.188101187500095079 ) ) ;
#26951 = CARTESIAN_POINT ( 'NONE',  ( 178.6463706910270730, 259.1961072996702455, -10.35245457583735629 ) ) ;
#26952 = CARTESIAN_POINT ( 'NONE',  ( 20.50317736733639862, 20.03677371833801502, 10.00000000000000533 ) ) ;
#26953 = CARTESIAN_POINT ( 'NONE',  ( -107.5954152546898257, 65.38554960527383741, -21.50000000000000000 ) ) ;
#26954 = CARTESIAN_POINT ( 'NONE',  ( 205.3704330671644414, 274.9349708856848338, -13.01557521325596944 ) ) ;
#26956 = AXIS2_PLACEMENT_3D ( 'NONE', #44463, #75395, #5978 ) ;
#26955 = CARTESIAN_POINT ( 'NONE',  ( 192.2321494539393996, 293.0484659149655045, -14.31527305258243743 ) ) ;
#26957 = CARTESIAN_POINT ( 'NONE',  ( 190.9498149295421570, 299.9122141765958531, -5.138500224925297566 ) ) ;
#26958 = CARTESIAN_POINT ( 'NONE',  ( 73.81127463411883127, 55.52226492712755856, -16.58648971016070561 ) ) ;
#26960 = CARTESIAN_POINT ( 'NONE',  ( 71.30684095964828373, 218.6427522451419065, 10.00000000000009237 ) ) ;
#26959 = DIRECTION ( 'NONE',  ( 0.000000000000000000, 0.000000000000000000, 1.000000000000000000 ) ) ;
#26961 = CARTESIAN_POINT ( 'NONE',  ( 74.61640982031720171, 67.04502654152244645, 12.50436240261666576 ) ) ;
#26962 = ADVANCED_FACE ( 'NONE', ( #59757 ), #68361, .T. ) ;
#26963 = LINE ( 'NONE', #99233, #96780 ) ;
#26964 = CARTESIAN_POINT ( 'NONE',  ( -110.0000000000000000, 0.000000000000000000, 59.99999999999999289 ) ) ;
#26965 = CIRCLE ( 'NONE', #62510, 2.471954595299370006 ) ;
#26966 = EDGE_CURVE ( 'NONE', #27863, #35723, #46544, .T. ) ;
#26967 = CARTESIAN_POINT ( 'NONE',  ( 179.1629783499468260, 294.4842721394058458, 1.069721132174473288 ) ) ;
#26968 = CARTESIAN_POINT ( 'NONE',  ( 40.86965645935567437, 187.7365022471901739, -10.00000000000009059 ) ) ;
#26969 = PLANE ( 'NONE',  #73359 ) ;
#26970 = CARTESIAN_POINT ( 'NONE',  ( 203.0337691736598629, 278.9821914694464340, 16.08167820133810011 ) ) ;
#26971 = CARTESIAN_POINT ( 'NONE',  ( -5.399728507075681527, 173.8149278399160949, -9.188101187500095079 ) ) ;
#26972 = CARTESIAN_POINT ( 'NONE',  ( 33.27084535048209091, 40.18502408145594273, 5.678558825948277544 ) ) ;
#26973 = CARTESIAN_POINT ( 'NONE',  ( 163.2659639011634169, 252.2459686854220422, 13.11545999390232353 ) ) ;
#26974 = CARTESIAN_POINT ( 'NONE',  ( 153.3703256797887775, 265.0017988796566897, 16.44314709207578318 ) ) ;
#26975 = CARTESIAN_POINT ( 'NONE',  ( 39.09967052555147404, 28.28920272979929962, -7.433330006724141015 ) ) ;
#26976 = CARTESIAN_POINT ( 'NONE',  ( 164.9103019330012216, 245.0139736909548560, 2.841678961959298810 ) ) ;
#26977 = CARTESIAN_POINT ( 'NONE',  ( 183.3303171387637747, 279.0281335762378490, 17.06007825884248064 ) ) ;
#26978 = DIRECTION ( 'NONE',  ( 0.000000000000000000, -1.000000000000000000, 0.000000000000000000 ) ) ;
#26979 = CARTESIAN_POINT ( 'NONE',  ( 70.67536410627006660, 211.6115022471902591, 10.00000000000009592 ) ) ;
#26980 = CARTESIAN_POINT ( 'NONE',  ( 146.4729408656479563, 243.8262482093457493, 3.021315404115420679E-15 ) ) ;
#26981 = CARTESIAN_POINT ( 'NONE',  ( 14.52619969316804394, 14.10170272979925699, -7.433330006724141015 ) ) ;
#26982 = CARTESIAN_POINT ( 'NONE',  ( 165.6069501779841460, 285.3987855451247810, 0.3448102065264236904 ) ) ;
#26983 = CARTESIAN_POINT ( 'NONE',  ( 14.21828646722447154, 29.18502408145591431, 5.678558825948276656 ) ) ;
#26984 = CARTESIAN_POINT ( 'NONE',  ( 181.8129518053731033, 270.5384970965435514, -17.23398818032472946 ) ) ;
#26985 = VECTOR ( 'NONE', #33044, 1000.000000000000000 ) ;
#26986 = CARTESIAN_POINT ( 'NONE',  ( 154.8679462054080318, 262.4078440388265676, 17.98338675682672871 ) ) ;
#26987 = VERTEX_POINT ( 'NONE', #84122 ) ;
#26988 = CARTESIAN_POINT ( 'NONE',  ( 25.88782454542109335, 20.11029122506295153, -8.090169943749478065 ) ) ;
#26989 = CARTESIAN_POINT ( 'NONE',  ( 47.39496755818312579, 108.2889530649357681, 10.00000000000000000 ) ) ;
#26990 = ORIENTED_EDGE ( 'NONE', *, *, #39507, .T. ) ;
#26991 = CARTESIAN_POINT ( 'NONE',  ( 153.4578721839791342, 264.8501638863745029, 16.85421393845643223 ) ) ;
#26992 = CARTESIAN_POINT ( 'NONE',  ( 164.2600772519394923, 246.1401958748887182, -2.110785484364219311 ) ) ;
#26993 = VECTOR ( 'NONE', #8202, 1000.000000000000114 ) ;
#26994 = CARTESIAN_POINT ( 'NONE',  ( 66.21641665491797824, 68.54611642907939029, 4.779534852452537841 ) ) ;
#26995 = CARTESIAN_POINT ( 'NONE',  ( 125.8043565786058906, 231.8932355074535394, -2.679491924311248496 ) ) ;
#26996 = ORIENTED_EDGE ( 'NONE', *, *, #88908, .F. ) ;
#26997 = EDGE_LOOP ( 'NONE', ( #43941, #86854, #48698, #94936 ) ) ;
#26998 = EDGE_CURVE ( 'NONE', #48579, #20542, #68855, .T. ) ;
#27000 = CARTESIAN_POINT ( 'NONE',  ( 164.2413944571582078, 246.1725554246774834, 7.304616466633322425 ) ) ;
#26999 = CARTESIAN_POINT ( 'NONE',  ( -19.65312891409030271, 93.06504152958497400, -10.00000000000000888 ) ) ;
#27001 = CARTESIAN_POINT ( 'NONE',  ( 85.94067892034982492, 47.59093751143262807, 10.86761488427001687 ) ) ;
#27002 = ORIENTED_EDGE ( 'NONE', *, *, #39709, .T. ) ;
#27003 = CARTESIAN_POINT ( 'NONE',  ( 77.27978102768229007, 55.00308727795876962, 16.10417966147982582 ) ) ;
#27004 = CARTESIAN_POINT ( 'NONE',  ( 177.1347673595945764, 262.9921672455169528, 15.53478677465993485 ) ) ;
#27005 = ORIENTED_EDGE ( 'NONE', *, *, #47231, .F. ) ;
#27006 = CARTESIAN_POINT ( 'NONE',  ( 77.08943580299947484, 49.61595851769168064, 15.51385818994994459 ) ) ;
#27007 = CARTESIAN_POINT ( 'NONE',  ( 79.50011211534433642, 50.05647880806598948, -14.69180297385495670 ) ) ;
#27008 = ADVANCED_FACE ( 'NONE', ( #30369 ), #61252, .T. ) ;
#27009 = EDGE_CURVE ( 'NONE', #18914, #90330, #53183, .T. ) ;
#27010 = B_SPLINE_CURVE_WITH_KNOTS ( 'NONE', 3,
 ( #94960, #89853, #66017, #96966, #13327, #82761, #27532, #89376, #59381, #37099, #36097, #29022, #19931, #90357, #66998, #58403, #27028, #20938, #74642, #52298, #13804, #50804 ),
 .UNSPECIFIED., .F., .F.,
 ( 4, 2, 2, 2, 2, 2, 2, 2, 2, 2, 4 ),
 ( 0.0003198756514526470991, 0.002147329819704916695, 0.002604193361768018626, 0.002661301304525904091, 0.002689855275904812562, 0.002718409247283721034, 0.002832625132799350583, 0.003061056903830601007, 0.003289488674861852299, 0.003517920445893102724, 0.003974783987955634798 ),
 .UNSPECIFIED. ) ;
#27011 = CARTESIAN_POINT ( 'NONE',  ( 80.98820082504030893, 43.58192978494404457, 9.409748623455859828 ) ) ;
#27012 = ORIENTED_EDGE ( 'NONE', *, *, #33619, .T. ) ;
#27013 = CARTESIAN_POINT ( 'NONE',  ( 161.7910648966377209, 250.4166507187868831, 13.19274492748169436 ) ) ;
#27014 = CARTESIAN_POINT ( 'NONE',  ( 166.1007185193450937, 274.1064974184767493, -15.20043799348013458 ) ) ;
#27015 = LINE ( 'NONE', #27520, #46114 ) ;
#27016 = ORIENTED_EDGE ( 'NONE', *, *, #351, .T. ) ;
#27017 = EDGE_CURVE ( 'NONE', #71681, #441, #24844, .T. ) ;
#27018 = CARTESIAN_POINT ( 'NONE',  ( 190.0340467409721441, 301.4983712071542641, 4.077645795029533282 ) ) ;
#27019 = CARTESIAN_POINT ( 'NONE',  ( 41.98277471387834225, 25.20801979619931998, -3.090169943749474069 ) ) ;
#27020 = EDGE_CURVE ( 'NONE', #34033, #81073, #15671, .T. ) ;
#27021 = ORIENTED_EDGE ( 'NONE', *, *, #63629, .T. ) ;
#27022 = CARTESIAN_POINT ( 'NONE',  ( 157.3910266414278851, 266.9754241737259122, -16.20060215746766374 ) ) ;
#27023 = EDGE_LOOP ( 'NONE', ( #31100, #98959, #58026, #9315, #64638 ) ) ;
#27024 = LINE ( 'NONE', #50305, #75179 ) ;
#27025 = VERTEX_POINT ( 'NONE', #7579 ) ;
#27026 = CARTESIAN_POINT ( 'NONE',  ( 159.1685125254583966, 259.5000883001122247, 16.69271994272259008 ) ) ;
#27027 = CARTESIAN_POINT ( 'NONE',  ( 193.8257114866206905, 294.9310152224236390, 14.87231647135867796 ) ) ;
#27028 = CARTESIAN_POINT ( 'NONE',  ( 188.5854780552674868, 298.6315526637507105, -4.814084629927046777 ) ) ;
#27029 = DIRECTION ( 'NONE',  ( -0.000000000000000000, -0.000000000000000000, -1.000000000000000000 ) ) ;
#27030 = CARTESIAN_POINT ( 'NONE',  ( 200.2629047362840424, 281.3048619616022279, -17.25979275631262055 ) ) ;
#27031 = CARTESIAN_POINT ( 'NONE',  ( 86.38422984226583878, 43.10374499244417024, 0.3565776162481382738 ) ) ;
#27032 = CARTESIAN_POINT ( 'NONE',  ( 158.4167541826878391, 256.2611283158722699, -16.34182606312789687 ) ) ;
#27033 = VERTEX_POINT ( 'NONE', #6595 ) ;
#27034 = DIRECTION ( 'NONE',  ( 0.8660254037844378194, 0.5000000000000015543, -0.000000000000000000 ) ) ;
#27035 = CARTESIAN_POINT ( 'NONE',  ( 23.41017057962146097, 28.91421378149919619, 9.188101187500008038 ) ) ;
#27036 = VECTOR ( 'NONE', #48998, 1000.000000000000000 ) ;
#27037 = CARTESIAN_POINT ( 'NONE',  ( 206.4537138826727301, 273.0586734743599209, 11.45643784582899016 ) ) ;
#27039 = CARTESIAN_POINT ( 'NONE',  ( 164.9103019330012216, 245.0139736909548560, 2.841678961959298810 ) ) ;
#27038 = CARTESIAN_POINT ( 'NONE',  ( 164.3036517873781008, 252.3706336020835579, 13.60069832213670082 ) ) ;
#27041 = ORIENTED_EDGE ( 'NONE', *, *, #9324, .F. ) ;
#27040 = CARTESIAN_POINT ( 'NONE',  ( 198.5612432604688991, 286.7288335892616260, 18.30793681285053509 ) ) ;
#27042 = VECTOR ( 'NONE', #42923, 1000.000000000000114 ) ;
#27043 = ORIENTED_EDGE ( 'NONE', *, *, #17582, .T. ) ;
#27044 = CARTESIAN_POINT ( 'NONE',  ( 187.3665724429023101, 277.0083082519628306, 16.89536893287339225 ) ) ;
#27045 = CARTESIAN_POINT ( 'NONE',  ( 38.67678797688638070, 22.73415679381825072, -6.890680421881970419E-14 ) ) ;
#27046 = LINE ( 'NONE', #42221, #90053 ) ;
#27047 = CARTESIAN_POINT ( 'NONE',  ( 10.05297690690921897, 28.73705186507752529, -3.090169943749475845 ) ) ;
#27048 = CARTESIAN_POINT ( 'NONE',  ( 199.0022468604825292, 285.9649929477169508, -18.62203328612563169 ) ) ;
#27049 = CARTESIAN_POINT ( 'NONE',  ( 148.4975630032294021, 273.4416714086831917, -10.35571102360928464 ) ) ;
#27050 = ORIENTED_EDGE ( 'NONE', *, *, #91613, .T. ) ;
#27051 = CARTESIAN_POINT ( 'NONE',  ( 167.5508029243457599, 252.8355245762918173, -12.42550861741178991 ) ) ;
#27052 = DIRECTION ( 'NONE',  ( -1.000000000000000000, 0.000000000000000000, 0.000000000000000000 ) ) ;
#27053 = DIRECTION ( 'NONE',  ( 0.000000000000000000, -1.000000000000000000, 1.065403912962273439E-14 ) ) ;
#27055 = ADVANCED_FACE ( 'NONE', ( #46565 ), #76017, .F. ) ;
#27054 = PLANE ( 'NONE',  #72677 ) ;
#27056 = CARTESIAN_POINT ( 'NONE',  ( 35.43895548624285396, 181.2677522451417929, -5.000000000000041744 ) ) ;
#27057 = CARTESIAN_POINT ( 'NONE',  ( 98.19890751640281223, 221.3768266524159856, -9.188101187500093303 ) ) ;
#27058 = CARTESIAN_POINT ( 'NONE',  ( 82.55891087508022963, 41.03829285859550424, -1.155036376835396839 ) ) ;
#27059 = CARTESIAN_POINT ( 'NONE',  ( 167.4021843883327278, 282.9460231506713512, -10.86961029474059259 ) ) ;
#27060 = DIRECTION ( 'NONE',  ( -0.000000000000000000, -0.000000000000000000, 1.000000000000000000 ) ) ;
#27061 = CARTESIAN_POINT ( 'NONE',  ( 162.4279131726858623, 249.3135971479585464, 10.85034575916916921 ) ) ;
#27062 = CARTESIAN_POINT ( 'NONE',  ( 17.65854496445001232, 174.8768266524159856, -9.188101187500091527 ) ) ;
#27063 = DIRECTION ( 'NONE',  ( 0.5000000000000005551, -0.8660254037844384856, 0.000000000000000000 ) ) ;
#27064 = ORIENTED_EDGE ( 'NONE', *, *, #19726, .T. ) ;
#27065 = VECTOR ( 'NONE', #10065, 1000.000000000000114 ) ;
#27066 = ORIENTED_EDGE ( 'NONE', *, *, #51502, .F. ) ;
#27067 = CARTESIAN_POINT ( 'NONE',  ( 147.7840609055601817, 276.6774932931532476, -0.9735537997635442808 ) ) ;
#27068 = CARTESIAN_POINT ( 'NONE',  ( 71.96766164200448657, 71.97375519272833344, -2.838622940868376077 ) ) ;
#27069 = CARTESIAN_POINT ( 'NONE',  ( 147.0670278774466908, 275.9194309285509235, 3.666898409139099257 ) ) ;
#27070 = CARTESIAN_POINT ( 'NONE',  ( 193.6564271169084464, 262.6014873983580742, -4.146719891036213745 ) ) ;
#27071 = DIRECTION ( 'NONE',  ( 0.9839629614562466209, -0.1783728972749306640, 0.000000000000000000 ) ) ;
#27072 = DIRECTION ( 'NONE',  ( 0.000000000000000000, 0.000000000000000000, 1.000000000000000000 ) ) ;
#27073 = CARTESIAN_POINT ( 'NONE',  ( 74.22912425478418186, 67.87594522781263606, -11.68556788600236374 ) ) ;
#27074 = VECTOR ( 'NONE', #23438, 1000.000000000000000 ) ;
#27075 = CARTESIAN_POINT ( 'NONE',  ( 46.72434903108273119, 197.7833772461660828, -9.188101187500095079 ) ) ;
#27076 = CARTESIAN_POINT ( 'NONE',  ( 86.02927282398376008, 227.1427522451419634, -10.00000000000009415 ) ) ;
#27077 = VERTEX_POINT ( 'NONE', #37469 ) ;
#27078 = CARTESIAN_POINT ( 'NONE',  ( 79.22574914704958360, 60.04803162267379690, -16.48148452078546100 ) ) ;
#27079 = B_SPLINE_CURVE_WITH_KNOTS ( 'NONE', 3,
 ( #8912, #61604, #69709, #86983 ),
 .UNSPECIFIED., .F., .F.,
 ( 4, 4 ),
 ( 0.03082140243953887179, 0.03988153003689407644 ),
 .UNSPECIFIED. ) ;
#27080 = EDGE_CURVE ( 'NONE', #38416, #24759, #99304, .T. ) ;
#27081 = CARTESIAN_POINT ( 'NONE',  ( 181.2305897479128305, 260.5010089447542896, -10.41488471035008168 ) ) ;
#27082 = CARTESIAN_POINT ( 'NONE',  ( -0.5554856785977280165, 179.6744531367911577, 4.594050593750047540 ) ) ;
#27083 = DIRECTION ( 'NONE',  ( 3.817860598523670672E-18, 1.090355031989287297E-16, 1.000000000000000000 ) ) ;
#27084 = CARTESIAN_POINT ( 'NONE',  ( 179.3484626673140383, 285.2557201243848795, -15.12459571388282420 ) ) ;
#27085 = CARTESIAN_POINT ( 'NONE',  ( 79.11036565982459479, 46.22622971652937451, -12.75658226733973066 ) ) ;
#27086 = CARTESIAN_POINT ( 'NONE',  ( 146.8868584395697781, 276.2314935489248455, -3.891417269505058396 ) ) ;
#27087 = CARTESIAN_POINT ( 'NONE',  ( 74.81832046901196520, 67.48663194201290594, -12.71244991431774984 ) ) ;
#27088 = CARTESIAN_POINT ( 'NONE',  ( 180.8890834033174713, 294.3766012452771861, 6.559837412958372305 ) ) ;
#27089 = ADVANCED_FACE ( 'NONE', ( #53666 ), #10084, .F. ) ;
#27090 = CARTESIAN_POINT ( 'NONE',  ( -32.85588310213878316, 95.75574514201873910, 44.05931881766424141 ) ) ;
#27091 = CARTESIAN_POINT ( 'NONE',  ( 164.9586510554008782, 244.9302305544571823, -1.717556444319656039 ) ) ;
#27092 = ORIENTED_EDGE ( 'NONE', *, *, #47470, .T. ) ;
#27093 = ADVANCED_FACE ( 'NONE', ( #94716 ), #30047, .T. ) ;
#27094 = ADVANCED_FACE ( 'NONE', ( #49088 ), #25431, .F. ) ;
#27095 = CARTESIAN_POINT ( 'NONE',  ( -0.8439004895947717078, 156.9865022471901455, 1.119607411625061291E-15 ) ) ;
#27096 = DIRECTION ( 'NONE',  ( -0.2551196190400349950, -0.9669094993746143452, 0.000000000000000000 ) ) ;
#27097 = CARTESIAN_POINT ( 'NONE',  ( 126.2364799639240260, 237.5643266524160140, 9.188101187500095079 ) ) ;
#27098 = CARTESIAN_POINT ( 'NONE',  ( 16.11390655273756778, 24.70171378149918340, -9.188101187500004485 ) ) ;
#27099 = CARTESIAN_POINT ( 'NONE',  ( 78.70378768487077537, 58.88177420653629213, -16.56922034439224234 ) ) ;
#27100 = CARTESIAN_POINT ( 'NONE',  ( -22.42236680055709641, 157.8615022471902591, 0.000000000000000000 ) ) ;
#27102 = CARTESIAN_POINT ( 'NONE',  ( 168.0462690533684338, 251.4142709888886884, 10.74789308012043954 ) ) ;
#27101 = CARTESIAN_POINT ( 'NONE',  ( 196.4390255720217908, 290.4046224503736653, 16.34739044515864848 ) ) ;
#27103 = CARTESIAN_POINT ( 'NONE',  ( 150.3471325113991952, 270.2381230484028833, -13.97988400279308330 ) ) ;
#27104 = ORIENTED_EDGE ( 'NONE', *, *, #80179, .T. ) ;
#27105 = CARTESIAN_POINT ( 'NONE',  ( 190.7851751463332164, 300.1973786460605425, 8.237717828100052486 ) ) ;
#27106 = CARTESIAN_POINT ( 'NONE',  ( 163.3471839416382352, 247.7213734702205841, 8.361547422486792058 ) ) ;
#27107 = VECTOR ( 'NONE', #43597, 1000.000000000000114 ) ;
#27108 = CARTESIAN_POINT ( 'NONE',  ( 159.6023402823087451, 258.6676503891110883, 17.43025742997651761 ) ) ;
#27109 = CARTESIAN_POINT ( 'NONE',  ( 171.1200255626874593, 267.0209532845146896, -16.45006463731995083 ) ) ;
#27110 = CARTESIAN_POINT ( 'NONE',  ( 81.44281134420617718, 55.17415802334473085, -15.93029283586374412 ) ) ;
#27111 = ORIENTED_EDGE ( 'NONE', *, *, #100167, .F. ) ;
#27112 = CARTESIAN_POINT ( 'NONE',  ( 69.24454181484452420, 67.43800925919231304, 8.968860985737871161 ) ) ;
#27113 = AXIS2_PLACEMENT_3D ( 'NONE', #89922, #40400, #9018 ) ;
#27114 = CARTESIAN_POINT ( 'NONE',  ( 165.5977178541590149, 269.2419187492577635, -16.64600468838175473 ) ) ;
#27115 = B_SPLINE_SURFACE_WITH_KNOTS ( 'NONE', 3, 1, ( 
 ( #36954, #68846 ),
 ( #54130, #53641 ),
 ( #37441, #68351 ),
 ( #29859, #60729 ),
 ( #69354, #100273 ),
 ( #7052, #30358 ),
 ( #30858, #53156 ),
 ( #91691, #76472 ),
 ( #22254, #84112 ),
 ( #14664, #45540 ),
 ( #46031, #46536 ),
 ( #37933, #75475 ),
 ( #98787, #99767 ),
 ( #8067, #61243 ),
 ( #92209, #22764 ),
 ( #77473, #7548 ),
 ( #61743, #15134 ),
 ( #92692, #21756 ),
 ( #38942, #98283 ),
 ( #83598, #28871 ),
 ( #59747, #60235 ),
 ( #21273, #52150 ),
 ( #83099, #44542 ),
 ( #6060, #67865 ),
 ( #29369, #91196 ),
 ( #18164, #54634 ),
 ( #70349, #93185 ),
 ( #78474, #55631 ),
 ( #1964, #8563 ),
 ( #77968, #48563 ),
 ( #32849, #23740 ),
 ( #71877, #40930 ),
 ( #31837, #460 ),
 ( #71375, #16652 ) ),
 .UNSPECIFIED., .T., .F., .F.,
 ( 4, 2, 2, 2, 2, 2, 2, 2, 2, 2, 2, 2, 2, 2, 2, 2, 4 ),
 ( 2, 2 ),
 ( 0.000000000000000000, 0.06250000000000000000, 0.1250000000000000000, 0.1875000000000000000, 0.2500000000000000000, 0.3125000000000000000, 0.3750000000000000000, 0.4375000000000000000, 0.5000000000000000000, 0.5625000000000000000, 0.6250000000000000000, 0.6875000000000000000, 0.7500000000000000000, 0.8125000000000000000, 0.8750000000000000000, 0.9375000000000000000, 1.000000000000000000 ),
 ( 0.000000000000000000, 1.000000000000000000 ),
 .UNSPECIFIED. ) ;
#27116 = CARTESIAN_POINT ( 'NONE',  ( 83.96855558776917405, 42.91945120030306526, 5.578457850387072980 ) ) ;
#27117 = CARTESIAN_POINT ( 'NONE',  ( 79.54380123660683921, 51.49935735363682454, 15.19165240974427000 ) ) ;
#27118 = CARTESIAN_POINT ( 'NONE',  ( 185.7140529529728497, 297.0115757928315361, 5.550365566574654963 ) ) ;
#27119 = PLANE ( 'NONE',  #30732 ) ;
#27120 = CARTESIAN_POINT ( 'NONE',  ( 149.6056361282314811, 276.8836032498194868, -0.0001402111935095534635 ) ) ;
#27121 = AXIS2_PLACEMENT_3D ( 'NONE', #91630, #30297, #84048 ) ;
#27122 =( BOUNDED_CURVE ( )  B_SPLINE_CURVE ( 2, ( #86964, #49900, #3811, #96541, #94535, #55476, #86462, #16987, #71219 ),
 .UNSPECIFIED., .F., .T. ) 
 B_SPLINE_CURVE_WITH_KNOTS ( ( 3, 2, 2, 2, 3 ),
 ( 0.9153225806451612545, 0.9166666666666666297, 0.9193548387096773800, 0.9220430107526881303, 0.9233870967741935054 ),
 .UNSPECIFIED. ) 
 CURVE ( )  GEOMETRIC_REPRESENTATION_ITEM ( )  RATIONAL_B_SPLINE_CURVE ( ( 0.9330127018922194093, 0.9330127018922194093, 1.000000000000000000, 0.8660254037844387076, 1.000000000000000000, 0.8660254037844387076, 1.000000000000000000, 0.9330127018922194093, 0.9330127018922194093 ) ) 
 REPRESENTATION_ITEM ( '' )  );
#27123 = ADVANCED_FACE ( 'NONE', ( #66280 ), #27287, .F. ) ;
#27124 = CARTESIAN_POINT ( 'NONE',  ( 194.4430534426562076, 282.9522031543310732, 17.75811852729254881 ) ) ;
#27125 = CARTESIAN_POINT ( 'NONE',  ( 5.867642952189433103, 25.16126292948893450, -6.180339887498951690 ) ) ;
#27126 = CARTESIAN_POINT ( 'NONE',  ( 173.8384530544828408, 272.7721218975195825, -16.35919102464103148 ) ) ;
#27127 = VERTEX_POINT ( 'NONE', #27782 ) ;
#27128 = CARTESIAN_POINT ( 'NONE',  ( 162.4683961769543146, 253.1913979656618778, 14.82777648277118310 ) ) ;
#27129 = CARTESIAN_POINT ( 'NONE',  ( 194.2154056360670040, 294.2560451561701029, -15.66696967429384557 ) ) ;
#27130 = DIRECTION ( 'NONE',  ( -0.9413434404457866611, 0.3374500364938339270, 0.000000000000000000 ) ) ;
#27131 = ORIENTED_EDGE ( 'NONE', *, *, #89441, .T. ) ;
#27132 = DIRECTION ( 'NONE',  ( 0.4999999999999998890, -0.8660254037844385966, 0.000000000000000000 ) ) ;
#27133 = CARTESIAN_POINT ( 'NONE',  ( -27.42236680055714260, 166.5217562850347406, 1.224646799147364892E-15 ) ) ;
#27134 = DIRECTION ( 'NONE',  ( -0.8806841296921844586, 0.4737039832092607705, 0.000000000000000000 ) ) ;
#27135 = ORIENTED_EDGE ( 'NONE', *, *, #49370, .F. ) ;
#27136 = CARTESIAN_POINT ( 'NONE',  ( 84.66726058227095564, 213.5643266524159856, 9.188101187500095079 ) ) ;
#27137 = CARTESIAN_POINT ( 'NONE',  ( 82.49529963037764446, 50.53747482938361202, -14.21121686865391354 ) ) ;
#27138 = CARTESIAN_POINT ( 'NONE',  ( 188.6826127332440421, 272.6057162039079458, 16.71479996418005243 ) ) ;
#27139 = CARTESIAN_POINT ( 'NONE',  ( 182.2345731410963197, 257.9208214993698220, -5.932519869942172619 ) ) ;
#27140 = VERTEX_POINT ( 'NONE', #34862 ) ;
#27141 = VERTEX_POINT ( 'NONE', #58656 ) ;
#27142 = DIRECTION ( 'NONE',  ( -0.5632146860273895550, 0.8263106059122495850, 0.000000000000000000 ) ) ;
#27143 = ORIENTED_EDGE ( 'NONE', *, *, #38385, .T. ) ;
#27144 = CARTESIAN_POINT ( 'NONE',  ( 84.99999999999997158, 27.49999999999999645, 59.99999999999999289 ) ) ;
#27145 = ORIENTED_EDGE ( 'NONE', *, *, #3015, .T. ) ;
#27146 = CARTESIAN_POINT ( 'NONE',  ( 206.8711744556208885, 269.6661967102621702, -5.660351959544826712E-12 ) ) ;
#27147 = CARTESIAN_POINT ( 'NONE',  ( 154.9067123643522734, 262.3406990819208886, -18.18534662427576265 ) ) ;
#27148 = ORIENTED_EDGE ( 'NONE', *, *, #51860, .F. ) ;
#27149 = CARTESIAN_POINT ( 'NONE',  ( 164.3614934205162399, 245.9645379182051101, 2.163927203393636312 ) ) ;
#27150 = CARTESIAN_POINT ( 'NONE',  ( 82.15942678738257143, 40.67362617692227644, 3.631441412251192880 ) ) ;
#27151 = CARTESIAN_POINT ( 'NONE',  ( 151.5945656433808324, 268.6161677518811075, 14.58547821675770351 ) ) ;
#27152 = CARTESIAN_POINT ( 'NONE',  ( 162.0103126358019097, 277.3769015859130604, -12.92703519490087594 ) ) ;
#27153 = CARTESIAN_POINT ( 'NONE',  ( 153.4542976351440302, 264.8563551865710224, -17.11782692037292009 ) ) ;
#27154 = CARTESIAN_POINT ( 'NONE',  ( 182.4502886106904214, 259.6876753163259650, 10.69873880494191631 ) ) ;
#27155 = DIRECTION ( 'NONE',  ( 0.000000000000000000, 0.000000000000000000, 1.000000000000000000 ) ) ;
#27156 = CARTESIAN_POINT ( 'NONE',  ( 132.6770232609233062, 259.6589784336661637, -6.496448406907675876E-16 ) ) ;
#27157 = CARTESIAN_POINT ( 'NONE',  ( 70.57887313579936972, 60.86954541810593611, -14.49646675233496218 ) ) ;
#27158 = CARTESIAN_POINT ( 'NONE',  ( 9.248262631489305718, 13.84335787977760823, 9.188101187500006262 ) ) ;
#27159 = EDGE_CURVE ( 'NONE', #82839, #51615, #35868, .T. ) ;
#27160 = ORIENTED_EDGE ( 'NONE', *, *, #95627, .T. ) ;
#27162 = ORIENTED_EDGE ( 'NONE', *, *, #22340, .F. ) ;
#27161 = CARTESIAN_POINT ( 'NONE',  ( 199.9021804882490017, 270.2741479731562322, 9.563714619189552124 ) ) ;
#27163 = CARTESIAN_POINT ( 'NONE',  ( -5.122212653107841795, 179.3967562850347406, 2.649461200531984646E-14 ) ) ;
#27164 = CARTESIAN_POINT ( 'NONE',  ( 78.21652899302088713, 47.47575335428597043, -13.80965570268340414 ) ) ;
#27165 = CARTESIAN_POINT ( 'NONE',  ( 76.08212860749918605, 65.40353610076411428, -14.00331547028825518 ) ) ;
#27166 = CARTESIAN_POINT ( 'NONE',  ( 154.5051885171875483, 277.5048442334672245, 7.163368614392425116 ) ) ;
#27167 = CARTESIAN_POINT ( 'NONE',  ( 165.3147752961083938, 246.7756614015693231, -1.872181691986823271 ) ) ;
#27168 = CARTESIAN_POINT ( 'NONE',  ( 192.6435868206044972, 292.3535262516610373, -14.36478698284807365 ) ) ;
#27169 = CARTESIAN_POINT ( 'NONE',  ( 85.98998294167898848, 43.32359931212324966, 3.421509554684789567 ) ) ;
#27170 = CARTESIAN_POINT ( 'NONE',  ( 88.30125181426937786, 44.32158129576059480, -2.141221342158480923 ) ) ;
#27171 = VERTEX_POINT ( 'NONE', #89629 ) ;
#27172 = CARTESIAN_POINT ( 'NONE',  ( -19.77595115955931249, 92.99413007310096191, 59.99999999999999289 ) ) ;
#27173 = CARTESIAN_POINT ( 'NONE',  ( 66.16284130609386693, 69.32471991931953426, 0.2281878490819576055 ) ) ;
#27174 = VERTEX_POINT ( 'NONE', #34379 ) ;
#27175 = CIRCLE ( 'NONE', #78964, 45.00000000000000000 ) ;
#27176 = CARTESIAN_POINT ( 'NONE',  ( 164.0069374096083550, 277.9889559920678153, 13.17848772514222411 ) ) ;
#27177 = CARTESIAN_POINT ( 'NONE',  ( 156.7704915376250767, 276.6929587230139873, 10.09098372363049201 ) ) ;
#27178 = CARTESIAN_POINT ( 'NONE',  ( 203.7728381401813920, 277.7020864691337465, -14.30591445410113494 ) ) ;
#27179 = CARTESIAN_POINT ( 'NONE',  ( 149.1903793729515257, 272.2416782560088677, 12.95958987445043675 ) ) ;
#27180 = CIRCLE ( 'NONE', #69162, 70.00000000000001421 ) ;
#27181 = CARTESIAN_POINT ( 'NONE',  ( 163.5827852761539987, 273.8567145120941291, 14.80360896856500119 ) ) ;
#27183 = CARTESIAN_POINT ( 'NONE',  ( 88.18822050095108978, 44.34076438004694154, 2.673349022503985761 ) ) ;
#27182 = CARTESIAN_POINT ( 'NONE',  ( 47.22349865033175575, 113.7415181542323097, -10.00000000000000000 ) ) ;
#27184 = CARTESIAN_POINT ( 'NONE',  ( 66.61587002248265321, 199.2677522451418213, -5.000000000000041744 ) ) ;
#27185 = ORIENTED_EDGE ( 'NONE', *, *, #223, .F. ) ;
#27186 = VECTOR ( 'NONE', #11053, 1000.000000000000114 ) ;
#27187 = CARTESIAN_POINT ( 'NONE',  ( 77.19709256177225143, 60.73830195696542233, -15.79962378659312883 ) ) ;
#27188 = CARTESIAN_POINT ( 'NONE',  ( 79.85233299459939360, 57.97614157916506628, 16.26679898004111990 ) ) ;
#27189 = CARTESIAN_POINT ( 'NONE',  ( 71.25744581038296133, 66.03388063194447000, -11.67341175673348630 ) ) ;
#27190 = CARTESIAN_POINT ( 'NONE',  ( 192.2943420783192323, 297.5834248427583475, 12.53393473147773562 ) ) ;
#27191 = AXIS2_PLACEMENT_3D ( 'NONE', #67808, #59174, #51609 ) ;
#27192 = CARTESIAN_POINT ( 'NONE',  ( 80.63212551389750615, 43.28576471723870611, -9.304653108355022795 ) ) ;
#27193 = LINE ( 'NONE', #65181, #62793 ) ;
#27194 = CARTESIAN_POINT ( 'NONE',  ( 16.49491010205593255, 171.1423013555409796, -4.594050593750043987 ) ) ;
#27195 = CARTESIAN_POINT ( 'NONE',  ( 97.06207562605321471, 226.8458772461660544, 9.188101187500095079 ) ) ;
#27196 = CARTESIAN_POINT ( 'NONE',  ( 154.9903553346911735, 262.1958252075976361, -18.39016733948542637 ) ) ;
#27197 = CARTESIAN_POINT ( 'NONE',  ( 87.76333951327919181, 44.16327574611633366, -4.502641440754712399 ) ) ;
#27198 = CARTESIAN_POINT ( 'NONE',  ( 186.2747105596910444, 296.7709437567457940, -7.332267729565418612 ) ) ;
#27199 = CARTESIAN_POINT ( 'NONE',  ( 77.61491115650760264, 49.94450177510211830, 15.01392251353181528 ) ) ;
#27200 = AXIS2_PLACEMENT_3D ( 'NONE', #97403, #83206, #45162 ) ;
#27201 = CARTESIAN_POINT ( 'NONE',  ( 77.26541432047375224, 51.19878943637716873, 15.46470134853914047 ) ) ;
#27202 = DIRECTION ( 'NONE',  ( -0.8660254037844387076, -0.4999999999999998890, -0.000000000000000000 ) ) ;
#27203 = CARTESIAN_POINT ( 'NONE',  ( 148.0826818691893152, 274.1602666119424043, -9.371267383421741926 ) ) ;
#27204 = DIRECTION ( 'NONE',  ( 1.000000000000000000, 0.000000000000000000, 0.000000000000000000 ) ) ;
#27205 = CARTESIAN_POINT ( 'NONE',  ( 84.81139823732658556, 50.24252652397250785, 13.36660589061055404 ) ) ;
#27206 = EDGE_CURVE ( 'NONE', #16059, #38622, #88644, .T. ) ;
#27207 = CARTESIAN_POINT ( 'NONE',  ( 79.33432753241152113, 54.60848390438605549, -15.97798455793337347 ) ) ;
#27208 = CARTESIAN_POINT ( 'NONE',  ( 82.12925965045128862, 52.94868272234815265, -15.66193675175870226 ) ) ;
#27209 = CARTESIAN_POINT ( 'NONE',  ( 88.77168660263453148, 215.3927522451417929, -10.00000000000009237 ) ) ;
#27210 = EDGE_CURVE ( 'NONE', #79692, #48169, #20685, .T. ) ;
#27211 = CIRCLE ( 'NONE', #72569, 50.00000000000000711 ) ;
#27213 = EDGE_CURVE ( 'NONE', #79909, #8078, #66770, .T. ) ;
#27212 = CARTESIAN_POINT ( 'NONE',  ( 173.7468028372802564, 264.4725572781864003, -15.47520981000551465 ) ) ;
#27214 = ADVANCED_FACE ( 'NONE', ( #5478 ), #18691, .F. ) ;
#27215 = CARTESIAN_POINT ( 'NONE',  ( 87.26533679362427165, 215.0643266524160140, 9.188101187500095079 ) ) ;
#27216 = CARTESIAN_POINT ( 'NONE',  ( 207.1007598919583472, 271.9379569114424271, -6.086525981869248092 ) ) ;
#27217 = DIRECTION ( 'NONE',  ( 0.000000000000000000, 0.000000000000000000, 1.000000000000000000 ) ) ;
#27218 = CYLINDRICAL_SURFACE ( 'NONE', #96744, 17.82106496071139645 ) ;
#27220 = CARTESIAN_POINT ( 'NONE',  ( 151.9006048953203276, 267.5474299512962943, 16.88304673825244251 ) ) ;
#27219 = CARTESIAN_POINT ( 'NONE',  ( 195.7617614321055157, 291.5776783508526364, 16.33009124109666033 ) ) ;
#27221 = CARTESIAN_POINT ( 'NONE',  ( 199.1944722252943905, 285.6320488493591938, -18.17555833707144686 ) ) ;
#27222 = CARTESIAN_POINT ( 'NONE',  ( 22.78591565582352985, 172.4155109091896065, 2.679491924311254714 ) ) ;
#27223 = CARTESIAN_POINT ( 'NONE',  ( 31.37640799630998956, 30.06628583063843507, -9.188101187500006262 ) ) ;
#27224 = CARTESIAN_POINT ( 'NONE',  ( 78.92023586790456591, 59.45316570216661489, -16.52216786098995982 ) ) ;
#27225 = CARTESIAN_POINT ( 'NONE',  ( 75.74710703992727190, 61.96519950925610942, 15.69174628608256405 ) ) ;
#27226 = ORIENTED_EDGE ( 'NONE', *, *, #31318, .F. ) ;
#27227 = CARTESIAN_POINT ( 'NONE',  ( 21.92109465949963720, 30.84336893147756697, -7.433330006724137462 ) ) ;
#27228 = LINE ( 'NONE', #41405, #92812 ) ;
#27229 = CARTESIAN_POINT ( 'NONE',  ( -32.94356256989596687, 94.79146141117595903, 10.56663419031904638 ) ) ;
#27230 = CARTESIAN_POINT ( 'NONE',  ( 188.1715415252454875, 286.2139794281218315, -16.72207616993653545 ) ) ;
#27231 = CARTESIAN_POINT ( 'NONE',  ( 86.41183189003805865, 47.25727891775800771, 10.78350007392548271 ) ) ;
#27232 = CARTESIAN_POINT ( 'NONE',  ( 74.15819116760899021, 61.47642609411447268, 15.57054964276887077 ) ) ;
#27233 = CARTESIAN_POINT ( 'NONE',  ( -52.35448371757384223, 98.99314617336143840, -10.00000000000000000 ) ) ;
#27234 = CARTESIAN_POINT ( 'NONE',  ( 120.0388121219830282, 250.1115022471903160, -5.000000000000047962 ) ) ;
#27235 = CARTESIAN_POINT ( 'NONE',  ( 205.2937235227012707, 275.0678357141204629, -12.80017165135291535 ) ) ;
#27236 = CARTESIAN_POINT ( 'NONE',  ( 74.95803460708295063, 53.16054836391673177, 16.51037805420591198 ) ) ;
#27237 = ORIENTED_EDGE ( 'NONE', *, *, #41670, .T. ) ;
#27238 = AXIS2_PLACEMENT_3D ( 'NONE', #6752, #5260, #59934 ) ;
#27239 = CARTESIAN_POINT ( 'NONE',  ( 168.5988957253557601, 248.5132396387117524, -1.885179999880600477 ) ) ;
#27240 = ORIENTED_EDGE ( 'NONE', *, *, #62157, .F. ) ;
#27241 = CARTESIAN_POINT ( 'NONE',  ( 163.3854574543125580, 247.6550818016845597, 10.82482370245618775 ) ) ;
#27242 = FACE_OUTER_BOUND ( 'NONE', #85339, .T. ) ;
#27243 = VERTEX_POINT ( 'NONE', #75898 ) ;
#27244 = CARTESIAN_POINT ( 'NONE',  ( 88.00349997577261263, 44.64923112938743088, 4.253506518527973235 ) ) ;
#27245 = VERTEX_POINT ( 'NONE', #21675 ) ;
#27246 = VECTOR ( 'NONE', #13648, 1000.000000000000000 ) ;
#27247 = CARTESIAN_POINT ( 'NONE',  ( 192.7167908629638760, 292.2639303239059814, 15.02160790781813660 ) ) ;
#27248 = CARTESIAN_POINT ( 'NONE',  ( 158.3286757630593513, 256.4136846137193970, 16.79716696587219005 ) ) ;
#27249 = CARTESIAN_POINT ( 'NONE',  ( 27.87199545867176198, 72.63159553030519078, 59.99999999999999289 ) ) ;
#27250 = CARTESIAN_POINT ( 'NONE',  ( 87.84569706029115821, 44.18597558567909545, -4.425511980624547093 ) ) ;
#27251 = DIRECTION ( 'NONE',  ( 1.000000000000000000, 0.000000000000000000, 0.000000000000000000 ) ) ;
#27252 = VECTOR ( 'NONE', #8193, 1000.000000000000114 ) ;
#27253 = AXIS2_PLACEMENT_3D ( 'NONE', #29015, #21407, #37576 ) ;
#27254 = CARTESIAN_POINT ( 'NONE',  ( 32.78369927745970358, 30.87878583063843863, -9.188101187500006262 ) ) ;
#27255 = CARTESIAN_POINT ( 'NONE',  ( 72.17023661803692391, 60.81924424899344928, -14.88691701024394298 ) ) ;
#27256 = CARTESIAN_POINT ( 'NONE',  ( 164.5789468726506470, 274.5585074141254722, 14.69886960705206569 ) ) ;
#27257 = ORIENTED_EDGE ( 'NONE', *, *, #81547, .F. ) ;
#27258 = ORIENTED_EDGE ( 'NONE', *, *, #88403, .F. ) ;
#27259 = CARTESIAN_POINT ( 'NONE',  ( 30.34687108590969373, 93.06504152958497400, -20.00000000000000355 ) ) ;
#27260 = VECTOR ( 'NONE', #85446, 1000.000000000000000 ) ;
#27262 = CARTESIAN_POINT ( 'NONE',  ( 147.6054094044680198, 274.9869267698931594, -8.596541856229405809 ) ) ;
#27261 = CARTESIAN_POINT ( 'NONE',  ( 68.21305639376519991, 65.88604169822291112, 10.81547118242297678 ) ) ;
#27263 = CARTESIAN_POINT ( 'NONE',  ( 85.73895798293081327, 48.63177274617319057, 12.34992197344710796 ) ) ;
#27264 = CARTESIAN_POINT ( 'NONE',  ( 154.9910882912764123, 262.1945556895526579, 18.38052604520346023 ) ) ;
#27265 = CARTESIAN_POINT ( 'NONE',  ( 147.4771028564622100, 275.6046161191591182, 9.141179566768406735E-14 ) ) ;
#27266 = FACE_OUTER_BOUND ( 'NONE', #91157, .T. ) ;
#27267 = CARTESIAN_POINT ( 'NONE',  ( 208.0730008398676318, 270.2539861924646516, -3.911917750280078376 ) ) ;
#27268 = LINE ( 'NONE', #88128, #77649 ) ;
#27269 = AXIS2_PLACEMENT_3D ( 'NONE', #86566, #17096, #54581 ) ;
#27270 = CARTESIAN_POINT ( 'NONE',  ( 10.12303320400422635, 49.19103222140901011, 59.99999999999999289 ) ) ;
#27271 = CARTESIAN_POINT ( 'NONE',  ( 108.5912123618160763, 227.3768266524159856, -9.188101187500091527 ) ) ;
#27272 = VERTEX_POINT ( 'NONE', #38851 ) ;
#27273 = CARTESIAN_POINT ( 'NONE',  ( 58.43017357788679789, 217.8207943907112849, 17.47570218321536473 ) ) ;
#27274 = CARTESIAN_POINT ( 'NONE',  ( 166.5201100233303464, 278.0365861635631859, -13.36835105817650060 ) ) ;
#27275 = EDGE_CURVE ( 'NONE', #3488, #12952, #21190, .T. ) ;
#27276 = ORIENTED_EDGE ( 'NONE', *, *, #89556, .T. ) ;
#27277 = ORIENTED_EDGE ( 'NONE', *, *, #3471, .T. ) ;
#27278 = CARTESIAN_POINT ( 'NONE',  ( 87.11842579636694950, 45.87328929624024454, -8.641498891285833039 ) ) ;
#27279 = CARTESIAN_POINT ( 'NONE',  ( 177.4333559188052050, 292.4950673467274669, -2.688042529096076994 ) ) ;
#27280 = CARTESIAN_POINT ( 'NONE',  ( 157.0957870390718369, 258.5491105237443321, 17.69218919045495397 ) ) ;
#27281 = CARTESIAN_POINT ( 'NONE',  ( 15.57129692638689633, 14.15404122711132295, 8.090169943749479842 ) ) ;
#27282 = CARTESIAN_POINT ( 'NONE',  ( 163.1968603775171118, 247.9817415208531202, 11.27455733958931994 ) ) ;
#27283 = CARTESIAN_POINT ( 'NONE',  ( 92.46148921633090367, 218.0643266524160140, 9.188101187500095079 ) ) ;
#27284 = ORIENTED_EDGE ( 'NONE', *, *, #60291, .F. ) ;
#27285 = AXIS2_PLACEMENT_3D ( 'NONE', #29920, #83159, #45115 ) ;
#27286 = ORIENTED_EDGE ( 'NONE', *, *, #40095, .F. ) ;
#27287 = PLANE ( 'NONE',  #76980 ) ;
#27288 = ORIENTED_EDGE ( 'NONE', *, *, #64821, .F. ) ;
#27289 = EDGE_CURVE ( 'NONE', #17528, #36742, #93219, .T. ) ;
#27290 = CARTESIAN_POINT ( 'NONE',  ( 191.5793115159691524, 263.6492056449409347, -8.156572570947284717 ) ) ;
#27291 = CARTESIAN_POINT ( 'NONE',  ( 154.2194984598485519, 265.5309884801890234, 17.12742652472672944 ) ) ;
#27292 = CARTESIAN_POINT ( 'NONE',  ( 72.06406741461755416, 69.35207420037858128, -8.748526250032554685 ) ) ;
#27294 = CARTESIAN_POINT ( 'NONE',  ( 69.42008239677498693, 62.93315161398718516, -13.66206540601166175 ) ) ;
#27293 = CARTESIAN_POINT ( 'NONE',  ( 137.1700506867025808, 243.8768266524160140, -9.188101187500091527 ) ) ;
#27295 = CARTESIAN_POINT ( 'NONE',  ( -10.09954699608895901, 171.6427522451419350, -10.00000000000009415 ) ) ;
#27296 = CARTESIAN_POINT ( 'NONE',  ( 171.3840324641641359, 249.8316075428874683, -4.467467663849890691 ) ) ;
#27297 = ORIENTED_EDGE ( 'NONE', *, *, #29049, .F. ) ;
#27298 = CARTESIAN_POINT ( 'NONE',  ( 204.5840280042472159, 276.2970644099866036, 14.65559382949596667 ) ) ;
#27299 = CARTESIAN_POINT ( 'NONE',  ( 81.69026040342092188, 48.56800976308773699, 13.34553584479553123 ) ) ;
#27300 = CARTESIAN_POINT ( 'NONE',  ( 93.60468337831817109, 236.3967562850347122, -4.648177544792955347E-16 ) ) ;
#27301 = CARTESIAN_POINT ( 'NONE',  ( 188.8377537886989899, 269.5936382258537378, 14.70355276031261660 ) ) ;
#27302 = CARTESIAN_POINT ( 'NONE',  ( 178.4489778659152250, 285.3664758674125892, 13.08110770347619400 ) ) ;
#27303 = DIRECTION ( 'NONE',  ( -0.4999999999999996669, 0.8660254037844387076, 0.000000000000000000 ) ) ;
#27304 = CARTESIAN_POINT ( 'NONE',  ( 198.4446623809833170, 281.5023889509741934, -16.57120230699170094 ) ) ;
#27305 = CARTESIAN_POINT ( 'NONE',  ( 122.1835217032046330, 252.8967562850346553, -4.648177544792955347E-16 ) ) ;
#27306 = CARTESIAN_POINT ( 'NONE',  ( 80.19859069096013116, 50.95987101629014404, 14.90308782861245263 ) ) ;
#27307 = CARTESIAN_POINT ( 'NONE',  ( 70.63484837994894860, 70.56325258955124013, -4.892680775417415084 ) ) ;
#27308 = VECTOR ( 'NONE', #37594, 1000.000000000000114 ) ;
#27309 = CARTESIAN_POINT ( 'NONE',  ( 167.8014687349847520, 250.0213847097312225, 6.957476650644477623 ) ) ;
#27310 = CARTESIAN_POINT ( 'NONE',  ( -63.30067564770008914, 39.94154026010144065, -10.00000000000000000 ) ) ;
#27311 = CARTESIAN_POINT ( 'NONE',  ( 208.3682389855799499, 269.7426187237583690, -1.431169231381201890 ) ) ;
#27312 = LINE ( 'NONE', #42484, #33278 ) ;
#27313 = AXIS2_PLACEMENT_3D ( 'NONE', #58225, #19752, #23430 ) ;
#27314 = VECTOR ( 'NONE', #18440, 1000.000000000000227 ) ;
#27315 = AXIS2_PLACEMENT_3D ( 'NONE', #98023, #28599, #51915 ) ;
#27316 =( LENGTH_UNIT ( ) NAMED_UNIT ( * ) SI_UNIT ( .MILLI., .METRE. ) );
#27318 = CARTESIAN_POINT ( 'NONE',  ( 74.24838807813938502, 55.19146615926651123, 16.60400907293851347 ) ) ;
#27317 = CARTESIAN_POINT ( 'NONE',  ( 47.54560441532652959, 78.55524412553474178, -10.00000000000000000 ) ) ;
#27319 = CARTESIAN_POINT ( 'NONE',  ( 180.0662822340164269, 262.4007578510376675, -14.24330825748563534 ) ) ;
#27320 = ADVANCED_FACE ( 'NONE', ( #15542 ), #53062, .T. ) ;
#27321 = CARTESIAN_POINT ( 'NONE',  ( 38.10324709940346821, 24.12755873383628114, -6.180339887498949025 ) ) ;
#27322 = CARTESIAN_POINT ( 'NONE',  ( -19.65312891409030271, 93.06504152958497400, -10.00000000000000888 ) ) ;
#27323 =( NAMED_UNIT ( * ) PLANE_ANGLE_UNIT ( ) SI_UNIT ( $, .RADIAN. ) );
#27324 = CARTESIAN_POINT ( 'NONE',  ( 158.3644695203838069, 271.4464815599769167, -14.70628431356059451 ) ) ;
#27325 = CARTESIAN_POINT ( 'NONE',  ( 205.7872507830675204, 272.2130214242461079, -9.506855900917111413 ) ) ;
#27326 = CARTESIAN_POINT ( 'NONE',  ( 207.1432938686257046, 271.8642859028066141, -6.405155839440290322 ) ) ;
#27327 = CARTESIAN_POINT ( 'NONE',  ( 10.89220085373657376, 189.3464784336661353, 1.353441290958777327E-15 ) ) ;
#27328 = CARTESIAN_POINT ( 'NONE',  ( 207.0320938795157417, 270.2489720413080363, 3.395226072341499979 ) ) ;
#27329 = EDGE_LOOP ( 'NONE', ( #29831, #49510, #86746, #90320 ) ) ;
#27330 = EDGE_CURVE ( 'NONE', #4429, #83781, #44958, .T. ) ;
#27331 = CARTESIAN_POINT ( 'NONE',  ( 86.75161163761312366, 46.45414409713080062, 9.084461998406249350 ) ) ;
#27332 = CARTESIAN_POINT ( 'NONE',  ( -22.42236680055709641, 157.8615022471902591, 0.000000000000000000 ) ) ;
#27333 = CARTESIAN_POINT ( 'NONE',  ( 71.56491451745446852, 72.38511813685279606, -1.315970478074329764 ) ) ;
#27334 = CARTESIAN_POINT ( 'NONE',  ( 41.20343708195693466, 194.5958772461660544, -9.188101187500095079 ) ) ;
#27335 = VECTOR ( 'NONE', #50844, 1000.000000000000000 ) ;
#27336 = CARTESIAN_POINT ( 'NONE',  ( 161.7910648966377209, 250.4166507187868831, 13.19274492748169436 ) ) ;
#27337 = CARTESIAN_POINT ( 'NONE',  ( 146.9324727656309335, 276.1524872186338371, 3.813717745456558728 ) ) ;
#27338 = CARTESIAN_POINT ( 'NONE',  ( 38.01218019840322881, 27.11029122506296929, -8.090169943749478065 ) ) ;
#27339 = CARTESIAN_POINT ( 'NONE',  ( 45.79324619304848909, 117.8999360398438654, -10.00000000000000000 ) ) ;
#27340 = CARTESIAN_POINT ( 'NONE',  ( 191.0702043019150835, 299.7036936669546776, -8.800021049343948576 ) ) ;
#27341 = CARTESIAN_POINT ( 'NONE',  ( 177.1262862392189845, 269.6057104283654553, 17.56656865388298172 ) ) ;
#27342 = CARTESIAN_POINT ( 'NONE',  ( 74.75130681297544299, 67.15234032204921277, -12.45738157583526373 ) ) ;
#27343 = B_SPLINE_SURFACE_WITH_KNOTS ( 'NONE', 3, 1, ( 
 ( #56340, #55822 ),
 ( #62429, #54843 ),
 ( #86816, #10263 ),
 ( #41132, #85824 ),
 ( #19868, #50246 ),
 ( #35546, #3672 ),
 ( #4145, #3190 ),
 ( #73074, #80198 ),
 ( #80706, #90296 ),
 ( #74065, #11282 ),
 ( #64964, #42142 ),
 ( #34073, #28434 ),
 ( #19387, #59316 ),
 ( #66447, #34550 ),
 ( #49262, #95909 ),
 ( #65448, #27468 ),
 ( #43122, #96394 ),
 ( #26958, #96898 ),
 ( #97375, #57841 ),
 ( #35040, #26467 ),
 ( #88821, #10767 ),
 ( #41641, #27941 ),
 ( #72584, #58823 ),
 ( #81200, #57343 ),
 ( #88317, #89785 ),
 ( #20361, #11769 ),
 ( #12263, #5152 ),
 ( #18871, #51232 ),
 ( #89314, #49754 ),
 ( #42632, #50735 ),
 ( #58338, #82200 ) ),
 .UNSPECIFIED., .F., .F., .F.,
 ( 4, 3, 3, 3, 3, 3, 3, 3, 3, 3, 4 ),
 ( 2, 2 ),
 ( 0.000000000000000000, 0.1122669598086892678, 0.2243161639709728983, 0.3396355846219379915, 0.4553962076585332253, 0.5677860799922617163, 0.6749047109689904067, 0.7773884377078581487, 0.8775581155834453195, 0.9782364162378207606, 1.000000000000000000 ),
 ( 0.000000000000000000, 1.000000000000000000 ),
 .UNSPECIFIED. ) ;
#27344 = DIRECTION ( 'NONE',  ( -8.673617379884075901E-16, 0.000000000000000000, 1.000000000000000000 ) ) ;
#27345 = CARTESIAN_POINT ( 'NONE',  ( 78.46959274033001464, 216.1115022471902591, 10.00000000000009592 ) ) ;
#27346 = CARTESIAN_POINT ( 'NONE',  ( 50.34412104557527812, 188.3262482093458061, 3.021315404115420679E-15 ) ) ;
#27347 = CARTESIAN_POINT ( 'NONE',  ( -51.42721978966704910, 42.16899896210639298, 10.00000000000001599 ) ) ;
#27348 = ORIENTED_EDGE ( 'NONE', *, *, #42979, .T. ) ;
#27349 = CARTESIAN_POINT ( 'NONE',  ( 43.96371950863733247, 202.3149278399160949, -9.188101187500095079 ) ) ;
#27350 = ORIENTED_EDGE ( 'NONE', *, *, #18531, .T. ) ;
#27351 = CARTESIAN_POINT ( 'NONE',  ( -14.40683470423637580, 84.83712956603842770, 15.00048218900240116 ) ) ;
#27352 = CARTESIAN_POINT ( 'NONE',  ( 151.1126408083691501, 268.9122237844355254, -15.82705194100464396 ) ) ;
#27353 = CARTESIAN_POINT ( 'NONE',  ( 67.01113855788433682, 66.95909584220486011, -8.721462188034738716 ) ) ;
#27354 = ORIENTED_EDGE ( 'NONE', *, *, #91967, .F. ) ;
#27355 = CARTESIAN_POINT ( 'NONE',  ( 171.3214800902178467, 286.5990332881968357, 8.223688229099183289 ) ) ;
#27356 = CARTESIAN_POINT ( 'NONE',  ( 164.4858674010174298, 245.7491158648375347, -2.958464974013825355 ) ) ;
#27357 = DIRECTION ( 'NONE',  ( -0.000000000000000000, -0.000000000000000000, -1.000000000000000000 ) ) ;
#27358 = CARTESIAN_POINT ( 'NONE',  ( 27.31210279805776509, 33.95586893147756768, 7.433330006724141015 ) ) ;
#27359 = CARTESIAN_POINT ( 'NONE',  ( 189.4145974059905200, 265.0249961711397191, 10.45958848644401407 ) ) ;
#27360 = CARTESIAN_POINT ( 'NONE',  ( 86.30977306730703447, 47.58285218899635538, -10.62438056216880611 ) ) ;
#27361 = CARTESIAN_POINT ( 'NONE',  ( 171.6881850446922613, 255.8132376700287125, 11.22435778083355196 ) ) ;
#27362 = ORIENTED_EDGE ( 'NONE', *, *, #87886, .F. ) ;
#27363 = CARTESIAN_POINT ( 'NONE',  ( 17.37926562425035826, 12.96004757982089117, -5.678558825948275768 ) ) ;
#27364 = CARTESIAN_POINT ( 'NONE',  ( 30.99507739981537213, 18.86426979415090699, -3.090169943749474069 ) ) ;
#27365 = CARTESIAN_POINT ( 'NONE',  ( 174.8451195330017640, 255.1849038048701459, 8.216676969017473908 ) ) ;
#27366 = DIRECTION ( 'NONE',  ( 0.8660254037844395958, 0.4999999999999985567, 0.000000000000000000 ) ) ;
#27367 = VERTEX_POINT ( 'NONE', #67773 ) ;
#27368 = CARTESIAN_POINT ( 'NONE',  ( 77.62509034109919526, 60.55547991676347408, 16.28574085379002412 ) ) ;
#27369 = CARTESIAN_POINT ( 'NONE',  ( 150.7226148805041817, 269.5877685077668957, 15.52819754351937576 ) ) ;
#27370 = PLANE ( 'NONE',  #77127 ) ;
#27371 = ORIENTED_EDGE ( 'NONE', *, *, #17547, .T. ) ;
#27372 = CARTESIAN_POINT ( 'NONE',  ( 161.7412967960748915, 250.5028515975580774, -14.36228887024421041 ) ) ;
#27373 = CARTESIAN_POINT ( 'NONE',  ( 46.80869107419874098, 110.6443039040113092, 10.00000000000000000 ) ) ;
#27374 = ORIENTED_EDGE ( 'NONE', *, *, #81348, .F. ) ;
#27375 = CARTESIAN_POINT ( 'NONE',  ( 66.54075137518582039, 68.81555626029070538, -2.231460399992864829 ) ) ;
#27376 = VECTOR ( 'NONE', #47333, 1000.000000000000000 ) ;
#27377 = CARTESIAN_POINT ( 'NONE',  ( 198.3075590527773784, 287.1682275260610027, 16.94807365630277118 ) ) ;
#27378 = DIRECTION ( 'NONE',  ( -0.4851478631379979034, 0.8403007481384877631, 0.2419218955996582654 ) ) ;
#27379 = CARTESIAN_POINT ( 'NONE',  ( 78.17692338680700459, 61.78069039082561886, -15.73643159653562229 ) ) ;
#27380 = CARTESIAN_POINT ( 'NONE',  ( 197.9813997048801184, 286.8186411885521920, 16.94230379787914131 ) ) ;
#27381 = CARTESIAN_POINT ( 'NONE',  ( 116.3579438323015012, 247.1744531367911293, 4.594050593750047540 ) ) ;
#27382 = VECTOR ( 'NONE', #49004, 1000.000000000000000 ) ;
#27383 = CARTESIAN_POINT ( 'NONE',  ( 150.7530568467738590, 269.5350414755053521, 15.60317050893315916 ) ) ;
#27384 = B_SPLINE_CURVE_WITH_KNOTS ( 'NONE', 3,
 ( #49496, #17607, #48516, #2425, #56600, #80452, #87586, #11024, #30927, #26706, #84668, #15211, #38517, #69428, #50003, #58579, #73803, #50487, #59573, #82459, #19131, #44381, #34786, #19628, #66690, #5894, #27212, #96644, #58096, #89552, #90036, #36287, #80959, #42870, #51491, #51996, #75313, #50985, #81935, #73315, #74327, #3906, #12513, #82937, #81442, #21119, #74824, #13022, #12013, #90548, #89079, #11524 ),
 .UNSPECIFIED., .F., .F.,
 ( 4, 2, 2, 2, 2, 2, 2, 2, 2, 2, 2, 2, 2, 2, 2, 2, 2, 2, 2, 2, 2, 2, 2, 2, 2, 4 ),
 ( 0.0008917468271082998289, 0.001373251144630191749, 0.001854755462152083562, 0.002095507620913045297, 0.002336259779674007466, 0.002456635859054485515, 0.002577011938434963564, 0.002697388017815441179, 0.002817764097195919228, 0.003058516255956880096, 0.003299268414717840964, 0.003780772732239826017, 0.004743781367283867248, 0.005706790002327906744, 0.006188294319849931696, 0.006669798637371957516, 0.006790174716752526637, 0.006850362756442810765, 0.006910550796133095759, 0.007030926875513786312, 0.007151302954894477731, 0.007392055113655964654, 0.007632807272417452445, 0.007873559431178938500, 0.008114311589940425423, 0.008595815907463411412 ),
 .UNSPECIFIED. ) ;
#27385 = CARTESIAN_POINT ( 'NONE',  ( -22.42236680055709641, 157.8615022471902591, 0.000000000000000000 ) ) ;
#27386 = CARTESIAN_POINT ( 'NONE',  ( 42.76202708541289610, 64.24573752441608576, -10.00000000000000000 ) ) ;
#27387 = EDGE_CURVE ( 'NONE', #26784, #7334, #77372, .T. ) ;
#27388 = EDGE_LOOP ( 'NONE', ( #95326, #90624, #74306, #59517 ) ) ;
#27389 = AXIS2_PLACEMENT_3D ( 'NONE', #21924, #22425, #63789 ) ;
#27390 = CARTESIAN_POINT ( 'NONE',  ( 163.7012083107868534, 247.1081852757374975, -6.544933039329257518 ) ) ;
#27391 = EDGE_LOOP ( 'NONE', ( #39646, #18140, #78107, #42679 ) ) ;
#27392 = CARTESIAN_POINT ( 'NONE',  ( 40.09738740370236343, 25.01110640527295104, 2.839279412974134775 ) ) ;
#27393 = CARTESIAN_POINT ( 'NONE',  ( 160.0072461633487535, 253.5063153963366744, 16.23938890643736244 ) ) ;
#27394 = CARTESIAN_POINT ( 'NONE',  ( 75.32215929224730644, 66.75623307483839142, -12.97587438736732857 ) ) ;
#27395 = EDGE_CURVE ( 'NONE', #82333, #57637, #6476, .T. ) ;
#27396 = CARTESIAN_POINT ( 'NONE',  ( 76.87303194821102181, 209.0643266524160424, 9.188101187500095079 ) ) ;
#27397 = ORIENTED_EDGE ( 'NONE', *, *, #82167, .T. ) ;
#27398 = CARTESIAN_POINT ( 'NONE',  ( 170.7667195423792066, 283.6621974811555447, 12.84944695255637548 ) ) ;
#27399 = CARTESIAN_POINT ( 'NONE',  ( 150.6571681785161445, 269.7011255207979730, 15.24894850018880454 ) ) ;
#27400 = CARTESIAN_POINT ( 'NONE',  ( 193.8603219414924013, 294.8710681561126989, 15.36476279452078586 ) ) ;
#27401 = CARTESIAN_POINT ( 'NONE',  ( 171.9660161825155171, 276.8101763654939305, 16.40752538293672202 ) ) ;
#27402 = ORIENTED_EDGE ( 'NONE', *, *, #41723, .T. ) ;
#27403 = VECTOR ( 'NONE', #16005, 1000.000000000000000 ) ;
#27404 =( BOUNDED_CURVE ( )  B_SPLINE_CURVE ( 2, ( #43027, #5063, #27364, #12676, #27855, #20771, #59737, #21260, #83089, #90197, #13660, #73968, #19775 ),
 .UNSPECIFIED., .F., .T. ) 
 B_SPLINE_CURVE_WITH_KNOTS ( ( 3, 2, 2, 2, 2, 2, 3 ),
 ( 0.5375000000000000888, 0.5400000000000000355, 0.5450000000000000400, 0.5500000000000000444, 0.5550000000000000488, 0.5600000000000000533, 0.5625000000000000000 ),
 .UNSPECIFIED. ) 
 CURVE ( )  GEOMETRIC_REPRESENTATION_ITEM ( )  RATIONAL_B_SPLINE_CURVE ( ( 0.9755282581475767101, 0.9755282581475772652, 1.000000000000000000, 0.9510565162951535312, 1.000000000000000000, 0.9510565162951535312, 1.000000000000000000, 0.9510565162951535312, 1.000000000000000000, 0.9510565162951535312, 1.000000000000000000, 0.9755282581475768211, 0.9755282581475768211 ) ) 
 REPRESENTATION_ITEM ( '' )  );
#27405 = CARTESIAN_POINT ( 'NONE',  ( 79.72917429462620476, 56.72943457089122887, -16.18511265363209262 ) ) ;
#27406 = CARTESIAN_POINT ( 'NONE',  ( 86.88643351309953289, 43.57251993220791064, -2.221051584189594141 ) ) ;
#27407 = LINE ( 'NONE', #97321, #22174 ) ;
#27408 = ORIENTED_EDGE ( 'NONE', *, *, #15045, .T. ) ;
#27409 = CARTESIAN_POINT ( 'NONE',  ( 147.9235661301700304, 274.4358631562076880, 9.736478568371106590 ) ) ;
#27410 = CARTESIAN_POINT ( 'NONE',  ( 72.15083153978913799, 69.85550926597292687, -8.070654529112998077 ) ) ;
#27411 = EDGE_CURVE ( 'NONE', #68946, #72634, #98057, .T. ) ;
#27412 = CARTESIAN_POINT ( 'NONE',  ( 161.2133744761260061, 251.4172398781588811, -14.30368667312104058 ) ) ;
#27413 = CARTESIAN_POINT ( 'NONE',  ( 206.4894746850401077, 270.6312975806551435, 2.443363978982824758 ) ) ;
#27414 = CARTESIAN_POINT ( 'NONE',  ( 199.6930299107040412, 283.1861613635016397, -17.43055490872784574 ) ) ;
#27415 = CARTESIAN_POINT ( 'NONE',  ( 176.9054780674279073, 269.9821856685988450, 16.79845386343675173 ) ) ;
#27416 = VECTOR ( 'NONE', #33580, 1000.000000000000114 ) ;
#27417 = CARTESIAN_POINT ( 'NONE',  ( 165.0297293518065658, 244.8071193337670195, 2.517333243890161665 ) ) ;
#27418 = CARTESIAN_POINT ( 'NONE',  ( 132.9389821956409037, 240.8927522451417929, -10.00000000000009237 ) ) ;
#27419 = CARTESIAN_POINT ( 'NONE',  ( 167.6768863921620039, 256.3367762910957026, 13.59289973228994342 ) ) ;
#27420 = CARTESIAN_POINT ( 'NONE',  ( 8.231324050681719129, 168.8927522451417929, -10.00000000000009237 ) ) ;
#27421 = B_SPLINE_CURVE_WITH_KNOTS ( 'NONE', 3,
 ( #3202, #2184, #41147, #63961, #49275, #34086, #81211, #87355, #17363, #64976, #80212, #55835, #72597, #94903, #26973, #88331, #57855, #2686 ),
 .UNSPECIFIED., .F., .F.,
 ( 4, 2, 2, 2, 2, 2, 2, 2, 4 ),
 ( 0.003270768999366409358, 0.003375574448574713074, 0.003480379897783016357, 0.003585185346991320073, 0.003689990796199623790, 0.003899601694616248136, 0.004109212593032872049, 0.004947656186699188156, 0.006624543374031750115 ),
 .UNSPECIFIED. ) ;
#27422 = CARTESIAN_POINT ( 'NONE',  ( 133.4083396129551602, 238.6423013555409796, -4.594050593750043987 ) ) ;
#27423 = ORIENTED_EDGE ( 'NONE', *, *, #56831, .F. ) ;
#27424 = CARTESIAN_POINT ( 'NONE',  ( 83.33713981978522156, 44.18474327606488572, -8.510079784887897958 ) ) ;
#27425 = CARTESIAN_POINT ( 'NONE',  ( -19.65312891409030271, 93.06504152958497400, -45.00000000000001421 ) ) ;
#27426 = CARTESIAN_POINT ( 'NONE',  ( 205.8278679583572739, 273.7726763696764465, -10.01757226791932176 ) ) ;
#27427 = EDGE_CURVE ( 'NONE', #78977, #38977, #45941, .T. ) ;
#27428 =( BOUNDED_CURVE ( )  B_SPLINE_CURVE ( 2, ( #19815, #13213, #74013, #75505, #89265 ),
 .UNSPECIFIED., .F., .T. ) 
 B_SPLINE_CURVE_WITH_KNOTS ( ( 3, 2, 3 ),
 ( 0.000000000000000000, 0.002688172043010752903, 0.004032258064516129788 ),
 .UNSPECIFIED. ) 
 CURVE ( )  GEOMETRIC_REPRESENTATION_ITEM ( )  RATIONAL_B_SPLINE_CURVE ( ( 1.000000000000000000, 0.8660254037844387076, 1.000000000000000000, 0.9330127018922194093, 0.9330127018922194093 ) ) 
 REPRESENTATION_ITEM ( '' )  );
#27429 = DIRECTION ( 'NONE',  ( 0.000000000000000000, -0.000000000000000000, 1.000000000000000000 ) ) ;
#27430 = CARTESIAN_POINT ( 'NONE',  ( 75.35881874794577584, 64.35819607451507807, 14.30177369286720612 ) ) ;
#27431 = CARTESIAN_POINT ( 'NONE',  ( 25.88271472100439041, 39.90032630942971537, 177.5919119679930134 ) ) ;
#27432 = ORIENTED_EDGE ( 'NONE', *, *, #99971, .F. ) ;
#27433 = CARTESIAN_POINT ( 'NONE',  ( 77.40971008714576840, 60.09314948727423200, 15.95988927257681311 ) ) ;
#27434 = CARTESIAN_POINT ( 'NONE',  ( 166.2052710271649687, 248.2504166283805489, -5.515680059214410846 ) ) ;
#27435 = CARTESIAN_POINT ( 'NONE',  ( 147.6576679470944384, 275.6425429203924296, 2.820251122944001487 ) ) ;
#27436 = DIRECTION ( 'NONE',  ( 1.000000000000000000, 0.000000000000000000, 0.000000000000000000 ) ) ;
#27437 = LINE ( 'NONE', #81173, #1406 ) ;
#27438 = DIRECTION ( 'NONE',  ( -0.4999999999999987788, 0.8660254037844392627, 0.000000000000000000 ) ) ;
#27439 = DIRECTION ( 'NONE',  ( 0.6778389383370672094, 0.7352104281592295454, 0.000000000000000000 ) ) ;
#27440 = CARTESIAN_POINT ( 'NONE',  ( 69.68758890477889167, 70.59674914774343790, 2.763705297544655437 ) ) ;
#27441 = CARTESIAN_POINT ( 'NONE',  ( 204.8385597977314490, 275.8562024115307167, -12.64672659107585240 ) ) ;
#27442 = CARTESIAN_POINT ( 'NONE',  ( 170.6631332514753581, 250.4690807168623508, 3.666193302703367962 ) ) ;
#27443 = EDGE_CURVE ( 'NONE', #79838, #35708, #36866, .T. ) ;
#27444 = CARTESIAN_POINT ( 'NONE',  ( 12.55362526388469746, 30.18080186712592194, 3.090169943749475401 ) ) ;
#27445 = CARTESIAN_POINT ( 'NONE',  ( 149.6877696051026305, 271.3801731027346591, 11.89134584187677390 ) ) ;
#27446 = CARTESIAN_POINT ( 'NONE',  ( 28.46864935082048831, 149.7156766241961350, -21.50000000000001421 ) ) ;
#27447 = CARTESIAN_POINT ( 'NONE',  ( 169.4870084614010750, 285.2172692466178319, -7.974559327038013734 ) ) ;
#27448 = CARTESIAN_POINT ( 'NONE',  ( 198.2489255580726422, 287.2697837179150042, 18.53597557040773225 ) ) ;
#27449 = CARTESIAN_POINT ( 'NONE',  ( 149.0244553356880886, 274.5290671187512999, 9.114935767028397251 ) ) ;
#27450 = EDGE_CURVE ( 'NONE', #8803, #99288, #71203, .T. ) ;
#27451 = CARTESIAN_POINT ( 'NONE',  ( 132.0007880082076781, 257.0177522451418781, 5.000000000000046185 ) ) ;
#27452 = CARTESIAN_POINT ( 'NONE',  ( 172.2607799805669515, 283.9270791244886141, -12.74676459771014336 ) ) ;
#27453 = ORIENTED_EDGE ( 'NONE', *, *, #68021, .T. ) ;
#27454 = B_SPLINE_CURVE_WITH_KNOTS ( 'NONE', 3,
 ( #55677, #2011, #17716, #32897 ),
 .UNSPECIFIED., .F., .F.,
 ( 4, 4 ),
 ( 0.003210172446339780092, 0.008633305421422422105 ),
 .UNSPECIFIED. ) ;
#27455 = AXIS2_PLACEMENT_3D ( 'NONE', #6812, #89957, #6316 ) ;
#27456 = EDGE_CURVE ( 'NONE', #85402, #26873, #86454, .T. ) ;
#27457 = CARTESIAN_POINT ( 'NONE',  ( 196.4982648257524147, 290.3020170531091821, 16.69353242256149628 ) ) ;
#27458 = CARTESIAN_POINT ( 'NONE',  ( 148.3280470635002928, 273.7352816289870248, 9.058704604771318003 ) ) ;
#27459 = CARTESIAN_POINT ( 'NONE',  ( -7.619092152155813480, 178.6589784336661637, -6.496448406907676862E-16 ) ) ;
#27460 = CARTESIAN_POINT ( 'NONE',  ( 41.01373370305532973, 203.6744531367911293, 4.594050593750047540 ) ) ;
#27461 = VECTOR ( 'NONE', #18877, 1000.000000000000000 ) ;
#27462 = CARTESIAN_POINT ( 'NONE',  ( 178.6059155966152048, 259.3514611767804467, -10.88062025991058235 ) ) ;
#27463 = CARTESIAN_POINT ( 'NONE',  ( 22.42372293028334340, 18.11029122506294442, -8.090169943749478065 ) ) ;
#27464 = CARTESIAN_POINT ( 'NONE',  ( 68.03436534181504669, 65.58245731312226212, -10.28075334492668880 ) ) ;
#27465 = CARTESIAN_POINT ( 'NONE',  ( 157.0887340267001946, 258.5613266995183039, -17.61824281915036394 ) ) ;
#27466 = CARTESIAN_POINT ( 'NONE',  ( 192.5757274456924222, 292.4492253229388439, -14.29994009178870940 ) ) ;
#27467 = DIRECTION ( 'NONE',  ( 0.000000000000000000, 0.000000000000000000, 1.000000000000000000 ) ) ;
#27468 = CARTESIAN_POINT ( 'NONE',  ( 73.85921800226309131, 55.30839618332183250, -16.11850250866768874 ) ) ;
#27470 = ADVANCED_FACE ( 'NONE', ( #61152 ), #6962, .F. ) ;
#27469 = B_SPLINE_CURVE_WITH_KNOTS ( 'NONE', 3,
 ( #39542, #31457, #85737, #23860, #48685, #25892 ),
 .UNSPECIFIED., .F., .F.,
 ( 4, 2, 4 ),
 ( 0.000000000000000000, 0.3122824062940924850, 0.6245648125881849699 ),
 .UNSPECIFIED. ) ;
#27471 = CARTESIAN_POINT ( 'NONE',  ( 68.70876474829495351, 217.1427522451419065, 10.00000000000009415 ) ) ;
#27472 = EDGE_CURVE ( 'NONE', #75021, #61794, #99680, .T. ) ;
#27473 = CARTESIAN_POINT ( 'NONE',  ( 75.23386090781256996, 66.95079165826535927, 12.80542170859955498 ) ) ;
#27474 = CARTESIAN_POINT ( 'NONE',  ( 163.3071340352992991, 277.0811303350653247, 14.49351327170118431 ) ) ;
#27475 = DIRECTION ( 'NONE',  ( -0.000000000000000000, -0.000000000000000000, -1.000000000000000000 ) ) ;
#27476 = CARTESIAN_POINT ( 'NONE',  ( 39.49844957003023893, 203.6115022471903160, -5.000000000000047962 ) ) ;
#27477 = CARTESIAN_POINT ( 'NONE',  ( 181.7453103611686629, 291.7118052563983497, 9.176684814609201268 ) ) ;
#27478 = CARTESIAN_POINT ( 'NONE',  ( 202.9689790241539242, 279.0944113002206564, 15.85114608332523289 ) ) ;
#27479 = CARTESIAN_POINT ( 'NONE',  ( 1.717831006336420607, 180.9869531367911293, 4.594050593750046652 ) ) ;
#27480 = CARTESIAN_POINT ( 'NONE',  ( 165.2814945196670919, 284.9282336261690034, 4.158235161442515704 ) ) ;
#27481 = CARTESIAN_POINT ( 'NONE',  ( 153.3100492430090753, 265.1062007306585997, 16.32434963471121492 ) ) ;
#27482 = CARTESIAN_POINT ( 'NONE',  ( 29.36891313204580456, 35.14336893147757479, 7.433330006724141015 ) ) ;
#27483 = CARTESIAN_POINT ( 'NONE',  ( 165.0538309624641613, 244.7653741195639157, 2.311334310144196547 ) ) ;
#27484 = CARTESIAN_POINT ( 'NONE',  ( 164.5416088356626290, 245.6525688679454618, -1.463507744092769292 ) ) ;
#27485 = CARTESIAN_POINT ( 'NONE',  ( 34.14357333472769085, 43.21091486745863364, 7.012934429366973338E-14 ) ) ;
#27486 = DIRECTION ( 'NONE',  ( -0.8660254037844387076, -0.4999999999999998890, -0.000000000000000000 ) ) ;
#27487 = CARTESIAN_POINT ( 'NONE',  ( 0.000000000000000000, 0.000000000000000000, 0.000000000000000000 ) ) ;
#27488 = CARTESIAN_POINT ( 'NONE',  ( 11.06209807803029221, 12.10170272979924988, -7.433330006724141015 ) ) ;
#27489 = CARTESIAN_POINT ( 'NONE',  ( 126.8249895137406043, 232.4824982072973683, 3.021315404115420679E-15 ) ) ;
#27490 = CARTESIAN_POINT ( 'NONE',  ( 21.25954720759204974, 17.98920272979926338, 7.433330006724137462 ) ) ;
#27491 = VECTOR ( 'NONE', #69787, 1000.000000000000000 ) ;
#27492 = DIRECTION ( 'NONE',  ( -0.8756465943326132706, -0.4829524219151361542, 0.000000000000000000 ) ) ;
#27493 = CARTESIAN_POINT ( 'NONE',  ( 152.7050834466765536, 278.6643962355284998, -4.749106930788815184 ) ) ;
#27494 = ORIENTED_EDGE ( 'NONE', *, *, #98548, .F. ) ;
#27495 = CARTESIAN_POINT ( 'NONE',  ( -22.42236680055716036, 157.8615022471903444, 5.188172501216621122E-14 ) ) ;
#27496 = CARTESIAN_POINT ( 'NONE',  ( 181.4735074999749145, 292.1586133693310785, 10.55809797880889001 ) ) ;
#27497 = AXIS2_PLACEMENT_3D ( 'NONE', #69907, #70415, #47608 ) ;
#27498 = VERTEX_POINT ( 'NONE', #7976 ) ;
#27499 = CARTESIAN_POINT ( 'NONE',  ( 192.8010417052266234, 296.7057953447782097, 12.10593424093686643 ) ) ;
#27500 = CARTESIAN_POINT ( 'NONE',  ( 2.487887237287232711, 134.7156766241960497, -21.50000000000002487 ) ) ;
#27501 = CARTESIAN_POINT ( 'NONE',  ( 66.56247904705401197, 68.75629519960098435, 4.749523133327839375 ) ) ;
#27502 = CARTESIAN_POINT ( 'NONE',  ( 87.39560864876780499, 44.96555158233554295, 6.898727475461874370 ) ) ;
#27503 = ORIENTED_EDGE ( 'NONE', *, *, #80937, .F. ) ;
#27504 = EDGE_LOOP ( 'NONE', ( #41806, #13303, #61865, #21676 ) ) ;
#27506 = DIRECTION ( 'NONE',  ( 0.000000000000000000, 0.4385670422228088450, 0.8986984752829710876 ) ) ;
#27505 = CARTESIAN_POINT ( 'NONE',  ( 164.2709363216550855, 246.8183101628254406, -5.373927384795599949 ) ) ;
#27507 = CARTESIAN_POINT ( 'NONE',  ( 192.8323852661406761, 296.6515067047851062, 11.86505947732313615 ) ) ;
#27508 = EDGE_LOOP ( 'NONE', ( #80006, #51258, #24236, #78729 ) ) ;
#27509 = CARTESIAN_POINT ( 'NONE',  ( 77.13411046628633017, 54.31893080425083298, 16.04542608317086660 ) ) ;
#27510 = CARTESIAN_POINT ( 'NONE',  ( 174.4445693293744455, 262.3909980173429517, 14.47875634103648856 ) ) ;
#27511 = ORIENTED_EDGE ( 'NONE', *, *, #87161, .T. ) ;
#27512 = CARTESIAN_POINT ( 'NONE',  ( 77.99518601148065500, 61.05539905302716619, -15.87786080876372274 ) ) ;
#27513 = CARTESIAN_POINT ( 'NONE',  ( 88.50685567279400345, 43.87431988399859506, -0.03150979628302760099 ) ) ;
#27514 = B_SPLINE_CURVE_WITH_KNOTS ( 'NONE', 3,
 ( #58864, #98409, #14286, #81733, #6689, #29487, #28482, #68473, #44172, #51278, #90340, #6184, #50783, #12310, #21393, #82245, #12820, #76115, #36080, #75109, #90842, #29003, #20916, #36575 ),
 .UNSPECIFIED., .F., .F.,
 ( 4, 2, 2, 2, 2, 2, 2, 2, 2, 2, 2, 4 ),
 ( 0.000000000000000000, 0.1249999999999918954, 0.2499999999999837907, 0.3749999999999756861, 0.4374999999999744094, 0.4999999999999731326, 0.5624999999999718003, 0.6249999999999705791, 0.6874999999999692468, 0.7499999999999680256, 0.8749999999999840128, 1.000000000000000000 ),
 .UNSPECIFIED. ) ;
#27515 = CARTESIAN_POINT ( 'NONE',  ( 80.90734640522499888, 43.51802416776986604, 9.388539139721732596 ) ) ;
#27516 = EDGE_CURVE ( 'NONE', #74992, #59506, #84506, .T. ) ;
#27517 = ORIENTED_EDGE ( 'NONE', *, *, #97146, .T. ) ;
#27518 = CARTESIAN_POINT ( 'NONE',  ( 159.5541294036357840, 254.7329949101089142, -15.49503750354262088 ) ) ;
#27519 = CARTESIAN_POINT ( 'NONE',  ( 169.2920866366192456, 276.4291702812190579, -16.06723518864265188 ) ) ;
#27520 = CARTESIAN_POINT ( 'NONE',  ( -13.86269525828471849, 104.2312461070085021, 45.19948692389422717 ) ) ;
#27521 = VERTEX_POINT ( 'NONE', #28772 ) ;
#27522 = CARTESIAN_POINT ( 'NONE',  ( 174.4842243494688034, 276.9690305039630971, -15.77146616506232668 ) ) ;
#27523 = CARTESIAN_POINT ( 'NONE',  ( 171.1204324191836292, 262.9359187872178154, -15.53146915371453929 ) ) ;
#27524 = EDGE_CURVE ( 'NONE', #69092, #61410, #38348, .T. ) ;
#27525 = ORIENTED_EDGE ( 'NONE', *, *, #51666, .F. ) ;
#27526 = DIRECTION ( 'NONE',  ( 0.4999999999999998890, -0.8660254037844385966, 0.000000000000000000 ) ) ;
#27527 = EDGE_LOOP ( 'NONE', ( #98190, #6754, #16953, #86042 ) ) ;
#27528 = PLANE ( 'NONE',  #71925 ) ;
#27529 = EDGE_LOOP ( 'NONE', ( #40979, #1339, #1711, #1666 ) ) ;
#27530 = CARTESIAN_POINT ( 'NONE',  ( 169.0163292910675636, 272.4602990133035405, 17.15131738099888636 ) ) ;
#27531 = CARTESIAN_POINT ( 'NONE',  ( 193.2864259971985916, 295.8650850898874296, 14.21409792694320551 ) ) ;
#27532 = CARTESIAN_POINT ( 'NONE',  ( 188.6635337462180928, 298.6204119622300368, -4.269177026095916538 ) ) ;
#27533 = CARTESIAN_POINT ( 'NONE',  ( 88.45958475239287111, 43.85926912372239883, -0.5941283661710258235 ) ) ;
#27534 = CARTESIAN_POINT ( 'NONE',  ( 192.0523540417460993, 298.0025604169266558, 12.03387399082417275 ) ) ;
#27535 = EDGE_CURVE ( 'NONE', #10970, #27272, #81576, .T. ) ;
#27537 = CARTESIAN_POINT ( 'NONE',  ( 178.5255977161920669, 291.5666061038359089, 6.170387333470672253 ) ) ;
#27536 = CIRCLE ( 'NONE', #6480, 0.1418229129681522482 ) ;
#27538 = CARTESIAN_POINT ( 'NONE',  ( 196.9669828711821538, 289.4901735840007291, -17.16750406591627254 ) ) ;
#27539 = ORIENTED_EDGE ( 'NONE', *, *, #96408, .F. ) ;
#27540 = CARTESIAN_POINT ( 'NONE',  ( 73.85277556690290623, 58.08781524499210747, -15.86821318995104768 ) ) ;
#27541 = CARTESIAN_POINT ( 'NONE',  ( 151.2546443255573934, 275.3395117651207897, -9.775857568146751220 ) ) ;
#27543 = CARTESIAN_POINT ( 'NONE',  ( 45.88188149789386472, 72.29567966924399514, -10.00000000000000000 ) ) ;
#27542 = CARTESIAN_POINT ( 'NONE',  ( 77.45268913986690507, 49.77012986150322149, -14.98312777078430535 ) ) ;
#27545 = EDGE_LOOP ( 'NONE', ( #55657, #40291, #69856, #44904, #13538, #52069, #46453, #68741, #67627, #31572, #57149 ) ) ;
#27544 = CARTESIAN_POINT ( 'NONE',  ( 159.4889735931715222, 254.4039898200529706, 16.88104032092801887 ) ) ;
#27546 = B_SPLINE_CURVE_WITH_KNOTS ( 'NONE', 3,
 ( #1785, #2292, #62042, #55938 ),
 .UNSPECIFIED., .F., .F.,
 ( 4, 4 ),
 ( 0.009717938389684965469, 0.01571428049324324894 ),
 .UNSPECIFIED. ) ;
#27547 = ORIENTED_EDGE ( 'NONE', *, *, #21783, .T. ) ;
#27548 = CARTESIAN_POINT ( 'NONE',  ( 147.3572860122106647, 275.4166890918294825, -2.824341378914994038 ) ) ;
#27549 = CARTESIAN_POINT ( 'NONE',  ( 199.0837164482014714, 266.3850903537827435, 6.043064621626092148 ) ) ;
#27550 = CARTESIAN_POINT ( 'NONE',  ( 164.1954676172330210, 247.3737367566268972, 7.269074065105377791 ) ) ;
#27551 = EDGE_CURVE ( 'NONE', #28990, #32652, #55539, .T. ) ;
#27552 = CARTESIAN_POINT ( 'NONE',  ( 125.1447535615809414, 236.3927522451417929, -10.00000000000009237 ) ) ;
#27553 = EDGE_CURVE ( 'NONE', #12202, #13902, #29511, .T. ) ;
#27554 = CARTESIAN_POINT ( 'NONE',  ( 198.6245008644510222, 286.6192682051993188, -17.88211844573111975 ) ) ;
#27555 = CARTESIAN_POINT ( 'NONE',  ( 91.12263257074930323, 234.9637435831424739, 2.679491924311251605 ) ) ;
#27556 = AXIS2_PLACEMENT_3D ( 'NONE', #78639, #34039, #71540 ) ;
#27557 = EDGE_LOOP ( 'NONE', ( #77994, #33716, #38358, #56879 ) ) ;
#27558 = CARTESIAN_POINT ( 'NONE',  ( 167.2506521577460603, 252.9623063650430197, -12.17192564457983828 ) ) ;
#27559 = LINE ( 'NONE', #58425, #16022 ) ;
#27560 = CARTESIAN_POINT ( 'NONE',  ( 134.5031927440161326, 236.9155109091896065, 2.679491924311254714 ) ) ;
#27561 = CARTESIAN_POINT ( 'NONE',  ( 207.0200405408487541, 272.0777669287182334, 6.494273599193515878 ) ) ;
#27562 = CARTESIAN_POINT ( 'NONE',  ( 34.06774859691749668, 177.1427522451417360, 1.119607411625061291E-15 ) ) ;
#27563 = CARTESIAN_POINT ( 'NONE',  ( 103.3950599391094443, 224.3768266524160140, -9.188101187500093303 ) ) ;
#27564 = CARTESIAN_POINT ( 'NONE',  ( 180.8406542025288388, 294.1182405763964880, -2.664013851607027306 ) ) ;
#27565 = CARTESIAN_POINT ( 'NONE',  ( 167.5023760217605400, 281.6905759989244871, -10.92128487528961678 ) ) ;
#27566 = CARTESIAN_POINT ( 'NONE',  ( 13.14225634397871367, 29.36126292948895156, 6.180339887498949913 ) ) ;
#27567 = LINE ( 'NONE', #67031, #36908 ) ;
#27568 = CARTESIAN_POINT ( 'NONE',  ( 20.95974617273066443, 195.1589784336661637, -6.496448406907675876E-16 ) ) ;
#27569 = CARTESIAN_POINT ( 'NONE',  ( 200.7897860911934913, 282.8688841796032420, 18.17522996445731920 ) ) ;
#27570 = ORIENTED_EDGE ( 'NONE', *, *, #13843, .T. ) ;
#27571 = EDGE_LOOP ( 'NONE', ( #46715, #54521, #58489, #90954 ) ) ;
#27572 = PLANE ( 'NONE',  #23603 ) ;
#27573 = FACE_OUTER_BOUND ( 'NONE', #47614, .T. ) ;
#27574 = EDGE_CURVE ( 'NONE', #89501, #76706, #17563, .T. ) ;
#27575 = CARTESIAN_POINT ( 'NONE',  ( 110.0000000000000000, 0.000000000000000000, 59.99999999999999289 ) ) ;
#27576 = CARTESIAN_POINT ( 'NONE',  ( -22.42236680055709641, 157.8615022471902591, 0.000000000000000000 ) ) ;
#27577 = DIRECTION ( 'NONE',  ( 0.5000000000000007772, -0.8660254037844381525, 0.000000000000000000 ) ) ;
#27578 = CARTESIAN_POINT ( 'NONE',  ( 182.4011669864173086, 284.2493615651014238, 14.92779187816798547 ) ) ;
#27579 = DIRECTION ( 'NONE',  ( 2.816764622163179958E-16, 1.626259812849721275E-16, -1.000000000000000000 ) ) ;
#27580 = EDGE_CURVE ( 'NONE', #89979, #44653, #366, .T. ) ;
#27581 = CARTESIAN_POINT ( 'NONE',  ( 47.75258065019424691, 204.5024278399160949, 9.188101187500095079 ) ) ;
#27582 = CARTESIAN_POINT ( 'NONE',  ( 91.36976281398776223, 236.8927522451419350, 2.944929066748280225E-16 ) ) ;
#27583 = ORIENTED_EDGE ( 'NONE', *, *, #75842, .T. ) ;
#27584 = CARTESIAN_POINT ( 'NONE',  ( 198.4497957874126257, 267.8821814322857904, -8.033238290564030493 ) ) ;
#27585 = EDGE_CURVE ( 'NONE', #17408, #72864, #75456, .T. ) ;
#27586 = EDGE_CURVE ( 'NONE', #2810, #70911, #1720, .T. ) ;
#27587 = CARTESIAN_POINT ( 'NONE',  ( 2.692369909191673294, 162.3615022471902023, 5.000000000000051514 ) ) ;
#27588 = CARTESIAN_POINT ( 'NONE',  ( -4.208943576872074210, 174.5024278399160949, 9.188101187500095079 ) ) ;
#27589 = ADVANCED_FACE ( 'NONE', ( #46962 ), #99789, .T. ) ;
#27590 = CARTESIAN_POINT ( 'NONE',  ( 150.7850480413316632, 269.4796311011364764, -14.43114374163211089 ) ) ;
#27591 = DIRECTION ( 'NONE',  ( -0.9708212084269268738, 0.2398044646550214765, 0.000000000000000000 ) ) ;
#27592 = CARTESIAN_POINT ( 'NONE',  ( 193.2053309019613891, 296.0055459150826778, -12.79465285318189061 ) ) ;
#27593 = CARTESIAN_POINT ( 'NONE',  ( 164.3545367017254364, 245.9765873086048487, -5.942639963102972267 ) ) ;
#27594 = CARTESIAN_POINT ( 'NONE',  ( 204.2143397907769611, 276.5280330293650195, 13.36303585211030054 ) ) ;
#27595 = CARTESIAN_POINT ( 'NONE',  ( 186.8003541658358984, 299.2222177555264011, -0.6103433986344138917 ) ) ;
#27596 = CARTESIAN_POINT ( 'NONE',  ( 207.4285356523023154, 271.3702326410368642, 7.833982582429932506 ) ) ;
#27597 = ORIENTED_EDGE ( 'NONE', *, *, #51710, .T. ) ;
#27598 = CARTESIAN_POINT ( 'NONE',  ( -4.235833321083918079, 178.3615022471903160, 5.000000000000046185 ) ) ;
#27599 = PLANE ( 'NONE',  #11049 ) ;
#27600 = CARTESIAN_POINT ( 'NONE',  ( 128.8345561752773278, 239.0643266524160140, 9.188101187500095079 ) ) ;
#27601 = CARTESIAN_POINT ( 'NONE',  ( 25.46698091360950045, 30.10171378149919974, 9.188101187500008038 ) ) ;
#27602 = CARTESIAN_POINT ( 'NONE',  ( 181.0193311394079103, 261.5502185760933003, 13.24438261311760812 ) ) ;
#27603 = CARTESIAN_POINT ( 'NONE',  ( 150.9903069161591418, 270.0165872255406612, 13.76682917664489381 ) ) ;
#27605 = CARTESIAN_POINT ( 'NONE',  ( 75.29614551415185986, 66.72342768736930907, 13.41754944753248324 ) ) ;
#27604 = CARTESIAN_POINT ( 'NONE',  ( -78.10577900106846982, 54.55156729251706338, -10.00000000000000000 ) ) ;
#27606 = CARTESIAN_POINT ( 'NONE',  ( 69.66731286396763778, 199.4824982072973967, 3.021315404115420679E-15 ) ) ;
#27607 = ORIENTED_EDGE ( 'NONE', *, *, #83276, .T. ) ;
#27608 = CARTESIAN_POINT ( 'NONE',  ( 150.6571681785161445, 269.7011255207979730, 15.24894850018880454 ) ) ;
#27609 = CARTESIAN_POINT ( 'NONE',  ( 163.4319133527347390, 247.5746178253062055, 7.647903095947664376 ) ) ;
#27610 = CARTESIAN_POINT ( 'NONE',  ( 190.6522387254234729, 300.0187146158233986, 3.894424434267832247 ) ) ;
#27611 = DIRECTION ( 'NONE',  ( -0.9054088711727195093, 0.4245406647209920559, 0.000000000000000000 ) ) ;
#27612 = CARTESIAN_POINT ( 'NONE',  ( 81.37674444193763179, 55.19836804271280073, -15.94010240901345909 ) ) ;
#27613 = ORIENTED_EDGE ( 'NONE', *, *, #67126, .F. ) ;
#27614 = CARTESIAN_POINT ( 'NONE',  ( 69.29409999990139113, 67.53033690639284714, 8.887769012565335913 ) ) ;
#27615 = CYLINDRICAL_SURFACE ( 'NONE', #66836, 45.19948692389423428 ) ;
#27616 = B_SPLINE_CURVE_WITH_KNOTS ( 'NONE', 3,
 ( #83341, #53874, #84836, #84343, #52894, #13905, #15374, #44786, #60984, #6306, #37197, #45293, #60480, #83846, #76227, #14888, #71620, #64502, #9821, #17914, #16888, #63993, #39665, #95462, #79249, #17392, #40682, #70589 ),
 .UNSPECIFIED., .F., .F.,
 ( 4, 2, 2, 2, 2, 2, 2, 2, 2, 2, 2, 2, 2, 4 ),
 ( 0.0003625531286933231386, 0.002366764927985090181, 0.002867817877808072260, 0.002993081115263782760, 0.003024396924627741935, 0.003055712733991701111, 0.003087028543355660286, 0.003118344352719619461, 0.003243607590175527286, 0.003368870827631435111, 0.003619397302543357446, 0.003869923777455280215, 0.004120450252367202117, 0.004370976727279125319 ),
 .UNSPECIFIED. ) ;
#27617 = CARTESIAN_POINT ( 'NONE',  ( 83.19806100981892882, 42.06058512007242456, 4.429552854493146619 ) ) ;
#27618 = CARTESIAN_POINT ( 'NONE',  ( 200.1686525782743331, 272.4625969671961343, 12.58813841635031849 ) ) ;
#27619 = CARTESIAN_POINT ( 'NONE',  ( 177.7342311040593756, 255.2532439957012684, -8.367404576774948310 ) ) ;
#27620 = CARTESIAN_POINT ( 'NONE',  ( 70.31263914188156150, 71.26601167383878987, 0.5666459716601885965 ) ) ;
#27621 = VECTOR ( 'NONE', #69139, 1000.000000000000000 ) ;
#27622 = CARTESIAN_POINT ( 'NONE',  ( 148.5349717444102566, 274.3968686471137630, -7.864641605647691769 ) ) ;
#27623 = EDGE_LOOP ( 'NONE', ( #15511, #65158, #94261, #71366 ) ) ;
#27624 = B_SPLINE_CURVE_WITH_KNOTS ( 'NONE', 3,
 ( #48929, #1833, #2337, #17518, #55990, #25631, #94061, #86988, #24614, #71240, #95069, #48424, #79373, #2849, #9936, #72243, #40799, #79867, #33738, #41301, #95583, #5321, #50905, #12941, #43800, #13430, #65611, #20528, #42303, #81854, #88485, #12430, #36695, #73235, #67103, #19047, #89951, #82859, #28108, #36198, #81367, #28603, #11449, #4832, #3827, #43298, #58015, #58982, #96068, #97064 ),
 .UNSPECIFIED., .F., .F.,
 ( 4, 2, 2, 2, 2, 2, 2, 2, 2, 2, 2, 2, 2, 2, 2, 2, 2, 2, 2, 2, 2, 2, 2, 2, 4 ),
 ( 0.0008219441068872318295, 0.001020485464105246216, 0.001119756142714287616, 0.001219026821323329016, 0.001417568178541411599, 0.001616109535759494183, 0.002013192250195829786, 0.002410274964632165388, 0.003204440393504899044, 0.003998605822377632700, 0.004792771251250365488, 0.005189853965686732316, 0.005388395322904916164, 0.005487666001513965587, 0.005586936680123015010, 0.005636572019427577886, 0.005686207358732140761, 0.005785478037341302074, 0.005984019394559623832, 0.006182560751777944723, 0.006381102108996266481, 0.006579643466214587372, 0.006778184823432909130, 0.006976726180651230021, 0.007175267537869550911 ),
 .UNSPECIFIED. ) ;
#27625 = CARTESIAN_POINT ( 'NONE',  ( 3.854092266844447501, 28.45370138451379560, 10.00000000000000000 ) ) ;
#27626 = CARTESIAN_POINT ( 'NONE',  ( 5.625422033609194017, 26.18080186712590773, 3.090169943749475401 ) ) ;
#27627 = CARTESIAN_POINT ( 'NONE',  ( 13.67211979723576931, 32.92651376809308772, -10.00000000000000000 ) ) ;
#27628 = ORIENTED_EDGE ( 'NONE', *, *, #91884, .T. ) ;
#27629 = CARTESIAN_POINT ( 'NONE',  ( 171.3751619920873281, 280.2398791927632828, 15.33202389549764888 ) ) ;
#27630 = EDGE_CURVE ( 'NONE', #63867, #9557, #60884, .T. ) ;
#27631 = CARTESIAN_POINT ( 'NONE',  ( 194.5298665426430489, 293.7113828889860656, -16.13302716640051315 ) ) ;
#27632 = CARTESIAN_POINT ( 'NONE',  ( 156.0746793001935657, 261.9946646095714300, -16.96186522563439780 ) ) ;
#27633 = ORIENTED_EDGE ( 'NONE', *, *, #306, .F. ) ;
#27634 = CARTESIAN_POINT ( 'NONE',  ( 78.76778807799331616, 60.01474888753965331, 16.11287639625045287 ) ) ;
#27635 = CYLINDRICAL_SURFACE ( 'NONE', #7104, 10.00000000000001066 ) ;
#27636 = CARTESIAN_POINT ( 'NONE',  ( -110.0000000000000142, -8.000000000000000000, -14.21260523776211926 ) ) ;
#27637 = CYLINDRICAL_SURFACE ( 'NONE', #34966, 17.82106496071139645 ) ;
#27638 = ORIENTED_EDGE ( 'NONE', *, *, #39847, .F. ) ;
#27639 = CARTESIAN_POINT ( 'NONE',  ( 89.24104401994878799, 213.1423013555409796, -4.594050593750043987 ) ) ;
#27640 = CARTESIAN_POINT ( 'NONE',  ( 83.81360984122501634, 50.06911063634414916, -13.60028881744086604 ) ) ;
#27641 = DIRECTION ( 'NONE',  ( 0.000000000000000000, 0.000000000000000000, 1.000000000000000000 ) ) ;
#27642 = CARTESIAN_POINT ( 'NONE',  ( 182.0114982784328959, 257.6695253748193863, -5.972343101773933682 ) ) ;
#27643 = EDGE_LOOP ( 'NONE', ( #87273, #95, #70590, #72914 ) ) ;
#27644 = VERTEX_POINT ( 'NONE', #67150 ) ;
#27645 = LINE ( 'NONE', #35724, #48129 ) ;
#27646 = ORIENTED_EDGE ( 'NONE', *, *, #34322, .T. ) ;
#27647 = CARTESIAN_POINT ( 'NONE',  ( 24.55112987542764458, 40.41347472807389352, -10.00000000000000000 ) ) ;
#27648 = VERTEX_POINT ( 'NONE', #91480 ) ;
#27649 = LINE ( 'NONE', #51933, #12048 ) ;
#27650 = CARTESIAN_POINT ( 'NONE',  ( 155.5066938333533528, 261.3015006940112244, -18.40036130547566273 ) ) ;
#27651 = VERTEX_POINT ( 'NONE', #52942 ) ;
#27652 = CARTESIAN_POINT ( 'NONE',  ( 80.66432953410600248, 43.23603845041665750, -9.222336552745701965 ) ) ;
#27653 = CARTESIAN_POINT ( 'NONE',  ( -76.99869489832862257, 52.47050021824117749, -10.00000000000000000 ) ) ;
#27654 = CARTESIAN_POINT ( 'NONE',  ( 85.88522298860537774, 42.48983236706607158, -1.987639973148706440 ) ) ;
#27655 = EDGE_CURVE ( 'NONE', #50908, #16006, #94863, .T. ) ;
#27656 = CARTESIAN_POINT ( 'NONE',  ( 157.4387554167717553, 281.9416217953914270, 2.906349061691626989 ) ) ;
#27657 = CARTESIAN_POINT ( 'NONE',  ( 149.7817191771959244, 245.0327760586659451, 1.948934522072303157E-15 ) ) ;
#27658 = CARTESIAN_POINT ( 'NONE',  ( -22.42236680055709641, 157.8615022471902591, 0.000000000000000000 ) ) ;
#27659 = ORIENTED_EDGE ( 'NONE', *, *, #54391, .F. ) ;
#27660 = LINE ( 'NONE', #90982, #54407 ) ;
#27661 = CARTESIAN_POINT ( 'NONE',  ( 11.67313376208573139, 15.24335787977761747, -9.188101187500008038 ) ) ;
#27662 = ORIENTED_EDGE ( 'NONE', *, *, #54652, .T. ) ;
#27663 = CARTESIAN_POINT ( 'NONE',  ( 163.9449312135976129, 281.9653101204439736, 8.519335645788913780 ) ) ;
#27665 = ORIENTED_EDGE ( 'NONE', *, *, #55435, .T. ) ;
#27664 = CARTESIAN_POINT ( 'NONE',  ( 203.6513521002680136, 271.6927919894359320, 9.604818643925334243 ) ) ;
#27666 = CARTESIAN_POINT ( 'NONE',  ( -13.95001416935992289, 104.7385778355855592, 10.43465946748403184 ) ) ;
#27667 = CYLINDRICAL_SURFACE ( 'NONE', #98222, 10.00000000000010658 ) ;
#27668 = CARTESIAN_POINT ( 'NONE',  ( 76.27995519852129291, 65.06343769965553747, -14.23913457056448451 ) ) ;
#27669 = CARTESIAN_POINT ( 'NONE',  ( 156.7777268389594667, 279.3827415317243776, 7.395700627148257489 ) ) ;
#27670 = EDGE_CURVE ( 'NONE', #76355, #35626, #77712, .T. ) ;
#27671 = CARTESIAN_POINT ( 'NONE',  ( 70.76455878343632833, 60.85362355774473997, 14.54687513196817861 ) ) ;
#27672 = DIRECTION ( 'NONE',  ( -0.8660254037844392627, -0.4999999999999987232, 0.000000000000000000 ) ) ;
#27673 = ADVANCED_FACE ( 'NONE', ( #9868 ), #8837, .T. ) ;
#27674 = CARTESIAN_POINT ( 'NONE',  ( 85.45242742188823115, 42.84966524789818010, 2.600776799952281504 ) ) ;
#27675 = CARTESIAN_POINT ( 'NONE',  ( 88.30346302270005765, 44.31045525142044994, -2.071979982890664651 ) ) ;
#27676 = EDGE_LOOP ( 'NONE', ( #52775, #18035 ) ) ;
#27677 = CARTESIAN_POINT ( 'NONE',  ( 196.9526636073363477, 287.5149752765084941, -17.63101726665603053 ) ) ;
#27678 = CARTESIAN_POINT ( 'NONE',  ( 66.37277438342361791, 68.89659095610979023, 0.08793121599326786386 ) ) ;
#27679 = ORIENTED_EDGE ( 'NONE', *, *, #68895, .F. ) ;
#27680 = CARTESIAN_POINT ( 'NONE',  ( 160.5181951850485405, 275.9162642635258749, 12.68197119230242542 ) ) ;
#27681 = DIRECTION ( 'NONE',  ( 1.000000000000000000, 1.784287003861858500E-15, 0.000000000000000000 ) ) ;
#27682 = DIRECTION ( 'NONE',  ( -0.8450603975019853609, 0.5346708562973920831, 0.000000000000000000 ) ) ;
#27683 = CARTESIAN_POINT ( 'NONE',  ( 80.79863759358339337, 44.88662211388689371, -10.92354475286181525 ) ) ;
#27684 = DIRECTION ( 'NONE',  ( -0.9331105242498700658, 0.3595896960900473172, 0.000000000000000000 ) ) ;
#27686 = CARTESIAN_POINT ( 'NONE',  ( 88.46324942983896733, 43.96425106107525949, 1.817931795122156080 ) ) ;
#27685 = CARTESIAN_POINT ( 'NONE',  ( 174.5885488454506174, 256.4458599265808516, 12.05082362884263425 ) ) ;
#27687 = CARTESIAN_POINT ( 'NONE',  ( 203.6314934253803131, 269.6250664415474034, 5.533663177072089212 ) ) ;
#27688 = ORIENTED_EDGE ( 'NONE', *, *, #37760, .T. ) ;
#27689 = ORIENTED_EDGE ( 'NONE', *, *, #87804, .T. ) ;
#27690 = CARTESIAN_POINT ( 'NONE',  ( 76.06646813575576971, 61.15541120234568240, -15.53810128048082539 ) ) ;
#27691 = CARTESIAN_POINT ( 'NONE',  ( 116.9873692804980010, 249.8967562850347122, -4.648177544792955347E-16 ) ) ;
#27692 = CARTESIAN_POINT ( 'NONE',  ( 70.44830684995079650, 66.16034588321909382, -11.13951868050791383 ) ) ;
#27693 = CARTESIAN_POINT ( 'NONE',  ( 175.2003707602579823, 290.7303100365182331, 2.563854479286836963 ) ) ;
#27694 = CARTESIAN_POINT ( 'NONE',  ( 192.7259387352017939, 296.8358775046606297, 11.24705370801146209 ) ) ;
#27695 = CIRCLE ( 'NONE', #87562, 70.00000000000001421 ) ;
#27696 = CARTESIAN_POINT ( 'NONE',  ( 80.86920046867821554, 43.29757878561761686, -9.961566104854268744 ) ) ;
#27697 = DIRECTION ( 'NONE',  ( -0.4999999999999987788, 0.8660254037844392627, 0.000000000000000000 ) ) ;
#27698 = EDGE_CURVE ( 'NONE', #90703, #2331, #11735, .T. ) ;
#27699 = CARTESIAN_POINT ( 'NONE',  ( 13.89683389070260944, 169.6423013555409796, -4.594050593750043987 ) ) ;
#27700 = CARTESIAN_POINT ( 'NONE',  ( 94.81556191316359161, 234.7369531367911009, -4.594050593750048428 ) ) ;
#27701 = CARTESIAN_POINT ( 'NONE',  ( 202.8874463667715133, 279.2356300052831557, -15.29930322226033468 ) ) ;
#27702 = CARTESIAN_POINT ( 'NONE',  ( 36.44700672854521883, 203.3967562850347122, 1.101618078115930403E-13 ) ) ;
#27703 = CARTESIAN_POINT ( 'NONE',  ( 186.4733072505212590, 296.4258963025324078, -7.261958780044511563 ) ) ;
#27704 = DIRECTION ( 'NONE',  ( 1.000000000000000000, 0.000000000000000000, 0.000000000000000000 ) ) ;
#27705 = CARTESIAN_POINT ( 'NONE',  ( 77.43171394984256040, 51.88891212959239851, 15.61825462552096333 ) ) ;
#27706 = CARTESIAN_POINT ( 'NONE',  ( 161.2168897513269314, 281.8122871204358262, 5.602797683376681270 ) ) ;
#27707 = CARTESIAN_POINT ( 'NONE',  ( 147.6512387128590262, 274.9075480792844246, -8.209968531507987777 ) ) ;
#27708 = ADVANCED_FACE ( 'NONE', ( #2261 ), #85910, .F. ) ;
#27709 = CARTESIAN_POINT ( 'NONE',  ( 84.82554225155547556, 50.21385520134798242, 13.77498508261128407 ) ) ;
#27710 = CARTESIAN_POINT ( 'NONE',  ( 82.36670705735998865, 218.3615022471902591, -10.00000000000009592 ) ) ;
#27711 = CARTESIAN_POINT ( 'NONE',  ( 138.9086373102437051, 262.5530062829863027, -4.648177544792955347E-16 ) ) ;
#27712 = LINE ( 'NONE', #36785, #23887 ) ;
#27713 = CARTESIAN_POINT ( 'NONE',  ( 82.55649720842890815, 206.2202760586659167, -5.415160957724236172E-17 ) ) ;
#27714 = CARTESIAN_POINT ( 'NONE',  ( 161.1093323826042933, 251.5974460702646809, -13.93502574894237078 ) ) ;
#27715 = CARTESIAN_POINT ( 'NONE',  ( 163.5420923545723326, 257.9286257799056443, 15.56078752504084761 ) ) ;
#27717 = CARTESIAN_POINT ( 'NONE',  ( 85.83204607333262004, 42.89671213125961913, -1.490302785022404430 ) ) ;
#27716 = CARTESIAN_POINT ( 'NONE',  ( 157.7233946900069839, 257.4620621851055375, 16.86796251324260254 ) ) ;
#27718 = CARTESIAN_POINT ( 'NONE',  ( 75.60765592493140730, 65.32810859375902623, 14.31319638027754237 ) ) ;
#27719 = CARTESIAN_POINT ( 'NONE',  ( 204.6250002032067528, 275.7806821083123623, -12.66782070737391130 ) ) ;
#27720 = CARTESIAN_POINT ( 'NONE',  ( 30.81771801958594281, 39.83396525600392835, -2.839279412974133887 ) ) ;
#27721 = CARTESIAN_POINT ( 'NONE',  ( 192.5076277540105423, 297.2140032159341558, -13.10094381206144298 ) ) ;
#27722 = CARTESIAN_POINT ( 'NONE',  ( 37.37548992677025694, 106.8700141554178913, 59.99999999999999289 ) ) ;
#27723 = VERTEX_POINT ( 'NONE', #15420 ) ;
#27724 = CARTESIAN_POINT ( 'NONE',  ( 19.06802872841732466, 31.98502408145592568, -5.678558825948271327 ) ) ;
#27725 = DIRECTION ( 'NONE',  ( -0.5000000000000016653, 0.8660254037844375974, 0.000000000000000000 ) ) ;
#27726 = DIRECTION ( 'NONE',  ( -0.000000000000000000, -0.000000000000000000, -1.000000000000000000 ) ) ;
#27727 = CARTESIAN_POINT ( 'NONE',  ( 70.92041665751398227, 60.95568174592694533, 14.54198497113668864 ) ) ;
#27729 = EDGE_CURVE ( 'NONE', #70893, #59464, #25280, .T. ) ;
#27728 = CARTESIAN_POINT ( 'NONE',  ( 153.7955429123465763, 266.9533995729482285, 16.35447140258466092 ) ) ;
#27730 = DIRECTION ( 'NONE',  ( -1.000000000000000000, 0.000000000000000000, 0.000000000000000000 ) ) ;
#27731 = CARTESIAN_POINT ( 'NONE',  ( 87.43197870664040749, 44.84778077074484770, -6.629285647492168643 ) ) ;
#27732 = CARTESIAN_POINT ( 'NONE',  ( 126.6061714340150104, 257.2365022471903444, 2.944929066748280225E-16 ) ) ;
#27733 = CARTESIAN_POINT ( 'NONE',  ( -13.11024591527734628, 6.000000000000000000, 32.50000000000000000 ) ) ;
#27734 = CARTESIAN_POINT ( 'NONE',  ( 28.12636825332733537, 17.20801979619929512, -3.090169943749474069 ) ) ;
#27735 = ORIENTED_EDGE ( 'NONE', *, *, #73652, .F. ) ;
#27736 = CARTESIAN_POINT ( 'NONE',  ( 169.5597748164675522, 248.6071028964281027, -1.929381512893630912 ) ) ;
#27737 = ORIENTED_EDGE ( 'NONE', *, *, #1001, .F. ) ;
#27738 = LINE ( 'NONE', #59096, #6225 ) ;
#27739 = CARTESIAN_POINT ( 'NONE',  ( 86.02466929436550913, 43.73270210902676780, 4.814314935600976675 ) ) ;
#27740 = ADVANCED_FACE ( 'NONE', ( #32130 ), #64043, .F. ) ;
#27741 = ORIENTED_EDGE ( 'NONE', *, *, #74460, .F. ) ;
#27742 = CARTESIAN_POINT ( 'NONE',  ( 85.73021612718905260, 42.77422022262896206, 0.5906291777517241881 ) ) ;
#27743 = ORIENTED_EDGE ( 'NONE', *, *, #86488, .F. ) ;
#27744 = CARTESIAN_POINT ( 'NONE',  ( 72.07419404290544662, 71.65773480557935216, 5.498832909113059664 ) ) ;
#27745 = CARTESIAN_POINT ( 'NONE',  ( 205.7101366950456338, 274.3465869426791528, 12.22104789793548818 ) ) ;
#27746 = DIRECTION ( 'NONE',  ( 0.8660254037844384856, 0.5000000000000002220, 3.252519625699449945E-16 ) ) ;
#27747 = CARTESIAN_POINT ( 'NONE',  ( 88.18429177444041045, 44.53138063026126048, -4.871266200417315950 ) ) ;
#27748 = CARTESIAN_POINT ( 'NONE',  ( 80.96506752577832344, 55.91141337780396015, 16.08528190432092231 ) ) ;
#27749 = CARTESIAN_POINT ( 'NONE',  ( 33.49697393745356777, 27.84335787977765264, 9.188101187500006262 ) ) ;
#27750 = DIRECTION ( 'NONE',  ( -0.8082118706970123911, -0.5888918169447047157, 0.000000000000000000 ) ) ;
#27751 = CARTESIAN_POINT ( 'NONE',  ( 164.7832096898899579, 274.5337176909793584, 14.74445750113318532 ) ) ;
#27752 = DIRECTION ( 'NONE',  ( 0.000000000000000000, 0.000000000000000000, 1.000000000000000000 ) ) ;
#27753 = ORIENTED_EDGE ( 'NONE', *, *, #39641, .T. ) ;
#27754 = VECTOR ( 'NONE', #15865, 1000.000000000000000 ) ;
#27755 = ORIENTED_EDGE ( 'NONE', *, *, #4916, .F. ) ;
#27756 = CARTESIAN_POINT ( 'NONE',  ( 182.9676386820643472, 296.0067668443529101, 0.4350290018456622887 ) ) ;
#27758 = CARTESIAN_POINT ( 'NONE',  ( 194.3177355571849318, 294.0788045336591381, -15.93712594727561616 ) ) ;
#27757 = CARTESIAN_POINT ( 'NONE',  ( 163.8147431267737204, 246.9115372060205118, 7.125417796469586840 ) ) ;
#27759 = CARTESIAN_POINT ( 'NONE',  ( 85.81856918057869166, 48.58455003273027017, 12.27698013059672455 ) ) ;
#27760 = CARTESIAN_POINT ( 'NONE',  ( 66.08737768631668530, 68.54322828898675368, -2.301609525100600795 ) ) ;
#27761 = CARTESIAN_POINT ( 'NONE',  ( 188.7214848040405286, 296.7531490838067612, -10.06825767521683801 ) ) ;
#27762 = CARTESIAN_POINT ( 'NONE',  ( 157.5487431480040925, 257.7645675294749594, -18.29554785922338311 ) ) ;
#27763 = CARTESIAN_POINT ( 'NONE',  ( 170.3178023250738420, 289.0326318653803241, -4.561300590322002080 ) ) ;
#27764 = CARTESIAN_POINT ( 'NONE',  ( 78.99848661620951873, 60.24637179098722584, -16.44349368446545867 ) ) ;
#27765 = CARTESIAN_POINT ( 'NONE',  ( 181.8155868826606536, 256.4333448833576767, 5.198317300223314064 ) ) ;
#27766 = CARTESIAN_POINT ( 'NONE',  ( 92.21748570181026139, 233.2369531367911009, -4.594050593750048428 ) ) ;
#27767 = ORIENTED_EDGE ( 'NONE', *, *, #99780, .T. ) ;
#27768 = CARTESIAN_POINT ( 'NONE',  ( 44.18536904650256503, 64.34838820550514527, 177.5919119679930134 ) ) ;
#27769 = CARTESIAN_POINT ( 'NONE',  ( 110.7831656154889259, 244.7677522451419065, -5.000000000000047962 ) ) ;
#27770 = ORIENTED_EDGE ( 'NONE', *, *, #15724, .T. ) ;
#27771 = VERTEX_POINT ( 'NONE', #63039 ) ;
#27772 = CARTESIAN_POINT ( 'NONE',  ( 87.12765551004491726, 46.34683270939126487, -8.629118549295082374 ) ) ;
#27773 = CARTESIAN_POINT ( 'NONE',  ( 72.02063440569831698, 59.20206202002285067, 15.36478115506978881 ) ) ;
#27774 = FACE_OUTER_BOUND ( 'NONE', #79826, .T. ) ;
#27775 = CARTESIAN_POINT ( 'NONE',  ( 17.56085832715719164, 11.10801979619927948, 3.090169943749476733 ) ) ;
#27776 = ADVANCED_FACE ( 'NONE', ( #93982 ), #86400, .T. ) ;
#27777 = CARTESIAN_POINT ( 'NONE',  ( 163.2189713653645242, 247.9434441664957944, 10.97120828841990914 ) ) ;
#27778 = ORIENTED_EDGE ( 'NONE', *, *, #59259, .F. ) ;
#27779 = ADVANCED_FACE ( 'NONE', ( #41224 ), #34153, .T. ) ;
#27780 = ORIENTED_EDGE ( 'NONE', *, *, #34423, .F. ) ;
#27781 = CARTESIAN_POINT ( 'NONE',  ( 182.3700640764176342, 263.2847133751610045, -13.94439451147478337 ) ) ;
#27783 = EDGE_CURVE ( 'NONE', #40696, #15491, #80801, .T. ) ;
#27782 = CARTESIAN_POINT ( 'NONE',  ( 179.9209375999747351, 276.5811748711908535, 17.74520275588677265 ) ) ;
#27784 = ORIENTED_EDGE ( 'NONE', *, *, #34637, .T. ) ;
#27785 = ADVANCED_FACE ( 'NONE', ( #43219 ), #42716, .T. ) ;
#27786 = CARTESIAN_POINT ( 'NONE',  ( 191.5054231872901767, 263.6613473635590594, -8.131552266941017848 ) ) ;
#27787 = CARTESIAN_POINT ( 'NONE',  ( 153.4893010137675731, 265.2713640115015892, 16.29005549651170881 ) ) ;
#27788 = CARTESIAN_POINT ( 'NONE',  ( 83.95007842832860945, 49.47769780624822999, 13.19600533624758043 ) ) ;
#27790 = CYLINDRICAL_SURFACE ( 'NONE', #70625, 10.00000000000010658 ) ;
#27789 = CARTESIAN_POINT ( 'NONE',  ( 125.3701074643745841, 249.3149278399160949, 9.188101187500093303 ) ) ;
#27791 = CARTESIAN_POINT ( 'NONE',  ( 168.2008345946905479, 248.1884056956802453, -5.064766917302788052 ) ) ;
#27792 = EDGE_LOOP ( 'NONE', ( #67631, #22559, #6926, #43034 ) ) ;
#27793 = CARTESIAN_POINT ( 'NONE',  ( 67.12105150802354103, 202.8927522451418213, 10.00000000000009948 ) ) ;
#27794 = CARTESIAN_POINT ( 'NONE',  ( 71.64910063594055600, 63.27319121282799586, 13.65625867040954233 ) ) ;
#27795 = CARTESIAN_POINT ( 'NONE',  ( 82.20602006260367034, 40.68642891347821688, -3.576342120315587181 ) ) ;
#27796 = CARTESIAN_POINT ( 'NONE',  ( 189.6400116240601221, 270.3132688328793733, 14.33464930468576171 ) ) ;
#27797 = CARTESIAN_POINT ( 'NONE',  ( 178.3967306507444164, 285.3765218324597868, 13.04961304002345734 ) ) ;
#27798 = CARTESIAN_POINT ( 'NONE',  ( 76.04745143182429956, 51.22931105158178866, -16.11652841588801621 ) ) ;
#27799 = CARTESIAN_POINT ( 'NONE',  ( 82.18336151548079727, 40.66633616100362758, -3.549285645192841621 ) ) ;
#27800 = DIRECTION ( 'NONE',  ( 1.000000000000000000, 0.000000000000000000, 0.000000000000000000 ) ) ;
#27801 = CARTESIAN_POINT ( 'NONE',  ( 79.67207043538442690, 48.87950828229436695, 14.12217693801051333 ) ) ;
#27802 = EDGE_CURVE ( 'NONE', #17891, #67005, #65046, .T. ) ;
#27803 = CARTESIAN_POINT ( 'NONE',  ( 206.7990506781679301, 271.8220439983479082, 6.357107087294847858 ) ) ;
#27804 = CARTESIAN_POINT ( 'NONE',  ( 19.38736881444313198, 23.14441083166260782, 10.00000000000000533 ) ) ;
#27805 = CARTESIAN_POINT ( 'NONE',  ( 77.67488635742661529, 61.95705115926814699, 15.64220015554268173 ) ) ;
#27806 = CARTESIAN_POINT ( 'NONE',  ( 207.7837159184916231, 270.7550423741513441, -2.369602332675663448 ) ) ;
#27807 = CARTESIAN_POINT ( 'NONE',  ( 69.16577226868226091, 70.40701545813222140, -2.181849231202375172 ) ) ;
#27808 = CARTESIAN_POINT ( 'NONE',  ( 80.87517248313827167, 58.64441083166272506, 0.000000000000000000 ) ) ;
#27809 = CARTESIAN_POINT ( 'NONE',  ( 67.66477494612622934, 65.93994996590180335, 10.43000742999573482 ) ) ;
#27810 = CARTESIAN_POINT ( 'NONE',  ( 27.96887745124769253, 39.08080186712594895, -3.090169943749475845 ) ) ;
#27811 = CYLINDRICAL_SURFACE ( 'NONE', #44956, 17.82106496071139645 ) ;
#27812 = CARTESIAN_POINT ( 'NONE',  ( -44.26501565779586400, 27.25709555612339230, 10.00000000000000000 ) ) ;
#27813 = CARTESIAN_POINT ( 'NONE',  ( 157.7229324233670980, 270.7041103179763581, -15.79028221516555419 ) ) ;
#27814 = CARTESIAN_POINT ( 'NONE',  ( 82.44511272049554407, 43.20545074304087052, -7.784461827744890705 ) ) ;
#27815 = CARTESIAN_POINT ( 'NONE',  ( 17.60459192459599365, 168.7202760586659736, -5.415160957724236172E-17 ) ) ;
#27816 = CARTESIAN_POINT ( 'NONE',  ( 48.91560817564824504, 80.00000000000000000, 54.99999999999999289 ) ) ;
#27817 = ORIENTED_EDGE ( 'NONE', *, *, #23575, .T. ) ;
#27818 = B_SPLINE_CURVE_WITH_KNOTS ( 'NONE', 3,
 ( #81752, #75127, #67497, #74134, #66509, #29020, #19451, #97435, #81260, #28005, #91838 ),
 .UNSPECIFIED., .F., .F.,
 ( 4, 2, 2, 2, 1, 4 ),
 ( 0.7748794552007052250, 0.8311595914005293073, 0.8874397276003532786, 0.9155797957002653753, 0.9437198638001773610, 1.000000000000000000 ),
 .UNSPECIFIED. ) ;
#27819 = CARTESIAN_POINT ( 'NONE',  ( 86.96880057233924788, 46.02321981727299516, 8.968744825131210519 ) ) ;
#27820 = CARTESIAN_POINT ( 'NONE',  ( 202.4677460062568173, 269.8620261455625950, 8.891765442197028690 ) ) ;
#27821 = CARTESIAN_POINT ( 'NONE',  ( 72.13778271599493053, 72.31753100054153549, -1.256476775470434237 ) ) ;
#27822 = CARTESIAN_POINT ( 'NONE',  ( 45.37135788555205096, 190.8768266524160140, 9.188101187500096856 ) ) ;
#27823 = EDGE_CURVE ( 'NONE', #55188, #69106, #22065, .T. ) ;
#27824 = CARTESIAN_POINT ( 'NONE',  ( 86.82393771405537564, 45.90093866298671799, 8.916403221032373594 ) ) ;
#27825 = CARTESIAN_POINT ( 'NONE',  ( 170.8524479326273138, 287.4302738079429673, 7.076016408304939276 ) ) ;
#27826 = CARTESIAN_POINT ( 'NONE',  ( 190.1858949294064871, 301.2353624297489887, -5.249932979468886707 ) ) ;
#27827 = CARTESIAN_POINT ( 'NONE',  ( 38.19650550196953986, 40.79103043416552765, 8.090169943749478065 ) ) ;
#27828 = CARTESIAN_POINT ( 'NONE',  ( 81.38228331512368641, 42.18052851754683275, 8.075145019496556387 ) ) ;
#27829 = CARTESIAN_POINT ( 'NONE',  ( 146.5502055023624735, 276.8145935406849389, 0.3770461397900869427 ) ) ;
#27830 = CARTESIAN_POINT ( 'NONE',  ( 176.4362609909801165, 275.0927880625443436, 17.39602988701090780 ) ) ;
#27831 = CARTESIAN_POINT ( 'NONE',  ( -15.18581709147259140, 60.13231987269209355, -10.00000000000000000 ) ) ;
#27832 = CARTESIAN_POINT ( 'NONE',  ( 68.09634862398104360, 67.84148155887413623, -7.379325992333486184 ) ) ;
#27833 = CARTESIAN_POINT ( 'NONE',  ( 166.8557127037659882, 257.9341067576638125, -15.25166664705231589 ) ) ;
#27834 = CARTESIAN_POINT ( 'NONE',  ( -22.42236680055709641, 157.8615022471902591, 0.000000000000000000 ) ) ;
#27835 = CARTESIAN_POINT ( 'NONE',  ( 85.03695205236195420, 233.2365022471903160, 2.944929066748280225E-16 ) ) ;
#27836 = CARTESIAN_POINT ( 'NONE',  ( 15.67199189347853761, 32.63213790969698636, -10.00000000000000000 ) ) ;
#27837 = CARTESIAN_POINT ( 'NONE',  ( 161.5877803775636039, 267.7196290107671075, -17.14067319960231472 ) ) ;
#27838 = VERTEX_POINT ( 'NONE', #72676 ) ;
#27839 = CARTESIAN_POINT ( 'NONE',  ( 62.15025298811053034, 212.8149278399160949, -9.188101187500095079 ) ) ;
#27840 = ORIENTED_EDGE ( 'NONE', *, *, #22388, .F. ) ;
#27841 = CARTESIAN_POINT ( 'NONE',  ( 162.7710398924988908, 263.3845876204081833, 17.15398367141938962 ) ) ;
#27842 = CARTESIAN_POINT ( 'NONE',  ( 162.1795029284002112, 250.7317292623248477, 12.60364379007453550 ) ) ;
#27843 = CARTESIAN_POINT ( 'NONE',  ( 67.60658015080353778, 66.82409088742160463, -8.485143750796469320 ) ) ;
#27844 = VERTEX_POINT ( 'NONE', #74161 ) ;
#27845 = CARTESIAN_POINT ( 'NONE',  ( 171.0113606419460837, 287.1407938163278573, 8.604837063268337971 ) ) ;
#27846 = CARTESIAN_POINT ( 'NONE',  ( 164.6460902696047128, 245.4716017159096566, -3.036414139157908476 ) ) ;
#27847 = DIRECTION ( 'NONE',  ( -0.000000000000000000, -0.000000000000000000, -1.000000000000000000 ) ) ;
#27848 = CARTESIAN_POINT ( 'NONE',  ( 28.60632300232807879, 31.91421378149921040, 9.188101187500008038 ) ) ;
#27849 = CARTESIAN_POINT ( 'NONE',  ( 189.7726967107949747, 264.4065126852114531, 11.24316165915873000 ) ) ;
#27850 = CARTESIAN_POINT ( 'NONE',  ( 181.1477013271936016, 287.8971774238942203, -14.15342935774602218 ) ) ;
#27851 = CARTESIAN_POINT ( 'NONE',  ( 171.3515257658276028, 255.7365519920522559, 11.37700587845633748 ) ) ;
#27853 = ORIENTED_EDGE ( 'NONE', *, *, #35519, .F. ) ;
#27852 = AXIS2_PLACEMENT_3D ( 'NONE', #27733, #26729, #18136 ) ;
#27854 = CARTESIAN_POINT ( 'NONE',  ( 14.59716579798650571, 20.37878583063839955, 9.188101187500006262 ) ) ;
#27855 = CARTESIAN_POINT ( 'NONE',  ( 29.35192616055884685, 22.11029122506295863, -8.090169943749478065 ) ) ;
#27856 = CARTESIAN_POINT ( 'NONE',  ( 171.8160532838503514, 252.3804680471336610, 8.773019167658075546 ) ) ;
#27857 = CARTESIAN_POINT ( 'NONE',  ( 11.62691283633230377, 30.21091486745859811, -1.111400068045478839E-16 ) ) ;
#27858 = ORIENTED_EDGE ( 'NONE', *, *, #1639, .T. ) ;
#27859 = CARTESIAN_POINT ( 'NONE',  ( 181.9839621645596992, 283.9156450579300213, 14.95553656096354622 ) ) ;
#27860 = CARTESIAN_POINT ( 'NONE',  ( 151.4281781455628675, 268.3656970847310390, 15.24742929158552585 ) ) ;
#27861 = FACE_OUTER_BOUND ( 'NONE', #50782, .T. ) ;
#27862 = VERTEX_POINT ( 'NONE', #96988 ) ;
#27863 = VERTEX_POINT ( 'NONE', #2770 ) ;
#27865 = CARTESIAN_POINT ( 'NONE',  ( 61.87308422990769685, 194.9824982072973967, 3.021315404115420679E-15 ) ) ;
#27864 = CARTESIAN_POINT ( 'NONE',  ( 207.6129110656513035, 271.0508850574501025, -5.265106572941297358 ) ) ;
#27866 = CARTESIAN_POINT ( 'NONE',  ( 196.5806080813426888, 290.1593943507663766, -16.31912166233602690 ) ) ;
#27867 = VERTEX_POINT ( 'NONE', #89401 ) ;
#27868 = CARTESIAN_POINT ( 'NONE',  ( 65.83016338625502328, 68.95036046686468012, -2.295610735544858283 ) ) ;
#27869 = CARTESIAN_POINT ( 'NONE',  ( 8.106622824862185439, 30.17147933776455204, 10.00000000000000000 ) ) ;
#27870 = DIRECTION ( 'NONE',  ( -0.000000000000000000, 0.000000000000000000, 1.000000000000000000 ) ) ;
#27871 = CARTESIAN_POINT ( 'NONE',  ( 78.15719359349522222, 61.55473184547404486, -16.14768920957587284 ) ) ;
#27872 = CARTESIAN_POINT ( 'NONE',  ( 114.4365367415960293, 243.0024278399160949, -9.188101187500093303 ) ) ;
#27873 = CARTESIAN_POINT ( 'NONE',  ( 120.5439936075240155, 233.7365022471902307, 10.00000000000009948 ) ) ;
#27874 = CARTESIAN_POINT ( 'NONE',  ( 199.5442653985851962, 283.0261893010793415, -17.63221794778640117 ) ) ;
#27875 = VERTEX_POINT ( 'NONE', #57430 ) ;
#27876 = CARTESIAN_POINT ( 'NONE',  ( 208.3132655666949233, 269.8378354783333180, 2.688523655043302707 ) ) ;
#27877 = ORIENTED_EDGE ( 'NONE', *, *, #80048, .F. ) ;
#27878 = ORIENTED_EDGE ( 'NONE', *, *, #38592, .F. ) ;
#27879 = FACE_BOUND ( 'NONE', #47778, .T. ) ;
#27880 = LINE ( 'NONE', #5577, #66069 ) ;
#27881 = CARTESIAN_POINT ( 'NONE',  ( 78.41572647264329987, 206.8923013555409796, 4.594050593750050204 ) ) ;
#27882 = LINE ( 'NONE', #4588, #96732 ) ;
#27883 = FACE_OUTER_BOUND ( 'NONE', #37070, .T. ) ;
#27884 = CARTESIAN_POINT ( 'NONE',  ( 198.7076130252130497, 286.4753137200327728, 17.36142183403824291 ) ) ;
#27885 = EDGE_CURVE ( 'NONE', #68960, #96482, #42755, .T. ) ;
#27886 = CARTESIAN_POINT ( 'NONE',  ( 175.5746833524315775, 278.5347786252573314, 16.94864957847115505 ) ) ;
#27887 = ORIENTED_EDGE ( 'NONE', *, *, #9111, .T. ) ;
#27888 = EDGE_CURVE ( 'NONE', #36836, #85089, #3757, .T. ) ;
#27889 = CARTESIAN_POINT ( 'NONE',  ( 72.50276366761895019, 63.69479216147543355, -13.71156667146904340 ) ) ;
#27890 = FACE_OUTER_BOUND ( 'NONE', #17340, .T. ) ;
#27891 = CARTESIAN_POINT ( 'NONE',  ( 66.18968672761215544, 68.49487770601442094, -4.881532527435783919 ) ) ;
#27892 = ORIENTED_EDGE ( 'NONE', *, *, #61047, .F. ) ;
#27893 = DIRECTION ( 'NONE',  ( -1.000000000000000000, 0.000000000000000000, 0.000000000000000000 ) ) ;
#27894 = CARTESIAN_POINT ( 'NONE',  ( 207.4541616930702617, 271.3258470364304458, -6.834942797545373594 ) ) ;
#27895 = EDGE_CURVE ( 'NONE', #312, #64387, #12325, .T. ) ;
#27896 = CARTESIAN_POINT ( 'NONE',  ( 192.5076277540105423, 297.2140032159341558, -13.10094381206144298 ) ) ;
#27897 = CARTESIAN_POINT ( 'NONE',  ( 172.6505904036989136, 280.8448313155626579, -15.39888677054324440 ) ) ;
#27898 = DIRECTION ( 'NONE',  ( 0.000000000000000000, -0.000000000000000000, 1.000000000000000000 ) ) ;
#27899 = SURFACE_STYLE_USAGE ( .BOTH. , #50691 ) ;
#27900 = CARTESIAN_POINT ( 'NONE',  ( 82.41914487369291464, 41.31337197830497132, 3.340431838514237750 ) ) ;
#27901 = CARTESIAN_POINT ( 'NONE',  ( 127.4269177983626236, 250.5024278399160949, -9.188101187500093303 ) ) ;
#27902 = ORIENTED_EDGE ( 'NONE', *, *, #34818, .F. ) ;
#27903 = CARTESIAN_POINT ( 'NONE',  ( 146.5865263025993954, 276.7516840693029962, 0.4918294119671828835 ) ) ;
#27904 = CARTESIAN_POINT ( 'NONE',  ( 85.88757390701229610, 44.14475701618168557, 5.957954596235570222 ) ) ;
#27905 = CARTESIAN_POINT ( 'NONE',  ( 198.8081898473356262, 282.3983615885804284, -17.60554210735202574 ) ) ;
#27906 = CARTESIAN_POINT ( 'NONE',  ( 79.28658851328975743, 59.85324873312088556, -16.14828164407633082 ) ) ;
#27907 = CARTESIAN_POINT ( 'NONE',  ( 74.20275025028655591, 58.27827946831821748, 15.87466641876757478 ) ) ;
#27908 = CARTESIAN_POINT ( 'NONE',  ( 178.6317619811870259, 253.9327355832967612, -4.167451725846189170 ) ) ;
#27909 = ORIENTED_EDGE ( 'NONE', *, *, #67258, .T. ) ;
#27910 = CARTESIAN_POINT ( 'NONE',  ( 28.46864935082048831, 149.7156766241961350, -21.50000000000001421 ) ) ;
#27911 = CARTESIAN_POINT ( 'NONE',  ( 120.6702889753612737, 247.1427522451419350, 10.00000000000009415 ) ) ;
#27912 = CARTESIAN_POINT ( 'NONE',  ( 167.4764150005448755, 249.1180365860762720, -5.480813618351669803 ) ) ;
#27913 = CARTESIAN_POINT ( 'NONE',  ( 205.9252530167937323, 273.9739945438741984, -10.37964514155334328 ) ) ;
#27914 = CARTESIAN_POINT ( 'NONE',  ( 202.6109660208213086, 267.6076335798982200, 0.8660040287496835187 ) ) ;
#27915 = CARTESIAN_POINT ( 'NONE',  ( 190.1752790837055045, 301.2537496138681945, -5.177773110520776711 ) ) ;
#27916 = CARTESIAN_POINT ( 'NONE',  ( -71.61465314115659453, 63.06504152958490295, 45.00000000000001421 ) ) ;
#27917 = VECTOR ( 'NONE', #43934, 1000.000000000000000 ) ;
#27918 = DIRECTION ( 'NONE',  ( 0.2639761180675095353, -0.9645292162967424865, 0.000000000000000000 ) ) ;
#27919 = CIRCLE ( 'NONE', #81420, 15.60714546451156970 ) ;
#27920 = B_SPLINE_SURFACE_WITH_KNOTS ( 'NONE', 3, 1, ( 
 ( #41688, #72631 ),
 ( #24498, #1723 ),
 ( #75111, #98410 ),
 ( #28483, #89836 ),
 ( #88872, #74114 ),
 ( #20919, #4190 ),
 ( #34596, #42676 ),
 ( #73125, #5686 ),
 ( #90843, #66492 ),
 ( #29004, #58868 ),
 ( #49797, #42190 ),
 ( #20411, #11331 ),
 ( #3716, #6185 ),
 ( #37566, #60857 ),
 ( #91321, #68971 ),
 ( #52767, #14289 ),
 ( #46672, #91822 ),
 ( #77598, #45663 ),
 ( #99894, #84720 ),
 ( #15261, #46156 ),
 ( #77074, #7681 ),
 ( #90, #23366 ),
 ( #54250, #24875 ),
 ( #93825, #41058 ),
 ( #70472, #71502 ),
 ( #9705, #1087 ),
 ( #49192, #32972 ),
 ( #16772, #55749 ),
 ( #87757, #86741 ),
 ( #48179, #31965 ),
 ( #80128, #34005 ),
 ( #10689, #41568 ),
 ( #93312, #16274 ),
 ( #47169, #65866 ) ),
 .UNSPECIFIED., .T., .F., .F.,
 ( 4, 2, 2, 2, 2, 2, 2, 2, 2, 2, 2, 2, 2, 2, 2, 2, 4 ),
 ( 2, 2 ),
 ( 0.000000000000000000, 0.06250000000000000000, 0.1250000000000000000, 0.1875000000000000000, 0.2500000000000000000, 0.3125000000000000000, 0.3750000000000000000, 0.4375000000000000000, 0.5000000000000000000, 0.5625000000000000000, 0.6250000000000000000, 0.6875000000000000000, 0.7500000000000000000, 0.8125000000000000000, 0.8750000000000000000, 0.9375000000000000000, 1.000000000000000000 ),
 ( 0.000000000000000000, 1.000000000000000000 ),
 .UNSPECIFIED. ) ;
#27921 = CARTESIAN_POINT ( 'NONE',  ( 11.41020553640983515, 28.36126292948894800, 6.180339887498949913 ) ) ;
#27922 = CARTESIAN_POINT ( 'NONE',  ( 190.6023073677431512, 300.5141149296460981, 3.174888932019753973 ) ) ;
#27923 = DIRECTION ( 'NONE',  ( 0.000000000000000000, -1.000000000000000000, 0.000000000000000000 ) ) ;
#27924 = LINE ( 'NONE', #58807, #61254 ) ;
#27925 = CARTESIAN_POINT ( 'NONE',  ( 155.1601726304954809, 261.9016930232608615, -18.56587418422714464 ) ) ;
#27926 = CARTESIAN_POINT ( 'NONE',  ( 149.0237174825091415, 274.5263358477994871, 9.114370506038131481 ) ) ;
#27927 = CARTESIAN_POINT ( 'NONE',  ( 135.5370584069941913, 242.3927522451417929, -10.00000000000009059 ) ) ;
#27928 = CARTESIAN_POINT ( 'NONE',  ( 172.4401916400875621, 283.6719894713717167, -12.41194507545851522 ) ) ;
#27929 = ORIENTED_EDGE ( 'NONE', *, *, #62397, .F. ) ;
#27930 = CARTESIAN_POINT ( 'NONE',  ( 66.60661563005250230, 67.77273566384381809, -7.043189648893246613 ) ) ;
#27931 = CARTESIAN_POINT ( 'NONE',  ( 151.1126408083691501, 268.9122237844355254, -15.82705194100464396 ) ) ;
#27932 = CARTESIAN_POINT ( 'NONE',  ( -5.021015940802495692, 180.1589784336661637, -6.496448406907676862E-16 ) ) ;
#27933 = B_SPLINE_CURVE_WITH_KNOTS ( 'NONE', 3,
 ( #23413, #29538, #67530, #61911 ),
 .UNSPECIFIED., .F., .F.,
 ( 4, 4 ),
 ( 0.009408440947594234535, 0.01495930912883047283 ),
 .UNSPECIFIED. ) ;
#27934 = ADVANCED_FACE ( 'NONE', ( #95509 ), #56930, .F. ) ;
#27935 = CARTESIAN_POINT ( 'NONE',  ( 53.97765888354242492, 189.7202760586659736, -5.415160957724236172E-17 ) ) ;
#27936 = CARTESIAN_POINT ( 'NONE',  ( 85.25467255710213976, 43.90411826015589725, 7.227896802836702328 ) ) ;
#27937 = CARTESIAN_POINT ( 'NONE',  ( 33.14255420672135699, 18.94473085651394229, 1.475505719884397138E-15 ) ) ;
#27938 = CARTESIAN_POINT ( 'NONE',  ( 85.18660547738458888, 49.05202258069147803, 12.45721658011292732 ) ) ;
#27939 = CARTESIAN_POINT ( 'NONE',  ( 204.9184781223158609, 275.7177798128946620, -12.59106622113254126 ) ) ;
#27940 = CARTESIAN_POINT ( 'NONE',  ( 192.4205004985176402, 292.7214258041265680, -14.22339032255528757 ) ) ;
#27941 = CARTESIAN_POINT ( 'NONE',  ( 74.01103629804136119, 55.46278365816274913, -16.11564949998087215 ) ) ;
#27942 = CARTESIAN_POINT ( 'NONE',  ( 167.8546155174443015, 256.7248629110974889, 13.70153385259920142 ) ) ;
#27943 = CARTESIAN_POINT ( 'NONE',  ( 77.12260313221874242, 61.62046618767455186, 16.01160934822282655 ) ) ;
#27944 = CARTESIAN_POINT ( 'NONE',  ( 198.0788209437629916, 287.5644135525011507, 18.31867165462247726 ) ) ;
#27945 = ADVANCED_FACE ( 'NONE', ( #57935 ), #7570, .F. ) ;
#27946 = CARTESIAN_POINT ( 'NONE',  ( 47.79785968963118137, 191.7365022471902307, 10.00000000000009592 ) ) ;
#27947 = CYLINDRICAL_SURFACE ( 'NONE', #50617, 17.82106496071139645 ) ;
#27948 = CARTESIAN_POINT ( 'NONE',  ( 189.8136646974935786, 301.8800841035353528, -0.6430783927310335102 ) ) ;
#27949 = CARTESIAN_POINT ( 'NONE',  ( 20.25662117580333188, 176.3768266524159856, -9.188101187500091527 ) ) ;
#27950 = CARTESIAN_POINT ( 'NONE',  ( 72.82118101371949592, 71.12637341421533677, -7.461520388884603783 ) ) ;
#27951 = EDGE_CURVE ( 'NONE', #73044, #40898, #74215, .T. ) ;
#27952 = CARTESIAN_POINT ( 'NONE',  ( 79.06624833104577021, 60.08073726494826161, 16.12333911585958290 ) ) ;
#27953 = CARTESIAN_POINT ( 'NONE',  ( 27.35361640444819287, 37.83396525600391413, -2.839279412974133887 ) ) ;
#27954 = CARTESIAN_POINT ( 'NONE',  ( 157.0239713899953244, 269.7369771206523978, 16.31777668093047851 ) ) ;
#27955 = CARTESIAN_POINT ( 'NONE',  ( 182.9121110983079745, 278.7409904731791244, 16.73155022942700398 ) ) ;
#27956 = CARTESIAN_POINT ( 'NONE',  ( 193.8603219414924013, 294.8710681561126989, 15.36476279452078586 ) ) ;
#27957 = CARTESIAN_POINT ( 'NONE',  ( 115.2756724011686202, 247.3615022471903160, 5.000000000000046185 ) ) ;
#27958 = CARTESIAN_POINT ( 'NONE',  ( 176.8095048781594869, 260.7838774868672544, -13.17535878752048539 ) ) ;
#27959 = CARTESIAN_POINT ( 'NONE',  ( 17.47068606603513530, 15.80170272979925628, 7.433330006724137462 ) ) ;
#27960 = CARTESIAN_POINT ( 'NONE',  ( 43.25185672232382217, 62.35734246106903811, 177.5919119679930134 ) ) ;
#27961 = CARTESIAN_POINT ( 'NONE',  ( 82.38367100173057622, 53.80119691343342225, 15.85271891126490829 ) ) ;
#27962 = CARTESIAN_POINT ( 'NONE',  ( -76.23101443460924997, 54.01191295053621388, -10.00000000000000000 ) ) ;
#27963 = LINE ( 'NONE', #20386, #87279 ) ;
#27964 = ORIENTED_EDGE ( 'NONE', *, *, #57179, .F. ) ;
#27965 = CARTESIAN_POINT ( 'NONE',  ( 156.8525332442023341, 276.4918820038299714, 10.31694992604559324 ) ) ;
#27966 = CARTESIAN_POINT ( 'NONE',  ( 75.02124847967681376, 53.56804290023246296, -16.54202287972591279 ) ) ;
#27967 = DIRECTION ( 'NONE',  ( -0.000000000000000000, -1.000000000000000000, -0.000000000000000000 ) ) ;
#27968 = CARTESIAN_POINT ( 'NONE',  ( 166.5483893385236627, 250.3327489066329292, -10.49964665769386762 ) ) ;
#27969 = EDGE_LOOP ( 'NONE', ( #15187, #83211, #77055, #82360 ) ) ;
#27970 = CARTESIAN_POINT ( 'NONE',  ( 192.1883190596398094, 297.7670620978826150, 12.41391288785556668 ) ) ;
#27971 = CARTESIAN_POINT ( 'NONE',  ( 82.76646413971928951, 40.58977954809799371, 0.9263384072861480245 ) ) ;
#27972 = B_SPLINE_CURVE_WITH_KNOTS ( 'NONE', 3,
 ( #85323, #46777, #29586, #7272, #53374, #76684, #77700, #23970, #39149, #16378, #6785, #70062, #91417, #47269, #680, #31561 ),
 .UNSPECIFIED., .F., .F.,
 ( 4, 2, 2, 2, 2, 2, 2, 4 ),
 ( 3.103167691559091397E-17, 0.0005277448334066532805, 0.0007916172501099130255, 0.001055489666813172987, 0.001319362083516432624, 0.001583234500219692477, 0.001847106916922952331, 0.002110979333626212401 ),
 .UNSPECIFIED. ) ;
#27973 = CARTESIAN_POINT ( 'NONE',  ( 66.57026871552700698, 68.76443072711541049, 4.738950751824671848 ) ) ;
#27974 = CARTESIAN_POINT ( 'NONE',  ( 155.5211745099813356, 261.2764194263634749, -17.18163098020766810 ) ) ;
#27975 = ORIENTED_EDGE ( 'NONE', *, *, #85928, .F. ) ;
#27976 =( BOUNDED_CURVE ( )  B_SPLINE_CURVE ( 2, ( #83754, #39082, #45687, #15796, #61889, #92840, #14315, #23391, #45202 ),
 .UNSPECIFIED., .F., .T. ) 
 B_SPLINE_CURVE_WITH_KNOTS ( ( 3, 2, 2, 2, 3 ),
 ( 0.6491935483870967527, 0.6505376344086021279, 0.6532258064516128782, 0.6559139784946236285, 0.6572580645161290036 ),
 .UNSPECIFIED. ) 
 CURVE ( )  GEOMETRIC_REPRESENTATION_ITEM ( )  RATIONAL_B_SPLINE_CURVE ( ( 0.9330127018922194093, 0.9330127018922194093, 1.000000000000000000, 0.8660254037844387076, 1.000000000000000000, 0.8660254037844387076, 1.000000000000000000, 0.9330127018922194093, 0.9330127018922194093 ) ) 
 REPRESENTATION_ITEM ( '' )  );
#27977 = ORIENTED_EDGE ( 'NONE', *, *, #71624, .F. ) ;
#27978 = CARTESIAN_POINT ( 'NONE',  ( 159.1344352748853055, 279.7114264697810313, -10.00621538743078354 ) ) ;
#27979 = CARTESIAN_POINT ( 'NONE',  ( 153.2712411579340426, 265.1734183057532732, 16.26687330118495467 ) ) ;
#27980 = EDGE_LOOP ( 'NONE', ( #91384, #61472, #12594, #18279 ) ) ;
#27981 = CARTESIAN_POINT ( 'NONE',  ( 87.98594423550160570, 43.75089820288621212, -2.253463800273092676 ) ) ;
#27982 = CARTESIAN_POINT ( 'NONE',  ( 80.34499676519902778, 57.43793486056498665, -16.58883017036144381 ) ) ;
#27983 = CARTESIAN_POINT ( 'NONE',  ( 178.2874402213737710, 264.0549037780814388, 14.92174102309952133 ) ) ;
#27984 = ORIENTED_EDGE ( 'NONE', *, *, #95033, .F. ) ;
#27985 = CARTESIAN_POINT ( 'NONE',  ( -28.04097607764120781, 24.82386083235215679, 10.00000000000000000 ) ) ;
#27986 = CARTESIAN_POINT ( 'NONE',  ( 83.44610441601685125, 48.89063263195148323, -12.98306697336452409 ) ) ;
#27987 = B_SPLINE_CURVE_WITH_KNOTS ( 'NONE', 3,
 ( #26787, #90630, #61158, #15547 ),
 .UNSPECIFIED., .F., .F.,
 ( 4, 4 ),
 ( 0.02131823508248953739, 0.02883180965995480252 ),
 .UNSPECIFIED. ) ;
#27988 = AXIS2_PLACEMENT_3D ( 'NONE', #91920, #45753, #94279 ) ;
#27989 = CARTESIAN_POINT ( 'NONE',  ( 81.22596495421952056, 43.17011023298827865, 9.564257120711848970 ) ) ;
#27990 = ORIENTED_EDGE ( 'NONE', *, *, #7917, .T. ) ;
#27991 = CARTESIAN_POINT ( 'NONE',  ( 160.1969820541083607, 255.1776831935258372, -16.37528374203482073 ) ) ;
#27992 = CARTESIAN_POINT ( 'NONE',  ( 164.3090168944849836, 246.0554299274959931, 2.641760039552302430 ) ) ;
#27993 = CARTESIAN_POINT ( 'NONE',  ( 73.73381220379675938, 59.87433565520142764, 15.47193064673703411 ) ) ;
#27994 = ORIENTED_EDGE ( 'NONE', *, *, #95052, .F. ) ;
#27995 = EDGE_CURVE ( 'NONE', #55869, #67607, #25289, .T. ) ;
#27996 = CARTESIAN_POINT ( 'NONE',  ( 174.5846041374311710, 276.7874870096778182, -16.75558966740674549 ) ) ;
#27997 = CARTESIAN_POINT ( 'NONE',  ( 172.3600888395878314, 263.7131837874231337, -15.46760836022099994 ) ) ;
#27998 = VECTOR ( 'NONE', #54214, 1000.000000000000000 ) ;
#27999 = ORIENTED_EDGE ( 'NONE', *, *, #58548, .F. ) ;
#28000 = FACE_OUTER_BOUND ( 'NONE', #12954, .T. ) ;
#28001 = ORIENTED_EDGE ( 'NONE', *, *, #15771, .T. ) ;
#28002 = CARTESIAN_POINT ( 'NONE',  ( 149.7854447168632817, 277.1467554076948545, 4.663160563959508842 ) ) ;
#28003 = ORIENTED_EDGE ( 'NONE', *, *, #36446, .T. ) ;
#28004 = CARTESIAN_POINT ( 'NONE',  ( 156.4811347401371506, 266.4657705092222386, -16.23271684233645118 ) ) ;
#28005 = CARTESIAN_POINT ( 'NONE',  ( 88.14265167143706492, 44.20527097481110701, 1.888012356971680683 ) ) ;
#28006 = LINE ( 'NONE', #21897, #16936 ) ;
#28007 = CARTESIAN_POINT ( 'NONE',  ( 61.15274061880273848, 58.80466486950705729, 0.000000000000000000 ) ) ;
#28008 = CARTESIAN_POINT ( 'NONE',  ( 15.05724179552094277, 20.64441083166259716, -10.00000000000000533 ) ) ;
#28009 = CARTESIAN_POINT ( 'NONE',  ( 153.3127735718713609, 265.1014820546527631, 17.57722645152040641 ) ) ;
#28010 = CARTESIAN_POINT ( 'NONE',  ( 178.1892993710524138, 292.1905823108662617, 7.166771068777840092 ) ) ;
#28011 = EDGE_CURVE ( 'NONE', #2192, #62885, #94881, .T. ) ;
#28012 = CARTESIAN_POINT ( 'NONE',  ( 158.8791574486372440, 255.4602223656619628, -17.57574691297732272 ) ) ;
#28013 = AXIS2_PLACEMENT_3D ( 'NONE', #95170, #58113, #89094 ) ;
#28014 = EDGE_LOOP ( 'NONE', ( #24268, #73733, #50798, #36932 ) ) ;
#28015 = DIRECTION ( 'NONE',  ( -0.1710100716628374096, 0.2961981327260301833, 0.9396926207859057634 ) ) ;
#28016 = CARTESIAN_POINT ( 'NONE',  ( 165.0308887387863876, 244.8051112166122891, 1.948365933089477808 ) ) ;
#28017 = CARTESIAN_POINT ( 'NONE',  ( 206.4695239676918845, 273.0312896038346366, 10.41704154450801667 ) ) ;
#28019 = ORIENTED_EDGE ( 'NONE', *, *, #54249, .F. ) ;
#28018 = CARTESIAN_POINT ( 'NONE',  ( 58.43017357788679789, 217.8207943907112849, 17.47570218321536117 ) ) ;
#28020 = CARTESIAN_POINT ( 'NONE',  ( -17.42236680055705023, 149.2012482093457777, 0.000000000000000000 ) ) ;
#28021 = CARTESIAN_POINT ( 'NONE',  ( 177.2307473631791765, 288.8998395665854559, -9.216979198774193804 ) ) ;
#28022 = ORIENTED_EDGE ( 'NONE', *, *, #18143, .F. ) ;
#28023 = CARTESIAN_POINT ( 'NONE',  ( 81.74830055843420951, 52.20847043234677187, -15.07709221969326308 ) ) ;
#28024 = CARTESIAN_POINT ( 'NONE',  ( 87.62133583293774564, 45.31115884160845297, -7.293173845241971875 ) ) ;
#28025 = CARTESIAN_POINT ( 'NONE',  ( 126.9410149175250524, 232.5494855054051868, -2.679491924311248496 ) ) ;
#28026 = CARTESIAN_POINT ( 'NONE',  ( 160.6612659640541381, 252.3735198723586848, -15.60644164121982591 ) ) ;
#28027 = CARTESIAN_POINT ( 'NONE',  ( 190.3150247411125804, 301.0117030351020730, 0.1088388511812921067 ) ) ;
#28028 = ORIENTED_EDGE ( 'NONE', *, *, #62275, .F. ) ;
#28029 = CARTESIAN_POINT ( 'NONE',  ( 170.5392822398632404, 255.6756181042317735, -11.78486988674311675 ) ) ;
#28030 = CARTESIAN_POINT ( 'NONE',  ( 191.4420812244453600, 260.8157448279923187, -1.331758356259544085 ) ) ;
#28031 = CARTESIAN_POINT ( 'NONE',  ( 52.48883062679681899, 211.1115022471903444, -5.000000000000047962 ) ) ;
#28032 = CARTESIAN_POINT ( 'NONE',  ( 164.2600772519394923, 246.1401958748887182, -2.110785484364219311 ) ) ;
#28033 = CARTESIAN_POINT ( 'NONE',  ( 27.13954536664190798, 193.1427522451419065, 10.00000000000009237 ) ) ;
#28034 = CARTESIAN_POINT ( 'NONE',  ( 108.7534185771431510, 233.5958772461660260, -9.188101187500095079 ) ) ;
#28035 = CARTESIAN_POINT ( 'NONE',  ( 183.5623937226978057, 296.1742073513109403, -2.708913905850958148 ) ) ;
#28036 = CARTESIAN_POINT ( 'NONE',  ( 164.0485396284991850, 280.4819838086867776, -11.53262238567191211 ) ) ;
#28037 = CARTESIAN_POINT ( 'NONE',  ( 6.599962460801562791, 15.76159833115048770, -9.594050593750004907 ) ) ;
#28038 = CARTESIAN_POINT ( 'NONE',  ( 208.2726345668874615, 269.9082104343620472, 2.818736869262927769 ) ) ;
#28039 = CARTESIAN_POINT ( 'NONE',  ( 41.04123086662985997, 188.3768266524159856, -9.188101187500091527 ) ) ;
#28040 = CARTESIAN_POINT ( 'NONE',  ( 173.3507806980417456, 251.4055554679256375, 5.750257727834116039 ) ) ;
#28041 = EDGE_LOOP ( 'NONE', ( #2086, #88018, #73753, #96006 ) ) ;
#28042 = ORIENTED_EDGE ( 'NONE', *, *, #83409, .T. ) ;
#28043 = CARTESIAN_POINT ( 'NONE',  ( 190.8089377949079903, 299.1047931790669736, 7.367255922332321738 ) ) ;
#28044 = CARTESIAN_POINT ( 'NONE',  ( 74.46528254340208264, 68.13939222454926892, -11.57304410484971235 ) ) ;
#28045 = CARTESIAN_POINT ( 'NONE',  ( 70.03054751895673746, 71.08012399627183697, -0.1251406234029079911 ) ) ;
#28046 = CARTESIAN_POINT ( 'NONE',  ( 190.2236813008869660, 301.1699145145108218, -5.401374690107298093 ) ) ;
#28047 = CARTESIAN_POINT ( 'NONE',  ( 104.3601438707544133, 224.3927522451418213, -10.00000000000009237 ) ) ;
#28048 = CARTESIAN_POINT ( 'NONE',  ( 161.8882824960653579, 250.2482648971885340, -13.83574485983625557 ) ) ;
#28049 = CARTESIAN_POINT ( 'NONE',  ( 176.1923717941176619, 285.1500375202994064, -12.53270729091486402 ) ) ;
#28050 = CARTESIAN_POINT ( 'NONE',  ( 73.86461842229320496, 68.29997319365683950, -11.61748300246921417 ) ) ;
#28051 = CARTESIAN_POINT ( 'NONE',  ( 86.17361039128113021, 233.8927522451419634, 2.944929066748280225E-16 ) ) ;
#28052 = ORIENTED_EDGE ( 'NONE', *, *, #90672, .F. ) ;
#28053 = CARTESIAN_POINT ( 'NONE',  ( -19.75394722521053126, 92.96529481642809856, 59.99999999999999289 ) ) ;
#28054 = B_SPLINE_CURVE_WITH_KNOTS ( 'NONE', 3,
 ( #50944, #89990, #90503, #42339, #20566, #73269, #27671, #65154, #89513, #72796 ),
 .UNSPECIFIED., .F., .F.,
 ( 4, 2, 2, 2, 4 ),
 ( 0.000000000000000000, 0.2500000000000000000, 0.5000000000000000000, 0.7500000000000000000, 1.000000000000000000 ),
 .UNSPECIFIED. ) ;
#28055 = CARTESIAN_POINT ( 'NONE',  ( 162.9466247808429102, 248.4151622881552441, 11.25765811906727443 ) ) ;
#28056 = CARTESIAN_POINT ( 'NONE',  ( 207.5920568422024814, 271.0870056320159165, -1.586464549033245186 ) ) ;
#28057 = VECTOR ( 'NONE', #67205, 1000.000000000000000 ) ;
#28058 = ADVANCED_FACE ( 'NONE', ( #72426 ), #49101, .T. ) ;
#28059 = CARTESIAN_POINT ( 'NONE',  ( 13.49027706508988267, 190.8464784336661637, 1.353441290958777327E-15 ) ) ;
#28060 = CARTESIAN_POINT ( 'NONE',  ( 198.4782858197754649, 286.8725200914082620, -17.44895083299520522 ) ) ;
#28061 = CARTESIAN_POINT ( 'NONE',  ( 173.8665542827094725, 250.6399523573830095, -0.9454928766311748722 ) ) ;
#28062 = CARTESIAN_POINT ( 'NONE',  ( -19.65312891409030271, 93.06504152958497400, 10.00000000000000888 ) ) ;
#28063 = CARTESIAN_POINT ( 'NONE',  ( 53.49034604603116350, 195.5643266524160140, 9.188101187500095079 ) ) ;
#28064 = EDGE_CURVE ( 'NONE', #315, #52745, #85167, .T. ) ;
#28065 = CARTESIAN_POINT ( 'NONE',  ( 164.0179800784044915, 246.5595204798204065, -5.772998092557310557 ) ) ;
#28066 = CARTESIAN_POINT ( 'NONE',  ( 72.55192422928334395, 57.28793452964083599, 16.33633438825195938 ) ) ;
#28067 = CARTESIAN_POINT ( 'NONE',  ( 71.56411227120165108, 71.63451761208904145, 3.366307055662708603 ) ) ;
#28068 = CARTESIAN_POINT ( 'NONE',  ( 66.06661787456808099, 68.52074721796333279, -4.599897531117440153 ) ) ;
#28069 = ORIENTED_EDGE ( 'NONE', *, *, #27574, .F. ) ;
#28070 = LINE ( 'NONE', #74705, #59131 ) ;
#28071 = CARTESIAN_POINT ( 'NONE',  ( 12.14648056717180680, 164.4865022471901455, 1.119607411625061291E-15 ) ) ;
#28072 = DIRECTION ( 'NONE',  ( -0.9669094993746144562, 0.2551196190400350505, 0.000000000000000000 ) ) ;
#28073 = VECTOR ( 'NONE', #33713, 1000.000000000000000 ) ;
#28074 = CARTESIAN_POINT ( 'NONE',  ( 124.8288415870092933, 249.0024278399161517, -9.188101187500093303 ) ) ;
#28075 = CARTESIAN_POINT ( 'NONE',  ( 31.93509797303403630, 20.29860640527293825, -2.839279412974138328 ) ) ;
#28077 = EDGE_CURVE ( 'NONE', #57607, #75521, #71912, .T. ) ;
#28076 = CARTESIAN_POINT ( 'NONE',  ( 183.7975612849717777, 256.6346208101135176, -2.981236333899912161 ) ) ;
#28078 = CARTESIAN_POINT ( 'NONE',  ( 188.3728390295439965, 260.6292366468635464, 6.857486809614422363 ) ) ;
#28079 = CARTESIAN_POINT ( 'NONE',  ( 196.2225432063612232, 281.9592983342773778, 17.73143785322795196 ) ) ;
#28080 = VECTOR ( 'NONE', #88869, 1000.000000000000000 ) ;
#28082 = CARTESIAN_POINT ( 'NONE',  ( 75.19340432564982279, 67.01774300492178327, 13.18884388031393051 ) ) ;
#28081 = CARTESIAN_POINT ( 'NONE',  ( 81.64762987783682036, 41.52940341837351923, -5.382017555150636845 ) ) ;
#28083 = CARTESIAN_POINT ( 'NONE',  ( 68.43388330429554856, 64.50992442928946957, 12.16968166442065957 ) ) ;
#28084 = VERTEX_POINT ( 'NONE', #56690 ) ;
#28085 = CARTESIAN_POINT ( 'NONE',  ( 160.7827666075975799, 284.1908911587130433, 0.8999949044102747431 ) ) ;
#28086 = DIRECTION ( 'NONE',  ( -0.000000000000000000, -0.000000000000000000, -1.000000000000000000 ) ) ;
#28087 = CARTESIAN_POINT ( 'NONE',  ( 67.78796486963464929, 67.26057969838673500, -8.930145946851032690 ) ) ;
#28088 = PLANE ( 'NONE',  #64496 ) ;
#28089 = CARTESIAN_POINT ( 'NONE',  ( 193.9123665762526798, 270.9003325324202365, -13.75132347621049433 ) ) ;
#28090 = ORIENTED_EDGE ( 'NONE', *, *, #18483, .F. ) ;
#28091 = CARTESIAN_POINT ( 'NONE',  ( 68.76233101952506388, 66.50715880584016304, 9.743774830957411481 ) ) ;
#28092 = LINE ( 'NONE', #13411, #87959 ) ;
#28093 = EDGE_CURVE ( 'NONE', #46269, #48318, #32396, .T. ) ;
#28094 = EDGE_CURVE ( 'NONE', #5477, #469, #22326, .T. ) ;
#28095 = CARTESIAN_POINT ( 'NONE',  ( 85.51217825735186295, 45.18995095854337762, 8.208790583656876194 ) ) ;
#28096 = CARTESIAN_POINT ( 'NONE',  ( 29.61132621015796218, 181.2365022471902307, 10.00000000000009948 ) ) ;
#28097 = CARTESIAN_POINT ( 'NONE',  ( 185.8703600842969479, 296.7409536067417548, 5.193023113616601627 ) ) ;
#28098 = DIRECTION ( 'NONE',  ( 0.8660254037844384856, 0.5000000000000002220, 0.000000000000000000 ) ) ;
#28099 = CARTESIAN_POINT ( 'NONE',  ( 150.7294676703291998, 278.2523418184223942, -9.598868465181176928E-05 ) ) ;
#28100 = CARTESIAN_POINT ( 'NONE',  ( 5.882932626810616128, 22.13478043621385893, 8.090169943749478065 ) ) ;
#28101 = CARTESIAN_POINT ( 'NONE',  ( 95.53204957371639239, 214.4155109091896065, 2.679491924311254714 ) ) ;
#28102 = ORIENTED_EDGE ( 'NONE', *, *, #99272, .F. ) ;
#28103 = DIRECTION ( 'NONE',  ( -0.9662637919863231728, -0.2575544297740022248, 0.000000000000000000 ) ) ;
#28104 = CARTESIAN_POINT ( 'NONE',  ( 71.80750138150710882, 71.32421890607284354, 5.932341145765938073 ) ) ;
#28105 = CARTESIAN_POINT ( 'NONE',  ( 156.3110802652713573, 261.4039762261047599, -17.34184811412823635 ) ) ;
#28106 = ORIENTED_EDGE ( 'NONE', *, *, #29269, .T. ) ;
#28107 = CARTESIAN_POINT ( 'NONE',  ( 147.1259762202154207, 275.8173294038533641, -0.6716460511724978710 ) ) ;
#28108 = CARTESIAN_POINT ( 'NONE',  ( 185.1915215135591666, 291.4364884111334391, 11.94946919150295983 ) ) ;
#28109 = CARTESIAN_POINT ( 'NONE',  ( 204.9427641582406636, 275.6757151647582305, 14.40446820030680897 ) ) ;
#28110 = CYLINDRICAL_SURFACE ( 'NONE', #33385, 4.999999999999993783 ) ;
#28111 = ORIENTED_EDGE ( 'NONE', *, *, #2279, .T. ) ;
#28112 = CARTESIAN_POINT ( 'NONE',  ( 87.75264963113552596, 209.2202760586659167, -5.415160957724236172E-17 ) ) ;
#28113 = FACE_OUTER_BOUND ( 'NONE', #17386, .T. ) ;
#28114 = CARTESIAN_POINT ( 'NONE',  ( 73.41259731428677071, 70.10201033320841191, -9.453773877498623079 ) ) ;
#28115 = CARTESIAN_POINT ( 'NONE',  ( 181.1066788586338703, 271.7431116842795973, -16.79793830016840772 ) ) ;
#28116 = CARTESIAN_POINT ( 'NONE',  ( 81.22775765764330913, 42.26095023371678394, -7.344287333291148911 ) ) ;
#28117 = VERTEX_POINT ( 'NONE', #57680 ) ;
#28118 = EDGE_CURVE ( 'NONE', #68592, #37083, #42473, .T. ) ;
#28119 = ORIENTED_EDGE ( 'NONE', *, *, #29347, .F. ) ;
#28120 = CARTESIAN_POINT ( 'NONE',  ( 88.49445028879968334, 43.86712364161932243, -9.307608808691473302E-08 ) ) ;
#28121 = ORIENTED_EDGE ( 'NONE', *, *, #79077, .F. ) ;
#28122 = DIRECTION ( 'NONE',  ( -0.4999999999999998890, 0.8660254037844387076, 0.000000000000000000 ) ) ;
#28123 = ORIENTED_EDGE ( 'NONE', *, *, #71694, .T. ) ;
#28124 = LINE ( 'NONE', #21053, #65401 ) ;
#28125 = DIRECTION ( 'NONE',  ( -0.4999999999999987788, 0.8660254037844392627, 0.000000000000000000 ) ) ;
#28126 = EDGE_LOOP ( 'NONE', ( #74295, #48799, #14778 ) ) ;
#28127 = EDGE_CURVE ( 'NONE', #8862, #32206, #28279, .T. ) ;
#28128 = CARTESIAN_POINT ( 'NONE',  ( 188.9164685758636608, 292.7259968989668550, -13.92583900068085612 ) ) ;
#28129 = CARTESIAN_POINT ( 'NONE',  ( 68.20887950783240683, 70.50781471800318911, 6.446984873749973067E-06 ) ) ;
#28130 = CARTESIAN_POINT ( 'NONE',  ( 74.67000616351418785, 66.81477949400925809, -13.12245706047551330 ) ) ;
#28131 = CARTESIAN_POINT ( 'NONE',  ( 194.5298665426430489, 293.7113828889860656, -16.13302716640051315 ) ) ;
#28132 = B_SPLINE_CURVE_WITH_KNOTS ( 'NONE', 3,
 ( #41846, #78373, #34256, #97450, #58894, #89864, #32250, #63150, #24647, #55529, #98937, #92352, #13813, #44203 ),
 .UNSPECIFIED., .F., .F.,
 ( 4, 2, 2, 2, 2, 2, 4 ),
 ( 0.0005908581131731061812, 0.0008957186388731243169, 0.001200579164573142670, 0.001505439690273160805, 0.001810300215973178941, 0.002420021267373170543, 0.003029742318773161712 ),
 .UNSPECIFIED. ) ;
#28133 = CARTESIAN_POINT ( 'NONE',  ( 11.25695247149110578, 165.7592609112379876, 2.679491924311254714 ) ) ;
#28134 = EDGE_CURVE ( 'NONE', #90765, #32988, #19224, .T. ) ;
#28135 = CARTESIAN_POINT ( 'NONE',  ( 166.6488341214076740, 266.2507106308010520, -16.67339293460069882 ) ) ;
#28136 = EDGE_LOOP ( 'NONE', ( #53981, #70327, #65719, #50064 ) ) ;
#28137 = DIRECTION ( 'NONE',  ( 0.000000000000000000, -0.000000000000000000, 1.000000000000000000 ) ) ;
#28138 = CARTESIAN_POINT ( 'NONE',  ( 7.601631632957884577, 27.49540643055185285, 3.479690158560446702E-15 ) ) ;
#28139 = ORIENTED_EDGE ( 'NONE', *, *, #93977, .F. ) ;
#28140 = LINE ( 'NONE', #90497, #4176 ) ;
#28142 = VERTEX_POINT ( 'NONE', #73408 ) ;
#28141 = CARTESIAN_POINT ( 'NONE',  ( 83.72375369157853697, 157.3685146834693569, 0.000000000000000000 ) ) ;
#28143 = EDGE_CURVE ( 'NONE', #100197, #12032, #44019, .T. ) ;
#28144 = DIRECTION ( 'NONE',  ( 1.000000000000000000, 1.252965984934105094E-13, 0.000000000000000000 ) ) ;
#28145 = CARTESIAN_POINT ( 'NONE',  ( 163.0309151244508712, 248.2691671304387739, 11.27270415168660200 ) ) ;
#28146 = EDGE_CURVE ( 'NONE', #35245, #33613, #754, .T. ) ;
#28147 = CARTESIAN_POINT ( 'NONE',  ( 75.97055471119503522, 64.69957879015430535, -14.33112692621818596 ) ) ;
#28148 = CARTESIAN_POINT ( 'NONE',  ( 149.0959959396991792, 276.3173998796609681, -5.502691077969892319 ) ) ;
#28149 = CARTESIAN_POINT ( 'NONE',  ( 175.5923782935951465, 257.1381361707857991, -12.16266005493879021 ) ) ;
#28150 = CARTESIAN_POINT ( 'NONE',  ( 157.5196022909033502, 258.1848738215194317, 16.72387774136761607 ) ) ;
#28151 = AXIS2_PLACEMENT_3D ( 'NONE', #50538, #51547, #89604 ) ;
#28152 = DIRECTION ( 'NONE',  ( 0.000000000000000000, 0.000000000000000000, 1.000000000000000000 ) ) ;
#28153 = DIRECTION ( 'NONE',  ( 0.000000000000000000, 0.000000000000000000, 1.000000000000000000 ) ) ;
#28154 = ORIENTED_EDGE ( 'NONE', *, *, #342, .T. ) ;
#28155 = CARTESIAN_POINT ( 'NONE',  ( 72.95830788359974406, 56.77128196665827176, -15.96545419981962333 ) ) ;
#28156 = CARTESIAN_POINT ( 'NONE',  ( 65.99695077750568828, 68.68160084762847362, -0.09952674157115595777 ) ) ;
#28157 = VERTEX_POINT ( 'NONE', #12100 ) ;
#28158 = CARTESIAN_POINT ( 'NONE',  ( 2.672015980952107572, 183.8967562850347122, -4.648177544792955347E-16 ) ) ;
#28159 = VECTOR ( 'NONE', #94938, 999.9999999999998863 ) ;
#28160 = CARTESIAN_POINT ( 'NONE',  ( 174.8100629882666226, 281.9492555863050711, -14.07939969178291051 ) ) ;
#28161 = LINE ( 'NONE', #4881, #53048 ) ;
#28162 = CARTESIAN_POINT ( 'NONE',  ( 82.41072854848420093, 44.74050089573861300, -9.837669175488398920 ) ) ;
#28163 = CARTESIAN_POINT ( 'NONE',  ( 161.2348838590686171, 272.7422516289890382, 15.21521688586838472 ) ) ;
#28165 = CARTESIAN_POINT ( 'NONE',  ( 88.21274111123641148, 43.92339361237885242, 2.502205135834632443 ) ) ;
#28164 = CARTESIAN_POINT ( 'NONE',  ( 161.4314170165220332, 281.4313146435951580, -6.707529758775564233 ) ) ;
#28166 = CARTESIAN_POINT ( 'NONE',  ( 201.3130515071547961, 268.8394849092184700, 6.031093409804897831 ) ) ;
#28167 = ORIENTED_EDGE ( 'NONE', *, *, #55322, .F. ) ;
#28168 = PRODUCT_DEFINITION_SHAPE ( 'NONE', 'NONE',  #71293 ) ;
#28169 = ORIENTED_EDGE ( 'NONE', *, *, #31216, .F. ) ;
#28170 = CARTESIAN_POINT ( 'NONE',  ( -41.60683341252619272, 44.79949203189799078, 59.99999999999999289 ) ) ;
#28171 = CARTESIAN_POINT ( 'NONE',  ( 189.8221425493700565, 274.2140629761119612, -15.64287807072788006 ) ) ;
#28172 = CARTESIAN_POINT ( 'NONE',  ( 68.63426881352062026, 66.33891898837059387, -9.865409556835679439 ) ) ;
#28173 = CARTESIAN_POINT ( 'NONE',  ( 175.6300312749814054, 290.9929735238556532, 2.874909097761923160 ) ) ;
#28174 = CARTESIAN_POINT ( 'NONE',  ( 152.7531861616124615, 266.0707158804971186, 17.45453282433162556 ) ) ;
#28175 = CARTESIAN_POINT ( 'NONE',  ( 191.3077102587145646, 274.7514833773715850, 16.90660339326615969 ) ) ;
#28176 = CARTESIAN_POINT ( 'NONE',  ( -9.055497838557604595, 23.87190447404379157, 10.00000000000000000 ) ) ;
#28177 = CARTESIAN_POINT ( 'NONE',  ( 7.212287079182728711, 162.7202760586659451, -5.415160957724236172E-17 ) ) ;
#28178 = CARTESIAN_POINT ( 'NONE',  ( 104.5047417616495125, 221.9548013555409511, -4.594050593750042211 ) ) ;
#28179 = CARTESIAN_POINT ( 'NONE',  ( 87.74907107289484998, 44.16117455547062320, -4.521424286948812821 ) ) ;
#28180 = CARTESIAN_POINT ( 'NONE',  ( 179.9432324357175617, 255.2313477386617819, -2.391771382723571371 ) ) ;
#28181 = CARTESIAN_POINT ( 'NONE',  ( 78.39381814541518168, 53.07351838901534080, 15.75876637147476877 ) ) ;
#28182 = DIRECTION ( 'NONE',  ( -0.8660254037844387076, -0.4999999999999998890, -0.000000000000000000 ) ) ;
#28183 = CARTESIAN_POINT ( 'NONE',  ( 193.7261517370125432, 295.1034577671335342, 14.97744313279139661 ) ) ;
#28184 = CARTESIAN_POINT ( 'NONE',  ( 76.51987890029035100, 63.61070592637643983, 14.91914813192731337 ) ) ;
#28185 = CARTESIAN_POINT ( 'NONE',  ( 147.9791529310278122, 274.3395839928920168, -7.789432462804474433 ) ) ;
#28186 = CARTESIAN_POINT ( 'NONE',  ( 196.5855195306807275, 266.6350943561007512, 8.187369356346602345 ) ) ;
#28187 = DIRECTION ( 'NONE',  ( 1.000000000000000000, 0.000000000000000000, 0.000000000000000000 ) ) ;
#28188 = CARTESIAN_POINT ( 'NONE',  ( 162.4519475857721886, 251.5162682124039577, -12.77131419988232786 ) ) ;
#28189 = CARTESIAN_POINT ( 'NONE',  ( 43.66619682219493370, 206.0177522451419350, 5.000000000000046185 ) ) ;
#28190 = CARTESIAN_POINT ( 'NONE',  ( 72.21491844529387549, 53.64441083166271085, 0.000000000000000000 ) ) ;
#28191 = CARTESIAN_POINT ( 'NONE',  ( 86.20995510670323370, 211.3923013555409796, 4.594050593750050204 ) ) ;
#28192 = CARTESIAN_POINT ( 'NONE',  ( 6.943673075435188302, 24.98502408145590437, -5.678558825948271327 ) ) ;
#28193 = EDGE_CURVE ( 'NONE', #90499, #31470, #53125, .T. ) ;
#28194 = DIRECTION ( 'NONE',  ( -1.000000000000000000, 0.000000000000000000, 0.000000000000000000 ) ) ;
#28196 = CARTESIAN_POINT ( 'NONE',  ( 151.9941942893360078, 267.3853283658117448, 16.97183802629870186 ) ) ;
#28195 = CARTESIAN_POINT ( 'NONE',  ( 196.3341081413628899, 290.5863447708742342, 16.12390540996472410 ) ) ;
#28197 = CARTESIAN_POINT ( 'NONE',  ( 149.7588342556250041, 271.2570855174081430, 12.14104876789268062 ) ) ;
#28198 = CARTESIAN_POINT ( 'NONE',  ( 75.74251350868291865, 65.46771939187904366, 14.28157630633085162 ) ) ;
#28199 = CARTESIAN_POINT ( 'NONE',  ( 204.6060263820569673, 275.8495439392309549, -12.70564820073907875 ) ) ;
#28200 = CARTESIAN_POINT ( 'NONE',  ( 29.08566721201706784, 38.83396525600392124, -2.839279412974133887 ) ) ;
#28201 = CARTESIAN_POINT ( 'NONE',  ( 147.3379027498079381, 275.4502618871274535, -3.695260257281167249 ) ) ;
#28202 = CARTESIAN_POINT ( 'NONE',  ( 84.07848607763526161, 46.87983176300981114, -11.10104033282832958 ) ) ;
#28203 = ORIENTED_EDGE ( 'NONE', *, *, #62836, .F. ) ;
#28204 = CARTESIAN_POINT ( 'NONE',  ( 24.63222838094502265, 17.14754757982090894, -5.678558825948276656 ) ) ;
#28205 = CARTESIAN_POINT ( 'NONE',  ( 60.73642589098854216, 194.3262482093457777, 3.021315404115420679E-15 ) ) ;
#28206 = CARTESIAN_POINT ( 'NONE',  ( 147.5381343315788172, 275.1034506142203782, -4.056595942992749393 ) ) ;
#28207 = CARTESIAN_POINT ( 'NONE',  ( 191.2640738146788806, 288.8540904607579591, -16.48495303880790530 ) ) ;
#28209 = ORIENTED_EDGE ( 'NONE', *, *, #96190, .T. ) ;
#28208 = EDGE_CURVE ( 'NONE', #32720, #33264, #76703, .T. ) ;
#28210 = ADVANCED_FACE ( 'NONE', ( #50095 ), #92137, .F. ) ;
#28211 = CARTESIAN_POINT ( 'NONE',  ( 70.36958601292586479, 61.09422941142852892, 14.35025779664269763 ) ) ;
#28212 = LINE ( 'NONE', #52018, #260 ) ;
#28213 = AXIS2_PLACEMENT_3D ( 'NONE', #61946, #1178, #70053 ) ;
#28214 = CARTESIAN_POINT ( 'NONE',  ( 73.42798026292116731, 58.39006275434417859, 16.23893788096608404 ) ) ;
#28215 = CARTESIAN_POINT ( 'NONE',  ( 48.58227110419247907, 77.44677708231240842, 10.00000000000000000 ) ) ;
#28216 = CARTESIAN_POINT ( 'NONE',  ( 142.1946287021350201, 246.2365022471901739, -10.00000000000009059 ) ) ;
#28217 = CARTESIAN_POINT ( 'NONE',  ( 88.29204076689052272, 44.29173939258662074, -2.000454734116386302 ) ) ;
#28218 = B_SPLINE_CURVE_WITH_KNOTS ( 'NONE', 3,
 ( #14855, #23444, #76664, #77685, #91398, #29568, #6767, #23949, #53838, #85830, #37645, #54333, #7252, #8268, #99982, #62434 ),
 .UNSPECIFIED., .F., .F.,
 ( 4, 1, 2, 2, 2, 1, 2, 2, 4 ),
 ( 0.000000000000000000, 0.1250000000000024425, 0.1875000000000014433, 0.2500000000000004441, 0.5000000000000011102, 0.6250000000000014433, 0.6875000000000021094, 0.7500000000000027756, 1.000000000000000000 ),
 .UNSPECIFIED. ) ;
#28219 = EDGE_LOOP ( 'NONE', ( #27755, #16560, #79516, #67504 ) ) ;
#28220 = CARTESIAN_POINT ( 'NONE',  ( 190.9372308562805642, 299.3033410696684200, -6.605635028715870938 ) ) ;
#28221 = ORIENTED_EDGE ( 'NONE', *, *, #59693, .T. ) ;
#28222 = CARTESIAN_POINT ( 'NONE',  ( 202.8787628851569593, 279.2506702366259788, 17.01435431865322556 ) ) ;
#28223 = CARTESIAN_POINT ( 'NONE',  ( 81.37287889836444776, 42.00540010751133480, -7.805683437329571817 ) ) ;
#28224 = ORIENTED_EDGE ( 'NONE', *, *, #100057, .F. ) ;
#28225 = DIRECTION ( 'NONE',  ( -0.8660254037844387076, -0.4999999999999998890, -0.000000000000000000 ) ) ;
#28227 = ORIENTED_EDGE ( 'NONE', *, *, #86723, .T. ) ;
#28226 = AXIS2_PLACEMENT_3D ( 'NONE', #81749, #12323, #43188 ) ;
#28228 = CARTESIAN_POINT ( 'NONE',  ( 49.65150239490934325, 78.72539382324355017, 10.00000000000000178 ) ) ;
#28229 = CARTESIAN_POINT ( 'NONE',  ( 158.6888631046942919, 255.7898218377643218, 16.04723042051886495 ) ) ;
#28230 = DIRECTION ( 'NONE',  ( -1.000000000000000000, 0.000000000000000000, 0.000000000000000000 ) ) ;
#28231 = CARTESIAN_POINT ( 'NONE',  ( 87.74907107289486419, 44.16117455547063742, -4.521424286948807492 ) ) ;
#28232 = CARTESIAN_POINT ( 'NONE',  ( 192.3713340522295709, 271.8780416168410170, 15.57788208939756380 ) ) ;
#28233 = CARTESIAN_POINT ( 'NONE',  ( 43.56148901884012048, 27.01110640527296169, 2.839279412974134775 ) ) ;
#28234 = CARTESIAN_POINT ( 'NONE',  ( 76.78229342072877728, 59.38575705617227385, -15.96769424347941779 ) ) ;
#28235 = CARTESIAN_POINT ( 'NONE',  ( 167.3724807468772156, 276.1273818265106570, 14.94019753784689364 ) ) ;
#28236 = CARTESIAN_POINT ( 'NONE',  ( 87.51245999513413665, 45.51585123121132881, 6.985658356529230950 ) ) ;
#28237 = ORIENTED_EDGE ( 'NONE', *, *, #57800, .T. ) ;
#28238 = VERTEX_POINT ( 'NONE', #22690 ) ;
#28239 = LINE ( 'NONE', #20656, #63808 ) ;
#28240 = EDGE_CURVE ( 'NONE', #71770, #88756, #14956, .T. ) ;
#28242 = CARTESIAN_POINT ( 'NONE',  ( 165.6659538038370272, 273.9139261607198250, -15.19161387577927869 ) ) ;
#28241 = CARTESIAN_POINT ( 'NONE',  ( 164.2851776226980860, 246.0967207574460929, 5.847738044744511754 ) ) ;
#28243 = CARTESIAN_POINT ( 'NONE',  ( 85.55195523353168596, 48.95437131750654203, -12.20589517503823807 ) ) ;
#28244 = DIRECTION ( 'NONE',  ( 0.09547062131715937372, -0.9954322480537364237, 0.000000000000000000 ) ) ;
#28245 = FACE_OUTER_BOUND ( 'NONE', #79284, .T. ) ;
#28246 = CARTESIAN_POINT ( 'NONE',  ( 190.1063449786324213, 301.3731469862293011, 0.2163967485516588019 ) ) ;
#28247 = FACE_OUTER_BOUND ( 'NONE', #92389, .T. ) ;
#28248 = CARTESIAN_POINT ( 'NONE',  ( 168.4629122334965530, 266.7134460659350452, 16.64887115331695355 ) ) ;
#28249 = CARTESIAN_POINT ( 'NONE',  ( 182.0214274888115256, 256.7798808314274766, 5.137347305127032193 ) ) ;
#28250 = ADVANCED_FACE ( 'NONE', ( #67606 ), #19551, .F. ) ;
#28251 = CARTESIAN_POINT ( 'NONE',  ( 108.2124997955428967, 221.0327760586659451, 1.948934522072303157E-15 ) ) ;
#28252 = VERTEX_POINT ( 'NONE', #98030 ) ;
#28253 = DIRECTION ( 'NONE',  ( -0.7845058662180028897, -0.6201213960746241316, 0.000000000000000000 ) ) ;
#28254 = CARTESIAN_POINT ( 'NONE',  ( 79.14312167556931854, 57.64441083166269664, 0.000000000000000000 ) ) ;
#28255 = CARTESIAN_POINT ( 'NONE',  ( 163.4018158682571595, 277.0544782939701918, -14.36443031031798512 ) ) ;
#28256 = ORIENTED_EDGE ( 'NONE', *, *, #95857, .T. ) ;
#28257 = ORIENTED_EDGE ( 'NONE', *, *, #78939, .T. ) ;
#28258 = CARTESIAN_POINT ( 'NONE',  ( 87.22108034532067222, 46.19249316086605006, -9.000540691006557736 ) ) ;
#28259 = EDGE_CURVE ( 'NONE', #47283, #11459, #33101, .T. ) ;
#28260 = CARTESIAN_POINT ( 'NONE',  ( 176.8648875818473698, 292.4786256060604615, -2.731852314562509321 ) ) ;
#28261 = CARTESIAN_POINT ( 'NONE',  ( 196.0395593785976018, 291.0965181932902510, 15.97855489120023087 ) ) ;
#28262 = CARTESIAN_POINT ( 'NONE',  ( 206.6268150440956504, 272.7588534679261443, -10.76664753678610609 ) ) ;
#28263 = CARTESIAN_POINT ( 'NONE',  ( 206.9821235601573051, 271.0354183991746595, -4.828536961709945174 ) ) ;
#28264 = VERTEX_POINT ( 'NONE', #4311 ) ;
#28265 = VERTEX_POINT ( 'NONE', #6313 ) ;
#28266 = CARTESIAN_POINT ( 'NONE',  ( 163.0056347026689707, 248.3129541054019569, -11.27842346302751508 ) ) ;
#28267 = ORIENTED_EDGE ( 'NONE', *, *, #9468, .F. ) ;
#28268 = CARTESIAN_POINT ( 'NONE',  ( 168.9925526219222434, 247.8045925068635142, -0.5692285522127000785 ) ) ;
#28269 = CARTESIAN_POINT ( 'NONE',  ( -14.83262083840143575, 124.7156766241961208, -21.50000000000003197 ) ) ;
#28270 = CARTESIAN_POINT ( 'NONE',  ( 81.74687756906948266, 43.62721439716015936, 8.949604777968817260 ) ) ;
#28272 = CARTESIAN_POINT ( 'NONE',  ( 69.44557037078072881, 62.66829723885497572, -13.82623753713334303 ) ) ;
#28271 = CARTESIAN_POINT ( 'NONE',  ( 137.3322569020296555, 250.0958772461660544, -9.188101187500095079 ) ) ;
#28273 = CARTESIAN_POINT ( 'NONE',  ( 147.1270795744234476, 264.4111747905818675, -1.822351119449947324E-15 ) ) ;
#28274 = ORIENTED_EDGE ( 'NONE', *, *, #27698, .T. ) ;
#28275 = CARTESIAN_POINT ( 'NONE',  ( 204.9620549308181694, 275.6423025665365572, 14.49661402992083481 ) ) ;
#28276 = CARTESIAN_POINT ( 'NONE',  ( -22.42236680055709641, 157.8615022471902591, 0.000000000000000000 ) ) ;
#28277 = CARTESIAN_POINT ( 'NONE',  ( 82.22171533294620360, 40.70355118814068618, -3.607997168176046543 ) ) ;
#28278 = CARTESIAN_POINT ( 'NONE',  ( 170.1446682757344320, 248.6762405125142550, -0.2689902457364031774 ) ) ;
#28279 = LINE ( 'NONE', #36375, #7483 ) ;
#28280 = CARTESIAN_POINT ( 'NONE',  ( -19.65312891409030271, 93.06504152958497400, -10.00000000000000000 ) ) ;
#28281 = VECTOR ( 'NONE', #49337, 1000.000000000000227 ) ;
#28282 = CARTESIAN_POINT ( 'NONE',  ( 82.28003896795380001, 40.62557011406286733, -3.142018250819525793 ) ) ;
#28283 = DIRECTION ( 'NONE',  ( -0.9738769792773346312, -0.2270762630343691746, 0.000000000000000000 ) ) ;
#28284 = CARTESIAN_POINT ( 'NONE',  ( 79.39955210850102674, 47.95772480916883040, 13.72164937866508616 ) ) ;
#28285 = CARTESIAN_POINT ( 'NONE',  ( 68.01518537448079371, 69.74548201687068172, -1.860190901650351503 ) ) ;
#28286 = CARTESIAN_POINT ( 'NONE',  ( 59.22776434610305785, 198.8768266524159856, -9.188101187500091527 ) ) ;
#28287 = CARTESIAN_POINT ( 'NONE',  ( 206.0870578475358172, 273.6937403561189512, -10.07771901274806581 ) ) ;
#28288 = CARTESIAN_POINT ( 'NONE',  ( 77.72825959162678089, 61.57464001967338163, 16.09025617263268870 ) ) ;
#28289 = CARTESIAN_POINT ( 'NONE',  ( 185.7187107349099335, 289.5908206096054300, -14.74808349899648441 ) ) ;
#28290 = ADVANCED_FACE ( 'NONE', ( #90962 ), #44300, .T. ) ;
#28291 = VECTOR ( 'NONE', #51773, 1000.000000000000114 ) ;
#28292 = CARTESIAN_POINT ( 'NONE',  ( 196.5206556047187405, 288.9772018564501650, -16.98128517232440515 ) ) ;
#28293 = CARTESIAN_POINT ( 'NONE',  ( 196.1245817477023650, 288.9492551302209336, 17.30641872853625074 ) ) ;
#28294 = CARTESIAN_POINT ( 'NONE',  ( -20.91904052551286597, 95.08750694953491234, 45.19940739266792207 ) ) ;
#28295 = CARTESIAN_POINT ( 'NONE',  ( 163.9961211234992788, 256.9275610305372766, 16.20495027727189807 ) ) ;
#28296 = DIRECTION ( 'NONE',  ( 0.8660254037844390407, 0.4999999999999993339, 0.000000000000000000 ) ) ;
#28297 = CARTESIAN_POINT ( 'NONE',  ( -19.59711038235854019, 93.19533221515142429, 59.99999999999999289 ) ) ;
#28298 = CARTESIAN_POINT ( 'NONE',  ( 82.78635604014235128, 53.79147356194603447, 15.41260086504908600 ) ) ;
#28299 = CARTESIAN_POINT ( 'NONE',  ( 187.9019955452718023, 260.0457317612239194, -6.306085470763082235 ) ) ;
#28300 = CARTESIAN_POINT ( 'NONE',  ( 16.84647260051960060, 180.5333772461660544, 9.188101187500095079 ) ) ;
#28301 = CARTESIAN_POINT ( 'NONE',  ( 50.34412104557527812, 188.3262482093458061, 3.021315404115420679E-15 ) ) ;
#28302 = ORIENTED_EDGE ( 'NONE', *, *, #86274, .F. ) ;
#28303 = CARTESIAN_POINT ( 'NONE',  ( 180.2008674086625888, 256.3788900776044102, -7.862092545524210330 ) ) ;
#28305 = ADVANCED_FACE ( 'NONE', ( #89954 ), #28110, .F. ) ;
#28304 = DIRECTION ( 'NONE',  ( -0.5000000000000003331, 0.8660254037844385966, -4.336808689942039923E-16 ) ) ;
#28306 = DIRECTION ( 'NONE',  ( -0.8660254037844378194, -0.5000000000000013323, 0.000000000000000000 ) ) ;
#28307 = CARTESIAN_POINT ( 'NONE',  ( 71.85962433970722429, 72.56121191805073067, -1.249447308665279088 ) ) ;
#28308 = CARTESIAN_POINT ( 'NONE',  ( 56.79189435007682363, 203.5958772461660544, -9.188101187500095079 ) ) ;
#28309 = VECTOR ( 'NONE', #21727, 1000.000000000000000 ) ;
#28310 = CARTESIAN_POINT ( 'NONE',  ( 87.35606880162971777, 45.77061481740688009, 8.290963297571636303 ) ) ;
#28311 = CARTESIAN_POINT ( 'NONE',  ( 151.2567985338353935, 268.6625352796243646, -15.71756535662528798 ) ) ;
#28312 = CARTESIAN_POINT ( 'NONE',  ( 190.5653282632609091, 300.5781646174276602, -5.775635208185608604 ) ) ;
#28313 = CARTESIAN_POINT ( 'NONE',  ( 13.25720545158990937, 8.449665230724928477, -2.296566073217252530E-15 ) ) ;
#28314 = CARTESIAN_POINT ( 'NONE',  ( 197.6456421031980994, 287.3858497455466932, 17.15283754821559015 ) ) ;
#28315 = CARTESIAN_POINT ( 'NONE',  ( 178.2069057043887597, 292.8217088069856686, 2.606728601885306418 ) ) ;
#28316 = CARTESIAN_POINT ( 'NONE',  ( 176.1898462797690286, 274.9273359329014284, 17.22711636514044642 ) ) ;
#28317 = CARTESIAN_POINT ( 'NONE',  ( 72.98545333942395530, 62.85874912432204553, 14.26892869598277436 ) ) ;
#28318 = CARTESIAN_POINT ( 'NONE',  ( 69.04645348238025804, 67.88810431568464310, -8.190965530494443314 ) ) ;
#28319 = CARTESIAN_POINT ( 'NONE',  ( 110.2779841299480239, 241.1427522451419350, 10.00000000000009415 ) ) ;
#28320 = ADVANCED_FACE ( 'NONE', ( #83348 ), #27637, .T. ) ;
#28321 = EDGE_CURVE ( 'NONE', #81514, #709, #91628, .T. ) ;
#28322 = CARTESIAN_POINT ( 'NONE',  ( 81.91818524605139373, 41.06078777436991345, 3.494940157278100923 ) ) ;
#28323 = CARTESIAN_POINT ( 'NONE',  ( -77.58047734835668052, 56.02942318228900120, -10.00000000000000000 ) ) ;
#28324 = CARTESIAN_POINT ( 'NONE',  ( 95.42925689777524667, 239.2365022471903160, 2.944929066748280225E-16 ) ) ;
#28325 = DIRECTION ( 'NONE',  ( -0.9599109957006544125, -0.2803049773603352168, 0.000000000000000000 ) ) ;
#28326 = CARTESIAN_POINT ( 'NONE',  ( 164.9724657260474885, 270.3093585490532291, -16.49746900520251813 ) ) ;
#28327 = ORIENTED_EDGE ( 'NONE', *, *, #81325, .F. ) ;
#28328 = CARTESIAN_POINT ( 'NONE',  ( 63.55789136502527015, 201.3768266524160140, 9.188101187500098632 ) ) ;
#28329 = VERTEX_POINT ( 'NONE', #21520 ) ;
#28330 = CARTESIAN_POINT ( 'NONE',  ( 166.1585231282997199, 265.3369310901885001, 16.55309318940343388 ) ) ;
#28331 = CARTESIAN_POINT ( 'NONE',  ( 161.5260038405503451, 251.2952618122203319, 12.95262340733779283 ) ) ;
#28332 = CARTESIAN_POINT ( 'NONE',  ( -17.33262083840142509, 129.0458036431182904, -21.50000000000003197 ) ) ;
#28333 = ORIENTED_EDGE ( 'NONE', *, *, #48161, .F. ) ;
#28334 = CARTESIAN_POINT ( 'NONE',  ( 65.47921168356343458, 208.6115022471902307, 10.00000000000009592 ) ) ;
#28335 = CARTESIAN_POINT ( 'NONE',  ( 165.0387478276132072, 244.7914988754632191, -2.473354058663827626 ) ) ;
#28336 = CARTESIAN_POINT ( 'NONE',  ( 79.99999999999998579, 9.999999999999985789, 59.99999999999999289 ) ) ;
#28337 = CARTESIAN_POINT ( 'NONE',  ( 26.01788259378743717, 35.99752408145593563, 5.678558825948277544 ) ) ;
#28338 = CARTESIAN_POINT ( 'NONE',  ( 188.9788064033937758, 265.5261700445853421, 10.73023398055530642 ) ) ;
#28339 = CARTESIAN_POINT ( 'NONE',  ( 196.2293283710122012, 290.7678286567270902, -17.07152402978540096 ) ) ;
#28340 = CARTESIAN_POINT ( 'NONE',  ( 156.6823612109870396, 259.2651850631482375, 17.57884712310819708 ) ) ;
#28341 = ORIENTED_EDGE ( 'NONE', *, *, #41819, .T. ) ;
#28342 = CARTESIAN_POINT ( 'NONE',  ( 24.68213521633936836, 16.11110640527292759, -2.839279412974138328 ) ) ;
#28343 = DIRECTION ( 'NONE',  ( -0.5169068966820336009, 0.8560416229147678191, 0.000000000000000000 ) ) ;
#28344 = CARTESIAN_POINT ( 'NONE',  ( 171.2037670605694473, 290.1117831344525939, -1.923673588436341841 ) ) ;
#28345 = CARTESIAN_POINT ( 'NONE',  ( 168.1721027265311648, 255.0603569770035222, -13.93527711627501198 ) ) ;
#28346 = VERTEX_POINT ( 'NONE', #12434 ) ;
#28347 = FACE_OUTER_BOUND ( 'NONE', #38190, .T. ) ;
#28348 = CARTESIAN_POINT ( 'NONE',  ( 167.5505310038667517, 261.6318463984700315, 17.07012949051403439 ) ) ;
#28349 = CARTESIAN_POINT ( 'NONE',  ( 206.1798448551755598, 273.5330285446045195, -10.53862763475382813 ) ) ;
#28350 = VECTOR ( 'NONE', #20049, 1000.000000000000114 ) ;
#28351 = ORIENTED_EDGE ( 'NONE', *, *, #37580, .F. ) ;
#28352 = ORIENTED_EDGE ( 'NONE', *, *, #47452, .T. ) ;
#28353 = EDGE_CURVE ( 'NONE', #76243, #8463, #50411, .T. ) ;
#28355 = PLANE ( 'NONE',  #29737 ) ;
#28354 = CARTESIAN_POINT ( 'NONE',  ( 207.1007598919583472, 271.9379569114424271, -6.086525981869248092 ) ) ;
#28356 = CARTESIAN_POINT ( 'NONE',  ( 71.96639307748559133, 71.49757472301890004, -5.734781593071435424 ) ) ;
#28357 = ORIENTED_EDGE ( 'NONE', *, *, #62855, .F. ) ;
#28358 = CARTESIAN_POINT ( 'NONE',  ( 66.22776509639551534, 69.21226861589723001, -2.085083696610475545 ) ) ;
#28359 = CARTESIAN_POINT ( 'NONE',  ( 198.2114954873088948, 287.3346145022089786, 18.52864136173620935 ) ) ;
#28360 = FACE_OUTER_BOUND ( 'NONE', #17380, .T. ) ;
#28361 = DIRECTION ( 'NONE',  ( 0.000000000000000000, 0.000000000000000000, 1.000000000000000000 ) ) ;
#28363 = CARTESIAN_POINT ( 'NONE',  ( 132.2986577904151204, 241.0643266524160424, -9.188101187500093303 ) ) ;
#28362 = VECTOR ( 'NONE', #99617, 1000.000000000000000 ) ;
#28364 = DIRECTION ( 'NONE',  ( 0.4999999999999998890, -0.8660254037844385966, 0.000000000000000000 ) ) ;
#28365 = ORIENTED_EDGE ( 'NONE', *, *, #42972, .T. ) ;
#28366 = CARTESIAN_POINT ( 'NONE',  ( 170.7338553607939957, 263.9049642311459252, 15.82425947459563353 ) ) ;
#28367 = CARTESIAN_POINT ( 'NONE',  ( 115.3478411848173693, 230.7365022471902307, 10.00000000000009948 ) ) ;
#28368 = VERTEX_POINT ( 'NONE', #74249 ) ;
#28369 = CARTESIAN_POINT ( 'NONE',  ( 87.63119364650854948, 45.29408460765224476, 6.394950601605615681 ) ) ;
#28370 = VERTEX_POINT ( 'NONE', #44792 ) ;
#28371 = ORIENTED_EDGE ( 'NONE', *, *, #98837, .F. ) ;
#28372 = CARTESIAN_POINT ( 'NONE',  ( 198.6755293322981117, 286.5308843062557571, 17.86676876308990103 ) ) ;
#28373 = CARTESIAN_POINT ( 'NONE',  ( -27.42236680055714260, 166.5217562850347406, 1.224646799147364892E-15 ) ) ;
#28374 = CARTESIAN_POINT ( 'NONE',  ( 72.54290492928882372, 206.5643266524159856, -9.188101187500093303 ) ) ;
#28375 = DIRECTION ( 'NONE',  ( -0.000000000000000000, 0.000000000000000000, 1.000000000000000000 ) ) ;
#28376 = CARTESIAN_POINT ( 'NONE',  ( 111.7394020023821781, 241.9865022471903160, 10.00000000000009415 ) ) ;
#28377 = PLANE ( 'NONE',  #56382 ) ;
#28378 = CARTESIAN_POINT ( 'NONE',  ( -17.65922707974272399, 170.6115022471903160, -5.000000000000047962 ) ) ;
#28379 = CARTESIAN_POINT ( 'NONE',  ( 105.0000000000000000, 10.00000000000003197, 59.99999999999999289 ) ) ;
#28380 = ORIENTED_EDGE ( 'NONE', *, *, #54579, .F. ) ;
#28381 = CARTESIAN_POINT ( 'NONE',  ( 71.07962098583328725, 64.00820346700967889, -13.02735857669132535 ) ) ;
#28382 = CARTESIAN_POINT ( 'NONE',  ( 153.4542976351440302, 264.8563551865710224, -17.11782692037292009 ) ) ;
#28383 = CARTESIAN_POINT ( 'NONE',  ( 203.4682009197399566, 278.2297336128146412, -15.36039508894693206 ) ) ;
#28384 = ORIENTED_EDGE ( 'NONE', *, *, #79534, .F. ) ;
#28385 = LINE ( 'NONE', #20814, #92276 ) ;
#28386 = CARTESIAN_POINT ( 'NONE',  ( 76.30616544034062088, 50.97262258187969763, -15.53540872755634084 ) ) ;
#28387 = CARTESIAN_POINT ( 'NONE',  ( 164.4320720012133847, 246.5467109461125119, 4.311465402957962212 ) ) ;
#28388 = CARTESIAN_POINT ( 'NONE',  ( 199.5442653985851962, 283.0261893010793415, -17.63221794778640117 ) ) ;
#28389 = EDGE_CURVE ( 'NONE', #68818, #35708, #51410, .T. ) ;
#28390 = DIRECTION ( 'NONE',  ( 0.9659258262890730862, -0.2588190451025027539, -1.337837478769339558E-14 ) ) ;
#28391 = VECTOR ( 'NONE', #79551, 1000.000000000000000 ) ;
#28392 = CARTESIAN_POINT ( 'NONE',  ( 149.1004267900891307, 272.3974806997987343, -12.86882154300063341 ) ) ;
#28393 = CARTESIAN_POINT ( 'NONE',  ( 36.56303213232966698, 203.4637435831424739, 2.679491924311303119 ) ) ;
#28394 = EDGE_LOOP ( 'NONE', ( #84395, #69704, #27770, #88347 ) ) ;
#28395 = CARTESIAN_POINT ( 'NONE',  ( 134.5444773117747275, 257.6744531367911577, 4.594050593750047540 ) ) ;
#28396 = ORIENTED_EDGE ( 'NONE', *, *, #19107, .F. ) ;
#28397 = CARTESIAN_POINT ( 'NONE',  ( 182.1984841339006778, 258.0221543759674887, 6.508891290182809541 ) ) ;
#28398 = CARTESIAN_POINT ( 'NONE',  ( 79.95001512610187433, 44.77191418025095260, -11.25851131356374069 ) ) ;
#28399 = CIRCLE ( 'NONE', #41343, 60.00000000000001421 ) ;
#28400 = CARTESIAN_POINT ( 'NONE',  ( 79.39506416949035383, 59.74337618841887121, -16.16789220604118427 ) ) ;
#28401 = DIRECTION ( 'NONE',  ( 0.000000000000000000, -0.000000000000000000, 1.000000000000000000 ) ) ;
#28402 = CARTESIAN_POINT ( 'NONE',  ( -19.65312891409030271, 93.06504152958497400, 177.5919119679930134 ) ) ;
#28403 = VERTEX_POINT ( 'NONE', #58019 ) ;
#28404 = DIRECTION ( 'NONE',  ( -1.000000000000000000, 0.000000000000000000, 0.000000000000000000 ) ) ;
#28405 = CARTESIAN_POINT ( 'NONE',  ( 182.1470424277336804, 275.5479489297672444, -16.45731081755295477 ) ) ;
#28406 = CARTESIAN_POINT ( 'NONE',  ( 72.52340034770776356, 71.25924148755669307, -6.049577167954354628 ) ) ;
#28407 = CARTESIAN_POINT ( 'NONE',  ( 206.1670584421323724, 273.5551752616418639, -11.23038754588519694 ) ) ;
#28408 = CARTESIAN_POINT ( 'NONE',  ( 201.7502332754098120, 267.6057469551752206, 0.8447870975616070810 ) ) ;
#28409 = CARTESIAN_POINT ( 'NONE',  ( 195.3076413944070566, 263.9809680824703833, 0.8396464432550897472 ) ) ;
#28410 = CARTESIAN_POINT ( 'NONE',  ( 3.330649899756923382, 26.67094063374350554, -10.00000000000000000 ) ) ;
#28411 = CARTESIAN_POINT ( 'NONE',  ( 70.72027907625651721, 71.44976051602542100, 1.172912725620659735 ) ) ;
#28412 = VECTOR ( 'NONE', #78556, 1000.000000000000000 ) ;
#28413 = CARTESIAN_POINT ( 'NONE',  ( 196.1609710299282767, 270.7725530739749047, 12.00615862555037161 ) ) ;
#28414 = CARTESIAN_POINT ( 'NONE',  ( 16.01772687902244741, 32.18080186712592905, 3.090169943749475401 ) ) ;
#28415 = CARTESIAN_POINT ( 'NONE',  ( 190.7222376050763444, 300.3063896652212179, 3.365789908110941475 ) ) ;
#28416 = CARTESIAN_POINT ( 'NONE',  ( -13.11024591527734628, 0.000000000000000000, 32.50000000000000000 ) ) ;
#28417 = FACE_OUTER_BOUND ( 'NONE', #4258, .T. ) ;
#28418 = VECTOR ( 'NONE', #326, 1000.000000000000000 ) ;
#28419 = B_SPLINE_CURVE_WITH_KNOTS ( 'NONE', 3,
 ( #90603, #75368, #22144, #61624 ),
 .UNSPECIFIED., .F., .F.,
 ( 4, 4 ),
 ( 0.008781669780308986456, 0.01506971286528496420 ),
 .UNSPECIFIED. ) ;
#28420 = CARTESIAN_POINT ( 'NONE',  ( 197.9598023461055902, 287.7705598106892921, 18.23120408239484291 ) ) ;
#28421 = CARTESIAN_POINT ( 'NONE',  ( 207.3536890771331116, 271.4998707120027461, 6.332947442802633553 ) ) ;
#28422 = CARTESIAN_POINT ( 'NONE',  ( 138.9289912384832917, 241.0177522451417929, 5.000000000000051514 ) ) ;
#28423 = CARTESIAN_POINT ( 'NONE',  ( 175.8485278518198527, 285.2463791769441173, -12.03390954887754383 ) ) ;
#28424 = ORIENTED_EDGE ( 'NONE', *, *, #45997, .T. ) ;
#28425 = CARTESIAN_POINT ( 'NONE',  ( 66.55102321144717337, 67.77113377364665325, -6.986612483274318386 ) ) ;
#28426 = CARTESIAN_POINT ( 'NONE',  ( 198.9225589249066957, 286.1030165008847916, -17.03502353404871883 ) ) ;
#28427 = CARTESIAN_POINT ( 'NONE',  ( 19.87790860953014160, 170.0327760586659451, 1.948934522072302763E-15 ) ) ;
#28428 = B_SPLINE_CURVE_WITH_KNOTS ( 'NONE', 3,
 ( #37551, #35582, #13300, #91306 ),
 .UNSPECIFIED., .F., .F.,
 ( 4, 4 ),
 ( 0.04785166522048146798, 0.04887066958154937663 ),
 .UNSPECIFIED. ) ;
#28429 = CARTESIAN_POINT ( 'NONE',  ( 177.5317288456356835, 258.4661256883071019, -10.34817642027781481 ) ) ;
#28430 = CARTESIAN_POINT ( 'NONE',  ( 28.84760059290936951, 18.78380873178787880, -6.180339887498949025 ) ) ;
#28431 = CARTESIAN_POINT ( 'NONE',  ( 85.14384985004556938, 49.02042691017501141, 12.45195446300535913 ) ) ;
#28432 = CARTESIAN_POINT ( 'NONE',  ( 157.1850763439666139, 258.3944569110938687, -16.98181238659443437 ) ) ;
#28433 = CARTESIAN_POINT ( 'NONE',  ( 71.96596176604222705, 72.21842720279319394, -3.609932465874673646 ) ) ;
#28434 = CARTESIAN_POINT ( 'NONE',  ( 73.82676074875507766, 55.15409192242278635, -16.12371039794902572 ) ) ;
#28436 = CARTESIAN_POINT ( 'NONE',  ( 69.71912771937687126, 204.3927522451418497, 10.00000000000009592 ) ) ;
#28435 = CARTESIAN_POINT ( 'NONE',  ( 167.4083242872330857, 256.8190524212876085, 14.60336118133068872 ) ) ;
#28437 = CARTESIAN_POINT ( 'NONE',  ( 74.88684299965727575, 67.20604708707715247, 12.50098552432902999 ) ) ;
#28438 = CARTESIAN_POINT ( 'NONE',  ( 150.5461004505574181, 269.8935004687035644, 13.73913105907748111 ) ) ;
#28439 = EDGE_CURVE ( 'NONE', #70463, #37554, #63490, .T. ) ;
#28440 = ADVANCED_FACE ( 'NONE', ( #29126 ), #92544, .T. ) ;
#28441 = CARTESIAN_POINT ( 'NONE',  ( 56.45811372747557044, 196.7365022471902023, -10.00000000000009059 ) ) ;
#28442 = CARTESIAN_POINT ( 'NONE',  ( 181.5699223927324795, 292.0049823800039803, 9.001579805457852856 ) ) ;
#28443 = CARTESIAN_POINT ( 'NONE',  ( 147.7978300115112233, 274.6536445020713018, 7.902890709649431855 ) ) ;
#28444 = EDGE_CURVE ( 'NONE', #7164, #22055, #4622, .T. ) ;
#28445 = CARTESIAN_POINT ( 'NONE',  ( 14.27519936121077926, 188.2369531367911293, -4.594050593750048428 ) ) ;
#28446 = CARTESIAN_POINT ( 'NONE',  ( 72.85870443091528159, 70.94102631263369574, -7.807649534274237801 ) ) ;
#28447 = EDGE_CURVE ( 'NONE', #49096, #7164, #25316, .T. ) ;
#28448 = CARTESIAN_POINT ( 'NONE',  ( 79.42893949975002954, 59.60668959204592454, 16.17820502721878739 ) ) ;
#28449 = CARTESIAN_POINT ( 'NONE',  ( 42.48198750171711424, 33.03085787977767041, 9.188101187500006262 ) ) ;
#28450 = CARTESIAN_POINT ( 'NONE',  ( 201.8291755756830241, 280.5217801640038715, -16.04463949318729021 ) ) ;
#28451 = CARTESIAN_POINT ( 'NONE',  ( 164.6649740431187183, 245.4388940607451843, -1.430729255012818557 ) ) ;
#28452 = DIRECTION ( 'NONE',  ( -0.8660254037844387076, -0.4999999999999998890, -0.000000000000000000 ) ) ;
#28453 = CARTESIAN_POINT ( 'NONE',  ( 153.5337505630658654, 266.4617915331671156, -16.61785508892420182 ) ) ;
#28454 = CARTESIAN_POINT ( 'NONE',  ( 46.88368875251780565, 110.3874725885333135, -10.00000000000000000 ) ) ;
#28455 = CARTESIAN_POINT ( 'NONE',  ( 0.000000000000000000, 0.000000000000000000, 0.000000000000000000 ) ) ;
#28456 = CARTESIAN_POINT ( 'NONE',  ( 17.99030130830579566, 16.10170272979926054, -7.433330006724141015 ) ) ;
#28457 = CARTESIAN_POINT ( 'NONE',  ( 165.6111162920294362, 285.3959942432976504, 0.3651359175268718560 ) ) ;
#28458 = CARTESIAN_POINT ( 'NONE',  ( 83.00815485991435594, 53.30142267139499523, 15.60062745561815944 ) ) ;
#28459 = DIRECTION ( 'NONE',  ( 0.4999999999999973910, -0.8660254037844401509, -1.249000902703321145E-14 ) ) ;
#28460 = AXIS2_PLACEMENT_3D ( 'NONE', #89172, #4494, #27800 ) ;
#28461 = LINE ( 'NONE', #20891, #51612 ) ;
#28462 = EDGE_LOOP ( 'NONE', ( #53706, #12666, #47797, #4851, #87726, #37210, #59606, #10581 ) ) ;
#28463 = CARTESIAN_POINT ( 'NONE',  ( 41.03800390905408335, 35.64441083166263979, -10.00000000000000533 ) ) ;
#28464 = CARTESIAN_POINT ( 'NONE',  ( 156.9140063554453377, 276.4170914181521539, 10.52199787263365494 ) ) ;
#28465 = CARTESIAN_POINT ( 'NONE',  ( 206.2809287719926488, 273.3579460648492159, -10.70911012174624588 ) ) ;
#28466 = ORIENTED_EDGE ( 'NONE', *, *, #45328, .F. ) ;
#28467 = CARTESIAN_POINT ( 'NONE',  ( 195.5602278707908397, 290.3821284405168512, -16.61863160252172023 ) ) ;
#28468 = LINE ( 'NONE', #4690, #57917 ) ;
#28469 = VECTOR ( 'NONE', #59161, 1000.000000000000000 ) ;
#28470 = CARTESIAN_POINT ( 'NONE',  ( 183.8754313647489198, 256.5225093191261294, -2.022205659181245174 ) ) ;
#28471 = CARTESIAN_POINT ( 'NONE',  ( 154.9792334219179679, 262.2150889255981951, -17.21325849938693153 ) ) ;
#28472 = VERTEX_POINT ( 'NONE', #95467 ) ;
#28473 = ORIENTED_EDGE ( 'NONE', *, *, #21602, .F. ) ;
#28475 = CARTESIAN_POINT ( 'NONE',  ( 204.8523313866422484, 275.8323493198358847, 14.65426965484541100 ) ) ;
#28474 = CARTESIAN_POINT ( 'NONE',  ( 159.7144335965733433, 278.4664156918360050, -9.777473725360442458 ) ) ;
#28476 = CARTESIAN_POINT ( 'NONE',  ( 152.9262073036446168, 265.7710344717137900, 16.19159804214501008 ) ) ;
#28477 = EDGE_LOOP ( 'NONE', ( #85325, #87017, #71483, #46219 ) ) ;
#28478 = CARTESIAN_POINT ( 'NONE',  ( 88.16692178265705593, 43.83444978110026824, -2.116868534317887462 ) ) ;
#28479 = CARTESIAN_POINT ( 'NONE',  ( 80.61280386015431532, 57.63106766464478170, 16.59051181579432210 ) ) ;
#28480 = DIRECTION ( 'NONE',  ( -0.000000000000000000, 0.000000000000000000, -1.000000000000000000 ) ) ;
#28481 = VERTEX_POINT ( 'NONE', #32603 ) ;
#28482 = CARTESIAN_POINT ( 'NONE',  ( 87.70143564587257856, 45.35820550660533712, -6.464259315817296958 ) ) ;
#28483 = CARTESIAN_POINT ( 'NONE',  ( 196.6317700900902139, 290.0707791521982131, -17.91116578096951883 ) ) ;
#28484 = VERTEX_POINT ( 'NONE', #33102 ) ;
#28485 = CARTESIAN_POINT ( 'NONE',  ( 164.7462163020046262, 245.2981783406326599, 1.451255823150352064 ) ) ;
#28486 = AXIS2_PLACEMENT_3D ( 'NONE', #74171, #33667, #41743 ) ;
#28487 = CARTESIAN_POINT ( 'NONE',  ( 74.07498815047767948, 61.33227585059758979, 15.11922174825890863 ) ) ;
#28488 = ORIENTED_EDGE ( 'NONE', *, *, #45507, .F. ) ;
#28489 = CARTESIAN_POINT ( 'NONE',  ( 174.4487371657580468, 277.2123390989709151, -15.64973371979014338 ) ) ;
#28490 = CARTESIAN_POINT ( 'NONE',  ( 169.6261978958059728, 261.9618702208159675, -15.78807854465063798 ) ) ;
#28491 = ORIENTED_EDGE ( 'NONE', *, *, #46624, .T. ) ;
#28492 = DIRECTION ( 'NONE',  ( -0.8718556560469457040, -0.4897629171537489778, 0.000000000000000000 ) ) ;
#28493 = CARTESIAN_POINT ( 'NONE',  ( 147.2567621633200474, 275.5908015054806128, -3.647191014543873955 ) ) ;
#28494 = VECTOR ( 'NONE', #147, 999.9999999999998863 ) ;
#28495 = VERTEX_POINT ( 'NONE', #47783 ) ;
#28496 = CARTESIAN_POINT ( 'NONE',  ( 157.7366572918917882, 268.9116757437374758, 15.63315894949619178 ) ) ;
#28497 = VERTEX_POINT ( 'NONE', #16892 ) ;
#28498 = CARTESIAN_POINT ( 'NONE',  ( 156.2224770818481545, 267.4677849582849376, -16.91854127892884208 ) ) ;
#28499 = CARTESIAN_POINT ( 'NONE',  ( 147.5848197185516142, 275.0225891520124151, 4.420251097676741736 ) ) ;
#28500 = CARTESIAN_POINT ( 'NONE',  ( 82.83837546952335629, 53.74639695667534767, 15.76443799962147096 ) ) ;
#28501 = DIRECTION ( 'NONE',  ( 1.000000000000000000, 1.776356839400250212E-13, 0.000000000000000000 ) ) ;
#28502 = CARTESIAN_POINT ( 'NONE',  ( 153.3703256797887775, 265.0017988796566897, 16.44314709207578318 ) ) ;
#28503 = CARTESIAN_POINT ( 'NONE',  ( 39.95181620016202118, 182.3262482093457209, 3.021315404115420679E-15 ) ) ;
#28504 = CARTESIAN_POINT ( 'NONE',  ( 191.0478321355427624, 299.7424433957868928, -9.006798842970001218 ) ) ;
#28505 = ORIENTED_EDGE ( 'NONE', *, *, #50988, .T. ) ;
#28506 = CARTESIAN_POINT ( 'NONE',  ( 80.38715323973768534, 55.64886525756523383, -16.07503577061131139 ) ) ;
#28507 = EDGE_CURVE ( 'NONE', #6045, #23996, #10132, .T. ) ;
#28508 = CARTESIAN_POINT ( 'NONE',  ( 33.70846307691164156, 35.16454794089043645, -10.00000000000000355 ) ) ;
#28510 = CARTESIAN_POINT ( 'NONE',  ( 165.0565241268390366, 244.7607094220335568, 2.191926263411719589 ) ) ;
#28509 = CARTESIAN_POINT ( 'NONE',  ( 149.3801359649374092, 271.9130101976182914, -11.41245530317637424 ) ) ;
#28511 = ORIENTED_EDGE ( 'NONE', *, *, #18971, .F. ) ;
#28512 = DIRECTION ( 'NONE',  ( 0.000000000000000000, 0.000000000000000000, 1.000000000000000000 ) ) ;
#28513 = CARTESIAN_POINT ( 'NONE',  ( 176.7429058980506227, 289.7743273258707291, -9.091347092446275369 ) ) ;
#28514 = VERTEX_POINT ( 'NONE', #48817 ) ;
#28515 = CARTESIAN_POINT ( 'NONE',  ( 149.4634369175186066, 271.7687287154290061, -11.52144114384952367 ) ) ;
#28516 = CARTESIAN_POINT ( 'NONE',  ( 70.71838976632287199, 66.47366496125707158, 11.00380527725184088 ) ) ;
#28517 = CARTESIAN_POINT ( 'NONE',  ( 86.30490461368275135, 44.79992195346583372, 7.720146956292412987 ) ) ;
#28518 = CARTESIAN_POINT ( 'NONE',  ( 118.5773942495488882, 249.2677522451419065, -5.000000000000047962 ) ) ;
#28519 = CARTESIAN_POINT ( 'NONE',  ( 159.8807525190996444, 253.7254088150106099, -15.62640036463813686 ) ) ;
#28520 = CARTESIAN_POINT ( 'NONE',  ( 96.65612621980322672, 226.6115022471902307, 10.00000000000009592 ) ) ;
#28521 = ORIENTED_EDGE ( 'NONE', *, *, #12641, .F. ) ;
#28522 = CARTESIAN_POINT ( 'NONE',  ( 170.5265982536998592, 255.7106794591476557, -12.46252183393470858 ) ) ;
#28523 = CARTESIAN_POINT ( 'NONE',  ( 84.89294916980452399, 45.33893183262856041, 9.636921286913860740 ) ) ;
#28525 = EDGE_CURVE ( 'NONE', #11450, #76998, #4241, .T. ) ;
#28524 = CARTESIAN_POINT ( 'NONE',  ( 207.1601050488701503, 271.8351680844880889, 6.320235450527015075 ) ) ;
#28526 = CARTESIAN_POINT ( 'NONE',  ( 40.63510790894947888, 184.2677522451417929, -5.000000000000041744 ) ) ;
#28527 = CARTESIAN_POINT ( 'NONE',  ( 115.5194155920915620, 231.3768266524159856, 9.188101187500096856 ) ) ;
#28528 = CARTESIAN_POINT ( 'NONE',  ( 181.1018697000030500, 294.2850109623373100, -2.647402609916298388 ) ) ;
#28529 = CARTESIAN_POINT ( 'NONE',  ( 162.7502451860280530, 249.5826859877889490, -11.13675961672946713 ) ) ;
#28530 = DIRECTION ( 'NONE',  ( -0.4330127018922169113, -0.2500000000000014433, -0.8660254037844393737 ) ) ;
#28531 = CARTESIAN_POINT ( 'NONE',  ( 39.80235952159635815, 84.99999999999998579, 59.99999999999999289 ) ) ;
#28532 = CARTESIAN_POINT ( 'NONE',  ( 25.77718602916411683, 191.8149278399160949, -9.188101187500095079 ) ) ;
#28533 = VECTOR ( 'NONE', #5571, 1000.000000000000114 ) ;
#28534 = PLANE ( 'NONE',  #91586 ) ;
#28535 = VECTOR ( 'NONE', #34146, 1000.000000000000227 ) ;
#28536 = ORIENTED_EDGE ( 'NONE', *, *, #77485, .F. ) ;
#28537 = CARTESIAN_POINT ( 'NONE',  ( 30.34687108590970794, 93.06504152958497400, 40.00000000000000000 ) ) ;
#28538 = CARTESIAN_POINT ( 'NONE',  ( 181.1611384956651705, 267.7195240920720494, 14.99755381712351365 ) ) ;
#28539 = CARTESIAN_POINT ( 'NONE',  ( 79.99999999999997158, 26.16025403784438907, 54.99999999999999289 ) ) ;
#28540 = AXIS2_PLACEMENT_3D ( 'NONE', #28643, #97579, #20071 ) ;
#28541 = CARTESIAN_POINT ( 'NONE',  ( 81.84558054786948844, 41.74795303040114192, -5.623115284622243415 ) ) ;
#28542 = B_SPLINE_CURVE_WITH_KNOTS ( 'NONE', 3,
 ( #33614, #86868, #64511, #87392, #42680, #32605, #55870, #95469, #26022, #56891, #17399, #48311, #87875, #18421, #79255, #49311, #26517, #80249, #3235, #57394, #88369, #18927, #9827, #43175, #45057, #7057, #68851, #15140, #69360, #37447, #35598, #85098, #53163, #35093, #74118, #61748, #89840, #37939, #22259, #76954, #45547, #23248, #4712, #22769, #58387, #53646, #84118, #99772, #100279, #75998 ),
 .UNSPECIFIED., .F., .F.,
 ( 4, 2, 2, 2, 2, 2, 2, 2, 2, 2, 2, 2, 2, 2, 2, 2, 2, 2, 2, 2, 2, 2, 2, 2, 4 ),
 ( 0.0001402968676236758798, 0.001130964830274715227, 0.001378631820937422162, 0.001626298811600129313, 0.001750132306931482997, 0.001873965802262836247, 0.001997799297594189932, 0.002121632792925543399, 0.002369299783588250767, 0.002616966774250957268, 0.003112300755576218915, 0.004102968718226588686, 0.005093636680876957590, 0.005588970662202106914, 0.005836637652864646447, 0.006084304643527185114, 0.006146221391192784218, 0.006208138138858384190, 0.006270054886523983295, 0.006331971634189583267, 0.006579638624852431582, 0.007074972606178260917, 0.007570306587504091987, 0.007817973578167001017, 0.008065640568829910914 ),
 .UNSPECIFIED. ) ;
#28543 = CARTESIAN_POINT ( 'NONE',  ( 207.7296438747196134, 270.8486979012336633, -6.692930657757584001 ) ) ;
#28544 = CARTESIAN_POINT ( 'NONE',  ( 178.1790154062099134, 287.6584321602529144, -13.04213889271035676 ) ) ;
#28545 = CARTESIAN_POINT ( 'NONE',  ( 164.3713690399699772, 250.1140898715638627, 10.21268107768454492 ) ) ;
#28546 = CARTESIAN_POINT ( 'NONE',  ( 93.89567024169240028, 225.0177522451418781, -10.00000000000009592 ) ) ;
#28547 = ORIENTED_EDGE ( 'NONE', *, *, #16849, .T. ) ;
#28548 = CARTESIAN_POINT ( 'NONE',  ( 79.21141449090156073, 59.45940664425067723, -16.53580481313993289 ) ) ;
#28549 =( REPRESENTATION_RELATIONSHIP ('NONE','NONE', #67038, #46310 ) REPRESENTATION_RELATIONSHIP_WITH_TRANSFORMATION ( #29953 )SHAPE_REPRESENTATION_RELATIONSHIP( ) );
#28550 = CARTESIAN_POINT ( 'NONE',  ( 157.6006514737650832, 281.0282930248237108, -1.590882658691914253 ) ) ;
#28551 = CARTESIAN_POINT ( 'NONE',  ( 207.7625791259561652, 270.7916523727319031, -1.015623356719550063 ) ) ;
#28552 = VECTOR ( 'NONE', #74436, 1000.000000000000114 ) ;
#28553 = CARTESIAN_POINT ( 'NONE',  ( 18.14551070619625150, 181.2833772461660544, -9.188101187500095079 ) ) ;
#28554 = CARTESIAN_POINT ( 'NONE',  ( 10.80369284495069238, 14.43677371833799405, -10.00000000000000355 ) ) ;
#28555 = AXIS2_PLACEMENT_3D ( 'NONE', #25059, #55935, #48374 ) ;
#28556 = CARTESIAN_POINT ( 'NONE',  ( 80.36164233910257337, 50.39821764556134553, 15.11645672796150208 ) ) ;
#28557 = CARTESIAN_POINT ( 'NONE',  ( 146.8574506849497538, 276.2824292740633041, -4.888313306692038118 ) ) ;
#28558 = CARTESIAN_POINT ( 'NONE',  ( 73.39522077465731797, 69.90148087279546019, 9.687480369506271671 ) ) ;
#28559 = ADVANCED_FACE ( 'NONE', ( #63001 ), #15663, .T. ) ;
#28560 = CARTESIAN_POINT ( 'NONE',  ( 60.66220569506229765, 196.6423013555410080, -4.594050593750043987 ) ) ;
#28561 = CARTESIAN_POINT ( 'NONE',  ( 207.9622466093905189, 270.4458181468041289, 3.586592550214158681 ) ) ;
#28562 = CARTESIAN_POINT ( 'NONE',  ( 203.6714976035736981, 276.2235336633698921, 13.32122003884233941 ) ) ;
#28563 = CARTESIAN_POINT ( 'NONE',  ( 70.95257891153383412, 70.90720881971088829, 4.546241700195112756 ) ) ;
#28564 = CARTESIAN_POINT ( 'NONE',  ( 66.10053949976611420, 68.48843487209605030, -4.753018814780690882 ) ) ;
#28565 = ORIENTED_EDGE ( 'NONE', *, *, #15064, .T. ) ;
#28566 = VECTOR ( 'NONE', #18742, 1000.000000000000000 ) ;
#28567 =( BOUNDED_CURVE ( )  B_SPLINE_CURVE ( 2, ( #57766, #89247, #73008, #20792, #80631, #82126, #13194, #3599, #19797 ),
 .UNSPECIFIED., .F., .T. ) 
 B_SPLINE_CURVE_WITH_KNOTS ( ( 3, 2, 2, 2, 3 ),
 ( 0.5120967741935483764, 0.5134408602150537515, 0.5161290322580645018, 0.5188172043010752521, 0.5201612903225806273 ),
 .UNSPECIFIED. ) 
 CURVE ( )  GEOMETRIC_REPRESENTATION_ITEM ( )  RATIONAL_B_SPLINE_CURVE ( ( 0.9330127018922194093, 0.9330127018922194093, 1.000000000000000000, 0.8660254037844387076, 1.000000000000000000, 0.8660254037844387076, 1.000000000000000000, 0.9330127018922194093, 0.9330127018922194093 ) ) 
 REPRESENTATION_ITEM ( '' )  );
#28568 = CARTESIAN_POINT ( 'NONE',  ( 18.71383987920374992, 181.6115022471902591, 10.00000000000009592 ) ) ;
#28569 = CARTESIAN_POINT ( 'NONE',  ( 77.32817876982271343, 63.13942984521013813, 15.61058464551962288 ) ) ;
#28570 = CARTESIAN_POINT ( 'NONE',  ( 137.4948102131217524, 244.0643266524159856, -9.188101187500093303 ) ) ;
#28571 = CARTESIAN_POINT ( 'NONE',  ( 30.43941648770709207, 23.28920272979928541, -7.433330006724141015 ) ) ;
#28572 = CARTESIAN_POINT ( 'NONE',  ( 207.2266458903087312, 271.7199159663382488, -8.370253452505480141 ) ) ;
#28573 = EDGE_CURVE ( 'NONE', #51377, #91972, #80412, .T. ) ;
#28574 = CARTESIAN_POINT ( 'NONE',  ( 16.83152549358277739, 56.39007365579823983, 59.99999999999999289 ) ) ;
#28575 = DIRECTION ( 'NONE',  ( -0.9576970189910627429, -0.2877784213863714968, 0.000000000000000000 ) ) ;
#28577 = CARTESIAN_POINT ( 'NONE',  ( 74.74196695595742312, 67.08715363026114176, 12.96493619559571719 ) ) ;
#28576 = CARTESIAN_POINT ( 'NONE',  ( 196.4677102463732012, 290.3549391369982686, 16.45225250689336249 ) ) ;
#28578 = CARTESIAN_POINT ( 'NONE',  ( 69.02995391522775037, 64.48250336152477757, 12.46069185683908387 ) ) ;
#28579 = ORIENTED_EDGE ( 'NONE', *, *, #720, .T. ) ;
#28580 = CARTESIAN_POINT ( 'NONE',  ( 151.4159295687746294, 268.3869122420484814, 14.78076517566594106 ) ) ;
#28581 = CARTESIAN_POINT ( 'NONE',  ( 163.3647850011336971, 247.6908875409073403, 8.475775724498188168 ) ) ;
#28582 = LINE ( 'NONE', #51895, #13565 ) ;
#28583 = CARTESIAN_POINT ( 'NONE',  ( 169.7091093167843496, 266.1397787582689602, -16.87065449823908736 ) ) ;
#28584 = CARTESIAN_POINT ( 'NONE',  ( 197.3149168070693520, 273.2883024837288417, -13.45903248082802506 ) ) ;
#28585 = VERTEX_POINT ( 'NONE', #42678 ) ;
#28586 = CARTESIAN_POINT ( 'NONE',  ( 71.35764812850149497, 70.85251640463194178, 5.283905016801779375 ) ) ;
#28587 = CARTESIAN_POINT ( 'NONE',  ( 168.4891346661264322, 282.2463884888330199, -10.92310856812336795 ) ) ;
#28588 = CARTESIAN_POINT ( 'NONE',  ( 85.82462382841984549, 45.79497946314377543, 8.828125997675229542 ) ) ;
#28589 = DIRECTION ( 'NONE',  ( 0.8660254037844379305, 0.5000000000000015543, 0.000000000000000000 ) ) ;
#28590 = CARTESIAN_POINT ( 'NONE',  ( 184.0101212780497235, 295.6693216559447706, 4.669920232876622279 ) ) ;
#28591 = CARTESIAN_POINT ( 'NONE',  ( 69.04595564537558516, 70.27680155102625292, 2.523699088812808355 ) ) ;
#28592 = CARTESIAN_POINT ( 'NONE',  ( 148.1500140211902874, 275.9675759909871999, -0.0001745395379542502687 ) ) ;
#28593 = CARTESIAN_POINT ( 'NONE',  ( 149.8363775701710381, 271.5102645707438000, -11.76379339081466568 ) ) ;
#28594 = ORIENTED_EDGE ( 'NONE', *, *, #1001, .T. ) ;
#28595 = CARTESIAN_POINT ( 'NONE',  ( 6.768841761084057218, 28.00034080476288878, -1.878358725466461243E-16 ) ) ;
#28596 = CARTESIAN_POINT ( 'NONE',  ( 166.7959447105422157, 276.3626885415273478, 15.91653206054683523 ) ) ;
#28597 = EDGE_LOOP ( 'NONE', ( #36715, #64230 ) ) ;
#28598 = CARTESIAN_POINT ( 'NONE',  ( -22.42236680055709641, 157.8615022471902591, 0.000000000000000000 ) ) ;
#28599 = DIRECTION ( 'NONE',  ( 0.9932214622066130039, -0.1162373735601320568, 0.000000000000000000 ) ) ;
#28600 = CARTESIAN_POINT ( 'NONE',  ( 156.0187427484829641, 261.9439754546441463, -16.96632779721737805 ) ) ;
#28601 = ORIENTED_EDGE ( 'NONE', *, *, #59058, .T. ) ;
#28602 = CARTESIAN_POINT ( 'NONE',  ( 146.8859094598974480, 276.2331372299326517, -0.7994986043261681496 ) ) ;
#28603 = CARTESIAN_POINT ( 'NONE',  ( 185.0260524818428678, 291.7194308270165948, 12.00076202787302826 ) ) ;
#28604 = CARTESIAN_POINT ( 'NONE',  ( 164.2712161151136172, 246.1209027979328710, 7.276091357954241445 ) ) ;
#28605 = CARTESIAN_POINT ( 'NONE',  ( -63.34358462235560694, 38.37368864812747660, 177.5919119679930134 ) ) ;
#28606 = VECTOR ( 'NONE', #28881, 1000.000000000000000 ) ;
#28607 = DIRECTION ( 'NONE',  ( 0.9999986627203610867, -0.001635407438361268905, 0.000000000000000000 ) ) ;
#28608 = ORIENTED_EDGE ( 'NONE', *, *, #98906, .F. ) ;
#28609 = CARTESIAN_POINT ( 'NONE',  ( 95.54687826519547400, 213.7202760586659167, -5.415160957724236172E-17 ) ) ;
#28610 = CARTESIAN_POINT ( 'NONE',  ( 199.9134407114337364, 283.6250491837689651, 17.05367660732407842 ) ) ;
#28611 = AXIS2_PLACEMENT_3D ( 'NONE', #17029, #63637, #84973 ) ;
#28612 = CARTESIAN_POINT ( 'NONE',  ( 178.9462863553024761, 269.7444581634086376, -16.16615938913098205 ) ) ;
#28613 = CARTESIAN_POINT ( 'NONE',  ( 81.41336698633861602, 41.94612678490528168, -7.669352666741279911 ) ) ;
#28614 = ORIENTED_EDGE ( 'NONE', *, *, #40477, .T. ) ;
#28615 = VERTEX_POINT ( 'NONE', #4191 ) ;
#28616 = DIRECTION ( 'NONE',  ( 0.8660254037844382635, 0.5000000000000004441, 0.000000000000000000 ) ) ;
#28617 = ORIENTED_EDGE ( 'NONE', *, *, #70776, .F. ) ;
#28618 = DIRECTION ( 'NONE',  ( 1.000000000000000000, 0.000000000000000000, 0.000000000000000000 ) ) ;
#28620 = ORIENTED_EDGE ( 'NONE', *, *, #79413, .T. ) ;
#28619 = B_SPLINE_CURVE_WITH_KNOTS ( 'NONE', 3,
 ( #29034, #98443, #21424, #52311 ),
 .UNSPECIFIED., .F., .F.,
 ( 4, 4 ),
 ( 0.003118693327000881740, 0.008537184786768493849 ),
 .UNSPECIFIED. ) ;
#28621 = CARTESIAN_POINT ( 'NONE',  ( 76.08510198875326580, 64.37462812208569574, 14.47852601845500509 ) ) ;
#28622 = CARTESIAN_POINT ( 'NONE',  ( 203.0026270830780675, 279.0361311525880978, -16.61345826058821373 ) ) ;
#28623 = VERTEX_POINT ( 'NONE', #35091 ) ;
#28624 = PLANE ( 'NONE',  #83140 ) ;
#28625 = CARTESIAN_POINT ( 'NONE',  ( -22.42236680055709641, 157.8615022471902591, 0.000000000000000000 ) ) ;
#28626 = CARTESIAN_POINT ( 'NONE',  ( 10.91961124514375925, 187.1115022471903160, -5.000000000000047962 ) ) ;
#28627 = CARTESIAN_POINT ( 'NONE',  ( 28.50119043139559238, 18.58380873178787951, 6.180339887498953466 ) ) ;
#28628 = LINE ( 'NONE', #71890, #64014 ) ;
#28629 = ORIENTED_EDGE ( 'NONE', *, *, #44370, .T. ) ;
#28630 = CARTESIAN_POINT ( 'NONE',  ( 76.20553726834548058, 57.21450367305868667, 16.12638719470323778 ) ) ;
#28631 = CARTESIAN_POINT ( 'NONE',  ( 11.06209807803029221, 12.10170272979924988, -7.433330006724141015 ) ) ;
#28632 = ORIENTED_EDGE ( 'NONE', *, *, #50952, .T. ) ;
#28633 = EDGE_CURVE ( 'NONE', #51824, #59759, #82676, .T. ) ;
#28634 = VECTOR ( 'NONE', #78654, 1000.000000000000114 ) ;
#28635 = CARTESIAN_POINT ( 'NONE',  ( 167.4649754880705643, 284.0871937547507287, 9.157884509665418449 ) ) ;
#28637 = ORIENTED_EDGE ( 'NONE', *, *, #549, .T. ) ;
#28636 = CARTESIAN_POINT ( 'NONE',  ( 199.9084271263513983, 270.2648688396561738, 9.879193358459824381 ) ) ;
#28638 = CARTESIAN_POINT ( 'NONE',  ( 203.0337691736598629, 278.9821914694464340, 16.08167820133810011 ) ) ;
#28639 = EDGE_CURVE ( 'NONE', #43030, #179, #73813, .T. ) ;
#28640 = CARTESIAN_POINT ( 'NONE',  ( 186.1788399154933416, 258.1552101551508827, 3.086633325358126623 ) ) ;
#28641 = CARTESIAN_POINT ( 'NONE',  ( 161.3307343759124990, 281.5446215756635979, -6.416395075942769921 ) ) ;
#28642 = DIRECTION ( 'NONE',  ( -0.8660254037844387076, -0.4999999999999998890, -0.000000000000000000 ) ) ;
#28643 = CARTESIAN_POINT ( 'NONE',  ( -19.65312891409030271, 93.06504152958497400, 59.99999999999999289 ) ) ;
#28644 = CARTESIAN_POINT ( 'NONE',  ( 86.51306616006753814, 43.84325935889563652, 4.272406052666638310 ) ) ;
#28645 = CARTESIAN_POINT ( 'NONE',  ( 88.24590225192910964, 44.24085665668349776, -1.852495053617905230 ) ) ;
#28646 = EDGE_LOOP ( 'NONE', ( #72368, #72205, #67576, #58013 ) ) ;
#28647 = CARTESIAN_POINT ( 'NONE',  ( 100.6254093204819497, 222.2365022471901739, -10.00000000000009237 ) ) ;
#28648 = CARTESIAN_POINT ( 'NONE',  ( 74.86346538573359055, 67.47285165321515876, -12.74145591711592118 ) ) ;
#28649 = ORIENTED_EDGE ( 'NONE', *, *, #60897, .F. ) ;
#28651 = ADVANCED_FACE ( 'NONE', ( #77600 ), #8186, .F. ) ;
#28650 = CARTESIAN_POINT ( 'NONE',  ( 193.6136754191833234, 294.1685928848680760, -14.20288964755752126 ) ) ;
#28652 = CARTESIAN_POINT ( 'NONE',  ( 171.6601131003222349, 279.7212932031995933, -14.57934018190033498 ) ) ;
#28653 = CARTESIAN_POINT ( 'NONE',  ( 204.2488672143813346, 276.8775799267394291, -15.19253025301563831 ) ) ;
#28654 = CARTESIAN_POINT ( 'NONE',  ( 84.23654874160455108, 44.64216667711589537, -8.426356101742397797 ) ) ;
#28655 = CARTESIAN_POINT ( 'NONE',  ( 164.7612133174728513, 274.2017939341284318, 14.96666266618639973 ) ) ;
#28657 = CARTESIAN_POINT ( 'NONE',  ( 76.19402696226363503, 65.29190987809512592, 14.49924708549197483 ) ) ;
#28656 = CARTESIAN_POINT ( 'NONE',  ( -1.664820405372784862, 169.8458772461660544, 9.188101187500095079 ) ) ;
#28658 = CARTESIAN_POINT ( 'NONE',  ( 185.1625343664165655, 295.6846680252337478, 8.558017805756747975 ) ) ;
#28659 = VERTEX_POINT ( 'NONE', #25378 ) ;
#28660 = B_SPLINE_CURVE_WITH_KNOTS ( 'NONE', 3,
 ( #37889, #68797, #76898, #44995, #99725, #14117, #52595, #52104, #44496, #61196 ),
 .UNSPECIFIED., .F., .F.,
 ( 4, 2, 2, 2, 4 ),
 ( 0.000000000000000000, 0.2500000000000000000, 0.5000000000000000000, 0.7500000000000000000, 1.000000000000000000 ),
 .UNSPECIFIED. ) ;
#28661 = ORIENTED_EDGE ( 'NONE', *, *, #71424, .F. ) ;
#28662 = DIRECTION ( 'NONE',  ( -0.1860369090531061309, -0.9825427565607343094, 0.000000000000000000 ) ) ;
#28663 = CARTESIAN_POINT ( 'NONE',  ( 190.1363311188550540, 273.6253742232181025, -15.77342137974315683 ) ) ;
#28664 = B_SPLINE_CURVE_WITH_KNOTS ( 'NONE', 3,
 ( #79360, #87490, #41796, #40285 ),
 .UNSPECIFIED., .F., .F.,
 ( 4, 4 ),
 ( 0.01180092279712636506, 0.02028068562175033493 ),
 .UNSPECIFIED. ) ;
#28665 = CARTESIAN_POINT ( 'NONE',  ( 85.57852021786813168, 48.96074862228688573, -12.66870494374460776 ) ) ;
#28666 = EDGE_CURVE ( 'NONE', #98668, #92719, #70474, .T. ) ;
#28667 = CARTESIAN_POINT ( 'NONE',  ( 87.14756827322403865, 44.11579270599533942, 4.133463102786264720 ) ) ;
#28668 = CARTESIAN_POINT ( 'NONE',  ( 85.00801151538682632, 48.68758372926721023, 12.25568936537549902 ) ) ;
#28669 = CARTESIAN_POINT ( 'NONE',  ( 153.1198285439165545, 279.2890930352092482, 3.903594709581249322 ) ) ;
#28670 = B_SPLINE_CURVE_WITH_KNOTS ( 'NONE', 3,
 ( #22017, #100036, #77735, #84853, #99042, #54905, #24007, #31101, #61988, #83866, #38704, #13929, #46288, #54385, #30118, #53894, #15395, #53410, #45311, #29625, #44805, #69612, #75742, #14907, #38193, #45797, #37216, #76247, #85359, #37704, #68116, #92941, #68612, #61000, #46812, #60498, #91971, #76718, #69109, #30623, #92457, #23002, #48832, #80262, #86377, #1221 ),
 .UNSPECIFIED., .F., .F.,
 ( 4, 1, 2, 2, 1, 2, 2, 1, 1, 2, 2, 1, 1, 2, 2, 1, 1, 2, 2, 1, 1, 1, 2, 2, 1, 1, 1, 2, 2, 4 ),
 ( 0.000000000000000000, 0.06249999999998609446, 0.09374999999998014089, 0.1249999999999741873, 0.1874999999999622802, 0.2187499999999571176, 0.2499999999999519829, 0.3124999999999434896, 0.3437499999999402700, 0.3593749999999396039, 0.3749999999999388822, 0.4374999999999416023, 0.4687499999999439892, 0.4843749999999444333, 0.4999999999999448219, 0.5624999999999447109, 0.5937499999999434896, 0.6093749999999437117, 0.6249999999999438227, 0.6874999999999463762, 0.7187499999999478195, 0.7343749999999483746, 0.7421874999999488187, 0.7499999999999491518, 0.8124999999999610312, 0.8437499999999665823, 0.8593749999999694689, 0.8671874999999716893, 0.8749999999999739098, 1.000000000000000000 ),
 .UNSPECIFIED. ) ;
#28671 = CARTESIAN_POINT ( 'NONE',  ( -1.610867365518755978, 176.0024278399160949, 9.188101187500095079 ) ) ;
#28672 = CARTESIAN_POINT ( 'NONE',  ( 124.1796696299359724, 236.3768266524159856, -9.188101187500091527 ) ) ;
#28673 = CARTESIAN_POINT ( 'NONE',  ( 75.28650001057751240, 66.67572118895704136, 13.44401380721711270 ) ) ;
#28674 = CARTESIAN_POINT ( 'NONE',  ( 181.4013813872246317, 255.1929875330831123, -2.500114065624810866 ) ) ;
#28675 = CARTESIAN_POINT ( 'NONE',  ( 79.34762228877008283, 58.72377720057313866, 16.21937645494816849 ) ) ;
#28676 = CARTESIAN_POINT ( 'NONE',  ( 47.32807415326522715, 108.5480133836684900, 10.00000000000000000 ) ) ;
#28677 = AXIS2_PLACEMENT_3D ( 'NONE', #16479, #62559, #23563 ) ;
#28678 = CARTESIAN_POINT ( 'NONE',  ( 82.92870420767373218, 52.52116137057526402, -14.95649373007994498 ) ) ;
#28679 = VECTOR ( 'NONE', #8033, 1000.000000000000000 ) ;
#28680 = CARTESIAN_POINT ( 'NONE',  ( 193.7114073116034945, 295.1289958610702797, 14.86160832869823345 ) ) ;
#28681 = CARTESIAN_POINT ( 'NONE',  ( 161.0965315767822972, 251.6196177163260188, -13.76772246540905442 ) ) ;
#28682 = CARTESIAN_POINT ( 'NONE',  ( 194.4666154385731431, 293.8209370148700827, -14.56896502715340702 ) ) ;
#28683 = DIRECTION ( 'NONE',  ( 0.8660254037844384856, 0.5000000000000002220, 0.000000000000000000 ) ) ;
#28684 = EDGE_CURVE ( 'NONE', #20915, #14295, #90767, .T. ) ;
#28685 = EDGE_CURVE ( 'NONE', #80346, #38805, #70404, .T. ) ;
#28686 = B_SPLINE_CURVE_WITH_KNOTS ( 'NONE', 3,
 ( #16020, #31213, #38810, #69716, #62099, #25112, #70207, #17519, #55011, #77841, #93046, #47901, #17011, #94556, #78338, #94063 ),
 .UNSPECIFIED., .F., .F.,
 ( 4, 1, 2, 2, 2, 1, 2, 2, 4 ),
 ( 0.000000000000000000, 0.1250000000000011657, 0.1875000000000017486, 0.2500000000000023315, 0.5000000000000039968, 0.6250000000000033307, 0.6875000000000033307, 0.7500000000000032196, 1.000000000000000000 ),
 .UNSPECIFIED. ) ;
#28687 = CARTESIAN_POINT ( 'NONE',  ( 84.13554962843576845, 50.44679214584963489, 13.72453037626170058 ) ) ;
#28688 = CARTESIAN_POINT ( 'NONE',  ( 192.7212156920602411, 265.2891116966523555, 7.789557535538737199 ) ) ;
#28689 = CARTESIAN_POINT ( 'NONE',  ( -14.83262083840143575, 124.7156766241961208, 21.50000000000006750 ) ) ;
#28690 = CARTESIAN_POINT ( 'NONE',  ( 162.3216050867536353, 251.8533766904920128, -12.94731468463284330 ) ) ;
#28691 = DIRECTION ( 'NONE',  ( -0.8660254037844387076, -0.4999999999999998890, -0.000000000000000000 ) ) ;
#28692 = EDGE_CURVE ( 'NONE', #37486, #2973, #98233, .T. ) ;
#28693 = AXIS2_PLACEMENT_3D ( 'NONE', #17579, #40854, #38843 ) ;
#28694 = LINE ( 'NONE', #13513, #67566 ) ;
#28695 = B_SPLINE_CURVE_WITH_KNOTS ( 'NONE', 3,
 ( #57779, #80642, #12710, #65882, #43063, #5583, #27401, #42570, #81143, #4591, #51175, #88755, #34979, #59257, #98304, #11709, #81628, #20299, #19327, #35975, #82140, #43581, #11219, #74005, #90235, #50190, #73503, #44063, #20804, #4087, #58282, #89258, #73018, #12201, #34488, #57281, #42086, #51697, #82647, #19808, #66878, #50675, #96331, #97318, #74515, #3610, #13205, #65389, #35485, #27886 ),
 .UNSPECIFIED., .F., .F.,
 ( 4, 2, 2, 2, 2, 2, 2, 2, 2, 2, 2, 2, 2, 2, 2, 2, 2, 2, 2, 2, 2, 2, 2, 2, 4 ),
 ( 0.0001844887274763776805, 0.001204547440118925936, 0.001714576796440233199, 0.001842084135520550203, 0.001969591474600867424, 0.002097098813681184427, 0.002224606152761501865, 0.002479620830922128066, 0.002734635509082753834, 0.003244664865404003201, 0.004264723578046429944, 0.005284782290688856687, 0.005794811647010033630, 0.006049826325170582636, 0.006304841003331129907, 0.006368594672871270845, 0.006432348342411410916, 0.006496102011951550986, 0.006559855681491691057, 0.006814870359652014549, 0.007324899715972662401, 0.007579914394132985893, 0.007834929072293307650, 0.008089943750453632010, 0.008344958428613956369 ),
 .UNSPECIFIED. ) ;
#28696 = CARTESIAN_POINT ( 'NONE',  ( 88.83448719433606300, 234.3464784336661353, 1.353441290958777327E-15 ) ) ;
#28697 = EDGE_CURVE ( 'NONE', #50302, #50839, #74504, .T. ) ;
#28698 = CARTESIAN_POINT ( 'NONE',  ( 6.194340351808173217, 26.68290643055185285, 3.479690158560446702E-15 ) ) ;
#28699 = CARTESIAN_POINT ( 'NONE',  ( 150.6571681785161445, 269.7011255207979730, 15.24894850018880454 ) ) ;
#28700 = EDGE_CURVE ( 'NONE', #73728, #56872, #34965, .T. ) ;
#28701 = DIRECTION ( 'NONE',  ( -0.000000000000000000, -0.000000000000000000, -1.000000000000000000 ) ) ;
#28703 = CARTESIAN_POINT ( 'NONE',  ( 199.8015111840774125, 284.5806265305737952, 18.33369416908775662 ) ) ;
#28702 = CARTESIAN_POINT ( 'NONE',  ( 157.2168982216852555, 258.3393398020932636, 18.09635675623264106 ) ) ;
#28704 = CARTESIAN_POINT ( 'NONE',  ( 75.99079911453461023, 65.46731794264749738, 14.35477091480207612 ) ) ;
#28705 = CARTESIAN_POINT ( 'NONE',  ( 203.8348497297200765, 275.8166909402214628, -13.89836469095587823 ) ) ;
#28706 = CARTESIAN_POINT ( 'NONE',  ( 41.44275701717578642, 32.43085787977767609, -9.188101187500008038 ) ) ;
#28707 = CARTESIAN_POINT ( 'NONE',  ( 6.117390533544194930, 29.33055864014943026, 10.00000000000000000 ) ) ;
#28708 = FACE_BOUND ( 'NONE', #80870, .T. ) ;
#28709 = ORIENTED_EDGE ( 'NONE', *, *, #28064, .T. ) ;
#28710 = CARTESIAN_POINT ( 'NONE',  ( 18.97660828663255117, 29.14336893147755703, 7.433330006724141015 ) ) ;
#28711 = AXIS2_PLACEMENT_3D ( 'NONE', #2128, #9218, #1122 ) ;
#28712 = CARTESIAN_POINT ( 'NONE',  ( 172.4964346338612984, 290.8364761718990508, -0.5259165075563734248 ) ) ;
#28713 = CARTESIAN_POINT ( 'NONE',  ( 147.5749551500760788, 275.0396750858066639, -4.254929048021584670 ) ) ;
#28714 = CARTESIAN_POINT ( 'NONE',  ( 191.7192842763342071, 288.0556307037572310, -15.81806397776715301 ) ) ;
#28715 = B_SPLINE_CURVE_WITH_KNOTS ( 'NONE', 3,
 ( #60736, #37448, #14173, #45548, #76481, #68358, #23249, #92218, #54642, #38949, #54137, #99773, #70355, #69361, #91698, #61749, #77479, #100280, #29865, #7555, #39436, #967, #15646, #62747, #45058, #92699, #93703, #76955, #8076, #22261, #69854, #53647, #23746, #467, #84603, #30366, #37940, #46038, #16163, #7058, #31356, #55143, #47061, #75999, #68852, #30866, #62239, #77974, #24266, #99283 ),
 .UNSPECIFIED., .F., .F.,
 ( 4, 2, 2, 2, 2, 2, 2, 2, 2, 2, 2, 2, 2, 2, 2, 2, 2, 2, 2, 2, 2, 2, 2, 2, 4 ),
 ( 0.0001446224335138595609, 0.0006466149904454740081, 0.001148607547377088591, 0.001399603825842918054, 0.001650600104308747517, 0.001776098243541699437, 0.001901596382774651574, 0.002027094522007603494, 0.002152592661240555413, 0.002403588939706498718, 0.002654585218172442456, 0.003156577775104445292, 0.004160562888968516448, 0.005164548002832586304, 0.005666540559764621232, 0.005917536838230639563, 0.006043034977463642224, 0.006168533116696644884, 0.006231282186313106750, 0.006294031255929570350, 0.006419529395162546989, 0.006670525673628498534, 0.007172518230560363459, 0.007674510787492226649, 0.008176503344424091574 ),
 .UNSPECIFIED. ) ;
#28716 = EDGE_CURVE ( 'NONE', #39441, #55671, #22672, .T. ) ;
#28717 = EDGE_CURVE ( 'NONE', #21425, #53525, #91942, .T. ) ;
#28718 = ORIENTED_EDGE ( 'NONE', *, *, #13269, .F. ) ;
#28719 = CARTESIAN_POINT ( 'NONE',  ( 70.98043770365947580, 61.04086187986361978, 14.52140827553137470 ) ) ;
#28720 = CARTESIAN_POINT ( 'NONE',  ( 159.9014600375868440, 253.6895423408921886, 15.57825579621527368 ) ) ;
#28721 = CARTESIAN_POINT ( 'NONE',  ( 157.7933305902885195, 268.4007073483575141, 16.64277213758561658 ) ) ;
#28722 = CARTESIAN_POINT ( 'NONE',  ( 170.0991740787100923, 252.5905740194307327, -8.760565947542348297 ) ) ;
#28723 = CARTESIAN_POINT ( 'NONE',  ( 137.7923328995641157, 240.3615022471902023, 5.000000000000051514 ) ) ;
#28724 = CARTESIAN_POINT ( 'NONE',  ( 157.8043799545718286, 257.3217915922150496, -17.97575562758749257 ) ) ;
#28725 = AXIS2_PLACEMENT_3D ( 'NONE', #82594, #13160, #29835 ) ;
#28726 = ORIENTED_EDGE ( 'NONE', *, *, #22460, .F. ) ;
#28727 = LINE ( 'NONE', #89580, #52044 ) ;
#28728 = ORIENTED_EDGE ( 'NONE', *, *, #63552, .T. ) ;
#28729 = CARTESIAN_POINT ( 'NONE',  ( 69.61542750552385428, 62.56132062511078828, -13.94275833699888700 ) ) ;
#28730 = CYLINDRICAL_SURFACE ( 'NONE', #20672, 17.82106496071139645 ) ;
#28731 = ORIENTED_EDGE ( 'NONE', *, *, #42578, .T. ) ;
#28732 = CARTESIAN_POINT ( 'NONE',  ( 87.83526388831070619, 44.46237794634081553, 3.930408651391872343 ) ) ;
#28733 = ORIENTED_EDGE ( 'NONE', *, *, #60320, .T. ) ;
#28734 = CARTESIAN_POINT ( 'NONE',  ( 163.2942584940569191, 258.1478583562382028, 16.77787020301746779 ) ) ;
#28735 = CARTESIAN_POINT ( 'NONE',  ( 158.4880851235930947, 256.1375795020725263, 17.48246009260925860 ) ) ;
#28736 = CARTESIAN_POINT ( 'NONE',  ( 84.74507488503365948, 50.24295689512916141, 13.81875560728438224 ) ) ;
#28737 = CARTESIAN_POINT ( 'NONE',  ( 193.0920876067732195, 296.2016890559648914, -13.46848876679793072 ) ) ;
#28738 = CARTESIAN_POINT ( 'NONE',  ( -24.92793671336084671, 23.00358903956173862, -10.00000000000000000 ) ) ;
#28739 = DIRECTION ( 'NONE',  ( -1.000000000000000000, 0.000000000000000000, 0.000000000000000000 ) ) ;
#28740 = CARTESIAN_POINT ( 'NONE',  ( 44.10936046141050326, 26.26216523072498532, -2.296566073217252530E-15 ) ) ;
#28741 = CARTESIAN_POINT ( 'NONE',  ( 72.02429414335679780, 60.85727294438741808, -14.84082463543404806 ) ) ;
#28742 = DIRECTION ( 'NONE',  ( -0.000000000000000000, -0.000000000000000000, -1.000000000000000000 ) ) ;
#28743 = LINE ( 'NONE', #98667, #15721 ) ;
#28744 = ORIENTED_EDGE ( 'NONE', *, *, #11365, .T. ) ;
#28745 = ORIENTED_EDGE ( 'NONE', *, *, #51700, .F. ) ;
#28746 = FACE_OUTER_BOUND ( 'NONE', #20921, .T. ) ;
#28748 = CARTESIAN_POINT ( 'NONE',  ( 147.6264044922760377, 274.9505622111005323, -8.841872555777701592 ) ) ;
#28747 = CARTESIAN_POINT ( 'NONE',  ( 174.2782839474101877, 256.8459632085913995, -12.31768510484773493 ) ) ;
#28749 = CARTESIAN_POINT ( 'NONE',  ( 204.1162911604698138, 275.2177209574938388, 13.42500254428782114 ) ) ;
#28750 = CARTESIAN_POINT ( 'NONE',  ( 66.48373673643996540, 68.79225009967480275, -2.167545776629342225 ) ) ;
#28751 = DIRECTION ( 'NONE',  ( -0.4055404667435467125, 0.9140770918436946779, 0.000000000000000000 ) ) ;
#28752 = FACE_OUTER_BOUND ( 'NONE', #70059, .T. ) ;
#28753 = VECTOR ( 'NONE', #15068, 1000.000000000000000 ) ;
#28754 = CARTESIAN_POINT ( 'NONE',  ( 171.0032295034350511, 287.8336240595702407, -4.402522906269554781 ) ) ;
#28755 = FACE_OUTER_BOUND ( 'NONE', #67536, .T. ) ;
#28756 = CARTESIAN_POINT ( 'NONE',  ( 195.1474640768281290, 265.6393084148356252, -8.887799905196541062 ) ) ;
#28757 = CARTESIAN_POINT ( 'NONE',  ( 100.0117143358702236, 237.7369531367911009, -4.594050593750048428 ) ) ;
#28758 = ORIENTED_EDGE ( 'NONE', *, *, #4394, .T. ) ;
#28759 = CARTESIAN_POINT ( 'NONE',  ( 6.212693912817788267, 48.26412221380545731, 59.99999999999999289 ) ) ;
#28760 = CARTESIAN_POINT ( 'NONE',  ( 165.6389704105113481, 271.1804200721081202, 16.38369493522007758 ) ) ;
#28761 = CARTESIAN_POINT ( 'NONE',  ( 190.8551004859573084, 274.8686381574206621, 15.92302825397800703 ) ) ;
#28762 = VERTEX_POINT ( 'NONE', #27874 ) ;
#28763 = VERTEX_POINT ( 'NONE', #89726 ) ;
#28764 = CARTESIAN_POINT ( 'NONE',  ( 87.13833003848017711, 45.89157147215227894, -8.651152695689850347 ) ) ;
#28766 = B_SPLINE_SURFACE_WITH_KNOTS ( 'NONE', 3, 1, ( 
 ( #31911, #79574 ),
 ( #2032, #95285 ),
 ( #59185, #51104 ),
 ( #81076, #82069 ),
 ( #18735, #43509 ),
 ( #74448, #50123 ),
 ( #88686, #35910 ),
 ( #97739, #51619 ),
 ( #11151, #42020 ),
 ( #72954, #11642 ),
 ( #42501, #34906 ),
 ( #96766, #92522 ),
 ( #36401, #70169 ),
 ( #62060, #16480 ),
 ( #53476, #30184 ),
 ( #78299, #15981 ),
 ( #92040, #39257 ),
 ( #15464, #7897 ),
 ( #70678, #69678 ),
 ( #31663, #32176 ),
 ( #63080, #13136 ),
 ( #11411, #63579 ),
 ( #3309, #9902 ),
 ( #88449, #56478 ),
 ( #55953, #86949 ),
 ( #26093, #34674 ),
 ( #19008, #65576 ),
 ( #17482, #96524 ),
 ( #86446, #40760 ),
 ( #78799, #18000 ),
 ( #9386, #43761 ),
 ( #59446, #50869 ),
 ( #43260, #90925 ),
 ( #50374, #51366 ) ),
 .UNSPECIFIED., .T., .F., .F.,
 ( 4, 2, 2, 2, 2, 2, 2, 2, 2, 2, 2, 2, 2, 2, 2, 2, 4 ),
 ( 2, 2 ),
 ( 0.000000000000000000, 0.06250000000000000000, 0.1250000000000000000, 0.1875000000000000000, 0.2500000000000000000, 0.3125000000000000000, 0.3750000000000000000, 0.4375000000000000000, 0.5000000000000000000, 0.5625000000000000000, 0.6250000000000000000, 0.6875000000000000000, 0.7500000000000000000, 0.8125000000000000000, 0.8750000000000000000, 0.9375000000000000000, 1.000000000000000000 ),
 ( 0.000000000000000000, 1.000000000000000000 ),
 .UNSPECIFIED. ) ;
#28765 = PLANE ( 'NONE',  #94887 ) ;
#28767 = CARTESIAN_POINT ( 'NONE',  ( 157.8849654228661166, 257.1822134667773980, 17.43614750057631468 ) ) ;
#28768 = CARTESIAN_POINT ( 'NONE',  ( 159.2122473525774069, 254.8832937285494609, -16.22689353966294590 ) ) ;
#28769 = DIRECTION ( 'NONE',  ( -0.9302793824855987159, 0.3668518372888613377, 0.000000000000000000 ) ) ;
#28770 = VERTEX_POINT ( 'NONE', #27386 ) ;
#28771 = ORIENTED_EDGE ( 'NONE', *, *, #33847, .T. ) ;
#28772 = CARTESIAN_POINT ( 'NONE',  ( 41.82599275875796963, 62.29945068332010294, -10.00000000000000000 ) ) ;
#28773 = ORIENTED_EDGE ( 'NONE', *, *, #49606, .T. ) ;
#28774 = EDGE_CURVE ( 'NONE', #30966, #34443, #72245, .T. ) ;
#28775 = AXIS2_PLACEMENT_3D ( 'NONE', #76690, #62983, #84332 ) ;
#28776 = CARTESIAN_POINT ( 'NONE',  ( 72.46511837996449401, 71.56249752072032777, 6.234640293157917235 ) ) ;
#28777 = CARTESIAN_POINT ( 'NONE',  ( 96.42157766939700991, 233.1427522451419065, -10.00000000000009592 ) ) ;
#28778 = CARTESIAN_POINT ( 'NONE',  ( 192.2881909306969135, 261.2467072465593105, -0.09875216535559103170 ) ) ;
#28780 = CARTESIAN_POINT ( 'NONE',  ( 69.59366227530321680, 62.45191379327602732, -13.42933426267537378 ) ) ;
#28779 = CARTESIAN_POINT ( 'NONE',  ( 186.7564666940997711, 290.4926955665019932, -13.42819013091626523 ) ) ;
#28781 = DIRECTION ( 'NONE',  ( 0.05364311403569549386, 0.9985601716053735810, 0.000000000000000000 ) ) ;
#28782 = ORIENTED_EDGE ( 'NONE', *, *, #84009, .F. ) ;
#28783 = AXIS2_PLACEMENT_3D ( 'NONE', #48066, #40457, #71393 ) ;
#28784 = CARTESIAN_POINT ( 'NONE',  ( 204.8176812644112204, 275.8923650920285695, 14.65594551021579051 ) ) ;
#28786 = CARTESIAN_POINT ( 'NONE',  ( 82.27576515736316765, 50.79558287279384388, 14.36463698561768965 ) ) ;
#28785 = B_SPLINE_SURFACE_WITH_KNOTS ( 'NONE', 3, 1, ( 
 ( #4644, #27931 ),
 ( #12762, #22328 ),
 ( #98356, #76062 ),
 ( #97365, #53228 ),
 ( #29434, #51222 ),
 ( #74056, #98858 ),
 ( #29928, #91762 ),
 ( #20857, #58815 ),
 ( #28945, #45124 ),
 ( #51749, #89777 ),
 ( #99349, #66440 ),
 ( #6131, #60803 ),
 ( #83675, #35537 ),
 ( #75546, #82691 ),
 ( #20353, #37515 ),
 ( #6641, #82191 ),
 ( #28426, #83169 ),
 ( #59822, #43627 ),
 ( #75054, #68422 ),
 ( #52716, #12254 ),
 ( #66925, #14238 ),
 ( #43111, #67936 ),
 ( #74566, #5144 ),
 ( #36025, #60309 ),
 ( #97856, #5630 ),
 ( #21831, #90788 ),
 ( #59308, #37028 ),
 ( #36524, #90288 ),
 ( #13257, #44117 ),
 ( #67424, #21339 ),
 ( #52224, #44610 ),
 ( #13732, #91266 ),
 ( #1547, #85690 ),
 ( #53710, #47119 ) ),
 .UNSPECIFIED., .T., .F., .F.,
 ( 4, 2, 2, 2, 2, 2, 2, 2, 2, 2, 2, 2, 2, 2, 2, 2, 4 ),
 ( 2, 2 ),
 ( 0.000000000000000000, 0.06250000000000000000, 0.1250000000000000000, 0.1875000000000000000, 0.2500000000000000000, 0.3125000000000000000, 0.3750000000000000000, 0.4375000000000000000, 0.5000000000000000000, 0.5625000000000000000, 0.6250000000000000000, 0.6875000000000000000, 0.7500000000000000000, 0.8125000000000000000, 0.8750000000000000000, 0.9375000000000000000, 1.000000000000000000 ),
 ( 0.000000000000000000, 1.000000000000000000 ),
 .UNSPECIFIED. ) ;
#28787 = CARTESIAN_POINT ( 'NONE',  ( 190.3734512952871967, 263.7599240487260204, -9.676642372964348482 ) ) ;
#28788 = CARTESIAN_POINT ( 'NONE',  ( 170.4175250103361066, 248.6523554852190330, -0.2712260920720951929 ) ) ;
#28789 = EDGE_CURVE ( 'NONE', #75521, #58073, #58271, .T. ) ;
#28790 = CARTESIAN_POINT ( 'NONE',  ( 72.14611019483686505, 72.30310738408833515, 3.684292749196569350 ) ) ;
#28791 = EDGE_CURVE ( 'NONE', #14425, #26183, #28567, .T. ) ;
#28792 = CARTESIAN_POINT ( 'NONE',  ( 199.0994567031226836, 281.8932881784735969, -16.60211735284051215 ) ) ;
#28793 = DIRECTION ( 'NONE',  ( 0.1710100716628310258, -0.2961981327260192476, 0.9396926207859104263 ) ) ;
#28794 = CARTESIAN_POINT ( 'NONE',  ( 80.82203068068015739, 54.54264130141514499, 15.85416842091752088 ) ) ;
#28795 = CIRCLE ( 'NONE', #14192, 70.00000000000001421 ) ;
#28796 = CARTESIAN_POINT ( 'NONE',  ( 206.5441577893546992, 271.9902398542315609, 7.330342545849478419 ) ) ;
#28797 = CARTESIAN_POINT ( 'NONE',  ( 62.52896555438372417, 219.1589784336661637, -6.496448406907675876E-16 ) ) ;
#28798 = CARTESIAN_POINT ( 'NONE',  ( 159.3451320108506764, 254.6531307488737355, -16.72997986213134425 ) ) ;
#28799 = CARTESIAN_POINT ( 'NONE',  ( 77.72205534048291042, 61.52847525230062331, 16.09962475150208761 ) ) ;
#28800 = CARTESIAN_POINT ( 'NONE',  ( 163.0424334805279045, 248.2492167524936804, -9.671494865076915914 ) ) ;
#28801 = CARTESIAN_POINT ( 'NONE',  ( 66.66342508697569258, 67.67433879810246822, 6.129251300726017426 ) ) ;
#28802 = CARTESIAN_POINT ( 'NONE',  ( 161.2488013048736377, 251.3558788108169040, -13.10044423494716170 ) ) ;
#28803 = CARTESIAN_POINT ( 'NONE',  ( 74.39841895140679640, 68.21392270468032848, 11.95628786500076579 ) ) ;
#28805 = CARTESIAN_POINT ( 'NONE',  ( -20.77164714902255582, 95.17350844815184985, 45.19940618238346275 ) ) ;
#28804 = CARTESIAN_POINT ( 'NONE',  ( 73.65879925253982208, 69.67557606723219976, -9.540597966332084567 ) ) ;
#28806 = CARTESIAN_POINT ( 'NONE',  ( 113.4714528099510744, 242.9865022471902876, -10.00000000000009592 ) ) ;
#28807 = CARTESIAN_POINT ( 'NONE',  ( 44.13025152078434132, 25.28848085856235173, 1.475505719884397138E-15 ) ) ;
#28808 = DIRECTION ( 'NONE',  ( -0.4999999999999995004, -0.8660254037844389297, -2.816764622163176506E-16 ) ) ;
#28809 = CARTESIAN_POINT ( 'NONE',  ( 157.6838031512220368, 270.7765766995603940, -14.92570125826960847 ) ) ;
#28810 = CARTESIAN_POINT ( 'NONE',  ( 71.76780065431621836, 72.18842372171909005, 3.264426277842173096 ) ) ;
#28811 = EDGE_CURVE ( 'NONE', #64867, #17145, #74991, .T. ) ;
#28812 = CARTESIAN_POINT ( 'NONE',  ( 30.97368554763575688, 182.5643266524159856, -9.188101187500093303 ) ) ;
#28813 = AXIS2_PLACEMENT_3D ( 'NONE', #10897, #24577, #71712 ) ;
#28814 = B_SPLINE_CURVE_WITH_KNOTS ( 'NONE', 3,
 ( #46218, #23934, #77667, #93890 ),
 .UNSPECIFIED., .F., .F.,
 ( 4, 4 ),
 ( 0.009363228237252623279, 0.01502890388146836675 ),
 .UNSPECIFIED. ) ;
#28815 = EDGE_CURVE ( 'NONE', #73927, #75268, #12482, .T. ) ;
#28816 = CARTESIAN_POINT ( 'NONE',  ( 157.4177733328310467, 257.9914139036126812, 18.29188238796808363 ) ) ;
#28817 = CARTESIAN_POINT ( 'NONE',  ( 199.4570567059534767, 277.6076089953632504, 15.22630486869836908 ) ) ;
#28818 = EDGE_CURVE ( 'NONE', #88861, #86378, #12698, .T. ) ;
#28819 = CARTESIAN_POINT ( 'NONE',  ( 197.6456421031980994, 287.3858497455466932, 17.15283754821559015 ) ) ;
#28820 = CARTESIAN_POINT ( 'NONE',  ( 71.75070072382382591, 72.06332698807560178, -1.650535781253756662 ) ) ;
#28821 = CARTESIAN_POINT ( 'NONE',  ( 45.45211389745056607, 206.2369531367911293, -4.594050593750048428 ) ) ;
#28822 = B_SPLINE_CURVE_WITH_KNOTS ( 'NONE', 3,
 ( #72654, #47800, #16911, #94456 ),
 .UNSPECIFIED., .F., .F.,
 ( 4, 4 ),
 ( 0.007537832009283896087, 0.01334040069055882592 ),
 .UNSPECIFIED. ) ;
#28823 = CIRCLE ( 'NONE', #14290, 70.00000000000001421 ) ;
#28824 = CARTESIAN_POINT ( 'NONE',  ( 20.59861825492957621, 33.93396525600390845, 2.839279412974139660 ) ) ;
#28825 = CARTESIAN_POINT ( 'NONE',  ( 171.5036904379427654, 286.7056378984830758, 7.451739084606072261 ) ) ;
#28826 = CARTESIAN_POINT ( 'NONE',  ( 48.98007068238331385, 88.97864505566217019, -10.00000000000000000 ) ) ;
#28827 = CARTESIAN_POINT ( 'NONE',  ( 46.41032958717836010, 27.76426979415094110, 3.090169943749476733 ) ) ;
#28828 = CARTESIAN_POINT ( 'NONE',  ( 202.9431422976768715, 270.0791902996022031, -6.592389727497273810 ) ) ;
#28829 = CARTESIAN_POINT ( 'NONE',  ( 176.0175147867288672, 291.2181479268968474, 2.555819555636972940 ) ) ;
#28830 = AXIS2_PLACEMENT_3D ( 'NONE', #3729, #87401, #58395 ) ;
#28831 = ADVANCED_FACE ( 'NONE', ( #57269 ), #12188, .T. ) ;
#28832 = CARTESIAN_POINT ( 'NONE',  ( 180.1023429053202847, 276.2675729333262780, 17.20643721484194799 ) ) ;
#28833 = CARTESIAN_POINT ( 'NONE',  ( 182.2148741171517088, 280.9993675977776206, -17.23122524679219225 ) ) ;
#28834 = CARTESIAN_POINT ( 'NONE',  ( 70.08428920641576099, 67.88371280376459538, -9.044488858928271924 ) ) ;
#28835 = CARTESIAN_POINT ( 'NONE',  ( 163.3019570347943841, 255.9604400728466373, -14.88202733670140887 ) ) ;
#28836 = EDGE_CURVE ( 'NONE', #28142, #54381, #49578, .T. ) ;
#28837 = CARTESIAN_POINT ( 'NONE',  ( 48.95103868752454446, 97.61288834769685252, 10.00000000000000000 ) ) ;
#28838 = AXIS2_PLACEMENT_3D ( 'NONE', #6799, #69587, #8300 ) ;
#28839 = CARTESIAN_POINT ( 'NONE',  ( 100.4810717531844944, 235.4865022471902876, -10.00000000000009415 ) ) ;
#28840 = CARTESIAN_POINT ( 'NONE',  ( 161.1027382213887336, 251.6088674925233022, 13.55451100897754557 ) ) ;
#28841 = CARTESIAN_POINT ( 'NONE',  ( 164.8959392045564982, 270.4400157944439798, -16.73020286746915630 ) ) ;
#28842 = ORIENTED_EDGE ( 'NONE', *, *, #54076, .T. ) ;
#28843 = CARTESIAN_POINT ( 'NONE',  ( 55.76366273096530080, 196.8768266524160140, 9.188101187500098632 ) ) ;
#28844 = ORIENTED_EDGE ( 'NONE', *, *, #21881, .T. ) ;
#28845 = CARTESIAN_POINT ( 'NONE',  ( 166.5588711558999364, 264.7233108584221100, 17.65853493413723641 ) ) ;
#28846 = DIRECTION ( 'NONE',  ( -0.000000000000000000, -0.000000000000000000, -1.000000000000000000 ) ) ;
#28847 = FACE_OUTER_BOUND ( 'NONE', #9432, .T. ) ;
#28848 = ORIENTED_EDGE ( 'NONE', *, *, #1251, .T. ) ;
#28849 = VECTOR ( 'NONE', #57931, 1000.000000000000000 ) ;
#28850 = CYLINDRICAL_SURFACE ( 'NONE', #2046, 17.82106496071139645 ) ;
#28851 = CARTESIAN_POINT ( 'NONE',  ( 79.27712787825650764, 45.82676469203064329, -12.41914995154098200 ) ) ;
#28852 = CARTESIAN_POINT ( 'NONE',  ( 193.9796946036068164, 292.6643086402947915, -15.64068455845557537 ) ) ;
#28853 = CARTESIAN_POINT ( 'NONE',  ( 176.9539730356219138, 274.6341514097922527, -16.77391188311105452 ) ) ;
#28854 = CARTESIAN_POINT ( 'NONE',  ( 42.87860686303044844, 124.5258428655388911, 10.00000000000000000 ) ) ;
#28855 = CARTESIAN_POINT ( 'NONE',  ( 204.7088172315186512, 276.0809231281156144, 13.09496711537969027 ) ) ;
#28856 = ORIENTED_EDGE ( 'NONE', *, *, #56228, .F. ) ;
#28857 = B_SPLINE_CURVE_WITH_KNOTS ( 'NONE', 3,
 ( #534, #55212, #16233, #30930, #22333, #92282, #31917, #16730, #62309, #54712, #8139, #31420, #32434, #38520, #14733, #8635, #92764, #38008, #85175, #7629, #84184, #45616, #46620, #69920, #24335, #9136, #22829 ),
 .UNSPECIFIED., .F., .F.,
 ( 4, 2, 2, 2, 1, 1, 2, 2, 1, 2, 2, 1, 2, 2, 1, 4 ),
 ( 0.3033294829601337894, 0.4774971122201073781, 0.4992680658776057490, 0.5101535427063552675, 0.5210390195351046749, 0.5645809268500957545, 0.6081228341650868341, 0.6298937878225825404, 0.6516647414800782467, 0.7387485561100566311, 0.7822904634250469336, 0.8258323707400372360, 0.8693742780550275384, 0.8911452317125228006, 0.9129161853700180629, 1.000000000000000000 ),
 .UNSPECIFIED. ) ;
#28858 = CARTESIAN_POINT ( 'NONE',  ( 23.32475077058400004, 14.26216523072494446, -2.296566073217252530E-15 ) ) ;
#28859 = CARTESIAN_POINT ( 'NONE',  ( 76.18316680938646357, 61.09795948472795857, 15.59353031967901693 ) ) ;
#28860 = CARTESIAN_POINT ( 'NONE',  ( 167.3911405578172946, 287.7797177684797134, -2.777254742693934020 ) ) ;
#28861 = CARTESIAN_POINT ( 'NONE',  ( 74.97996761797445231, 67.38724533294663388, -12.85106452774880381 ) ) ;
#28862 = VERTEX_POINT ( 'NONE', #60246 ) ;
#28863 = LINE ( 'NONE', #51664, #90286 ) ;
#28864 = CARTESIAN_POINT ( 'NONE',  ( 166.9564976376358061, 261.4857389862473269, 16.50069698162775467 ) ) ;
#28865 = CARTESIAN_POINT ( 'NONE',  ( 159.2289198208967775, 254.8544161663325838, -15.88961297684315888 ) ) ;
#28866 = EDGE_LOOP ( 'NONE', ( #1858, #47831 ) ) ;
#28867 = VERTEX_POINT ( 'NONE', #99287 ) ;
#28868 = AXIS2_PLACEMENT_3D ( 'NONE', #97172, #20639, #89583 ) ;
#28870 = CARTESIAN_POINT ( 'NONE',  ( 61.98910963369213789, 195.0494855054051584, -2.679491924311248496 ) ) ;
#28869 = CARTESIAN_POINT ( 'NONE',  ( 71.97460576983348801, 66.57329172194043565, 12.17197637779258734 ) ) ;
#28871 = CARTESIAN_POINT ( 'NONE',  ( 162.6757594134126350, 248.8843148665554281, -10.86406770146305867 ) ) ;
#28872 = CARTESIAN_POINT ( 'NONE',  ( 66.17027418025043062, 69.18316985973861222, -2.056876225022604920 ) ) ;
#28873 = CARTESIAN_POINT ( 'NONE',  ( 176.3865323452404823, 258.8737835494043225, 13.24306684835586623 ) ) ;
#28874 = CARTESIAN_POINT ( 'NONE',  ( -19.65312891409030271, 93.06504152958497400, 20.00000000000000355 ) ) ;
#28875 = CARTESIAN_POINT ( 'NONE',  ( 161.0313979157349991, 262.9719707653000000, -17.46358780386706400 ) ) ;
#28876 = EDGE_CURVE ( 'NONE', #33752, #34753, #44716, .T. ) ;
#28877 = CARTESIAN_POINT ( 'NONE',  ( 120.4987145680870952, 246.5024278399160949, 9.188101187500095079 ) ) ;
#28878 = FACE_OUTER_BOUND ( 'NONE', #61862, .T. ) ;
#28879 = VERTEX_POINT ( 'NONE', #98797 ) ;
#28880 = CARTESIAN_POINT ( 'NONE',  ( 170.1749377657032198, 264.1434158296717101, 16.24854282405526718 ) ) ;
#28881 = DIRECTION ( 'NONE',  ( -0.000000000000000000, -1.000000000000000000, -0.000000000000000000 ) ) ;
#28882 = VECTOR ( 'NONE', #14229, 1000.000000000000000 ) ;
#28883 = VERTEX_POINT ( 'NONE', #45063 ) ;
#28884 = CARTESIAN_POINT ( 'NONE',  ( 201.0536821592508829, 281.7069444607843138, 16.57790100734148453 ) ) ;
#28885 = EDGE_LOOP ( 'NONE', ( #22772, #90427, #71121, #54766, #28352 ) ) ;
#28886 = ORIENTED_EDGE ( 'NONE', *, *, #66514, .T. ) ;
#28887 = FACE_BOUND ( 'NONE', #48527, .T. ) ;
#28888 = CARTESIAN_POINT ( 'NONE',  ( 75.31813185017509227, 66.77598452293851494, -12.96073926456471881 ) ) ;
#28889 = CARTESIAN_POINT ( 'NONE',  ( 194.4891008911482118, 284.8786197582770114, 17.21347455856521691 ) ) ;
#28890 = CARTESIAN_POINT ( 'NONE',  ( -31.21596018254677674, 96.31576462380481018, 12.43553956882932354 ) ) ;
#28891 =( BOUNDED_CURVE ( )  B_SPLINE_CURVE ( 2, ( #68839, #31344, #55129, #84590, #75986, #85608, #15632, #15128, #77962 ),
 .UNSPECIFIED., .F., .T. ) 
 B_SPLINE_CURVE_WITH_KNOTS ( ( 3, 2, 2, 2, 3 ),
 ( 0.9233870967741935054, 0.9247311827956988806, 0.9274193548387096309, 0.9301075268817203812, 0.9314516129032257563 ),
 .UNSPECIFIED. ) 
 CURVE ( )  GEOMETRIC_REPRESENTATION_ITEM ( )  RATIONAL_B_SPLINE_CURVE ( ( 0.9330127018922194093, 0.9330127018922194093, 1.000000000000000000, 0.8660254037844387076, 1.000000000000000000, 0.8660254037844387076, 1.000000000000000000, 0.9330127018922194093, 0.9330127018922194093 ) ) 
 REPRESENTATION_ITEM ( '' )  );
#28892 = CARTESIAN_POINT ( 'NONE',  ( 81.65957865058895493, 55.81781964966066312, 16.00564737419913186 ) ) ;
#28893 = CARTESIAN_POINT ( 'NONE',  ( 155.1376601545389917, 261.9406857754215707, 18.55063430030667959 ) ) ;
#28894 = CARTESIAN_POINT ( 'NONE',  ( 72.92667516200663158, 70.31269505470191916, 8.108358915573942838 ) ) ;
#28895 = CARTESIAN_POINT ( 'NONE',  ( 87.70668618551661666, 45.11329565042249357, 6.837976445409226223 ) ) ;
#28896 = ORIENTED_EDGE ( 'NONE', *, *, #58915, .F. ) ;
#28897 = CARTESIAN_POINT ( 'NONE',  ( 73.59724665734155735, 63.41105048715310488, -14.19156318116282378 ) ) ;
#28898 = CARTESIAN_POINT ( 'NONE',  ( 201.2535035105529744, 282.0657020489176716, -18.08976065250591958 ) ) ;
#28899 = CARTESIAN_POINT ( 'NONE',  ( 155.6569868912636991, 261.0411854816857158, -17.75433477650897984 ) ) ;
#28900 = AXIS2_PLACEMENT_3D ( 'NONE', #18354, #41626, #72568 ) ;
#28901 = VERTEX_POINT ( 'NONE', #84608 ) ;
#28902 = CARTESIAN_POINT ( 'NONE',  ( 72.51315417358483728, 69.83750700119627197, -8.417205730241819950 ) ) ;
#28903 = CARTESIAN_POINT ( 'NONE',  ( 76.06215586834144915, 51.32791385274359186, -15.64516872477013365 ) ) ;
#28904 = CARTESIAN_POINT ( 'NONE',  ( 164.1492509520389831, 246.7605600116641540, 4.961886042938450814 ) ) ;
#28905 = EDGE_CURVE ( 'NONE', #94224, #56024, #93414, .T. ) ;
#28906 = VECTOR ( 'NONE', #99966, 1000.000000000000227 ) ;
#28907 = CARTESIAN_POINT ( 'NONE',  ( 80.41801566324240014, 54.65175397312741978, 16.29095433313647234 ) ) ;
#28908 = AXIS2_PLACEMENT_3D ( 'NONE', #32511, #2115, #70496 ) ;
#28909 = CARTESIAN_POINT ( 'NONE',  ( 164.7297297678022403, 245.3267338555121455, 3.020078936458732599 ) ) ;
#28910 = CARTESIAN_POINT ( 'NONE',  ( 195.2792143904551949, 279.2177904473068679, 16.31973602825316405 ) ) ;
#28911 = CARTESIAN_POINT ( 'NONE',  ( 164.1146561143383167, 246.3920726737087534, -7.362905700427413436 ) ) ;
#28912 = AXIS2_PLACEMENT_3D ( 'NONE', #1455, #56118, #70843 ) ;
#28913 = CARTESIAN_POINT ( 'NONE',  ( 141.8249372320439647, 246.5643266524160140, 9.188101187500095079 ) ) ;
#28914 = VERTEX_POINT ( 'NONE', #92703 ) ;
#28915 = CARTESIAN_POINT ( 'NONE',  ( 87.98321614449201888, 44.37542847539244661, 4.756797044073172387 ) ) ;
#28916 = CARTESIAN_POINT ( 'NONE',  ( 86.01542015185120249, 44.31831041030510221, 6.184598332866396930 ) ) ;
#28917 = PLANE ( 'NONE',  #46464 ) ;
#28918 = EDGE_CURVE ( 'NONE', #24285, #690, #63239, .T. ) ;
#28919 = CARTESIAN_POINT ( 'NONE',  ( 72.80104277311302496, 70.83185719937777947, 7.190015310759124034 ) ) ;
#28920 = EDGE_CURVE ( 'NONE', #91209, #17524, #89835, .T. ) ;
#28921 = CARTESIAN_POINT ( 'NONE',  ( 178.4631826488540867, 254.6961106986615562, 4.321611361837887522 ) ) ;
#28922 = VERTEX_POINT ( 'NONE', #46549 ) ;
#28923 = CARTESIAN_POINT ( 'NONE',  ( 77.19380876746809861, 58.51342845908217072, 16.11897871819916972 ) ) ;
#28924 = AXIS2_PLACEMENT_3D ( 'NONE', #13798, #21408, #29016 ) ;
#28925 = CARTESIAN_POINT ( 'NONE',  ( -17.33262083840143930, 129.0458036431182904, 30.52142883766505221 ) ) ;
#28926 = CARTESIAN_POINT ( 'NONE',  ( 72.60433947765299934, 71.50525637487901065, -5.566970196651008784 ) ) ;
#28927 = CARTESIAN_POINT ( 'NONE',  ( 81.51711570496432557, 54.24218815797082982, 15.69287892032614273 ) ) ;
#28928 = CARTESIAN_POINT ( 'NONE',  ( 182.3988913246011521, 262.5264951803217741, -13.38846801953669008 ) ) ;
#28929 = CARTESIAN_POINT ( 'NONE',  ( 147.5848197185516142, 275.0225891520124151, 4.420251097676741736 ) ) ;
#28930 = CARTESIAN_POINT ( 'NONE',  ( 182.8533132515951536, 280.6317719585726422, 16.86240594373356672 ) ) ;
#28931 = CARTESIAN_POINT ( 'NONE',  ( 204.7764732025852084, 275.9637395487929439, -14.02287343454361412 ) ) ;
#28932 = CARTESIAN_POINT ( 'NONE',  ( 192.8825254575952499, 268.5331795959783676, 12.33565966346110265 ) ) ;
#28933 = CARTESIAN_POINT ( 'NONE',  ( 21.80251038182309387, 34.36126292948896577, 6.180339887498949913 ) ) ;
#28934 = DIRECTION ( 'NONE',  ( -0.9999990636452668058, -0.001368469433204066998, 0.000000000000000000 ) ) ;
#28935 = CARTESIAN_POINT ( 'NONE',  ( 21.35627990119762032, 12.73415679381821519, 1.333680081654574804E-15 ) ) ;
#28936 = DIRECTION ( 'NONE',  ( 0.4999999999999998890, -0.8660254037844385966, 0.000000000000000000 ) ) ;
#28937 = CARTESIAN_POINT ( 'NONE',  ( 159.6610344727618269, 254.1059716346071866, 15.33388637456589620 ) ) ;
#28938 = CARTESIAN_POINT ( 'NONE',  ( 207.2594843487139542, 271.6630380879379345, 5.140243983758119306 ) ) ;
#28939 = EDGE_CURVE ( 'NONE', #31618, #2827, #6070, .T. ) ;
#28940 = CARTESIAN_POINT ( 'NONE',  ( -10.43332761869022640, 164.7833772461660544, -9.188101187500095079 ) ) ;
#28941 = CARTESIAN_POINT ( 'NONE',  ( 175.3356445731998008, 284.9523473448756477, -12.04348899028328468 ) ) ;
#28942 = ORIENTED_EDGE ( 'NONE', *, *, #65390, .T. ) ;
#28943 = CARTESIAN_POINT ( 'NONE',  ( 66.61927972294286349, 68.05145527290748930, -6.517764413741313767 ) ) ;
#28944 = CARTESIAN_POINT ( 'NONE',  ( 72.84756190538607257, 70.91156448913385191, -7.844936087786372525 ) ) ;
#28945 = CARTESIAN_POINT ( 'NONE',  ( 199.2205425252482200, 285.5868937652708155, -18.05012564782189344 ) ) ;
#28946 = CARTESIAN_POINT ( 'NONE',  ( 12.08367997547019002, 165.5327760586659451, 1.948934522072302763E-15 ) ) ;
#28947 = CARTESIAN_POINT ( 'NONE',  ( 181.8637735408910316, 276.0006342513588606, -16.50086996363865666 ) ) ;
#28948 = CARTESIAN_POINT ( 'NONE',  ( 23.31615823149838462, 29.16454794089042579, -10.00000000000000355 ) ) ;
#28949 = CARTESIAN_POINT ( 'NONE',  ( -13.86269525828471672, 104.2312461070085021, 43.89948692389422291 ) ) ;
#28950 = CARTESIAN_POINT ( 'NONE',  ( 71.81202244518927102, 202.2677522451417929, -5.000000000000041744 ) ) ;
#28951 = DIRECTION ( 'NONE',  ( 0.000000000000000000, 0.000000000000000000, 1.000000000000000000 ) ) ;
#28952 = CARTESIAN_POINT ( 'NONE',  ( -50.44023328799576689, 80.54804368980198603, -10.00000000000000000 ) ) ;
#28953 = CARTESIAN_POINT ( 'NONE',  ( 196.3825633952734790, 269.6078319146020021, -10.80602553522919251 ) ) ;
#28954 = EDGE_CURVE ( 'NONE', #94086, #99632, #68073, .T. ) ;
#28955 = CARTESIAN_POINT ( 'NONE',  ( 82.36042285506233895, 42.91861834903688333, 8.349967097983880038 ) ) ;
#28956 = CARTESIAN_POINT ( 'NONE',  ( 198.0167861310041530, 287.6718610000373246, 18.15276047493383160 ) ) ;
#28957 = CARTESIAN_POINT ( 'NONE',  ( 180.3483110632917885, 294.3099715515549519, 1.024573422989016880 ) ) ;
#28958 = CARTESIAN_POINT ( 'NONE',  ( 48.51954752611815991, 205.4865022471903444, -10.00000000000009415 ) ) ;
#28959 = CARTESIAN_POINT ( 'NONE',  ( 70.99909089399695006, 61.09348569631758608, 14.50421621802051853 ) ) ;
#28960 = CARTESIAN_POINT ( 'NONE',  ( 190.5444288681022442, 300.6143634316900943, -1.000014190476072873 ) ) ;
#28961 = AXIS2_PLACEMENT_3D ( 'NONE', #67650, #11978, #66657 ) ;
#28962 = CARTESIAN_POINT ( 'NONE',  ( 11.05475416482865114, 183.3149278399160664, 9.188101187500093303 ) ) ;
#28963 = CARTESIAN_POINT ( 'NONE',  ( 164.2764444823383769, 284.8899537207625485, 4.278381809041608363 ) ) ;
#28964 = CARTESIAN_POINT ( 'NONE',  ( 79.40635770460171727, 59.70624924693522928, 16.17064410388787365 ) ) ;
#28965 = CARTESIAN_POINT ( 'NONE',  ( 45.07042791025775585, 28.94754757982093452, 5.678558825948272215 ) ) ;
#28966 = CARTESIAN_POINT ( 'NONE',  ( 202.1632097545547424, 279.9122701607644785, -15.78860785990872451 ) ) ;
#28968 = CARTESIAN_POINT ( 'NONE',  ( 164.6460902696047128, 245.4716017159096566, -3.036414139157908476 ) ) ;
#28967 = CIRCLE ( 'NONE', #96913, 60.00000000000002132 ) ;
#28969 = DIRECTION ( 'NONE',  ( 0.5000000000000048850, -0.8660254037844358210, 0.000000000000000000 ) ) ;
#28970 = CARTESIAN_POINT ( 'NONE',  ( 92.93017357788669131, 158.0650415295850735, 36.50000000000000000 ) ) ;
#28971 = CARTESIAN_POINT ( 'NONE',  ( 161.8743800460768796, 280.4803551579017267, 8.950406917861062794 ) ) ;
#28972 = CARTESIAN_POINT ( 'NONE',  ( 0.000000000000000000, 0.000000000000000000, 0.000000000000000000 ) ) ;
#28974 = EDGE_CURVE ( 'NONE', #57520, #64780, #60740, .T. ) ;
#28973 = AXIS2_PLACEMENT_3D ( 'NONE', #28280, #36883, #52082 ) ;
#28975 = CARTESIAN_POINT ( 'NONE',  ( 17.75393198606386136, 12.11110640527291160, -2.839279412974138328 ) ) ;
#28976 = CARTESIAN_POINT ( 'NONE',  ( 71.49724145223211735, 72.36708001998829332, 1.062265253749092420 ) ) ;
#28977 = CARTESIAN_POINT ( 'NONE',  ( 82.95708619573620979, 53.58516627418447342, 15.69712586674409849 ) ) ;
#28978 = CARTESIAN_POINT ( 'NONE',  ( 71.41016749218992743, 59.45273978182969188, 15.69346469621916995 ) ) ;
#28979 = CARTESIAN_POINT ( 'NONE',  ( 155.6518451030846961, 261.0500913200531841, 17.91778754207898317 ) ) ;
#28980 = ORIENTED_EDGE ( 'NONE', *, *, #44182, .T. ) ;
#28981 = VECTOR ( 'NONE', #70898, 1000.000000000000000 ) ;
#28982 = CARTESIAN_POINT ( 'NONE',  ( -19.65312891409030271, 93.06504152958497400, 177.5919119679930134 ) ) ;
#28983 = CARTESIAN_POINT ( 'NONE',  ( 2.953350652821653988, 23.74646525600387648, 2.839279412974139660 ) ) ;
#28984 = CARTESIAN_POINT ( 'NONE',  ( 81.11978968823368064, 42.58148117026868107, 7.963302174025969293 ) ) ;
#28985 = ORIENTED_EDGE ( 'NONE', *, *, #29297, .F. ) ;
#28986 = CARTESIAN_POINT ( 'NONE',  ( 196.2472167001637899, 289.0877869373891826, -17.11100897825607348 ) ) ;
#28987 = CARTESIAN_POINT ( 'NONE',  ( 67.23170740046823823, 69.33908408813277902, 1.348601409716759347 ) ) ;
#28988 = CARTESIAN_POINT ( 'NONE',  ( 76.81132113734133782, 63.87275317464699498, 14.88576141942193942 ) ) ;
#28989 = CARTESIAN_POINT ( 'NONE',  ( 154.9528145190857344, 262.2608478075840708, -17.26679351315302213 ) ) ;
#28990 = VERTEX_POINT ( 'NONE', #67876 ) ;
#28991 = AXIS2_PLACEMENT_3D ( 'NONE', #86861, #94433, #23989 ) ;
#28992 = ORIENTED_EDGE ( 'NONE', *, *, #86110, .F. ) ;
#28994 = CARTESIAN_POINT ( 'NONE',  ( -25.89332989531674301, 24.59406508915897760, -10.00000000000000000 ) ) ;
#28993 = LINE ( 'NONE', #84710, #34128 ) ;
#28995 = B_SPLINE_CURVE_WITH_KNOTS ( 'NONE', 3,
 ( #12765, #50729, #19381, #12257, #35541, #97370, #73555, #5147, #27936, #89780, #20356, #50240, #51226, #81194, #82194, #36028 ),
 .UNSPECIFIED., .F., .F.,
 ( 4, 1, 2, 2, 2, 1, 2, 2, 4 ),
 ( 0.000000000000000000, 0.1250000000000036360, 0.1875000000000049405, 0.2500000000000062728, 0.5000000000000048850, 0.6250000000000044409, 0.6875000000000039968, 0.7500000000000035527, 1.000000000000000000 ),
 .UNSPECIFIED. ) ;
#28996 = CARTESIAN_POINT ( 'NONE',  ( 152.6757560589063303, 266.2048287524194166, 16.73757896668104195 ) ) ;
#28997 = EDGE_LOOP ( 'NONE', ( #5071, #94941, #48935, #1508 ) ) ;
#28998 = CARTESIAN_POINT ( 'NONE',  ( 88.36865033182888851, 43.96674011622069855, -2.220889795100837283 ) ) ;
#28999 = CARTESIAN_POINT ( 'NONE',  ( 80.50291573656390653, 57.83591419990552396, 16.24909409233076119 ) ) ;
#29000 = CARTESIAN_POINT ( 'NONE',  ( 16.79905537663784898, 192.0530062829863311, -4.648177544792955347E-16 ) ) ;
#29002 = ORIENTED_EDGE ( 'NONE', *, *, #38710, .T. ) ;
#29001 = ADVANCED_FACE ( 'NONE', ( #59758 ), #45553, .F. ) ;
#29003 = CARTESIAN_POINT ( 'NONE',  ( 87.34722152284756191, 44.99461385121256285, -6.156066689881265930 ) ) ;
#29004 = CARTESIAN_POINT ( 'NONE',  ( 197.0226655822963551, 289.3937282992477549, -17.28982543158101493 ) ) ;
#29005 = VECTOR ( 'NONE', #77811, 999.9999999999998863 ) ;
#29006 = ORIENTED_EDGE ( 'NONE', *, *, #46394, .F. ) ;
#29007 = CARTESIAN_POINT ( 'NONE',  ( 206.2456893945931142, 273.4189824569319285, 10.13882547285618152 ) ) ;
#29008 = CARTESIAN_POINT ( 'NONE',  ( 82.86586985908988368, 152.2544130683315871, 0.000000000000000000 ) ) ;
#29009 = PRODUCT ( 'Screw-Connected Movable Jaw', 'Screw-Connected Movable Jaw', '', ( #65967 ) ) ;
#29010 = ORIENTED_EDGE ( 'NONE', *, *, #54181, .F. ) ;
#29011 = CARTESIAN_POINT ( 'NONE',  ( 174.6285408418798966, 276.7099930269583865, -16.43498402137660364 ) ) ;
#29012 = CARTESIAN_POINT ( 'NONE',  ( 172.2074374934617822, 264.1263164429906283, -15.87731566018440965 ) ) ;
#29013 = ORIENTED_EDGE ( 'NONE', *, *, #99963, .F. ) ;
#29014 = CARTESIAN_POINT ( 'NONE',  ( 158.6437384181921573, 274.8702825545737483, -13.55642847048332200 ) ) ;
#29015 = CARTESIAN_POINT ( 'NONE',  ( 57.56414817410228579, 217.3207943907112281, -18.47570218321542868 ) ) ;
#29016 = DIRECTION ( 'NONE',  ( 0.000000000000000000, 0.000000000000000000, -1.000000000000000000 ) ) ;
#29017 = ORIENTED_EDGE ( 'NONE', *, *, #5586, .T. ) ;
#29018 = ORIENTED_EDGE ( 'NONE', *, *, #15629, .T. ) ;
#29019 = CARTESIAN_POINT ( 'NONE',  ( 81.62548306449865265, 50.91212887389385600, -15.04074333791695572 ) ) ;
#29020 = CARTESIAN_POINT ( 'NONE',  ( 87.75573343511427993, 43.92582870660319827, 1.242921438624202901 ) ) ;
#29021 = CARTESIAN_POINT ( 'NONE',  ( 147.1249913145849177, 275.8190353104462815, 3.637773609013635223 ) ) ;
#29022 = CARTESIAN_POINT ( 'NONE',  ( 188.6203220463457626, 298.5727710222585074, -4.346736981754744100 ) ) ;
#29023 = CARTESIAN_POINT ( 'NONE',  ( 148.9694607950094394, 272.6243204573405592, 11.81236034532910573 ) ) ;
#29024 = CARTESIAN_POINT ( 'NONE',  ( 152.9920137376499838, 265.6570543845515431, 16.15798175643282164 ) ) ;
#29025 = CARTESIAN_POINT ( 'NONE',  ( 191.4409630708763927, 299.0615206417621721, 9.874182956795676702 ) ) ;
#29026 = CARTESIAN_POINT ( 'NONE',  ( 191.6723191112861855, 298.6608002251342100, -9.737039817265848995 ) ) ;
#29027 = ORIENTED_EDGE ( 'NONE', *, *, #2276, .F. ) ;
#29028 = CARTESIAN_POINT ( 'NONE',  ( 74.41611649102104309, 57.90871829712388319, -15.94991086904226663 ) ) ;
#29029 = DIRECTION ( 'NONE',  ( 0.000000000000000000, -0.000000000000000000, 1.000000000000000000 ) ) ;
#29031 = DIRECTION ( 'NONE',  ( -0.5000000000000002220, 0.8660254037844385966, 0.000000000000000000 ) ) ;
#29030 = CARTESIAN_POINT ( 'NONE',  ( 149.7200635338602410, 271.3242383773507527, -12.12223662813266500 ) ) ;
#29032 = DIRECTION ( 'NONE',  ( 0.000000000000000000, 0.000000000000000000, 1.000000000000000000 ) ) ;
#29033 = CARTESIAN_POINT ( 'NONE',  ( 168.4907652997964931, 286.4387392943589816, 4.072501019507571485 ) ) ;
#29034 = CARTESIAN_POINT ( 'NONE',  ( 163.8070446421170629, 255.0663642890118581, -15.42060242571707818 ) ) ;
#29035 = ORIENTED_EDGE ( 'NONE', *, *, #54003, .F. ) ;
#29036 = CARTESIAN_POINT ( 'NONE',  ( 205.7456069296021894, 269.2916946144356416, -2.908540672199198429 ) ) ;
#29037 = CARTESIAN_POINT ( 'NONE',  ( 78.05657720352552076, 53.54917886275364225, -15.89405086258497235 ) ) ;
#29038 = CARTESIAN_POINT ( 'NONE',  ( 148.7862567239304781, 273.6578808824901898, 8.926082407994170964 ) ) ;
#29039 = CARTESIAN_POINT ( 'NONE',  ( 79.43493723186259103, 45.78179558321050990, 12.93201222421020447 ) ) ;
#29040 = EDGE_CURVE ( 'NONE', #56569, #79042, #85275, .T. ) ;
#29041 = CARTESIAN_POINT ( 'NONE',  ( 180.3999454879367192, 283.0679475345629612, -15.21805286706472060 ) ) ;
#29042 = ADVANCED_FACE ( 'NONE', ( #14674 ), #30870, .T. ) ;
#29043 = CYLINDRICAL_SURFACE ( 'NONE', #95213, 10.00000000000001066 ) ;
#29044 = VERTEX_POINT ( 'NONE', #15651 ) ;
#29045 = CARTESIAN_POINT ( 'NONE',  ( 208.3764315856425640, 269.7284287242038658, -1.833640725398759441 ) ) ;
#29046 = CARTESIAN_POINT ( 'NONE',  ( 85.08842198125357470, 45.78556742147969771, 10.02268771122703050 ) ) ;
#29047 = EDGE_CURVE ( 'NONE', #78500, #77084, #16042, .T. ) ;
#29048 = CARTESIAN_POINT ( 'NONE',  ( 164.9836323268835940, 244.8869617230113249, -2.696511969808454534 ) ) ;
#29049 = EDGE_CURVE ( 'NONE', #6804, #40677, #13679, .T. ) ;
#29050 = CARTESIAN_POINT ( 'NONE',  ( 57.45043449909734079, 190.6427522451417644, 1.119607411625061291E-15 ) ) ;
#29051 = CARTESIAN_POINT ( 'NONE',  ( 118.9835172072293403, 233.3768266524159571, -9.188101187500093303 ) ) ;
#29052 = CARTESIAN_POINT ( 'NONE',  ( 66.22544472841278207, 69.36168339246577830, 0.1681495645362227065 ) ) ;
#29053 = VECTOR ( 'NONE', #62067, 1000.000000000000227 ) ;
#29054 = DIRECTION ( 'NONE',  ( -0.5888918169447132644, 0.8082118706970061739, 0.000000000000000000 ) ) ;
#29055 = CARTESIAN_POINT ( 'NONE',  ( 192.7874605187217014, 292.5376213369709149, 15.36506066506490598 ) ) ;
#29056 = CARTESIAN_POINT ( 'NONE',  ( 35.84507844392322085, 185.3768266524159856, -9.188101187500091527 ) ) ;
#29057 = CARTESIAN_POINT ( 'NONE',  ( 147.6207062567320918, 275.4717883725331831, -2.882099113126173950 ) ) ;
#29058 = VECTOR ( 'NONE', #76550, 1000.000000000000000 ) ;
#29059 = ORIENTED_EDGE ( 'NONE', *, *, #45821, .T. ) ;
#29060 = CARTESIAN_POINT ( 'NONE',  ( 9.025180670817464446, 166.0177522451418213, 5.000000000000051514 ) ) ;
#29061 = CARTESIAN_POINT ( 'NONE',  ( 180.0656950739936519, 267.0717194386327833, 15.04285446902010293 ) ) ;
#29062 = CARTESIAN_POINT ( 'NONE',  ( 70.43250933021919025, 71.30870369305561951, -0.6892231058542993560 ) ) ;
#29063 = CARTESIAN_POINT ( 'NONE',  ( 167.6146168596400514, 252.8497314824998909, -12.44459218179994231 ) ) ;
#29064 = CARTESIAN_POINT ( 'NONE',  ( 81.85620833974131472, 41.16559107020475494, -5.619287453036919011 ) ) ;
#29065 = CARTESIAN_POINT ( 'NONE',  ( 185.9240074134731060, 297.6458951198301861, -5.725235308961436509 ) ) ;
#29066 = VECTOR ( 'NONE', #81499, 1000.000000000000000 ) ;
#29067 = CARTESIAN_POINT ( 'NONE',  ( 74.14312167556930433, 66.30466486950707861, 1.224646799147354045E-15 ) ) ;
#29068 = CARTESIAN_POINT ( 'NONE',  ( 181.8543694586977324, 262.7755081626895048, 12.52910138123640671 ) ) ;
#29069 = CARTESIAN_POINT ( 'NONE',  ( 97.28760307318144385, 233.6427522451419065, 10.00000000000009237 ) ) ;
#29070 = B_SPLINE_SURFACE_WITH_KNOTS ( 'NONE', 3, 1, ( 
 ( #23711, #39903 ),
 ( #53617, #15111 ),
 ( #8534, #69329 ),
 ( #14637, #46004 ),
 ( #76922, #61221 ),
 ( #92665, #31322 ),
 ( #93670, #7521 ),
 ( #93161, #38414 ),
 ( #935, #99746 ),
 ( #55112, #30331 ),
 ( #37909, #86099 ),
 ( #92185, #32327 ),
 ( #16130, #100250 ),
 ( #7025, #30832 ),
 ( #23218, #47028 ),
 ( #77945, #39406 ),
 ( #70321, #9031 ),
 ( #24722, #31811 ),
 ( #85064, #15612 ),
 ( #62711, #77448 ),
 ( #46510, #8044 ),
 ( #24234, #16625 ),
 ( #63228, #94170 ),
 ( #47521, #78449 ),
 ( #45517, #70835 ),
 ( #1447, #76448 ),
 ( #55605, #19031 ),
 ( #26611, #66598 ),
 ( #5305, #58483 ),
 ( #17124, #4816 ),
 ( #57487, #78963 ) ),
 .UNSPECIFIED., .F., .F., .F.,
 ( 4, 3, 3, 3, 3, 3, 3, 3, 3, 3, 4 ),
 ( 2, 2 ),
 ( 0.000000000000000000, 0.1122669598086679377, 0.2243161639709564115, 0.3396355846218893637, 0.4553962076585015284, 0.5677860799922294088, 0.6749047109689492174, 0.7773884377078165153, 0.8775581155833958036, 0.9782364162377762407, 1.000000000000000000 ),
 ( 0.000000000000000000, 1.000000000000000000 ),
 .UNSPECIFIED. ) ;
#29071 = ORIENTED_EDGE ( 'NONE', *, *, #11354, .T. ) ;
#29072 = CARTESIAN_POINT ( 'NONE',  ( 79.31081143133006606, 59.61002059306026268, -16.52811874246031465 ) ) ;
#29073 = CARTESIAN_POINT ( 'NONE',  ( 202.2773826701151165, 280.2922913237452462, 16.62862787739668846 ) ) ;
#29074 = CARTESIAN_POINT ( 'NONE',  ( 162.7738416911812180, 248.7144313781379310, -11.09964294874192525 ) ) ;
#29075 = AXIS2_PLACEMENT_3D ( 'NONE', #18522, #88472, #19034 ) ;
#29076 = CARTESIAN_POINT ( 'NONE',  ( 11.65032017781297036, 177.5333772461660544, 9.188101187500095079 ) ) ;
#29077 = CARTESIAN_POINT ( 'NONE',  ( 11.84292332949202020, 15.03677371833799903, 10.00000000000000533 ) ) ;
#29078 = CARTESIAN_POINT ( 'NONE',  ( 192.1269172743776892, 272.3004713032796644, 14.80205975413855946 ) ) ;
#29079 = CARTESIAN_POINT ( 'NONE',  ( 71.65615954623328321, 59.54154983785703337, -15.70934178226849731 ) ) ;
#29080 = CARTESIAN_POINT ( 'NONE',  ( 5.871984111234073822, 29.22396284167520619, 10.00000000000000000 ) ) ;
#29082 = CARTESIAN_POINT ( 'NONE',  ( 62.82726920452340380, 197.8923013555409796, 4.594050593750050204 ) ) ;
#29081 = CARTESIAN_POINT ( 'NONE',  ( 194.8372111074683914, 274.9995225832199708, -16.05741363709758573 ) ) ;
#29083 = CARTESIAN_POINT ( 'NONE',  ( 208.2555382576270233, 269.9378221106229034, 3.215405476967123199 ) ) ;
#29084 = CARTESIAN_POINT ( 'NONE',  ( 72.49015541307309718, 57.42129546939775508, 15.82701281140211691 ) ) ;
#29085 = CARTESIAN_POINT ( 'NONE',  ( 67.96351782124591523, 66.04854104595484898, 9.746239896112580681 ) ) ;
#29086 = CARTESIAN_POINT ( 'NONE',  ( 207.6727254509676186, 270.9472835030587703, 7.315149605389819953 ) ) ;
#29087 = VERTEX_POINT ( 'NONE', #76485 ) ;
#29088 = CARTESIAN_POINT ( 'NONE',  ( 13.95070015838929400, 188.8615022471903160, 5.000000000000046185 ) ) ;
#29089 = CARTESIAN_POINT ( 'NONE',  ( 207.5583741822599393, 271.1453457103705205, 3.140867606700001424 ) ) ;
#29090 = CARTESIAN_POINT ( 'NONE',  ( 144.9103262809084924, 242.2202760586659167, -5.415160957724236172E-17 ) ) ;
#29091 = CARTESIAN_POINT ( 'NONE',  ( 19.06802872841732466, 31.98502408145592568, -5.678558825948271327 ) ) ;
#29092 = PLANE ( 'NONE',  #31314 ) ;
#29093 = DIRECTION ( 'NONE',  ( -0.000000000000000000, -0.000000000000000000, 1.000000000000000000 ) ) ;
#29094 = CARTESIAN_POINT ( 'NONE',  ( -23.32062891409032090, 78.77562236714182120, 59.99999999999999289 ) ) ;
#29096 = CARTESIAN_POINT ( 'NONE',  ( 75.28650001057752661, 66.67572118895705557, 13.44401380721711270 ) ) ;
#29095 = CARTESIAN_POINT ( 'NONE',  ( 88.23680129110753967, 43.93620611740951176, 2.496076054743395556 ) ) ;
#29097 = CARTESIAN_POINT ( 'NONE',  ( 68.97219946460526785, 64.39425464503430874, 12.50242288874033392 ) ) ;
#29098 = ORIENTED_EDGE ( 'NONE', *, *, #75358, .F. ) ;
#29099 = CARTESIAN_POINT ( 'NONE',  ( 82.93017357788673394, 175.3855496052738374, 21.50000000000000000 ) ) ;
#29100 = CARTESIAN_POINT ( 'NONE',  ( 163.3607625274802899, 247.6978546696471710, 7.891137406151327305 ) ) ;
#29101 = ADVANCED_FACE ( 'NONE', ( #78485 ), #82024, .F. ) ;
#29102 = CARTESIAN_POINT ( 'NONE',  ( 81.82036482989325066, 42.35048943672428834, -7.944650131338364396 ) ) ;
#29103 = FACE_OUTER_BOUND ( 'NONE', #91220, .T. ) ;
#29104 = CARTESIAN_POINT ( 'NONE',  ( 196.5746262556701822, 272.7668379574431015, -13.37129446457116622 ) ) ;
#29105 = ORIENTED_EDGE ( 'NONE', *, *, #14355, .F. ) ;
#29106 = CARTESIAN_POINT ( 'NONE',  ( 69.66188720561194714, 68.19766641142308572, 8.278177376932148945 ) ) ;
#29107 = DIRECTION ( 'NONE',  ( 0.9505498757754579087, -0.3105719460338643434, 0.000000000000000000 ) ) ;
#29108 = CARTESIAN_POINT ( 'NONE',  ( 82.21410988452117863, 40.73976263626466476, 3.762362152834610729 ) ) ;
#29109 = CARTESIAN_POINT ( 'NONE',  ( 196.1715942132062764, 270.9921725689870868, 12.26687914476305608 ) ) ;
#29110 = CARTESIAN_POINT ( 'NONE',  ( -22.42236680055709641, 157.8615022471902591, 0.000000000000000000 ) ) ;
#29111 = CARTESIAN_POINT ( 'NONE',  ( 13.13128053955749408, 45.28703501410428345, 59.99999999999999289 ) ) ;
#29112 = LINE ( 'NONE', #64233, #66139 ) ;
#29113 = CARTESIAN_POINT ( 'NONE',  ( 43.63646518856938172, 66.22046553916848666, -10.00000000000000000 ) ) ;
#29114 = CARTESIAN_POINT ( 'NONE',  ( 8.500892568652933079, 29.00034080476289233, -1.878358725466461243E-16 ) ) ;
#29115 = CARTESIAN_POINT ( 'NONE',  ( 191.8610655169697452, 287.8363447181971537, -15.91263000500258507 ) ) ;
#29116 = ORIENTED_EDGE ( 'NONE', *, *, #19468, .F. ) ;
#29117 = FACE_OUTER_BOUND ( 'NONE', #19293, .T. ) ;
#29118 = ADVANCED_FACE ( 'NONE', ( #24271 ), #39440, .F. ) ;
#29119 = CARTESIAN_POINT ( 'NONE',  ( -13.11024591527734628, 27.99999999999999645, 32.50000000000000000 ) ) ;
#29120 = CARTESIAN_POINT ( 'NONE',  ( 80.06222361221591655, 45.69665893710951821, -11.99569225509787351 ) ) ;
#29121 = ORIENTED_EDGE ( 'NONE', *, *, #93118, .T. ) ;
#29122 = VECTOR ( 'NONE', #50433, 1000.000000000000000 ) ;
#29123 = CARTESIAN_POINT ( 'NONE',  ( 191.5893301551938350, 298.8045413135534432, -8.323356515452589477 ) ) ;
#29124 = DIRECTION ( 'NONE',  ( 0.9619696745371171254, -0.2731562652969042326, 0.000000000000000000 ) ) ;
#29125 = CARTESIAN_POINT ( 'NONE',  ( 204.3574891606595827, 276.6894411969685166, 13.41627538812899978 ) ) ;
#29126 = FACE_OUTER_BOUND ( 'NONE', #6547, .T. ) ;
#29127 = VERTEX_POINT ( 'NONE', #31360 ) ;
#29128 = CARTESIAN_POINT ( 'NONE',  ( 82.93520977470207356, 212.5643266524159856, -9.188101187500093303 ) ) ;
#29129 = CARTESIAN_POINT ( 'NONE',  ( 198.7134558283731280, 282.8386145195935910, 17.66748989068429054 ) ) ;
#29130 = CARTESIAN_POINT ( 'NONE',  ( 178.5276804562001871, 269.4738238426553494, -16.27363614876470166 ) ) ;
#29131 = CARTESIAN_POINT ( 'NONE',  ( 81.27662216513620308, 42.46107531295264437, -7.622153486729677851 ) ) ;
#29132 = VERTEX_POINT ( 'NONE', #49076 ) ;
#29133 = ORIENTED_EDGE ( 'NONE', *, *, #97670, .F. ) ;
#29134 = CARTESIAN_POINT ( 'NONE',  ( -13.49147982757802389, 173.0177522451419350, 5.000000000000046185 ) ) ;
#29135 = VERTEX_POINT ( 'NONE', #86133 ) ;
#29136 = CARTESIAN_POINT ( 'NONE',  ( 81.59591673450252358, 50.88875380172861185, 14.58497109559629479 ) ) ;
#29137 = ORIENTED_EDGE ( 'NONE', *, *, #7239, .T. ) ;
#29138 = LINE ( 'NONE', #12955, #86505 ) ;
#29139 = VECTOR ( 'NONE', #88048, 1000.000000000000000 ) ;
#29140 = ORIENTED_EDGE ( 'NONE', *, *, #41862, .F. ) ;
#29141 = CARTESIAN_POINT ( 'NONE',  ( 207.1388427945310582, 271.8719953892863828, -6.773753280169677815 ) ) ;
#29142 = DIRECTION ( 'NONE',  ( 0.4999999999999992784, -0.8660254037844390407, 0.000000000000000000 ) ) ;
#29143 = CARTESIAN_POINT ( 'NONE',  ( 194.4032909867620447, 293.9306181827685123, -16.05392006271526384 ) ) ;
#29144 = CARTESIAN_POINT ( 'NONE',  ( 82.69964235597838353, 53.57960405717556540, -15.73923566368025995 ) ) ;
#29145 = CARTESIAN_POINT ( 'NONE',  ( 166.9053537448537270, 266.3976873878679044, -16.70102891481623431 ) ) ;
#29146 = VERTEX_POINT ( 'NONE', #95219 ) ;
#29147 = CARTESIAN_POINT ( 'NONE',  ( 66.00490917976195249, 68.68606793243894515, -0.05709965366314424112 ) ) ;
#29148 = CARTESIAN_POINT ( 'NONE',  ( 15.30080465516770616, 11.76004757982088300, 5.678558825948272215 ) ) ;
#29149 = ORIENTED_EDGE ( 'NONE', *, *, #3560, .T. ) ;
#29150 = CARTESIAN_POINT ( 'NONE',  ( 165.0419687026099496, 282.1322928540902240, 8.848871264540955295 ) ) ;
#29152 = ORIENTED_EDGE ( 'NONE', *, *, #34996, .T. ) ;
#29151 = CARTESIAN_POINT ( 'NONE',  ( -19.65312891409030271, 93.06504152958497400, 10.00000000000000888 ) ) ;
#29153 = CARTESIAN_POINT ( 'NONE',  ( 163.2919429874875448, 247.8170536094679903, 9.876785378511263147 ) ) ;
#29154 = CARTESIAN_POINT ( 'NONE',  ( 188.9334919176225753, 259.5804479054066292, 2.551952175883118734 ) ) ;
#29155 = CARTESIAN_POINT ( 'NONE',  ( 152.6320618002989136, 277.3629613401518554, -5.218654699652803153 ) ) ;
#29156 = DIRECTION ( 'NONE',  ( 0.7713975076906492978, 0.000000000000000000, -0.6363535849892373308 ) ) ;
#29157 = CARTESIAN_POINT ( 'NONE',  ( 192.6848806138171142, 292.2684757097440524, -14.43291781176028010 ) ) ;
#29158 = CARTESIAN_POINT ( 'NONE',  ( 168.2548547082295443, 252.8785486555144075, 11.97806002154297467 ) ) ;
#29159 = CARTESIAN_POINT ( 'NONE',  ( 194.8138150604092402, 263.1618850616820282, -0.7962985949493808224 ) ) ;
#29160 = ORIENTED_EDGE ( 'NONE', *, *, #75790, .F. ) ;
#29161 = CARTESIAN_POINT ( 'NONE',  ( 181.8990295830258219, 270.3834252994221288, -16.69949221592476007 ) ) ;
#29162 = CARTESIAN_POINT ( 'NONE',  ( 69.69046828898208901, 63.66106611675193250, -12.72546107364192913 ) ) ;
#29163 = ORIENTED_EDGE ( 'NONE', *, *, #40432, .F. ) ;
#29164 = CARTESIAN_POINT ( 'NONE',  ( 160.9611857202788201, 281.7540198505617468, 8.630106242394084859 ) ) ;
#29165 = EDGE_CURVE ( 'NONE', #80375, #43945, #64266, .T. ) ;
#29166 = CARTESIAN_POINT ( 'NONE',  ( -9.955209428791576443, 178.3927522451419350, 2.944929066748280225E-16 ) ) ;
#29167 = CARTESIAN_POINT ( 'NONE',  ( 196.1419589699951871, 269.5805659641910097, -10.92749632951035821 ) ) ;
#29168 = CARTESIAN_POINT ( 'NONE',  ( 174.8241034426651765, 281.2870359428685560, -14.17652806122567988 ) ) ;
#29169 = CARTESIAN_POINT ( 'NONE',  ( 203.8706191249530093, 277.5327248354951735, -15.89555175277244992 ) ) ;
#29170 = CARTESIAN_POINT ( 'NONE',  ( 82.47404279536071670, 44.73581219917306839, -9.792184509178092355 ) ) ;
#29171 = CARTESIAN_POINT ( 'NONE',  ( 164.2916406588784923, 274.2388883841279608, 14.76576668727659047 ) ) ;
#29173 = CARTESIAN_POINT ( 'NONE',  ( 2.169146224190643846, 165.3927522451418213, 10.00000000000009948 ) ) ;
#29172 = CARTESIAN_POINT ( 'NONE',  ( -12.05712525078605069, 163.8458772461660544, 9.188101187500095079 ) ) ;
#29174 = CARTESIAN_POINT ( 'NONE',  ( 188.9577279717659621, 296.9832364615082838, 8.133352747287846185 ) ) ;
#29175 = VERTEX_POINT ( 'NONE', #31849 ) ;
#29176 = ORIENTED_EDGE ( 'NONE', *, *, #56808, .F. ) ;
#29177 = DIRECTION ( 'NONE',  ( -0.8868092729070087277, -0.4621356007560363244, 0.000000000000000000 ) ) ;
#29178 = CARTESIAN_POINT ( 'NONE',  ( 38.14196570358561900, 88.90782515902715488, 59.99999999999999289 ) ) ;
#29179 = APPLICATION_CONTEXT ( 'automotive_design' ) ;
#29180 = CARTESIAN_POINT ( 'NONE',  ( 173.1133627894660947, 289.7078603327026940, 2.584739366812427885 ) ) ;
#29181 = DIRECTION ( 'NONE',  ( -0.8660254037844387076, -0.4999999999999998890, -0.000000000000000000 ) ) ;
#29182 = DIRECTION ( 'NONE',  ( 0.4999999999999998890, -0.8660254037844385966, 0.000000000000000000 ) ) ;
#29183 =( BOUNDED_CURVE ( )  B_SPLINE_CURVE ( 2, ( #71478, #69945, #61348, #78071, #9161, #84698, #31444, #93290, #40037, #31943, #32462, #94298, #70876 ),
 .UNSPECIFIED., .F., .T. ) 
 B_SPLINE_CURVE_WITH_KNOTS ( ( 3, 2, 2, 2, 2, 2, 3 ),
 ( 0.9375000000000000000, 0.9399999999999999467, 0.9449999999999999512, 0.9499999999999999556, 0.9549999999999999600, 0.9599999999999999645, 0.9625000000000000222 ),
 .UNSPECIFIED. ) 
 CURVE ( )  GEOMETRIC_REPRESENTATION_ITEM ( )  RATIONAL_B_SPLINE_CURVE ( ( 0.9755282581475768211, 0.9755282581475768211, 1.000000000000000000, 0.9510565162951535312, 1.000000000000000000, 0.9510565162951535312, 1.000000000000000000, 0.9510565162951535312, 1.000000000000000000, 0.9510565162951535312, 1.000000000000000000, 0.9755282581475761550, 0.9755282581475767101 ) ) 
 REPRESENTATION_ITEM ( '' )  );
#29184 = LINE ( 'NONE', #91015, #75663 ) ;
#29185 = CARTESIAN_POINT ( 'NONE',  ( 150.8203273413079728, 276.8881287278626928, 3.694477562601145681 ) ) ;
#29186 = CARTESIAN_POINT ( 'NONE',  ( 27.50958393249801404, 180.5643266524160424, 9.188101187500095079 ) ) ;
#29187 = CARTESIAN_POINT ( 'NONE',  ( 109.7816501962546454, 240.3149278399160949, 9.188101187500093303 ) ) ;
#29188 = DIRECTION ( 'NONE',  ( -1.000000000000000000, 0.000000000000000000, 0.000000000000000000 ) ) ;
#29189 = CARTESIAN_POINT ( 'NONE',  ( 182.7638336887914079, 257.5540677396648448, -2.311609576158096147 ) ) ;
#29191 = CARTESIAN_POINT ( 'NONE',  ( 79.20958550591666381, 57.62938875652737636, 16.22140153437238297 ) ) ;
#29190 = VECTOR ( 'NONE', #1334, 1000.000000000000227 ) ;
#29192 = CARTESIAN_POINT ( 'NONE',  ( 175.3541623712593491, 281.5767007636894164, -14.18713308759929248 ) ) ;
#29193 = CARTESIAN_POINT ( 'NONE',  ( 76.71058889096842393, 54.71840718949849958, -16.09767432139937782 ) ) ;
#29194 = CARTESIAN_POINT ( 'NONE',  ( 193.8913555215501390, 294.8173164187117550, 15.40725395879721837 ) ) ;
#29195 = CARTESIAN_POINT ( 'NONE',  ( 161.8926315922002743, 250.2407320417157166, -13.77020595223768495 ) ) ;
#29196 = CARTESIAN_POINT ( 'NONE',  ( 83.03373565306426940, 49.73266685372522744, 14.08671670346445204 ) ) ;
#29197 = LINE ( 'NONE', #38253, #1247 ) ;
#29198 = CARTESIAN_POINT ( 'NONE',  ( 84.79185039598577589, 50.39256584352096269, 13.46671255472566564 ) ) ;
#29199 = CARTESIAN_POINT ( 'NONE',  ( 196.3831153806621046, 266.1916474279236695, 8.338913457951525388 ) ) ;
#29200 = CARTESIAN_POINT ( 'NONE',  ( 78.01622611019826081, 227.3967562850346837, -4.648177544792955347E-16 ) ) ;
#29201 = CYLINDRICAL_SURFACE ( 'NONE', #75518, 10.00000000000001066 ) ;
#29202 = CARTESIAN_POINT ( 'NONE',  ( 40.41628377845469089, 57.12529113016345406, 10.00000000000000000 ) ) ;
#29203 = CIRCLE ( 'NONE', #84192, 70.00000000000001421 ) ;
#29204 = CARTESIAN_POINT ( 'NONE',  ( 182.0490020842017600, 268.2371330760522028, 15.01509780616252421 ) ) ;
#29205 = CARTESIAN_POINT ( 'NONE',  ( 99.63334886536203783, 219.1423013555409796, -4.594050593750043987 ) ) ;
#29206 = CARTESIAN_POINT ( 'NONE',  ( 67.74244556568478970, 65.67873629388216727, 10.75033511117075413 ) ) ;
#29207 = DIRECTION ( 'NONE',  ( 0.000000000000000000, 0.000000000000000000, 1.000000000000000000 ) ) ;
#29209 = CARTESIAN_POINT ( 'NONE',  ( 200.3852774630119029, 283.5695136757138357, 18.18377108216431992 ) ) ;
#29208 = CARTESIAN_POINT ( 'NONE',  ( 157.8360072705708603, 257.2670114739976839, 17.12122855844125269 ) ) ;
#29210 = CARTESIAN_POINT ( 'NONE',  ( 149.3915652274231149, 271.8932141343000239, 13.09942943774031221 ) ) ;
#29211 = B_SPLINE_CURVE_WITH_KNOTS ( 'NONE', 3,
 ( #61070, #92039, #84426, #14972 ),
 .UNSPECIFIED., .F., .F.,
 ( 4, 4 ),
 ( 0.02816671503466520315, 0.03735342737572562577 ),
 .UNSPECIFIED. ) ;
#29212 = CARTESIAN_POINT ( 'NONE',  ( 150.6626254231123880, 269.6916732958875969, -15.32062296289003811 ) ) ;
#29213 = LINE ( 'NONE', #60081, #42873 ) ;
#29214 = EDGE_CURVE ( 'NONE', #65497, #37415, #79515, .T. ) ;
#29215 = CARTESIAN_POINT ( 'NONE',  ( 40.22068564906490451, 26.14754757982093381, -5.678558825948275768 ) ) ;
#29216 = FACE_OUTER_BOUND ( 'NONE', #70375, .T. ) ;
#29217 = FACE_BOUND ( 'NONE', #12702, .T. ) ;
#29218 = ORIENTED_EDGE ( 'NONE', *, *, #1304, .F. ) ;
#29219 = CARTESIAN_POINT ( 'NONE',  ( 27.11361191214091804, 16.44966523072495335, -2.296566073217252530E-15 ) ) ;
#29220 = CARTESIAN_POINT ( 'NONE',  ( -19.51336063033015122, 93.04098814110220417, 59.99999999999999289 ) ) ;
#29221 = CARTESIAN_POINT ( 'NONE',  ( 192.4663556654298588, 297.2854885702906245, -12.98646995774174684 ) ) ;
#29222 = CARTESIAN_POINT ( 'NONE',  ( 149.5796913320911870, 271.5673701627850960, -12.80793412251569841 ) ) ;
#29223 = ORIENTED_EDGE ( 'NONE', *, *, #51709, .F. ) ;
#29224 = CARTESIAN_POINT ( 'NONE',  ( 70.65976107414203966, 60.91110302911690866, 15.02673238886433893 ) ) ;
#29225 = CARTESIAN_POINT ( 'NONE',  ( 159.7953104873542145, 253.8733987550956783, 15.41928249285404107 ) ) ;
#29227 = EDGE_CURVE ( 'NONE', #46907, #79781, #80008, .T. ) ;
#29226 = CARTESIAN_POINT ( 'NONE',  ( 157.6371076352215823, 268.6636118182534005, 15.72487649508922480 ) ) ;
#29228 = CARTESIAN_POINT ( 'NONE',  ( -71.61465314115659453, 63.06504152958490295, -45.00000000000001421 ) ) ;
#29229 = CARTESIAN_POINT ( 'NONE',  ( 139.5965524907815904, 264.7365022471903444, 2.944929066748280225E-16 ) ) ;
#29230 = ORIENTED_EDGE ( 'NONE', *, *, #35773, .T. ) ;
#29231 = CARTESIAN_POINT ( 'NONE',  ( 72.49754614901047489, 69.63129987044148095, 9.402869901847884293 ) ) ;
#29232 = ORIENTED_EDGE ( 'NONE', *, *, #85259, .T. ) ;
#29233 = CARTESIAN_POINT ( 'NONE',  ( 196.0106993659726413, 265.2146929077559889, -4.435233568084376188 ) ) ;
#29234 = CARTESIAN_POINT ( 'NONE',  ( 85.78016935146355593, 43.45830298991825202, 4.388455215017684097 ) ) ;
#29235 = EDGE_CURVE ( 'NONE', #690, #94448, #35414, .T. ) ;
#29236 = VERTEX_POINT ( 'NONE', #85623 ) ;
#29237 = CARTESIAN_POINT ( 'NONE',  ( 181.6032198279386307, 290.8331366659457444, -10.99987666991614610 ) ) ;
#29238 = ORIENTED_EDGE ( 'NONE', *, *, #91059, .F. ) ;
#29239 = CARTESIAN_POINT ( 'NONE',  ( -22.42236680055709641, 157.8615022471902591, 0.000000000000000000 ) ) ;
#29240 = CARTESIAN_POINT ( 'NONE',  ( 206.1959456970884617, 273.5051410683664130, 10.96659245355821533 ) ) ;
#29241 = CARTESIAN_POINT ( 'NONE',  ( 192.1389822274309722, 279.7169248230215430, -16.65130882895569187 ) ) ;
#29242 = CARTESIAN_POINT ( 'NONE',  ( 88.03469742524457331, 44.28626028149027860, -4.397723919905308421 ) ) ;
#29243 = CARTESIAN_POINT ( 'NONE',  ( 201.0468719883840265, 282.4235983437597497, -16.59631526626950659 ) ) ;
#29244 = CARTESIAN_POINT ( 'NONE',  ( 35.68911091587340678, 42.64646525600393545, -2.839279412974133887 ) ) ;
#29245 = CARTESIAN_POINT ( 'NONE',  ( 80.09407555685091040, 44.71242426696124994, 11.12975979062820642 ) ) ;
#29246 = CARTESIAN_POINT ( 'NONE',  ( 79.15025889697260197, 58.45979598525892840, -16.21445014555780872 ) ) ;
#29247 = CARTESIAN_POINT ( 'NONE',  ( -61.61048871844075592, 38.59675092633816007, -10.00000000000000000 ) ) ;
#29248 = CARTESIAN_POINT ( 'NONE',  ( 169.6623362669060668, 268.6156801215794303, -17.83028812261259333 ) ) ;
#29249 = ORIENTED_EDGE ( 'NONE', *, *, #87198, .T. ) ;
#29250 = ORIENTED_EDGE ( 'NONE', *, *, #8847, .T. ) ;
#29251 = CARTESIAN_POINT ( 'NONE',  ( 157.6921299354026189, 257.5162143285667753, -18.18720974599499840 ) ) ;
#29252 = DIRECTION ( 'NONE',  ( 0.8660254037844378194, 0.5000000000000014433, 0.000000000000000000 ) ) ;
#29254 = CARTESIAN_POINT ( 'NONE',  ( 165.9193144349327724, 274.0694398605538140, -15.17841830940742476 ) ) ;
#29253 = DIRECTION ( 'NONE',  ( -0.5000000000000002220, 0.8660254037844385966, -9.251858538542986372E-17 ) ) ;
#29255 = CARTESIAN_POINT ( 'NONE',  ( 204.0884846259506276, 275.1553707185394728, 13.46337290381501717 ) ) ;
#29256 = CARTESIAN_POINT ( 'NONE',  ( 68.42202639013687815, 68.53051497116777568, 7.558587510793364217 ) ) ;
#29257 = CARTESIAN_POINT ( 'NONE',  ( 156.6084421796713002, 261.3932165810376205, -17.82046942966612590 ) ) ;
#29258 = CARTESIAN_POINT ( 'NONE',  ( 82.09069798584521038, 40.79266795312825877, 1.461721908553118343 ) ) ;
#29259 = CARTESIAN_POINT ( 'NONE',  ( 167.3883760682938089, 286.9270113580703878, -4.952300633368714955 ) ) ;
#29260 = CARTESIAN_POINT ( 'NONE',  ( 77.22560725433092443, 63.51237900320956697, -15.09333827328594779 ) ) ;
#29261 = CARTESIAN_POINT ( 'NONE',  ( 178.1219001827957698, 255.2992632418402650, 5.629378456750874449 ) ) ;
#29262 = CARTESIAN_POINT ( 'NONE',  ( 111.5137010038235417, 241.3149278399161233, -9.188101187500095079 ) ) ;
#29263 = ORIENTED_EDGE ( 'NONE', *, *, #63853, .F. ) ;
#29264 = CARTESIAN_POINT ( 'NONE',  ( 184.8686473015538922, 260.4039463730296120, -9.780166574822738212 ) ) ;
#29265 = CARTESIAN_POINT ( 'NONE',  ( 36.43182450750798296, 23.96004757982092315, -5.678558825948276656 ) ) ;
#29266 = CARTESIAN_POINT ( 'NONE',  ( 190.0706732994661365, 292.5512512978990003, -14.47399639281167083 ) ) ;
#29267 = ORIENTED_EDGE ( 'NONE', *, *, #2597, .F. ) ;
#29268 = VERTEX_POINT ( 'NONE', #94701 ) ;
#29269 = EDGE_CURVE ( 'NONE', #78719, #54783, #48720, .T. ) ;
#29270 = CARTESIAN_POINT ( 'NONE',  ( 86.76444126019434577, 45.86660341771494842, -8.261827951889216592 ) ) ;
#29271 = EDGE_CURVE ( 'NONE', #45307, #72476, #86890, .T. ) ;
#29272 = DIRECTION ( 'NONE',  ( -0.4386133837897759347, -0.6599160945941885403, -0.6100238090894788412 ) ) ;
#29273 = CARTESIAN_POINT ( 'NONE',  ( 196.4351339088274813, 290.4113630087520050, 17.20526457544535504 ) ) ;
#29274 = CARTESIAN_POINT ( 'NONE',  ( 159.2394649670193303, 254.8361514374751664, -16.43133403737800791 ) ) ;
#29275 = CARTESIAN_POINT ( 'NONE',  ( -66.55019942848203129, 42.78701949053055387, -10.00000000000000000 ) ) ;
#29276 = ORIENTED_EDGE ( 'NONE', *, *, #76496, .T. ) ;
#29277 = CARTESIAN_POINT ( 'NONE',  ( 147.9431929457713011, 274.4018685143957441, 9.901114480726821654 ) ) ;
#29278 = AXIS2_PLACEMENT_3D ( 'NONE', #12988, #29654, #91001 ) ;
#29279 = VERTEX_POINT ( 'NONE', #49561 ) ;
#29280 = CARTESIAN_POINT ( 'NONE',  ( 74.14312167556930433, 66.30466486950707861, 1.224646799147354045E-15 ) ) ;
#29281 = ORIENTED_EDGE ( 'NONE', *, *, #32022, .F. ) ;
#29283 = CARTESIAN_POINT ( 'NONE',  ( 164.9356397357043704, 244.9700873293209042, 2.799217332519396972 ) ) ;
#29282 = B_SPLINE_CURVE_WITH_KNOTS ( 'NONE', 3,
 ( #45724, #15830, #29065, #76647 ),
 .UNSPECIFIED., .F., .F.,
 ( 4, 4 ),
 ( 0.03863331949670163745, 0.04715616731377302029 ),
 .UNSPECIFIED. ) ;
#29284 = EDGE_CURVE ( 'NONE', #75541, #18309, #22151, .T. ) ;
#29285 = CARTESIAN_POINT ( 'NONE',  ( 167.4962802984076689, 246.9545338215429808, -0.8696054547567072524 ) ) ;
#29286 = FACE_OUTER_BOUND ( 'NONE', #31222, .T. ) ;
#29287 = CARTESIAN_POINT ( 'NONE',  ( 82.73930168436014299, 45.65283476154188236, 10.64355013692776808 ) ) ;
#29289 = CARTESIAN_POINT ( 'NONE',  ( 158.1893771932294896, 280.3773502170195684, 5.704923391183662318 ) ) ;
#29288 = FACE_OUTER_BOUND ( 'NONE', #37214, .T. ) ;
#29290 = PLANE ( 'NONE',  #21985 ) ;
#29291 = ORIENTED_EDGE ( 'NONE', *, *, #21595, .F. ) ;
#29292 = CARTESIAN_POINT ( 'NONE',  ( 68.78093353194373094, 200.5177522451417929, 5.000000000000051514 ) ) ;
#29293 = EDGE_CURVE ( 'NONE', #37700, #38232, #43365, .T. ) ;
#29294 = CARTESIAN_POINT ( 'NONE',  ( 71.34228633229245986, 62.25329621047778517, 14.07928033790851252 ) ) ;
#29295 = B_SPLINE_CURVE_WITH_KNOTS ( 'NONE', 3,
 ( #49844, #56438, #17965, #47820 ),
 .UNSPECIFIED., .F., .F.,
 ( 4, 4 ),
 ( 0.03424363036717037456, 0.04307889571479175950 ),
 .UNSPECIFIED. ) ;
#29296 = CARTESIAN_POINT ( 'NONE',  ( 189.6922020185305655, 263.1654225416511963, -9.791328709709494760 ) ) ;
#29297 = EDGE_CURVE ( 'NONE', #14857, #53916, #71695, .T. ) ;
#29298 = CARTESIAN_POINT ( 'NONE',  ( 192.6263115592815893, 271.4202054200192720, 14.08161611139827052 ) ) ;
#29299 = CARTESIAN_POINT ( 'NONE',  ( 189.0338852884921721, 270.0244833716615176, -14.06004501950776842 ) ) ;
#29300 = CARTESIAN_POINT ( 'NONE',  ( 152.3107445603601491, 271.8204453097907276, -13.76269077489604875 ) ) ;
#29301 = LINE ( 'NONE', #384, #46905 ) ;
#29302 = CARTESIAN_POINT ( 'NONE',  ( -67.83107014231842413, 42.28230845022619633, 177.5919119679930134 ) ) ;
#29303 = CARTESIAN_POINT ( 'NONE',  ( 23.45662567177863167, 195.8967562850347122, -4.648177544792955347E-16 ) ) ;
#29304 = CARTESIAN_POINT ( 'NONE',  ( 82.74206721279597332, 53.66691124579689642, -15.75745978315255513 ) ) ;
#29305 = CARTESIAN_POINT ( 'NONE',  ( 78.60473566001486745, 222.3149278399160664, 9.188101187500093303 ) ) ;
#29306 = CARTESIAN_POINT ( 'NONE',  ( 159.9647205790309101, 253.5799718689968927, -16.48298384325780219 ) ) ;
#29307 = FACE_OUTER_BOUND ( 'NONE', #94106, .T. ) ;
#29308 = CARTESIAN_POINT ( 'NONE',  ( 187.1789365411204926, 291.3781964708418286, -14.15416893886036220 ) ) ;
#29309 = CARTESIAN_POINT ( 'NONE',  ( 161.1150691641480535, 251.5875096731584506, -13.48836942566120101 ) ) ;
#29310 = CARTESIAN_POINT ( 'NONE',  ( 151.2671975087473015, 270.6445237267302559, 14.15418255155509542 ) ) ;
#29311 = CARTESIAN_POINT ( 'NONE',  ( -20.84245520245646333, 95.08111133751313560, 45.19948159324908943 ) ) ;
#29312 = DIRECTION ( 'NONE',  ( -0.9963824715083249295, 0.08498217737244645464, 0.000000000000000000 ) ) ;
#29313 = CARTESIAN_POINT ( 'NONE',  ( 35.32779635548150310, 39.13478043621390867, 8.090169943749478065 ) ) ;
#29314 = LINE ( 'NONE', #50598, #80672 ) ;
#29315 = CARTESIAN_POINT ( 'NONE',  ( 195.9359860111818250, 291.2759125279654882, 17.49638312768267312 ) ) ;
#29316 = CARTESIAN_POINT ( 'NONE',  ( 71.87971293488917013, 71.94524500174831871, 2.848367791380675307 ) ) ;
#29317 = CARTESIAN_POINT ( 'NONE',  ( 21.77181853666109745, 189.5024278399160949, 9.188101187500095079 ) ) ;
#29318 = CARTESIAN_POINT ( 'NONE',  ( 169.9904317359561219, 275.5861877515991978, -16.87365932016444603 ) ) ;
#29319 = CARTESIAN_POINT ( 'NONE',  ( 42.16454434324483458, 125.9067112960471064, 177.5919119679930134 ) ) ;
#29320 = CARTESIAN_POINT ( 'NONE',  ( 78.90362582645330747, 50.91995579366576408, -15.11086290727698334 ) ) ;
#29321 = CARTESIAN_POINT ( 'NONE',  ( -62.95439910331221256, 68.06504152958493137, -24.99999999999999289 ) ) ;
#29322 = CARTESIAN_POINT ( 'NONE',  ( 52.54321753458319932, 191.9548013555410080, -4.594050593750042211 ) ) ;
#29323 = EDGE_CURVE ( 'NONE', #5053, #37567, #14077, .T. ) ;
#29324 = CARTESIAN_POINT ( 'NONE',  ( 24.44820476603448611, 26.06628583063842086, -9.188101187500006262 ) ) ;
#29325 = CARTESIAN_POINT ( 'NONE',  ( 165.5093369583051128, 275.0219039653110258, -16.16693748275729803 ) ) ;
#29326 = CARTESIAN_POINT ( 'NONE',  ( -9.359816960141781550, 158.7365022471902023, 10.00000000000009948 ) ) ;
#29327 = CARTESIAN_POINT ( 'NONE',  ( 5.120201826081539842, 21.14336893147752861, 7.433330006724141015 ) ) ;
#29328 = PLANE ( 'NONE',  #94222 ) ;
#29329 = CARTESIAN_POINT ( 'NONE',  ( 159.5137144416034403, 255.6472557863606028, -16.29473761095158579 ) ) ;
#29330 = CARTESIAN_POINT ( 'NONE',  ( 75.23362143766534871, 55.25164565488622515, 16.61958235066795453 ) ) ;
#29331 = CARTESIAN_POINT ( 'NONE',  ( 179.8145615969634434, 276.7378561409443591, 16.32957337418346100 ) ) ;
#29332 = CARTESIAN_POINT ( 'NONE',  ( 73.51157771055966350, 64.85277606651841609, 13.41954812668761043 ) ) ;
#29333 = CARTESIAN_POINT ( 'NONE',  ( 69.54925760825628345, 67.89440790003212101, -8.609516418554425954 ) ) ;
#29334 = CARTESIAN_POINT ( 'NONE',  ( 192.3032628966054460, 266.2805749702787921, 11.62727084212969864 ) ) ;
#29335 = EDGE_CURVE ( 'NONE', #78112, #13195, #25351, .T. ) ;
#29336 = VECTOR ( 'NONE', #79757, 1000.000000000000000 ) ;
#29337 = CARTESIAN_POINT ( 'NONE',  ( 21.99520779934447745, 195.0530062829863311, -4.648177544792955347E-16 ) ) ;
#29338 = CARTESIAN_POINT ( 'NONE',  ( 87.69706225426612889, 45.27692322852378481, -6.313661759682479335 ) ) ;
#29339 = CARTESIAN_POINT ( 'NONE',  ( 101.4192659406176915, 219.3615022471902023, 5.000000000000051514 ) ) ;
#29340 = CARTESIAN_POINT ( 'NONE',  ( 161.3193951073452581, 251.2336067582368742, 13.01220207292984377 ) ) ;
#29341 = PLANE ( 'NONE',  #2965 ) ;
#29342 = ORIENTED_EDGE ( 'NONE', *, *, #27802, .T. ) ;
#29343 = CARTESIAN_POINT ( 'NONE',  ( 57.82012596918833935, 210.3149278399160664, 9.188101187500093303 ) ) ;
#29344 = ORIENTED_EDGE ( 'NONE', *, *, #66648, .F. ) ;
#29345 = CARTESIAN_POINT ( 'NONE',  ( 166.5857064600952526, 264.6722026030038251, 17.46362175718670429 ) ) ;
#29346 = CARTESIAN_POINT ( 'NONE',  ( 190.2287563641723978, 301.1611242470490311, -4.521471513871881953 ) ) ;
#29347 = EDGE_CURVE ( 'NONE', #8797, #59906, #40249, .T. ) ;
#29348 = LINE ( 'NONE', #22742, #32136 ) ;
#29349 = VERTEX_POINT ( 'NONE', #23131 ) ;
#29350 = CARTESIAN_POINT ( 'NONE',  ( 28.46864935082048831, 149.7156766241961350, 21.50000000000008527 ) ) ;
#29351 = CARTESIAN_POINT ( 'NONE',  ( 165.0532575723395041, 244.7663672603923715, -2.144843157699870773 ) ) ;
#29352 = CARTESIAN_POINT ( 'NONE',  ( 71.63207289816666901, 60.29376661390504211, 15.47974284963322766 ) ) ;
#29353 = CARTESIAN_POINT ( 'NONE',  ( 73.10219508433868896, 70.64483191105212256, -7.776791464595123493 ) ) ;
#29354 = CARTESIAN_POINT ( 'NONE',  ( 82.41933087055697627, 40.38430946167127189, -0.8419157719606927825 ) ) ;
#29355 = CARTESIAN_POINT ( 'NONE',  ( 204.6487448717501252, 276.1849715073653897, 14.68262965895386607 ) ) ;
#29356 = ORIENTED_EDGE ( 'NONE', *, *, #91935, .F. ) ;
#29357 = CARTESIAN_POINT ( 'NONE',  ( 14.52983486323338802, 31.49540643055186706, 3.479690158560446702E-15 ) ) ;
#29358 = CARTESIAN_POINT ( 'NONE',  ( 67.93740734008792970, 69.57397595783162103, -2.710152877030299390 ) ) ;
#29359 = CARTESIAN_POINT ( 'NONE',  ( 172.6847352287274759, 251.7905635882845559, -7.423737323049481418 ) ) ;
#29360 = EDGE_CURVE ( 'NONE', #31691, #89234, #86261, .T. ) ;
#29361 = VERTEX_POINT ( 'NONE', #26533 ) ;
#29362 = CARTESIAN_POINT ( 'NONE',  ( 182.3977840624999658, 284.1126370688600105, 14.97779424287036854 ) ) ;
#29363 = ADVANCED_FACE ( 'NONE', ( #69740 ), #3735, .T. ) ;
#29364 = CARTESIAN_POINT ( 'NONE',  ( 206.7923762329701276, 272.4720930770340033, -9.496103119940368487 ) ) ;
#29365 = EDGE_LOOP ( 'NONE', ( #85215, #37453, #73155, #28237 ) ) ;
#29366 = ORIENTED_EDGE ( 'NONE', *, *, #59666, .T. ) ;
#29368 = DIRECTION ( 'NONE',  ( -0.5000000000000006661, 0.8660254037844382635, -1.877843081442121204E-16 ) ) ;
#29367 = CARTESIAN_POINT ( 'NONE',  ( 72.92559869912804515, 69.38761754411618199, 9.979010455306335459 ) ) ;
#29369 = CARTESIAN_POINT ( 'NONE',  ( 207.8446715390582540, 270.6494641423232679, -2.429516028743652800 ) ) ;
#29370 = CARTESIAN_POINT ( 'NONE',  ( 164.3853877993040840, 245.9231516401292197, 5.995325337583643943 ) ) ;
#29371 = CARTESIAN_POINT ( 'NONE',  ( 159.9014600375868440, 253.6895423408921886, 15.57825579621527368 ) ) ;
#29372 = CARTESIAN_POINT ( 'NONE',  ( 81.58121470000600084, 55.78443411318616540, 16.36431025809738671 ) ) ;
#29373 = CARTESIAN_POINT ( 'NONE',  ( 204.3760460221041342, 271.7077994814860062, 9.919166744778580735 ) ) ;
#29374 = CARTESIAN_POINT ( 'NONE',  ( 133.4083396129551602, 238.6423013555409796, -4.594050593750043987 ) ) ;
#29375 = CARTESIAN_POINT ( 'NONE',  ( 82.23173768200972233, 206.0327760586659451, 1.948934522072303157E-15 ) ) ;
#29376 = ORIENTED_EDGE ( 'NONE', *, *, #58612, .T. ) ;
#29377 = CARTESIAN_POINT ( 'NONE',  ( 171.1449649924396397, 264.1412602032671657, 15.82665639531467150 ) ) ;
#29378 = CARTESIAN_POINT ( 'NONE',  ( 74.52062983175133581, 59.67663687933149674, -16.10628646854518919 ) ) ;
#29379 = DIRECTION ( 'NONE',  ( -0.9999580202055560196, -0.009162850352621043637, 0.000000000000000000 ) ) ;
#29380 = ORIENTED_EDGE ( 'NONE', *, *, #33879, .T. ) ;
#29381 = CARTESIAN_POINT ( 'NONE',  ( 160.7612047594922160, 254.0226279303306569, 15.66240655037786489 ) ) ;
#29382 = VERTEX_POINT ( 'NONE', #42205 ) ;
#29383 = ORIENTED_EDGE ( 'NONE', *, *, #25640, .F. ) ;
#29384 = EDGE_CURVE ( 'NONE', #8463, #4641, #2743, .T. ) ;
#29385 = FACE_BOUND ( 'NONE', #84476, .T. ) ;
#29386 = CARTESIAN_POINT ( 'NONE',  ( 66.74918157967780985, 67.50276577062598449, 6.564943354671691544 ) ) ;
#29387 = CARTESIAN_POINT ( 'NONE',  ( 194.1866705654072689, 284.7458260699956440, 17.61685658156456213 ) ) ;
#29388 = CARTESIAN_POINT ( 'NONE',  ( 191.7934382699952494, 298.4510156884799699, -8.680100145728863126 ) ) ;
#29389 = CARTESIAN_POINT ( 'NONE',  ( 81.69344565705650041, 55.64297880859076173, 15.97102128751869543 ) ) ;
#29390 = CARTESIAN_POINT ( 'NONE',  ( 154.9683083969241011, 262.2340116239618055, 18.33261662430134109 ) ) ;
#29391 = CARTESIAN_POINT ( 'NONE',  ( 71.15088032201443013, 65.96942632406533846, 11.64872445604752471 ) ) ;
#29392 = ORIENTED_EDGE ( 'NONE', *, *, #14115, .T. ) ;
#29393 = EDGE_CURVE ( 'NONE', #59906, #47888, #65562, .T. ) ;
#29394 = CARTESIAN_POINT ( 'NONE',  ( 200.4628475472039213, 283.4351583487458583, -16.90921332594512450 ) ) ;
#29395 = ORIENTED_EDGE ( 'NONE', *, *, #59489, .T. ) ;
#29396 = CARTESIAN_POINT ( 'NONE',  ( 163.7388909753429118, 261.0030389665530492, -17.17036421060282336 ) ) ;
#29397 = CARTESIAN_POINT ( 'NONE',  ( 164.6597889008906463, 246.7339933633426483, 5.500642480278799873 ) ) ;
#29398 = EDGE_CURVE ( 'NONE', #30511, #55652, #27010, .T. ) ;
#29399 = CARTESIAN_POINT ( 'NONE',  ( 147.4427322147670907, 275.2686919276877120, -3.117028667211196868 ) ) ;
#29400 = CARTESIAN_POINT ( 'NONE',  ( 164.9103019330012216, 245.0139736909548560, 2.841678961959298810 ) ) ;
#29401 = CARTESIAN_POINT ( 'NONE',  ( 196.2878005184348353, 290.6665519265632724, -16.69183432842427806 ) ) ;
#29402 = CARTESIAN_POINT ( 'NONE',  ( 201.6593076491624856, 268.7283862757352608, -7.798329487074514788 ) ) ;
#29403 = CARTESIAN_POINT ( 'NONE',  ( 137.1425535231280151, 259.1744531367911009, 4.594050593750047540 ) ) ;
#29404 = ORIENTED_EDGE ( 'NONE', *, *, #63416, .T. ) ;
#29405 = CARTESIAN_POINT ( 'NONE',  ( 88.00768034709845722, 44.38581256804975794, 4.745967170566631310 ) ) ;
#29406 = EDGE_CURVE ( 'NONE', #74380, #15461, #68003, .T. ) ;
#29407 = CARTESIAN_POINT ( 'NONE',  ( 182.0290520670355647, 257.6954483311129707, 6.591660305417710752 ) ) ;
#29408 = CARTESIAN_POINT ( 'NONE',  ( 155.9450630872215982, 261.9324000175035394, -16.96800591457008878 ) ) ;
#29409 = CARTESIAN_POINT ( 'NONE',  ( 72.99786219007800980, 70.75108751906873295, 8.232086053012805493 ) ) ;
#29410 = CARTESIAN_POINT ( 'NONE',  ( 72.11059876947601310, 67.12034913926613910, -11.19373116030997295 ) ) ;
#29411 = ORIENTED_EDGE ( 'NONE', *, *, #73942, .T. ) ;
#29412 = CARTESIAN_POINT ( 'NONE',  ( 185.2961235551778714, 291.2460235572835927, 13.48139818756336616 ) ) ;
#29413 = CARTESIAN_POINT ( 'NONE',  ( 182.1763566781647512, 275.7876014702704310, -16.43406825299696550 ) ) ;
#29414 = CARTESIAN_POINT ( 'NONE',  ( 48.92549481379852949, 97.87922363803308201, 10.00000000000000000 ) ) ;
#29415 = CARTESIAN_POINT ( 'NONE',  ( 72.51849084938635315, 71.52899382949979668, -5.376470287118201519 ) ) ;
#29416 = CARTESIAN_POINT ( 'NONE',  ( 80.31617148571714893, 48.80743944517941202, 13.89541408168290992 ) ) ;
#29417 = CARTESIAN_POINT ( 'NONE',  ( 199.4759783357731351, 266.7372442807093762, 0.8265985939221809353 ) ) ;
#29418 = CARTESIAN_POINT ( 'NONE',  ( 195.3555557534167519, 264.0388318245352934, 0.8383882831563513882 ) ) ;
#29419 = CARTESIAN_POINT ( 'NONE',  ( 147.2443490232117256, 275.6123016948292275, 5.226063659459642352 ) ) ;
#29420 = CARTESIAN_POINT ( 'NONE',  ( 183.8623045117518586, 281.0860684350564611, 16.35513551783298780 ) ) ;
#29421 = CARTESIAN_POINT ( 'NONE',  ( 193.7028804065858480, 269.2481018004579596, 12.11718006226955602 ) ) ;
#29422 = CARTESIAN_POINT ( 'NONE',  ( 27.69565257936902469, 21.15404122711134605, 8.090169943749479842 ) ) ;
#29423 = CARTESIAN_POINT ( 'NONE',  ( 73.08094384907833785, 54.14441083166271795, 0.000000000000000000 ) ) ;
#29424 = CARTESIAN_POINT ( 'NONE',  ( 205.2203921948319589, 274.5650203181114648, 11.44562195678287253 ) ) ;
#29425 = LINE ( 'NONE', #37507, #28882 ) ;
#29426 = CARTESIAN_POINT ( 'NONE',  ( 198.2040940955416488, 287.3474340887963763, 16.95806375232200480 ) ) ;
#29427 = CARTESIAN_POINT ( 'NONE',  ( 72.17591038400095727, 71.86111175976400034, -3.889098828490574533 ) ) ;
#29428 = CARTESIAN_POINT ( 'NONE',  ( -3.180017766230537557, 156.7202760586659736, -5.415160957724236172E-17 ) ) ;
#29429 = CARTESIAN_POINT ( 'NONE',  ( 172.1831654133907819, 283.7635488940352388, -12.63565973616138294 ) ) ;
#29430 = ORIENTED_EDGE ( 'NONE', *, *, #46761, .F. ) ;
#29431 = CARTESIAN_POINT ( 'NONE',  ( 66.46511978770725193, 67.85058371895827634, -6.740288372309689358 ) ) ;
#29432 = CARTESIAN_POINT ( 'NONE',  ( 73.06733342522696262, 70.46939842116798047, -8.031525681787078597 ) ) ;
#29433 = CARTESIAN_POINT ( 'NONE',  ( 202.4716377814179680, 274.0562387935223114, -13.02713981561660184 ) ) ;
#29434 = CARTESIAN_POINT ( 'NONE',  ( 198.9832789858017463, 285.9978462703757600, -18.55676541969546278 ) ) ;
#29435 = CARTESIAN_POINT ( 'NONE',  ( 2.232293911657190488, 172.0958772461660544, -9.188101187500095079 ) ) ;
#29436 = CIRCLE ( 'NONE', #8476, 70.00000000000001421 ) ;
#29437 = CARTESIAN_POINT ( 'NONE',  ( 20.02985575298534471, 35.65659080271450421, -1.878358725466461243E-16 ) ) ;
#29438 = CARTESIAN_POINT ( 'NONE',  ( 85.07387056782178547, 48.93214387692037093, 12.41537898381571026 ) ) ;
#29439 = CARTESIAN_POINT ( 'NONE',  ( -18.15312891409030627, 78.77562236714182120, 59.99999999999999289 ) ) ;
#29440 = CARTESIAN_POINT ( 'NONE',  ( 72.15423005933928380, 71.84479394171614786, -3.903858941020849738 ) ) ;
#29441 = DIRECTION ( 'NONE',  ( 0.4999999999999992784, -0.8660254037844390407, 0.000000000000000000 ) ) ;
#29442 = CARTESIAN_POINT ( 'NONE',  ( 175.8941432106488492, 252.8195566316572922, -3.266688834427511789 ) ) ;
#29443 = CARTESIAN_POINT ( 'NONE',  ( 150.6051381537932343, 269.7912441671369947, 13.72054362922755999 ) ) ;
#29444 = CARTESIAN_POINT ( 'NONE',  ( 182.7446153974817946, 296.3825044924181498, 1.852756993870850133 ) ) ;
#29445 = CARTESIAN_POINT ( 'NONE',  ( 57.17980156396254898, 210.4865022471903160, 10.00000000000009237 ) ) ;
#29446 = CARTESIAN_POINT ( 'NONE',  ( -71.61465314115659453, 63.06504152958490295, -25.00000000000000000 ) ) ;
#29447 = CARTESIAN_POINT ( 'NONE',  ( 190.1730848958311810, 301.2575500587478814, 0.2415986433272204748 ) ) ;
#29448 = VECTOR ( 'NONE', #92890, 1000.000000000000000 ) ;
#29449 = CARTESIAN_POINT ( 'NONE',  ( 9.512059640396367755, 185.4869531367911293, 4.594050593750046652 ) ) ;
#29450 = CARTESIAN_POINT ( 'NONE',  ( 164.5169933802496587, 285.4399748993757271, 4.369849052753852270 ) ) ;
#29451 = CARTESIAN_POINT ( 'NONE',  ( 152.8134625983922490, 265.9663140294953791, 17.57333028169644251 ) ) ;
#29452 = CARTESIAN_POINT ( 'NONE',  ( 42.04415689841856363, 29.98920272979930246, 7.433330006724137462 ) ) ;
#29453 = PLANE ( 'NONE',  #17470 ) ;
#29455 = EDGE_CURVE ( 'NONE', #87618, #17797, #51819, .T. ) ;
#29454 = B_SPLINE_CURVE_WITH_KNOTS ( 'NONE', 3,
 ( #88879, #3723, #65500, #19441, #66003, #43178, #96954, #49313, #89363, #50791, #12315, #4715, #35600, #66498, #27993, #97912, #58872, #20416, #51283, #82252, #12825, #28487, #59368, #18423, #80252, #41695, #20923, #36581, #37569, #22386, #76119, #5690, #83730, #15264, #52283, #6692, #83224, #51806, #67989, #92330, #90847, #53283, #67486, #99898, #45180, #60863 ),
 .UNSPECIFIED., .F., .F.,
 ( 4, 1, 1, 1, 2, 2, 1, 1, 1, 2, 2, 1, 1, 2, 2, 1, 1, 2, 2, 1, 1, 2, 2, 1, 2, 2, 1, 2, 2, 4 ),
 ( 0.000000000000000000, 0.06250000000002371714, 0.09375000000003461120, 0.1093750000000400652, 0.1171875000000423134, 0.1250000000000445755, 0.1875000000000582590, 0.2187500000000651423, 0.2343750000000676403, 0.2421875000000674738, 0.2500000000000672795, 0.3125000000000652811, 0.3437500000000648370, 0.3593750000000646150, 0.3750000000000643374, 0.4375000000000635048, 0.4687500000000631162, 0.4843750000000619504, 0.5000000000000607292, 0.5625000000000570655, 0.5937500000000536238, 0.6093750000000520695, 0.6250000000000504041, 0.6875000000000429656, 0.7187500000000411893, 0.7500000000000393019, 0.8125000000000316414, 0.8437500000000254241, 0.8750000000000192069, 1.000000000000000000 ),
 .UNSPECIFIED. ) ;
#29456 = CARTESIAN_POINT ( 'NONE',  ( 206.9377610035629118, 272.2202792677204002, 7.440532334334675646 ) ) ;
#29457 = CARTESIAN_POINT ( 'NONE',  ( 188.7267008190097499, 267.6263124316118933, 14.18876842644463920 ) ) ;
#29458 = CARTESIAN_POINT ( 'NONE',  ( 116.9355544250887959, 244.9865022471903160, 10.00000000000009415 ) ) ;
#29459 = LINE ( 'NONE', #91290, #56877 ) ;
#29460 = CARTESIAN_POINT ( 'NONE',  ( 19.31277771287585310, 13.01110640527291551, 2.839279412974134775 ) ) ;
#29461 = CARTESIAN_POINT ( 'NONE',  ( 148.3997536239841679, 273.6110822229926498, 8.713694244701960301 ) ) ;
#29462 = CARTESIAN_POINT ( 'NONE',  ( 71.70303330742534342, 59.04301762528319131, 15.85811543470831353 ) ) ;
#29463 = CARTESIAN_POINT ( 'NONE',  ( 198.5765922241581336, 267.0449333599083275, 7.976362536003974490 ) ) ;
#29464 = ORIENTED_EDGE ( 'NONE', *, *, #97587, .F. ) ;
#29465 = DIRECTION ( 'NONE',  ( 0.8080546441192343332, -0.5891075386695858729, 0.000000000000000000 ) ) ;
#29466 = DIRECTION ( 'NONE',  ( -1.000000000000000000, 0.000000000000000000, 0.000000000000000000 ) ) ;
#29467 = CARTESIAN_POINT ( 'NONE',  ( 75.04791297046116938, 53.45263424984147349, -16.05211567179630805 ) ) ;
#29468 = CARTESIAN_POINT ( 'NONE',  ( 88.26230900456008044, 44.35601202938862997, 2.501165180090373141 ) ) ;
#29469 = EDGE_CURVE ( 'NONE', #44408, #97401, #80441, .T. ) ;
#29470 = ORIENTED_EDGE ( 'NONE', *, *, #75706, .F. ) ;
#29472 = CARTESIAN_POINT ( 'NONE',  ( 195.8779528940816874, 290.3143152550151740, -16.43829057065248023 ) ) ;
#29471 =( BOUNDED_CURVE ( )  B_SPLINE_CURVE ( 2, ( #21930, #20968, #6232, #52328, #36128, #75159, #74671, #36622, #12360 ),
 .UNSPECIFIED., .F., .T. ) 
 B_SPLINE_CURVE_WITH_KNOTS ( ( 3, 2, 2, 2, 3 ),
 ( 0.7056451612903226200, 0.7069892473118279952, 0.7096774193548387455, 0.7123655913978494958, 0.7137096774193548709 ),
 .UNSPECIFIED. ) 
 CURVE ( )  GEOMETRIC_REPRESENTATION_ITEM ( )  RATIONAL_B_SPLINE_CURVE ( ( 0.9330127018922194093, 0.9330127018922194093, 1.000000000000000000, 0.8660254037844387076, 1.000000000000000000, 0.8660254037844387076, 1.000000000000000000, 0.9330127018922194093, 0.9330127018922194093 ) ) 
 REPRESENTATION_ITEM ( '' )  );
#29473 = DIRECTION ( 'NONE',  ( -0.1269555777209495084, -0.9919084036772447543, 0.000000000000000000 ) ) ;
#29474 = CARTESIAN_POINT ( 'NONE',  ( 77.14822757211506143, 63.64430466641118755, 15.03252049986617500 ) ) ;
#29475 = ADVANCED_FACE ( 'NONE', ( #74136, #81754 ), #82266, .T. ) ;
#29476 = CARTESIAN_POINT ( 'NONE',  ( 155.4495868485232108, 261.4004128932040203, -18.48326470492642315 ) ) ;
#29477 = VERTEX_POINT ( 'NONE', #59893 ) ;
#29478 = VERTEX_POINT ( 'NONE', #88891 ) ;
#29480 = CARTESIAN_POINT ( 'NONE',  ( 204.9432097630379417, 275.6749433546094679, 13.74700047688257776 ) ) ;
#29479 = CARTESIAN_POINT ( 'NONE',  ( 186.3138579965807935, 271.9636586987053306, -16.45016817854244096 ) ) ;
#29481 = ORIENTED_EDGE ( 'NONE', *, *, #73145, .T. ) ;
#29482 = CARTESIAN_POINT ( 'NONE',  ( 191.4044787581200069, 299.1247133251352466, 7.435199718141230818 ) ) ;
#29483 = CARTESIAN_POINT ( 'NONE',  ( 71.43724303959665178, 68.55867823653906612, 9.960316262241418528 ) ) ;
#29484 = CARTESIAN_POINT ( 'NONE',  ( 80.31886729598942054, 57.42767889257750369, -16.58902572440456780 ) ) ;
#29485 = LINE ( 'NONE', #7678, #75939 ) ;
#29486 = ORIENTED_EDGE ( 'NONE', *, *, #43944, .T. ) ;
#29487 = CARTESIAN_POINT ( 'NONE',  ( 87.69383267149372330, 45.37878083771482807, -6.511118445142236588 ) ) ;
#29488 = ORIENTED_EDGE ( 'NONE', *, *, #16685, .F. ) ;
#29489 = CARTESIAN_POINT ( 'NONE',  ( 206.0627831668701901, 273.7357853363691902, 10.14454147593459687 ) ) ;
#29490 = LINE ( 'NONE', #60366, #49404 ) ;
#29491 = ORIENTED_EDGE ( 'NONE', *, *, #93713, .F. ) ;
#29492 = CARTESIAN_POINT ( 'NONE',  ( 149.7166446726674565, 271.3301600186404698, 12.26048591517335495 ) ) ;
#29493 = CARTESIAN_POINT ( 'NONE',  ( 172.3444904895413856, 263.8722161183861203, -15.54433039079544088 ) ) ;
#29494 = VERTEX_POINT ( 'NONE', #28007 ) ;
#29495 = CARTESIAN_POINT ( 'NONE',  ( -18.06678529174625325, 77.67718851601459562, 13.60376042076901371 ) ) ;
#29496 = LINE ( 'NONE', #35605, #14293 ) ;
#29497 = CYLINDRICAL_SURFACE ( 'NONE', #22398, 70.00000000000002842 ) ;
#29498 = CARTESIAN_POINT ( 'NONE',  ( 41.54549712337441747, 24.39040679176986615, -6.890680421881970419E-14 ) ) ;
#29500 = ORIENTED_EDGE ( 'NONE', *, *, #37989, .F. ) ;
#29499 = B_SPLINE_CURVE_WITH_KNOTS ( 'NONE', 3,
 ( #51566, #72905, #57656, #4469, #43948, #58161, #41968, #74398, #27773, #4983 ),
 .UNSPECIFIED., .F., .F.,
 ( 4, 2, 2, 2, 4 ),
 ( 0.000000000000000000, 0.2500000000000000000, 0.5000000000000000000, 0.7500000000000000000, 1.000000000000000000 ),
 .UNSPECIFIED. ) ;
#29501 = VERTEX_POINT ( 'NONE', #58884 ) ;
#29502 = EDGE_CURVE ( 'NONE', #34466, #57243, #60684, .T. ) ;
#29503 = CARTESIAN_POINT ( 'NONE',  ( 73.47134878188418838, 69.83576924732003022, 9.227620320897900186 ) ) ;
#29504 = DIRECTION ( 'NONE',  ( 0.3301025504114332154, 0.9439450758449174916, 0.000000000000000000 ) ) ;
#29505 = CARTESIAN_POINT ( 'NONE',  ( 189.9052851100924215, 301.7213928939034986, -1.077181946533001256 ) ) ;
#29506 = CARTESIAN_POINT ( 'NONE',  ( 175.0305792595766263, 260.7322313912393952, -14.80875141956958707 ) ) ;
#29507 = CARTESIAN_POINT ( 'NONE',  ( 192.4454213697443095, 297.3217478340386606, 12.58566886711101596 ) ) ;
#29508 = CARTESIAN_POINT ( 'NONE',  ( 191.0739205222354258, 299.6972569845476073, 8.800115285385583519 ) ) ;
#29509 = CARTESIAN_POINT ( 'NONE',  ( 146.5689048584090699, 276.7822053059436485, -0.4306668706573002492 ) ) ;
#29510 = ADVANCED_FACE ( 'NONE', ( #30500 ), #86141, .F. ) ;
#29512 = CARTESIAN_POINT ( 'NONE',  ( -38.35373792487678202, 26.90998726756845727, -10.00000000000000000 ) ) ;
#29511 = B_SPLINE_CURVE_WITH_KNOTS ( 'NONE', 3,
 ( #8962, #94105, #860, #55049, #16061, #56038, #48470, #87031, #94601, #18077, #33263, #40838, #79907, #1874, #86524, #47453, #16559, #24164, #78381, #24656 ),
 .UNSPECIFIED., .F., .F.,
 ( 4, 2, 2, 2, 2, 2, 2, 2, 2, 4 ),
 ( 0.003588130654998039452, 0.003719546847186400683, 0.003850963039374761913, 0.003982379231563123144, 0.004113795423751483507, 0.004376627808128081068, 0.004639460192504678629, 0.005690789730011110506, 0.006742119267517541516, 0.007793448805023973393 ),
 .UNSPECIFIED. ) ;
#29513 = B_SPLINE_CURVE_WITH_KNOTS ( 'NONE', 3,
 ( #28303, #90157, #20731, #74933, #51616, #44495 ),
 .UNSPECIFIED., .F., .F.,
 ( 4, 2, 4 ),
 ( 0.01829576855254007664, 0.02279459486296724416, 0.02729342117339441168 ),
 .UNSPECIFIED. ) ;
#29514 = CARTESIAN_POINT ( 'NONE',  ( -78.57153713424663977, 57.64153020465174393, -10.00000000000000000 ) ) ;
#29515 = VECTOR ( 'NONE', #43004, 1000.000000000000000 ) ;
#29517 = DIRECTION ( 'NONE',  ( 1.000000000000000000, 0.000000000000000000, 0.000000000000000000 ) ) ;
#29516 = CARTESIAN_POINT ( 'NONE',  ( 196.9319848161575806, 289.5507919934690335, -17.64330560362266453 ) ) ;
#29518 = CARTESIAN_POINT ( 'NONE',  ( -70.89022602266993545, 47.22876919346843749, -10.00000000000000000 ) ) ;
#29519 = CARTESIAN_POINT ( 'NONE',  ( 168.3229878282932361, 286.3524262165808523, 4.038607488141395585 ) ) ;
#29520 = CARTESIAN_POINT ( 'NONE',  ( 50.13870555935887552, 87.67061469898740711, 177.5919119679930134 ) ) ;
#29521 = EDGE_LOOP ( 'NONE', ( #59503, #582, #42785, #93330 ) ) ;
#29522 = CARTESIAN_POINT ( 'NONE',  ( 190.5470883969117892, 300.6097569926677693, -3.254269538324694455 ) ) ;
#29523 = CARTESIAN_POINT ( 'NONE',  ( 76.63684583903793168, 54.02340966775668107, -16.04885996875553644 ) ) ;
#29524 = EDGE_CURVE ( 'NONE', #45207, #66378, #9726, .T. ) ;
#29525 = CARTESIAN_POINT ( 'NONE',  ( 84.23708473736340352, 41.98719078163990304, 4.050242299038782079 ) ) ;
#29526 = CARTESIAN_POINT ( 'NONE',  ( 79.22627167205122589, 45.80186466725063354, 13.02917726998096271 ) ) ;
#29527 = CARTESIAN_POINT ( 'NONE',  ( 191.4500230558827809, 297.4070410935535165, -10.84401322141531487 ) ) ;
#29528 = CARTESIAN_POINT ( 'NONE',  ( 189.8160923722963389, 301.8758792474325787, -0.7767885082579778500 ) ) ;
#29529 = CARTESIAN_POINT ( 'NONE',  ( 69.23870777756563655, 65.06122599265698625, -11.45902463328623178 ) ) ;
#29530 = ORIENTED_EDGE ( 'NONE', *, *, #17227, .F. ) ;
#29531 = CARTESIAN_POINT ( 'NONE',  ( 208.2874212803407090, 269.8825990953837390, -1.143705256421198690 ) ) ;
#29532 = CARTESIAN_POINT ( 'NONE',  ( 36.10619739613039769, 52.83927550304669296, -10.00000000000000000 ) ) ;
#29533 = CARTESIAN_POINT ( 'NONE',  ( 72.32137329212656596, 71.76143927211870732, 5.594163357809740944 ) ) ;
#29534 = CARTESIAN_POINT ( 'NONE',  ( 51.02741275436275004, 190.2677522451418213, -5.000000000000041744 ) ) ;
#29535 = CARTESIAN_POINT ( 'NONE',  ( 107.1835739849013578, 238.8149278399160949, 9.188101187500093303 ) ) ;
#29536 = CARTESIAN_POINT ( 'NONE',  ( 198.7829547491859330, 286.3448180261817129, -18.59838968157616179 ) ) ;
#29537 = VECTOR ( 'NONE', #43002, 1000.000000000000114 ) ;
#29538 = CARTESIAN_POINT ( 'NONE',  ( 167.4968739850875750, 271.4686504602936452, 17.49260192182149254 ) ) ;
#29539 = CARTESIAN_POINT ( 'NONE',  ( 195.7291850945597957, 291.6341022226063160, 17.08310330964873813 ) ) ;
#29540 = DIRECTION ( 'NONE',  ( 0.5000000000000014433, -0.8660254037844378194, 0.000000000000000000 ) ) ;
#29541 = CARTESIAN_POINT ( 'NONE',  ( 34.97905304013878691, 184.8768266524159856, 9.188101187500098632 ) ) ;
#29542 = CARTESIAN_POINT ( 'NONE',  ( 147.7362813631496863, 275.4859596630231522, -3.675214258173687298 ) ) ;
#29543 = ORIENTED_EDGE ( 'NONE', *, *, #44983, .F. ) ;
#29544 = CARTESIAN_POINT ( 'NONE',  ( 191.3220911622827600, 298.6397096588477780, 8.200542337010491067 ) ) ;
#29545 = CARTESIAN_POINT ( 'NONE',  ( 181.6523902737856417, 267.3132069320698747, 14.96885079024440834 ) ) ;
#29546 = DIRECTION ( 'NONE',  ( 0.000000000000000000, 0.000000000000000000, 1.000000000000000000 ) ) ;
#29547 = CARTESIAN_POINT ( 'NONE',  ( 190.9441801652054096, 299.9219738747156043, -4.765040093794296716 ) ) ;
#29548 = CARTESIAN_POINT ( 'NONE',  ( 81.95746785621842889, 41.34290087354509780, -5.897592725355119470 ) ) ;
#29549 = DIRECTION ( 'NONE',  ( 0.4999999999999992784, -0.8660254037844390407, 0.000000000000000000 ) ) ;
#29550 = CARTESIAN_POINT ( 'NONE',  ( 179.0422977575919390, 287.4129436693755792, -12.34808154371113709 ) ) ;
#29551 = CARTESIAN_POINT ( 'NONE',  ( 164.1116730098435426, 250.1177055282117863, 10.48172797642971155 ) ) ;
#29552 = ADVANCED_BREP_SHAPE_REPRESENTATION ( '', ( #76389, #68784 ), #70444 ) ;
#29553 = CARTESIAN_POINT ( 'NONE',  ( 117.2061873602236233, 225.1427522451417929, 1.119607411625061291E-15 ) ) ;
#29554 = ORIENTED_EDGE ( 'NONE', *, *, #34195, .F. ) ;
#29555 = EDGE_CURVE ( 'NONE', #24507, #6222, #54794, .T. ) ;
#29556 = CARTESIAN_POINT ( 'NONE',  ( 194.7741005058701660, 266.3470718410572999, -7.689080487137245790 ) ) ;
#29557 = CARTESIAN_POINT ( 'NONE',  ( 158.0650824465715516, 281.3856441582040588, -1.598288696427632827 ) ) ;
#29558 = CARTESIAN_POINT ( 'NONE',  ( 208.2912792141756029, 269.8759169579697641, -2.198672330625011995 ) ) ;
#29559 = CARTESIAN_POINT ( 'NONE',  ( 20.20266813594930611, 170.2202760586659736, -5.415160957724236172E-17 ) ) ;
#29560 = CARTESIAN_POINT ( 'NONE',  ( 7.533646096595723485, 16.30066082961419482, -10.00000000000000533 ) ) ;
#29561 = CARTESIAN_POINT ( 'NONE',  ( 192.1761047855001152, 272.2161798191603452, 14.46851533410970880 ) ) ;
#29562 = CARTESIAN_POINT ( 'NONE',  ( 71.65411058451715576, 58.83614272603743700, -15.40970175268381404 ) ) ;
#29563 = CARTESIAN_POINT ( 'NONE',  ( 73.09565900097605606, 69.67901489450639474, 9.155081292670679716 ) ) ;
#29565 = CARTESIAN_POINT ( 'NONE',  ( 54.68078388046974680, 208.5024278399160664, -9.188101187500093303 ) ) ;
#29564 = CARTESIAN_POINT ( 'NONE',  ( 174.0659358162305068, 287.4380069074235280, 10.67600509024926581 ) ) ;
#29566 = CARTESIAN_POINT ( 'NONE',  ( 163.8947349411736525, 246.7729873192901664, -5.868803394723933309 ) ) ;
#29567 = CARTESIAN_POINT ( 'NONE',  ( 73.13622937094719134, 57.24645749009919626, 16.39293205268555909 ) ) ;
#29568 = CARTESIAN_POINT ( 'NONE',  ( 69.82165319358976774, 66.39592426718104434, 11.22546775247526973 ) ) ;
#29569 = CARTESIAN_POINT ( 'NONE',  ( 66.15839288007977359, 68.64661655514622396, -4.374828951538166422 ) ) ;
#29570 = ORIENTED_EDGE ( 'NONE', *, *, #49180, .F. ) ;
#29571 = CARTESIAN_POINT ( 'NONE',  ( 17.34263298987836066, 187.4865022471903444, -10.00000000000009415 ) ) ;
#29572 = CARTESIAN_POINT ( 'NONE',  ( 208.3117541397001844, 269.8404533466799080, 2.895672523916592578 ) ) ;
#29573 = CARTESIAN_POINT ( 'NONE',  ( 128.9153121871758572, 254.4244531367911293, -4.594050593750046652 ) ) ;
#29574 = CARTESIAN_POINT ( 'NONE',  ( 24.77416059058194620, 29.70171378149920471, -9.188101187500004485 ) ) ;
#29575 = CARTESIAN_POINT ( 'NONE',  ( 188.0428171265000117, 264.4088423580298581, 12.23537495986646029 ) ) ;
#29576 = LINE ( 'NONE', #36663, #67821 ) ;
#29577 = B_SPLINE_CURVE_WITH_KNOTS ( 'NONE', 3,
 ( #66607, #65129, #73245, #65622 ),
 .UNSPECIFIED., .F., .F.,
 ( 4, 4 ),
 ( 0.004660457163933351930, 0.01266542117972364531 ),
 .UNSPECIFIED. ) ;
#29578 = DIRECTION ( 'NONE',  ( -0.9756173257765591300, -0.2194785493951409983, 0.000000000000000000 ) ) ;
#29580 = CARTESIAN_POINT ( 'NONE',  ( 187.2510800322089324, 288.7440624129242224, 14.48677483733536420 ) ) ;
#29579 = CARTESIAN_POINT ( 'NONE',  ( 84.89744547285587828, 41.79037650531964943, -3.168800655305855967E-06 ) ) ;
#29581 = CARTESIAN_POINT ( 'NONE',  ( 68.79284463328235688, 64.08361226851032200, 12.02460708678565560 ) ) ;
#29582 = VERTEX_POINT ( 'NONE', #86760 ) ;
#29583 = CARTESIAN_POINT ( 'NONE',  ( 81.18224314092121574, 50.95777291934366104, 15.14991892385681282 ) ) ;
#29584 = CARTESIAN_POINT ( 'NONE',  ( 180.6665526851674599, 287.6815954905284798, 14.11204521094005671 ) ) ;
#29585 = CIRCLE ( 'NONE', #86263, 17.82106496071138224 ) ;
#29586 = CARTESIAN_POINT ( 'NONE',  ( 196.3883463204838051, 288.9924089565074610, 17.07220126560286388 ) ) ;
#29587 = CARTESIAN_POINT ( 'NONE',  ( 193.8905572877353052, 270.7343714464398658, -13.92882677973582872 ) ) ;
#29588 = EDGE_LOOP ( 'NONE', ( #39074, #15614, #38970, #72391 ) ) ;
#29589 = PLANE ( 'NONE',  #48983 ) ;
#29590 = CARTESIAN_POINT ( 'NONE',  ( 81.98204644731730184, 41.14170830008083612, -5.380964918418897902 ) ) ;
#29592 = VECTOR ( 'NONE', #83712, 1000.000000000000114 ) ;
#29591 = CARTESIAN_POINT ( 'NONE',  ( 75.30369160444902832, 53.36362683429165088, 16.03060775139856631 ) ) ;
#29593 = B_SPLINE_SURFACE_WITH_KNOTS ( 'NONE', 3, 1, ( 
 ( #25201, #31299 ),
 ( #78938, #69800 ),
 ( #63206, #62690 ),
 ( #62186, #94148 ),
 ( #54582, #100227 ),
 ( #9007, #1421 ),
 ( #70815, #87079 ),
 ( #94646, #56084 ),
 ( #15589, #38896 ),
 ( #93646, #17611 ),
 ( #70299, #46490 ),
 ( #48519, #9526 ),
 ( #40387, #24701 ),
 ( #55092, #93138 ),
 ( #8024, #85563 ),
 ( #39381, #39878 ),
 ( #86078, #55583 ),
 ( #86568, #79455 ),
 ( #71327, #909 ),
 ( #23687, #23193 ),
 ( #16108, #47007 ),
 ( #16602, #1918 ),
 ( #47501, #61692 ),
 ( #32804, #77921 ),
 ( #31788, #8513 ),
 ( #78426, #38394 ),
 ( #69305, #30813 ),
 ( #92645, #54086 ),
 ( #77423, #85040 ),
 ( #89555, #79950 ),
 ( #10517, #41899 ) ),
 .UNSPECIFIED., .F., .F., .F.,
 ( 4, 3, 3, 3, 3, 3, 3, 3, 3, 3, 4 ),
 ( 2, 2 ),
 ( 0.000000000000000000, 0.1333490885032313222, 0.3007194338854298210, 0.4699862290245092056, 0.5844252810809273946, 0.6686540514502635757, 0.7354980260655534785, 0.8028463152565743499, 0.8633854507757382502, 0.9437142632667581132, 1.000000000000000000 ),
 ( 0.000000000000000000, 1.000000000000000000 ),
 .UNSPECIFIED. ) ;
#29594 = EDGE_CURVE ( 'NONE', #57617, #76220, #56065, .T. ) ;
#29595 = CARTESIAN_POINT ( 'NONE',  ( 35.32845566053276087, 49.32197259295687530, 10.00000000000000000 ) ) ;
#29596 = CARTESIAN_POINT ( 'NONE',  ( -49.12564547450223529, 77.70627210468882140, -10.00000000000000000 ) ) ;
#29597 = CARTESIAN_POINT ( 'NONE',  ( 93.89567024169240028, 225.0177522451418781, -10.00000000000009592 ) ) ;
#29598 = EDGE_CURVE ( 'NONE', #100032, #61618, #72884, .T. ) ;
#29599 = CARTESIAN_POINT ( 'NONE',  ( 68.41443082112564866, 69.68312250061349289, 3.489189732842724379 ) ) ;
#29600 = CARTESIAN_POINT ( 'NONE',  ( 152.6740002182599767, 266.2078699576288159, -17.16212636348624088 ) ) ;
#29601 = CARTESIAN_POINT ( 'NONE',  ( -19.65312891409030271, 93.06504152958497400, -10.00000000000000888 ) ) ;
#29602 = CARTESIAN_POINT ( 'NONE',  ( 16.09091216865756024, 14.45404122711132366, -8.090169943749478065 ) ) ;
#29603 = CARTESIAN_POINT ( 'NONE',  ( 175.1378461883211912, 279.3152656845848583, 16.63146252814350134 ) ) ;
#29604 = ORIENTED_EDGE ( 'NONE', *, *, #36576, .F. ) ;
#29605 = CARTESIAN_POINT ( 'NONE',  ( 149.0359194785865498, 272.5092106407810206, 12.76357969772040590 ) ) ;
#29606 = CARTESIAN_POINT ( 'NONE',  ( -22.42236680055709641, 157.8615022471902591, 0.000000000000000000 ) ) ;
#29607 = CARTESIAN_POINT ( 'NONE',  ( 81.64570241471020040, 45.46107742057574086, -11.03823634419222088 ) ) ;
#29608 = ORIENTED_EDGE ( 'NONE', *, *, #57373, .F. ) ;
#29609 = CARTESIAN_POINT ( 'NONE',  ( 147.2784190576484491, 275.5532906641692534, 0.2793038414862047958 ) ) ;
#29610 = PLANE ( 'NONE',  #15188 ) ;
#29611 = AXIS2_PLACEMENT_3D ( 'NONE', #97660, #74857, #68715 ) ;
#29612 = CARTESIAN_POINT ( 'NONE',  ( 163.8147431267737204, 246.9115372060205118, 7.125417796469586840 ) ) ;
#29613 = CARTESIAN_POINT ( 'NONE',  ( 69.54173309467141451, 62.57597753113334704, 13.33913063052011516 ) ) ;
#29614 = ORIENTED_EDGE ( 'NONE', *, *, #50427, .T. ) ;
#29615 = CARTESIAN_POINT ( 'NONE',  ( 97.11602866590727956, 233.0024278399160664, 9.188101187500095079 ) ) ;
#29616 = CARTESIAN_POINT ( 'NONE',  ( 202.9830217136424437, 279.0700886485516889, 15.21791590704638075 ) ) ;
#29617 = CARTESIAN_POINT ( 'NONE',  ( 178.3900700529107439, 269.3831628842910959, -16.31511681271764047 ) ) ;
#29618 = CARTESIAN_POINT ( 'NONE',  ( 81.56933533924238588, 42.63988948739947205, -7.637657182551536472 ) ) ;
#29619 = B_SPLINE_SURFACE_WITH_KNOTS ( 'NONE', 3, 1, ( 
 ( #88738, #65373 ),
 ( #35468, #20284 ),
 ( #96821, #27379 ),
 ( #3594, #49670 ),
 ( #73987, #51158 ),
 ( #82122, #43043 ),
 ( #80124, #64887 ),
 ( #58751, #3116 ),
 ( #81612, #95833 ),
 ( #81128, #58264 ),
 ( #97303, #34002 ),
 ( #12695, #89242 ),
 ( #19792, #26386 ),
 ( #64380, #50660 ),
 ( #27871, #57762 ),
 ( #4571, #42554 ),
 ( #89723, #12182 ),
 ( #19309, #74501 ),
 ( #34474, #5079 ),
 ( #95342, #56771 ),
 ( #25899, #87753 ),
 ( #42072, #18294 ),
 ( #49188, #10686 ),
 ( #41564, #57264 ),
 ( #50175, #72508 ),
 ( #88239, #18790 ),
 ( #80626, #11202 ),
 ( #73004, #96315 ),
 ( #26883, #11695 ),
 ( #73487, #22257 ),
 ( #97791, #45055 ) ),
 .UNSPECIFIED., .F., .F., .F.,
 ( 4, 3, 3, 3, 3, 3, 3, 3, 3, 3, 4 ),
 ( 2, 2 ),
 ( 0.000000000000000000, 0.1333490885032390105, 0.3007194338854328186, 0.4699862290245252483, 0.5844252810809424936, 0.6686540514502805621, 0.7354980260655528124, 0.8028463152565618044, 0.8633854507757205976, 0.9437142632667329112, 1.000000000000000000 ),
 ( 0.000000000000000000, 1.000000000000000000 ),
 .UNSPECIFIED. ) ;
#29620 = VERTEX_POINT ( 'NONE', #17813 ) ;
#29621 = ORIENTED_EDGE ( 'NONE', *, *, #75477, .F. ) ;
#29622 = ORIENTED_EDGE ( 'NONE', *, *, #97854, .F. ) ;
#29623 = LINE ( 'NONE', #84357, #62800 ) ;
#29624 = ORIENTED_EDGE ( 'NONE', *, *, #73145, .F. ) ;
#29625 = CARTESIAN_POINT ( 'NONE',  ( 69.55938073166919366, 70.14142446728632763, 4.291733062184300174 ) ) ;
#29626 = VERTEX_POINT ( 'NONE', #93846 ) ;
#29627 = CARTESIAN_POINT ( 'NONE',  ( 208.2175703429120688, 270.0035844679667889, 2.257951022351344150 ) ) ;
#29628 = EDGE_CURVE ( 'NONE', #2384, #94954, #13547, .T. ) ;
#29629 = CARTESIAN_POINT ( 'NONE',  ( 82.38632442250769827, 41.28528657744342922, 3.301102426468717432 ) ) ;
#29630 = CARTESIAN_POINT ( 'NONE',  ( -19.66825484588498085, 93.20605551765035557, 59.99999999999999289 ) ) ;
#29631 = CARTESIAN_POINT ( 'NONE',  ( -19.65312891409030271, 93.06504152958497400, 177.5919119679930134 ) ) ;
#29632 = CARTESIAN_POINT ( 'NONE',  ( 82.69574664279603837, 54.03060105484253484, -15.86596363536033394 ) ) ;
#29633 = CARTESIAN_POINT ( 'NONE',  ( -4.170157060006060235, 26.08383846222962887, -10.00000000000000000 ) ) ;
#29634 = ORIENTED_EDGE ( 'NONE', *, *, #68811, .T. ) ;
#29635 = CARTESIAN_POINT ( 'NONE',  ( 76.92699712112981558, 61.20612098636846099, 15.66493907231634708 ) ) ;
#29636 = CARTESIAN_POINT ( 'NONE',  ( 17.37926562425035826, 12.96004757982088762, -5.678558825948276656 ) ) ;
#29637 = ORIENTED_EDGE ( 'NONE', *, *, #30883, .T. ) ;
#29638 = CARTESIAN_POINT ( 'NONE',  ( 167.4154476021087135, 283.9804021233929348, 9.114543589697493786 ) ) ;
#29639 = CARTESIAN_POINT ( 'NONE',  ( 80.07172880487748046, 57.71088839156739425, 16.60216399474093052 ) ) ;
#29641 = EDGE_LOOP ( 'NONE', ( #91910, #14586, #11933, #91062 ) ) ;
#29640 = CARTESIAN_POINT ( 'NONE',  ( 124.3429387061717364, 231.0494855054051300, -2.679491924311248496 ) ) ;
#29642 = CARTESIAN_POINT ( 'NONE',  ( 202.9216520459657147, 279.1763840310111391, 15.75371595331685803 ) ) ;
#29643 = CARTESIAN_POINT ( 'NONE',  ( 188.2136819673668242, 260.7815903057019682, 2.765234107804726005 ) ) ;
#29644 = CARTESIAN_POINT ( 'NONE',  ( 160.9550112742611248, 282.2102974542603420, -6.127038402763485436 ) ) ;
#29645 = LINE ( 'NONE', #31119, #32782 ) ;
#29646 = CARTESIAN_POINT ( 'NONE',  ( 158.0940639500165901, 257.7445122115800586, 16.87026726729103387 ) ) ;
#29647 = CARTESIAN_POINT ( 'NONE',  ( 174.5970010251735687, 290.1372909713314243, 7.765872408461218512 ) ) ;
#29648 = CARTESIAN_POINT ( 'NONE',  ( 194.6410797438239229, 263.4546428906130018, -0.7807572112392382468 ) ) ;
#29649 = ORIENTED_EDGE ( 'NONE', *, *, #18453, .F. ) ;
#29650 = CARTESIAN_POINT ( 'NONE',  ( 94.05805000844988228, 235.1115022471902876, -5.000000000000047962 ) ) ;
#29651 = CARTESIAN_POINT ( 'NONE',  ( 194.1568482115562517, 293.9028091603209987, -14.13911859744283461 ) ) ;
#29652 = CARTESIAN_POINT ( 'NONE',  ( 2.169146224190643846, 165.3927522451418213, 10.00000000000009592 ) ) ;
#29653 = CARTESIAN_POINT ( 'NONE',  ( 82.86199955364607206, 53.47446029988319793, -15.31866780845555098 ) ) ;
#29654 = DIRECTION ( 'NONE',  ( 0.000000000000000000, 0.000000000000000000, 1.000000000000000000 ) ) ;
#29655 = CARTESIAN_POINT ( 'NONE',  ( 164.0834751870549439, 246.4460796239905562, -8.551802143958536107 ) ) ;
#29656 = CARTESIAN_POINT ( 'NONE',  ( 85.60939809066302075, 44.62657166848472912, -7.207540832648801299 ) ) ;
#29657 = EDGE_CURVE ( 'NONE', #7863, #45522, #79144, .T. ) ;
#29658 = CARTESIAN_POINT ( 'NONE',  ( 161.5845086034577776, 251.1610536727440603, -12.80556992964895713 ) ) ;
#29660 = CARTESIAN_POINT ( 'NONE',  ( 76.09137042060903866, 65.46242010497813624, 13.98445105613830286 ) ) ;
#29659 = CARTESIAN_POINT ( 'NONE',  ( -3.478321416370212305, 177.9869531367911293, 4.594050593750046652 ) ) ;
#29661 = CARTESIAN_POINT ( 'NONE',  ( 185.0981174815935617, 295.5755628286759134, 8.523774916173438854 ) ) ;
#29662 = ORIENTED_EDGE ( 'NONE', *, *, #63348, .F. ) ;
#29663 = ORIENTED_EDGE ( 'NONE', *, *, #65791, .T. ) ;
#29664 = DIRECTION ( 'NONE',  ( -0.000000000000000000, -0.000000000000000000, -1.000000000000000000 ) ) ;
#29665 = CARTESIAN_POINT ( 'NONE',  ( -19.65312891409030271, 93.06504152958497400, 59.99999999999999289 ) ) ;
#29666 = CARTESIAN_POINT ( 'NONE',  ( 175.5383291916544408, 291.1589915617879001, 3.239589670356908258 ) ) ;
#29667 = CARTESIAN_POINT ( 'NONE',  ( 87.51647913336857698, 44.56403561216112053, 4.883618514853080406 ) ) ;
#29668 = CARTESIAN_POINT ( 'NONE',  ( 201.9466639498089648, 280.8651129503298876, -16.50130735264049164 ) ) ;
#29669 = CARTESIAN_POINT ( 'NONE',  ( 83.75618562079634444, 45.13567822924630235, 9.457446474821283644 ) ) ;
#29670 = CARTESIAN_POINT ( 'NONE',  ( 150.0383903883423500, 276.7166470372682738, 3.302347238614709912 ) ) ;
#29671 = B_SPLINE_CURVE_WITH_KNOTS ( 'NONE', 3,
 ( #27067, #95522, #26567, #96497, #64565, #43234, #57948, #19966, #97004, #19493 ),
 .UNSPECIFIED., .F., .F.,
 ( 4, 2, 2, 2, 4 ),
 ( 2.941174414789049541E-15, 0.0004007808608854804104, 0.0008015617217680197056, 0.001202342582650559001, 0.001603123443533098188 ),
 .UNSPECIFIED. ) ;
#29672 = CARTESIAN_POINT ( 'NONE',  ( 20.74358691754956396, 182.7833772461660544, -9.188101187500095079 ) ) ;
#29673 = VECTOR ( 'NONE', #37295, 1000.000000000000000 ) ;
#29674 = CARTESIAN_POINT ( 'NONE',  ( 128.9971094863694532, 233.0327760586659451, 1.948934522072303157E-15 ) ) ;
#29675 = CARTESIAN_POINT ( 'NONE',  ( 178.7059724048094154, 292.0117454520415095, -7.090766484047969165 ) ) ;
#29676 = CARTESIAN_POINT ( 'NONE',  ( 183.0630607540572043, 257.7369719463336537, -2.333968474862014642 ) ) ;
#29677 = CARTESIAN_POINT ( 'NONE',  ( 206.3344875830494516, 271.9951829204101159, -7.959596699499296157 ) ) ;
#29678 = CONICAL_SURFACE ( 'NONE', #54798, 10.00000000000000711, 0.7853981633974608245 ) ;
#29679 = AXIS2_PLACEMENT_3D ( 'NONE', #59945, #85300, #7755 ) ;
#29680 = CARTESIAN_POINT ( 'NONE',  ( 178.1741645575075381, 283.4573702867252791, -14.54551446833769290 ) ) ;
#29681 = CARTESIAN_POINT ( 'NONE',  ( 77.91090169867500492, 54.32762231749097026, -16.00590757115833540 ) ) ;
#29682 = CARTESIAN_POINT ( 'NONE',  ( 155.3738696901333469, 261.5315588585399951, 17.02116401938635804 ) ) ;
#29683 = CARTESIAN_POINT ( 'NONE',  ( 161.2977680094314223, 251.2710659906439616, -13.03191437619249982 ) ) ;
#29684 = CARTESIAN_POINT ( 'NONE',  ( 189.6666044902458168, 284.7049877867155487, 17.41007887138588117 ) ) ;
#29685 = FACE_OUTER_BOUND ( 'NONE', #14566, .T. ) ;
#29686 = CARTESIAN_POINT ( 'NONE',  ( 170.7208444631169755, 279.4758202746681377, 13.90914101253246393 ) ) ;
#29687 = CARTESIAN_POINT ( 'NONE',  ( 192.6195712009543399, 265.2424128860524206, 7.804296869474439013 ) ) ;
#29688 = CARTESIAN_POINT ( 'NONE',  ( 174.4665098196985298, 288.5002641398569949, -10.08633113632384237 ) ) ;
#29689 = CARTESIAN_POINT ( 'NONE',  ( 61.41971759977597145, 206.2677522451418781, 10.00000000000009592 ) ) ;
#29690 = CARTESIAN_POINT ( 'NONE',  ( -32.57773935851065517, 93.92637809958223727, 43.89948692389421581 ) ) ;
#29691 = CARTESIAN_POINT ( 'NONE',  ( 185.0331805397589733, 269.4951233173647438, 15.91801816997161545 ) ) ;
#29692 = CARTESIAN_POINT ( 'NONE',  ( 86.72372382049398709, 227.0024278399160949, 9.188101187500095079 ) ) ;
#29693 = CARTESIAN_POINT ( 'NONE',  ( 14.44138481658839090, 10.19860640527290663, 2.839279412974134775 ) ) ;
#29694 = CARTESIAN_POINT ( 'NONE',  ( 150.8757650385446993, 269.3225046528533539, 14.31332712971473953 ) ) ;
#29695 = DIRECTION ( 'NONE',  ( 1.000000000000000000, -7.930164461608259453E-16, 0.000000000000000000 ) ) ;
#29697 = CARTESIAN_POINT ( 'NONE',  ( 83.90285338613423960, 42.24628314658283301, -3.729123792273444149 ) ) ;
#29696 = CARTESIAN_POINT ( 'NONE',  ( 49.93886538132678510, 83.40144735776343055, -10.00000000000000000 ) ) ;
#29698 = FACE_OUTER_BOUND ( 'NONE', #48413, .T. ) ;
#29699 = DIRECTION ( 'NONE',  ( 0.5000000000000002220, -0.8660254037844387076, -0.000000000000000000 ) ) ;
#29700 = CARTESIAN_POINT ( 'NONE',  ( 173.5309596338303493, 267.4569899417176657, -16.80614428785976955 ) ) ;
#29701 = CARTESIAN_POINT ( 'NONE',  ( 32.17510246534131113, 41.68290643055190259, 3.479690158560446702E-15 ) ) ;
#29702 = CARTESIAN_POINT ( 'NONE',  ( 147.1125781744767949, 275.8405354997948962, -5.216646253929903665 ) ) ;
#29703 = CARTESIAN_POINT ( 'NONE',  ( -22.42236680055709641, 157.8615022471902591, 0.000000000000000000 ) ) ;
#29704 = ORIENTED_EDGE ( 'NONE', *, *, #50811, .F. ) ;
#29705 = CARTESIAN_POINT ( 'NONE',  ( 31.76189289227714951, 20.19860640527293683, 2.839279412974134775 ) ) ;
#29706 = CARTESIAN_POINT ( 'NONE',  ( 28.35053034700846197, 115.5856344849812274, 59.99999999999999289 ) ) ;
#29707 = CARTESIAN_POINT ( 'NONE',  ( 193.1649355862271591, 296.0755126543221536, -12.21556774862162698 ) ) ;
#29708 = PLANE ( 'NONE',  #76816 ) ;
#29709 = ORIENTED_EDGE ( 'NONE', *, *, #8899, .F. ) ;
#29710 = ADVANCED_FACE ( 'NONE', ( #71021 ), #2618, .F. ) ;
#29711 = CARTESIAN_POINT ( 'NONE',  ( 70.54793603911069511, 60.92313004140932264, 14.99536235483401292 ) ) ;
#29712 = CARTESIAN_POINT ( 'NONE',  ( 159.5764336135613632, 254.2525046211064819, 15.32981087583629076 ) ) ;
#29713 = CARTESIAN_POINT ( 'NONE',  ( 180.7071999899477532, 263.3223274914530521, -12.85640988611793745 ) ) ;
#29714 = EDGE_CURVE ( 'NONE', #14275, #91554, #99779, .T. ) ;
#29715 = CARTESIAN_POINT ( 'NONE',  ( 169.3416567082309712, 252.0478821765268549, -8.660523848214891629 ) ) ;
#29716 = LINE ( 'NONE', #82961, #98008 ) ;
#29717 = CARTESIAN_POINT ( 'NONE',  ( 140.8234218128096700, 242.1115022471902023, -5.000000000000041744 ) ) ;
#29718 = VERTEX_POINT ( 'NONE', #95851 ) ;
#29719 = CARTESIAN_POINT ( 'NONE',  ( 73.04738217724886340, 69.71546789186045601, 9.669594540409617522 ) ) ;
#29720 = EDGE_CURVE ( 'NONE', #31958, #29236, #74017, .T. ) ;
#29721 = VERTEX_POINT ( 'NONE', #94337 ) ;
#29722 = CARTESIAN_POINT ( 'NONE',  ( 78.38601017018802963, 61.50250219569392129, 16.18534724403902914 ) ) ;
#29723 = EDGE_CURVE ( 'NONE', #39441, #59283, #51704, .T. ) ;
#29724 = CARTESIAN_POINT ( 'NONE',  ( 185.2584469233223388, 292.7362939515155631, -10.54904948314711177 ) ) ;
#29725 = ORIENTED_EDGE ( 'NONE', *, *, #32427, .F. ) ;
#29726 = CARTESIAN_POINT ( 'NONE',  ( 199.4720805209845196, 266.1420231043892954, 4.760232788326643316 ) ) ;
#29727 = CARTESIAN_POINT ( 'NONE',  ( 159.1834766195183022, 255.6368035042336260, 16.04288454290252375 ) ) ;
#29728 = CARTESIAN_POINT ( 'NONE',  ( 190.9576542968843569, 279.0470868181286619, -16.53509681315556890 ) ) ;
#29729 = CARTESIAN_POINT ( 'NONE',  ( 192.9443876183610769, 296.4575129401721370, -13.55710008152484569 ) ) ;
#29730 = CARTESIAN_POINT ( 'NONE',  ( 153.0790963368640689, 265.5062228982576471, -17.74594954892339160 ) ) ;
#29731 = VECTOR ( 'NONE', #5544, 1000.000000000000114 ) ;
#29732 = CARTESIAN_POINT ( 'NONE',  ( 32.50825522076439000, 36.95586893147758190, 7.433330006724141015 ) ) ;
#29733 = CARTESIAN_POINT ( 'NONE',  ( 81.62968001876643598, 55.78593752935011452, -16.36028778889454927 ) ) ;
#29734 = DIRECTION ( 'NONE',  ( -0.000000000000000000, 0.000000000000000000, 1.000000000000000000 ) ) ;
#29735 = CARTESIAN_POINT ( 'NONE',  ( 87.45809072578427390, 45.51379687347738923, 7.041989649719552880 ) ) ;
#29736 = ORIENTED_EDGE ( 'NONE', *, *, #53101, .F. ) ;
#29737 = AXIS2_PLACEMENT_3D ( 'NONE', #59232, #20781, #15638 ) ;
#29738 = ORIENTED_EDGE ( 'NONE', *, *, #78554, .T. ) ;
#29739 = CARTESIAN_POINT ( 'NONE',  ( 205.0994677818405023, 275.4042965269534307, -14.14519517703424789 ) ) ;
#29740 = CARTESIAN_POINT ( 'NONE',  ( 161.9775247817796924, 252.0936927241524472, 14.33142805341373283 ) ) ;
#29741 = CARTESIAN_POINT ( 'NONE',  ( 79.60263393892513761, 55.67592396758841744, 16.11189329299018880 ) ) ;
#29742 = B_SPLINE_CURVE_WITH_KNOTS ( 'NONE', 3,
 ( #13147, #50615, #82584, #97265, #66822, #12651, #27832, #20746, #75440, #51117, #73447, #89202, #28318, #19266, #81085, #98246, #29333, #67318, #6023, #60199, #28834, #34919, #81569, #59715, #74459, #36414, #90681, #36919, #19750, #44004, #65815, #5039, #11651, #35921, #50133, #96777, #21237, #42511, #74946, #98753, #51632, #44510, #97750, #52116, #27342, #59197 ),
 .UNSPECIFIED., .F., .F.,
 ( 4, 1, 1, 1, 2, 2, 1, 1, 1, 2, 2, 1, 1, 2, 2, 1, 1, 2, 2, 1, 1, 2, 2, 1, 2, 2, 1, 2, 2, 4 ),
 ( 0.000000000000000000, 0.06250000000001772194, 0.09375000000002634004, 0.1093750000000307532, 0.1171875000000328210, 0.1250000000000348888, 0.1875000000000514588, 0.2187500000000598410, 0.2343750000000623945, 0.2421875000000621170, 0.2500000000000618394, 0.3125000000000588973, 0.3437500000000590084, 0.3593750000000572875, 0.3750000000000555112, 0.4375000000000416334, 0.4687500000000364708, 0.4843750000000339173, 0.5000000000000313083, 0.5625000000000253131, 0.5937500000000219824, 0.6093750000000203171, 0.6250000000000186517, 0.6875000000000177636, 0.7187500000000156541, 0.7500000000000134337, 0.8125000000000118794, 0.8437500000000092149, 0.8750000000000065503, 1.000000000000000000 ),
 .UNSPECIFIED. ) ;
#29744 = CARTESIAN_POINT ( 'NONE',  ( 165.1530561822516461, 246.1540134663977426, 3.111834517001636602 ) ) ;
#29743 = CARTESIAN_POINT ( 'NONE',  ( 164.3330377059402849, 246.0138246616164110, 7.208046019122525294 ) ) ;
#29745 = CARTESIAN_POINT ( 'NONE',  ( 78.60735446187601383, 47.91558663937575346, -14.46554739992949834 ) ) ;
#29746 = CARTESIAN_POINT ( 'NONE',  ( 149.0807665407234026, 276.4376266709116408, -5.539133476438467873 ) ) ;
#29747 = CARTESIAN_POINT ( 'NONE',  ( 76.11246596381349150, 60.38636913568999631, -15.73763889482215284 ) ) ;
#29748 = CARTESIAN_POINT ( 'NONE',  ( 82.11498198633205448, 40.81356640863849350, 1.533337055892688428 ) ) ;
#29749 = CARTESIAN_POINT ( 'NONE',  ( 170.7538221939619518, 287.5752100735740555, -4.616036123583530326 ) ) ;
#29750 = CARTESIAN_POINT ( 'NONE',  ( 77.10166062722221625, 63.64310012191319288, -15.01751612965061788 ) ) ;
#29751 = AXIS2_PLACEMENT_3D ( 'NONE', #39426, #99764, #15131 ) ;
#29752 = CARTESIAN_POINT ( 'NONE',  ( 178.0362721790638716, 255.4572819550275256, 5.227042922011960968 ) ) ;
#29753 = CARTESIAN_POINT ( 'NONE',  ( 112.3797264076079756, 241.8149278399160949, 9.188101187500093303 ) ) ;
#29754 = EDGE_LOOP ( 'NONE', ( #19165, #73836, #66615, #93167 ) ) ;
#29755 = CARTESIAN_POINT ( 'NONE',  ( 183.3817364967617607, 260.1897163651752294, -9.412515908218015426 ) ) ;
#29756 = CARTESIAN_POINT ( 'NONE',  ( 38.99862784774133218, 37.91421378149922816, 9.188101187500008038 ) ) ;
#29757 = CARTESIAN_POINT ( 'NONE',  ( 188.3087688221885685, 273.5212203147432319, 15.65619296925988380 ) ) ;
#29758 = EDGE_LOOP ( 'NONE', ( #57441, #29767, #95896, #84712 ) ) ;
#29759 = ORIENTED_EDGE ( 'NONE', *, *, #54053, .F. ) ;
#29760 = CARTESIAN_POINT ( 'NONE',  ( 86.79909420986851387, 45.86349359382401047, -8.229471332425589480 ) ) ;
#29761 = FACE_OUTER_BOUND ( 'NONE', #73105, .T. ) ;
#29762 = CARTESIAN_POINT ( 'NONE',  ( 192.8192650027745572, 296.6742316675438929, 11.53388506931248969 ) ) ;
#29763 = CARTESIAN_POINT ( 'NONE',  ( 25.64143417502910083, 37.73705186507756082, -3.090169943749475845 ) ) ;
#29764 = ORIENTED_EDGE ( 'NONE', *, *, #59224, .T. ) ;
#29765 = CARTESIAN_POINT ( 'NONE',  ( 147.9745743502305118, 274.3475143274592938, 10.02752110366533778 ) ) ;
#29766 =( BOUNDED_CURVE ( )  B_SPLINE_CURVE ( 2, ( #92410, #17366, #34088, #95435, #41149, #18887, #56358, #9793, #3684 ),
 .UNSPECIFIED., .F., .T. ) 
 B_SPLINE_CURVE_WITH_KNOTS ( ( 3, 2, 2, 2, 3 ),
 ( 0.2459677419354838745, 0.2473118279569892497, 0.2500000000000000000, 0.2526881720430107503, 0.2540322580645161255 ),
 .UNSPECIFIED. ) 
 CURVE ( )  GEOMETRIC_REPRESENTATION_ITEM ( )  RATIONAL_B_SPLINE_CURVE ( ( 0.9330127018922194093, 0.9330127018922194093, 1.000000000000000000, 0.8660254037844387076, 1.000000000000000000, 0.8660254037844387076, 1.000000000000000000, 0.9330127018922194093, 0.9330127018922194093 ) ) 
 REPRESENTATION_ITEM ( '' )  );
#29767 = ORIENTED_EDGE ( 'NONE', *, *, #98949, .F. ) ;
#29768 = CARTESIAN_POINT ( 'NONE',  ( 45.83126033165611091, 187.2677522451417929, -5.000000000000041744 ) ) ;
#29769 = ORIENTED_EDGE ( 'NONE', *, *, #5220, .F. ) ;
#29770 = CARTESIAN_POINT ( 'NONE',  ( 151.3542526322075901, 269.2885850756041464, -14.28695254860580199 ) ) ;
#29771 = LINE ( 'NONE', #7459, #44943 ) ;
#29772 = CARTESIAN_POINT ( 'NONE',  ( 8.758203689844268780, 28.55466486950697913, -1.111400068045478839E-16 ) ) ;
#29773 = EDGE_CURVE ( 'NONE', #97093, #87466, #27407, .T. ) ;
#29774 = CARTESIAN_POINT ( 'NONE',  ( 83.23441648756779898, 46.93106052681729778, 11.58471493876596270 ) ) ;
#29776 = CARTESIAN_POINT ( 'NONE',  ( -19.65312891409030271, 93.06504152958497400, -10.00000000000000888 ) ) ;
#29775 = DIRECTION ( 'NONE',  ( -0.000000000000000000, 0.000000000000000000, -1.000000000000000000 ) ) ;
#29777 = CARTESIAN_POINT ( 'NONE',  ( 153.4495116231415750, 264.8646448025247082, -16.73555355292144498 ) ) ;
#29778 = ORIENTED_EDGE ( 'NONE', *, *, #72017, .F. ) ;
#29779 = CARTESIAN_POINT ( 'NONE',  ( 204.7705395286511703, 275.9740169735222821, 14.67688412961845579 ) ) ;
#29780 = B_SPLINE_CURVE_WITH_KNOTS ( 'NONE', 3,
 ( #77111, #6726, #37604, #46712, #22420, #53311, #84266, #76624, #22908, #5724, #38608, #36612, #75634, #14813, #53795, #46195, #69512, #29041, #126, #6220, #31010, #61900, #92850, #59911, #90882, #21430, #37116, #68020, #48732, #77640, #39093, #8720, #31502, #79164, #32524, #72033, #2637, #24912, #47210, #32002, #47699, #64420, #25935, #33014 ),
 .UNSPECIFIED., .F., .F.,
 ( 4, 2, 2, 2, 2, 2, 2, 2, 2, 2, 2, 2, 2, 2, 2, 2, 2, 2, 2, 2, 2, 4 ),
 ( 0.001220187808576486330, 0.001695729215737192637, 0.002171270622897898944, 0.002409041326478252205, 0.002646812030058605034, 0.002765697381848733743, 0.002884582733638858115, 0.003122353437219106426, 0.003597894844379531491, 0.004073436251539956122, 0.005024519065860657933, 0.005975601880181360612, 0.006451143287341669884, 0.006926684694501980023, 0.007045570046292093554, 0.007105012722187119961, 0.007164455398082144634, 0.007283340749872173163, 0.007402226101662200825, 0.007877767508822457188, 0.008353308915982713551, 0.008828850323142968179 ),
 .UNSPECIFIED. ) ;
#29781 = CARTESIAN_POINT ( 'NONE',  ( 70.99909089399695006, 61.09348569631758608, 14.50421621802051853 ) ) ;
#29782 = CARTESIAN_POINT ( 'NONE',  ( 190.6381889276718482, 264.1129242778857815, -9.562837835864641534 ) ) ;
#29783 = CARTESIAN_POINT ( 'NONE',  ( 170.1122289929976432, 248.6907458515703411, -0.2685048055858946237 ) ) ;
#29784 = CARTESIAN_POINT ( 'NONE',  ( 189.1301257125411723, 269.7442529300492424, -13.96337808587025719 ) ) ;
#29785 = PLANE ( 'NONE',  #46746 ) ;
#29786 = ADVANCED_FACE ( 'NONE', ( #11713 ), #90240, .F. ) ;
#29787 = CARTESIAN_POINT ( 'NONE',  ( 82.37260210843921016, 42.16043560824383718, 5.885805237006764834 ) ) ;
#29788 = CARTESIAN_POINT ( 'NONE',  ( 21.28706459136418871, 17.45404122711133255, -8.090169943749478065 ) ) ;
#29789 = CARTESIAN_POINT ( 'NONE',  ( 189.6102000772831104, 298.8605291158151545, 7.657631583920184504 ) ) ;
#29790 = CARTESIAN_POINT ( 'NONE',  ( 72.66873115938952310, 70.75946716845891160, -7.138114697723673352 ) ) ;
#29791 = CARTESIAN_POINT ( 'NONE',  ( 80.68904315757745849, 208.2048013555409796, 4.594050593750051981 ) ) ;
#29792 = CARTESIAN_POINT ( 'NONE',  ( 159.3237119419271437, 254.6902313965507858, -15.56765445935501191 ) ) ;
#29793 = CARTESIAN_POINT ( 'NONE',  ( -17.42236680055705023, 149.2012482093457777, 0.000000000000000000 ) ) ;
#29794 = CARTESIAN_POINT ( 'NONE',  ( -53.13161237510370682, 51.94668121853939624, 59.99999999999999289 ) ) ;
#29795 = EDGE_CURVE ( 'NONE', #58166, #20250, #17099, .T. ) ;
#29796 = CARTESIAN_POINT ( 'NONE',  ( 197.3670252091396549, 288.0924216084537761, -16.92913523793449571 ) ) ;
#29797 = CARTESIAN_POINT ( 'NONE',  ( 161.5757715694810770, 250.7895496999525449, -14.51803553215175135 ) ) ;
#29798 = CARTESIAN_POINT ( 'NONE',  ( 66.87949033550695788, 69.18773745924302432, 0.7640449060900401657 ) ) ;
#29800 = CARTESIAN_POINT ( 'NONE',  ( 105.0000000000000000, 10.00000000000003197, 59.99999999999999289 ) ) ;
#29799 = CARTESIAN_POINT ( 'NONE',  ( 73.47103776244834705, 69.18898954907001553, -9.996715955230138562 ) ) ;
#29801 = CARTESIAN_POINT ( 'NONE',  ( 112.2445834879230944, 245.6115022471903160, -5.000000000000047962 ) ) ;
#29802 = CARTESIAN_POINT ( 'NONE',  ( 36.54023192077972482, 39.83478043621391151, -8.090169943749479842 ) ) ;
#29803 = DIRECTION ( 'NONE',  ( -0.000000000000000000, -0.000000000000000000, -1.000000000000000000 ) ) ;
#29804 = DIRECTION ( 'NONE',  ( -0.4055404667435369426, 0.9140770918436990078, 0.000000000000000000 ) ) ;
#29805 = CARTESIAN_POINT ( 'NONE',  ( 72.14269493036653103, 72.23228066185846785, 3.937576401637844281 ) ) ;
#29806 = VECTOR ( 'NONE', #62670, 1000.000000000000000 ) ;
#29807 = CARTESIAN_POINT ( 'NONE',  ( 26.88721494746919660, 177.1423013555409796, -4.594050593750043987 ) ) ;
#29808 = CARTESIAN_POINT ( 'NONE',  ( 52.43496435911014686, 191.8923013555410080, 4.594050593750050204 ) ) ;
#29809 = CARTESIAN_POINT ( 'NONE',  ( 196.4982648257524147, 290.3020170531091821, 16.69353242256149628 ) ) ;
#29811 = DIRECTION ( 'NONE',  ( 0.8660254037844379305, 0.5000000000000011102, 0.000000000000000000 ) ) ;
#29810 = AXIS2_PLACEMENT_3D ( 'NONE', #95595, #86495, #48943 ) ;
#29812 = DIRECTION ( 'NONE',  ( -1.000000000000000000, 0.000000000000000000, 0.000000000000000000 ) ) ;
#29813 = CARTESIAN_POINT ( 'NONE',  ( 143.8274474304129171, 253.8458772461660260, 9.188101187500095079 ) ) ;
#29814 = CARTESIAN_POINT ( 'NONE',  ( 50.56751030825868298, 193.8768266524160140, 9.188101187500096856 ) ) ;
#29815 = CARTESIAN_POINT ( 'NONE',  ( 20.18904385193075868, 29.84336893147756342, -7.433330006724137462 ) ) ;
#29816 = CARTESIAN_POINT ( 'NONE',  ( 199.2383506163646132, 285.5560492466715345, -17.78808061564097898 ) ) ;
#29817 = CARTESIAN_POINT ( 'NONE',  ( -15.56633235393031178, 168.4865022471903160, 10.00000000000009415 ) ) ;
#29818 = CARTESIAN_POINT ( 'NONE',  ( 36.20694410119924811, 43.83705186507757645, 3.090169943749475401 ) ) ;
#29819 = DIRECTION ( 'NONE',  ( 0.9998476951563911586, -0.01745240643728540250, 0.000000000000000000 ) ) ;
#29820 = CARTESIAN_POINT ( 'NONE',  ( 77.17614375499567814, 63.59805229717832731, 15.05336917137992359 ) ) ;
#29821 = CARTESIAN_POINT ( 'NONE',  ( 76.62156306105930526, 63.43458379359962152, 15.37592086074861619 ) ) ;
#29822 = CARTESIAN_POINT ( 'NONE',  ( 179.9582481332349460, 276.5203812193133217, 17.70049429017921128 ) ) ;
#29823 = CARTESIAN_POINT ( 'NONE',  ( 82.10205964440194748, 40.74581685175329682, -0.8055849532097474341 ) ) ;
#29824 = CARTESIAN_POINT ( 'NONE',  ( 153.5342532903791550, 264.7178679293513710, 18.03047267014487431 ) ) ;
#29825 = EDGE_CURVE ( 'NONE', #52395, #31328, #36484, .T. ) ;
#29826 = DIRECTION ( 'NONE',  ( 0.1783728972749415442, 0.9839629614562446225, 0.000000000000000000 ) ) ;
#29827 = CARTESIAN_POINT ( 'NONE',  ( 87.76806118867082773, 45.25231315247835084, -7.033483185435909668 ) ) ;
#29828 = CARTESIAN_POINT ( 'NONE',  ( 99.75938391669748739, 221.7365022471902023, 10.00000000000009592 ) ) ;
#29829 = CARTESIAN_POINT ( 'NONE',  ( 161.3644539559160478, 251.1555625431813894, 12.97746593258196413 ) ) ;
#29830 = CARTESIAN_POINT ( 'NONE',  ( 164.8599319342901310, 270.5031674125197583, -17.06886410118275776 ) ) ;
#29831 = ORIENTED_EDGE ( 'NONE', *, *, #48309, .F. ) ;
#29832 = CARTESIAN_POINT ( 'NONE',  ( 53.24634253151052832, 210.7369531367911293, -4.594050593750048428 ) ) ;
#29833 = EDGE_LOOP ( 'NONE', ( #5468, #88382, #20307, #987 ) ) ;
#29834 = EDGE_CURVE ( 'NONE', #31605, #1734, #43586, .T. ) ;
#29835 = DIRECTION ( 'NONE',  ( 0.4999999999999998890, -0.8660254037844385966, 0.000000000000000000 ) ) ;
#29836 = CARTESIAN_POINT ( 'NONE',  ( 190.5541309856500050, 300.5975588711562523, -4.167177996129430184 ) ) ;
#29837 = CARTESIAN_POINT ( 'NONE',  ( 204.8008807586744524, 272.7600038595665524, -10.89009281376315741 ) ) ;
#29838 = ADVANCED_FACE ( 'NONE', ( #89262 ), #38288, .F. ) ;
#29839 = VERTEX_POINT ( 'NONE', #55567 ) ;
#29840 = FACE_OUTER_BOUND ( 'NONE', #45774, .T. ) ;
#29841 = CARTESIAN_POINT ( 'NONE',  ( 79.26833296275110285, 45.71260820663386681, -12.95081413666752113 ) ) ;
#29842 = CARTESIAN_POINT ( 'NONE',  ( 148.0346525705264469, 274.2434557974783615, -9.381294579651672905 ) ) ;
#29843 = CARTESIAN_POINT ( 'NONE',  ( 44.08135397534552169, 118.8355609772188188, 10.00000000000000000 ) ) ;
#29844 = CARTESIAN_POINT ( 'NONE',  ( 70.34454795188869980, 61.29844696716961749, 14.78467410895967760 ) ) ;
#29845 = CARTESIAN_POINT ( 'NONE',  ( 157.3370492947211119, 258.1312320390110244, 17.02065074437983228 ) ) ;
#29846 = EDGE_LOOP ( 'NONE', ( #40355, #98523, #86147, #56384 ) ) ;
#29847 = CARTESIAN_POINT ( 'NONE',  ( 15.07770630580378501, 30.74646525600389424, 2.839279412974139660 ) ) ;
#29848 = CARTESIAN_POINT ( 'NONE',  ( 75.87287823110008844, 59.20612602118985279, 15.91568303443457388 ) ) ;
#29849 = CARTESIAN_POINT ( 'NONE',  ( 69.39565660130948288, 70.00884411262029516, -4.393149027308437482 ) ) ;
#29850 = CARTESIAN_POINT ( 'NONE',  ( 170.8843335314017509, 274.4719442773359219, 17.28596511953734449 ) ) ;
#29851 = VERTEX_POINT ( 'NONE', #87058 ) ;
#29852 = CARTESIAN_POINT ( 'NONE',  ( 174.1122061744133021, 261.2364706500421789, -15.53837272058243890 ) ) ;
#29853 = DIRECTION ( 'NONE',  ( 0.4242989612870595728, -0.9055221650797523614, 0.000000000000000000 ) ) ;
#29854 = ORIENTED_EDGE ( 'NONE', *, *, #65299, .F. ) ;
#29855 = VERTEX_POINT ( 'NONE', #45967 ) ;
#29856 = CARTESIAN_POINT ( 'NONE',  ( 80.96765023889031454, 49.62782080103354332, -14.15289701881580520 ) ) ;
#29858 = CARTESIAN_POINT ( 'NONE',  ( -68.10632939235270555, 44.28490124273479012, 10.00000000000000000 ) ) ;
#29857 = CARTESIAN_POINT ( 'NONE',  ( 159.4259928985412103, 282.8382026192845160, -3.335402803703788166 ) ) ;
#29859 = CARTESIAN_POINT ( 'NONE',  ( 208.3790849386676598, 269.7238329819538762, -1.525282248498321946 ) ) ;
#29860 = CARTESIAN_POINT ( 'NONE',  ( 204.2129321040862919, 276.9398213635460024, 14.41515352680879758 ) ) ;
#29861 = CARTESIAN_POINT ( 'NONE',  ( 198.6587626159274294, 286.5599251108861267, 17.99840276545888784 ) ) ;
#29862 = DIRECTION ( 'NONE',  ( 1.000000000000000000, 0.000000000000000000, 0.000000000000000000 ) ) ;
#29863 = CARTESIAN_POINT ( 'NONE',  ( 128.9153121871758572, 254.4244531367911293, -4.594050593750046652 ) ) ;
#29864 = CARTESIAN_POINT ( 'NONE',  ( 159.6568082460325115, 254.5034209454928202, -15.34944651258716242 ) ) ;
#29865 = CARTESIAN_POINT ( 'NONE',  ( 178.8631597503538728, 258.1335624377610429, 9.789943529626453866 ) ) ;
#29866 = CARTESIAN_POINT ( 'NONE',  ( 69.78227540684341079, 211.0958772461660544, -9.188101187500095079 ) ) ;
#29867 = ORIENTED_EDGE ( 'NONE', *, *, #83155, .F. ) ;
#29868 = CARTESIAN_POINT ( 'NONE',  ( 174.0353712165220088, 265.6378307261092004, 16.31703135812460914 ) ) ;
#29869 = CARTESIAN_POINT ( 'NONE',  ( 184.3288588942493504, 256.6513847527468215, 0.3136419966290590056 ) ) ;
#29870 = ORIENTED_EDGE ( 'NONE', *, *, #30959, .F. ) ;
#29871 = FACE_OUTER_BOUND ( 'NONE', #52060, .T. ) ;
#29872 = ORIENTED_EDGE ( 'NONE', *, *, #1488, .F. ) ;
#29873 = ORIENTED_EDGE ( 'NONE', *, *, #95425, .T. ) ;
#29874 = CARTESIAN_POINT ( 'NONE',  ( 80.03926378114135787, 227.0177522451419350, 5.000000000000046185 ) ) ;
#29875 = CARTESIAN_POINT ( 'NONE',  ( 66.81218498664068761, 67.51421540899519869, 6.611934933653538238 ) ) ;
#29876 = CARTESIAN_POINT ( 'NONE',  ( 184.3226795282388650, 274.5458599865910969, 17.66928848808302988 ) ) ;
#29877 = CARTESIAN_POINT ( 'NONE',  ( 191.1747001918821525, 299.5227014763493116, -9.654804683100723040 ) ) ;
#29878 = CARTESIAN_POINT ( 'NONE',  ( 15.09101445147005727, 32.21091486745859811, -1.111400068045478839E-16 ) ) ;
#29879 = CARTESIAN_POINT ( 'NONE',  ( 194.4165969972361552, 293.9075714965812267, 14.23342188338008718 ) ) ;
#29880 = CARTESIAN_POINT ( 'NONE',  ( 73.04277380876573034, 70.56196896876862468, 7.835544939490341143 ) ) ;
#29881 = VERTEX_POINT ( 'NONE', #62169 ) ;
#29882 = AXIS2_PLACEMENT_3D ( 'NONE', #87018, #31724, #17549 ) ;
#29883 = CARTESIAN_POINT ( 'NONE',  ( 201.0110605751355877, 282.4856255309966286, -16.99872517744415035 ) ) ;
#29884 = VERTEX_POINT ( 'NONE', #8495 ) ;
#29885 = B_SPLINE_CURVE_WITH_KNOTS ( 'NONE', 3,
 ( #49530, #67092, #50037, #5797, #74732, #80989, #57119, #64747, #83334, #49043 ),
 .UNSPECIFIED., .F., .F.,
 ( 4, 2, 2, 2, 4 ),
 ( 0.000000000000000000, 0.0002622400424272852194, 0.0005244800848545704388, 0.0007867201272818557124, 0.001048960169709140878 ),
 .UNSPECIFIED. ) ;
#29886 = CARTESIAN_POINT ( 'NONE',  ( 76.05862284836669573, 51.28839337040800217, -15.63733761827814561 ) ) ;
#29887 = VECTOR ( 'NONE', #6157, 1000.000000000000000 ) ;
#29888 = CARTESIAN_POINT ( 'NONE',  ( 76.03787485198571972, 65.47122818424047352, -14.36642907054480744 ) ) ;
#29889 = EDGE_CURVE ( 'NONE', #94973, #1578, #40371, .T. ) ;
#29890 = CARTESIAN_POINT ( 'NONE',  ( 197.0145049354283913, 280.1669261707720580, 16.47791621818247165 ) ) ;
#29891 = CARTESIAN_POINT ( 'NONE',  ( 198.2505066714982149, 285.2670451491296149, 0.000000000000000000 ) ) ;
#29892 = CARTESIAN_POINT ( 'NONE',  ( 140.7695555451228984, 242.8923013555409796, 4.594050593750050204 ) ) ;
#29893 = ORIENTED_EDGE ( 'NONE', *, *, #21601, .F. ) ;
#29894 = CARTESIAN_POINT ( 'NONE',  ( 1.096698433646719151, 159.8932355074535678, -2.679491924311248496 ) ) ;
#29895 = CARTESIAN_POINT ( 'NONE',  ( 182.5394281695505185, 257.5236203636924301, 6.760540572999865994 ) ) ;
#29896 = ADVANCED_FACE ( 'NONE', ( #71309, #39366 ), #94130, .F. ) ;
#29897 = DIRECTION ( 'NONE',  ( 1.000000000000000000, 0.000000000000000000, 0.000000000000000000 ) ) ;
#29898 = CARTESIAN_POINT ( 'NONE',  ( 153.2906404175950854, 265.1398178023911782, -17.60231834963988007 ) ) ;
#29899 = CARTESIAN_POINT ( 'NONE',  ( 72.78673888116644264, 70.95540242780744222, 7.715912594624938059 ) ) ;
#29900 = CARTESIAN_POINT ( 'NONE',  ( 69.93916249099559934, 67.39072072629922161, -9.564019846174506512 ) ) ;
#29901 = ORIENTED_EDGE ( 'NONE', *, *, #72773, .T. ) ;
#29902 = CARTESIAN_POINT ( 'NONE',  ( 195.7060787468133185, 265.4134732632927580, 4.554624283109690808 ) ) ;
#29903 = DIRECTION ( 'NONE',  ( -0.8660254037844387076, -0.4999999999999998890, -0.000000000000000000 ) ) ;
#29904 = CARTESIAN_POINT ( 'NONE',  ( 72.40111988405350019, 71.17098879578473714, -6.090184461575853803 ) ) ;
#29905 = CARTESIAN_POINT ( 'NONE',  ( 184.7951035468651355, 263.5683215496842990, -12.50918047892673890 ) ) ;
#29906 = CARTESIAN_POINT ( 'NONE',  ( 73.71283706923053103, 69.58716896801121266, -9.688382991847833026 ) ) ;
#29907 = EDGE_CURVE ( 'NONE', #22014, #42521, #31769, .T. ) ;
#29908 = CARTESIAN_POINT ( 'NONE',  ( 198.7483143037687796, 265.7987759441807043, 0.1112591014730011513 ) ) ;
#29909 = ORIENTED_EDGE ( 'NONE', *, *, #66198, .F. ) ;
#29910 = DIRECTION ( 'NONE',  ( 0.000000000000000000, 0.000000000000000000, 1.000000000000000000 ) ) ;
#29911 = CARTESIAN_POINT ( 'NONE',  ( 71.23505992429709011, 71.80871246845643441, 0.3731813833289527316 ) ) ;
#29912 = AXIS2_PLACEMENT_3D ( 'NONE', #57610, #80473, #48014 ) ;
#29913 = B_SPLINE_CURVE_WITH_KNOTS ( 'NONE', 3,
 ( #64373, #65367, #41050, #87747, #32963, #41559, #11195, #96309, #64881, #25893, #11688, #57756, #71986, #96816 ),
 .UNSPECIFIED., .F., .F.,
 ( 4, 2, 2, 2, 2, 2, 4 ),
 ( 0.0008768251031193197457, 0.001145890065292074367, 0.001414955027464828881, 0.001684019989637583394, 0.001953084951810337908, 0.002491214876155846934, 0.003029344800501355961 ),
 .UNSPECIFIED. ) ;
#29914 = PLANE ( 'NONE',  #67947 ) ;
#29916 = CARTESIAN_POINT ( 'NONE',  ( 196.2319806131264954, 270.7896828814228911, 11.99002728859442257 ) ) ;
#29915 = CARTESIAN_POINT ( 'NONE',  ( 177.3366806090162697, 264.4717330485077014, -15.58596816512555883 ) ) ;
#29917 = CARTESIAN_POINT ( 'NONE',  ( 29.68521398013932711, 18.10801979619930080, 3.090169943749476733 ) ) ;
#29918 = EDGE_CURVE ( 'NONE', #82741, #40944, #9960, .T. ) ;
#29919 = CARTESIAN_POINT ( 'NONE',  ( 151.2546443255573934, 275.3395117651207897, -9.775857568146751220 ) ) ;
#29920 = CARTESIAN_POINT ( 'NONE',  ( 42.87900647455834502, 24.75620593066997444, 8.404119662683931360E-14 ) ) ;
#29921 = CARTESIAN_POINT ( 'NONE',  ( -18.45562326176555956, 23.07528527759725989, 10.00000000000000000 ) ) ;
#29922 = CARTESIAN_POINT ( 'NONE',  ( 159.5764336135613632, 254.2525046211064819, 15.32981087583629076 ) ) ;
#29923 = CARTESIAN_POINT ( 'NONE',  ( -16.57695564860984661, 170.4244531367911293, -4.594050593750046652 ) ) ;
#29924 = PLANE ( 'NONE',  #76005 ) ;
#29925 = ORIENTED_EDGE ( 'NONE', *, *, #12935, .F. ) ;
#29926 = CARTESIAN_POINT ( 'NONE',  ( 178.7469694055837692, 256.4911572975941567, 8.720117528295025622 ) ) ;
#29927 = CARTESIAN_POINT ( 'NONE',  ( 72.57773168451070944, 70.69087215581754435, -7.948841485240754068 ) ) ;
#29928 = CARTESIAN_POINT ( 'NONE',  ( 199.1216527653377000, 285.7581758537840528, -18.37739894744384728 ) ) ;
#29929 = CARTESIAN_POINT ( 'NONE',  ( 13.57207436428344316, 169.4548013555409796, -4.594050593750042211 ) ) ;
#29930 = CARTESIAN_POINT ( 'NONE',  ( 21.58410742392950610, 28.16454794089041869, -10.00000000000000355 ) ) ;
#29931 = CARTESIAN_POINT ( 'NONE',  ( 85.41200716118709124, 49.08779630762384727, 12.38492377717305182 ) ) ;
#29932 = CARTESIAN_POINT ( 'NONE',  ( 157.7847820078105201, 257.3557362317297361, -18.02899742403477035 ) ) ;
#29933 = CARTESIAN_POINT ( 'NONE',  ( 71.86410153269953582, 71.70156373010919992, -3.808556656956898490 ) ) ;
#29934 = CARTESIAN_POINT ( 'NONE',  ( 149.8257819617332700, 277.0756371120140784, 4.657797871342554963 ) ) ;
#29935 = EDGE_CURVE ( 'NONE', #95983, #6973, #42860, .T. ) ;
#29936 = CARTESIAN_POINT ( 'NONE',  ( 175.5126768985223009, 253.5007195332992183, -3.702306847772006915 ) ) ;
#29937 = CARTESIAN_POINT ( 'NONE',  ( 197.9988809731023025, 287.7028736432410483, 18.08661327024293897 ) ) ;
#29938 = VECTOR ( 'NONE', #46069, 1000.000000000000000 ) ;
#29939 = ADVANCED_FACE ( 'NONE', ( #49485 ), #80949, .T. ) ;
#29940 = CARTESIAN_POINT ( 'NONE',  ( 181.9363424492615309, 295.0529423534600255, 1.015868974045746720 ) ) ;
#29941 = CARTESIAN_POINT ( 'NONE',  ( 52.99401211233780629, 194.7365022471902023, 10.00000000000009592 ) ) ;
#29942 = DIRECTION ( 'NONE',  ( 0.4999999999999998890, -0.8660254037844385966, 0.000000000000000000 ) ) ;
#29943 = CARTESIAN_POINT ( 'NONE',  ( 8.456677953475336906, 181.8149278399161233, 9.188101187500093303 ) ) ;
#29944 = CARTESIAN_POINT ( 'NONE',  ( 67.00398746445188181, 69.51674466867500257, -2.934459324224529819 ) ) ;
#29945 = CARTESIAN_POINT ( 'NONE',  ( 36.37119629183458613, 23.12755873383628114, -6.180339887498949025 ) ) ;
#29946 = CARTESIAN_POINT ( 'NONE',  ( 74.18762515466688967, 72.22758258259658248, 0.000000000000000000 ) ) ;
#29947 = CARTESIAN_POINT ( 'NONE',  ( 158.4546827590755811, 270.8972676159339699, 16.19068674916076844 ) ) ;
#29948 = DIRECTION ( 'NONE',  ( -0.03004293549037828290, -0.9995486091367047354, 0.000000000000000000 ) ) ;
#29949 = EDGE_CURVE ( 'NONE', #53789, #87662, #5213, .T. ) ;
#29950 = CARTESIAN_POINT ( 'NONE',  ( 185.2016103895410595, 266.7518736163806352, 14.11053221384207212 ) ) ;
#29951 = CARTESIAN_POINT ( 'NONE',  ( 153.7186906689185832, 265.0943440466812149, -16.48577743300708320 ) ) ;
#29952 = CARTESIAN_POINT ( 'NONE',  ( 160.5614375844315305, 280.0629237280704160, 9.137926588329262856 ) ) ;
#29953 = ITEM_DEFINED_TRANSFORMATION ( 'NONE', 'NONE', #75317,  #68784 ) ;
#29954 = CARTESIAN_POINT ( 'NONE',  ( 14.05709621874952475, 23.51421378149918340, -9.188101187500004485 ) ) ;
#29955 = CARTESIAN_POINT ( 'NONE',  ( 147.7978300115112233, 274.6536445020713018, 7.902890709649431855 ) ) ;
#29956 = CARTESIAN_POINT ( 'NONE',  ( 72.00843944767480309, 59.19984693747115045, 15.36336254789745581 ) ) ;
#29957 = CARTESIAN_POINT ( 'NONE',  ( 194.4459411895494725, 293.8567458645873103, 14.31012567920753042 ) ) ;
#29958 = ORIENTED_EDGE ( 'NONE', *, *, #94882, .F. ) ;
#29959 = CARTESIAN_POINT ( 'NONE',  ( 184.7666555901016636, 290.6098824792631490, 12.15622735957478540 ) ) ;
#29960 = DIRECTION ( 'NONE',  ( -0.3986482622784180418, -0.9171038997749370036, 0.000000000000000000 ) ) ;
#29961 = EDGE_CURVE ( 'NONE', #48040, #35225, #18098, .T. ) ;
#29962 = CARTESIAN_POINT ( 'NONE',  ( 75.30550521261754682, 53.62394084548385109, -16.53342909214022782 ) ) ;
#29963 = CARTESIAN_POINT ( 'NONE',  ( 81.23883169307138985, 42.40595559033209838, 7.569205759766643560 ) ) ;
#29964 = VERTEX_POINT ( 'NONE', #12002 ) ;
#29965 = FACE_OUTER_BOUND ( 'NONE', #92220, .T. ) ;
#29966 = CARTESIAN_POINT ( 'NONE',  ( 72.59885289546373599, 71.51145701098552365, -5.543222466649145197 ) ) ;
#29967 = CARTESIAN_POINT ( 'NONE',  ( -5.101858724868291617, 167.8615022471904012, 2.586156800657061008E-14 ) ) ;
#29968 = CARTESIAN_POINT ( 'NONE',  ( 155.5322964227545413, 261.2571557083629159, -18.35853982030605280 ) ) ;
#29969 = ORIENTED_EDGE ( 'NONE', *, *, #17035, .T. ) ;
#29970 = ORIENTED_EDGE ( 'NONE', *, *, #32439, .T. ) ;
#29972 = CARTESIAN_POINT ( 'NONE',  ( 204.2556901454867955, 276.8657622634082713, 13.61111001399713949 ) ) ;
#29971 = CARTESIAN_POINT ( 'NONE',  ( 186.2372707961799563, 272.0007479897874987, -16.24101813976637487 ) ) ;
#29973 = EDGE_LOOP ( 'NONE', ( #17516, #44959, #33866, #39659 ) ) ;
#29974 = CARTESIAN_POINT ( 'NONE',  ( 201.3715986869907510, 281.8611552031986776, -17.89433714524984964 ) ) ;
#29975 = CARTESIAN_POINT ( 'NONE',  ( 24.60437102317565206, 29.90829794293881605, 10.00000000000000355 ) ) ;
#29976 = FACE_OUTER_BOUND ( 'NONE', #44081, .T. ) ;
#29977 = CARTESIAN_POINT ( 'NONE',  ( 77.32817876982272765, 63.13942984521013813, 15.61058464551962111 ) ) ;
#29978 = ORIENTED_EDGE ( 'NONE', *, *, #51565, .T. ) ;
#29979 = CARTESIAN_POINT ( 'NONE',  ( 148.1672759425158290, 274.0137453789218398, 7.847779094015780110 ) ) ;
#29980 = CIRCLE ( 'NONE', #39652, 70.00000000000001421 ) ;
#29981 = ORIENTED_EDGE ( 'NONE', *, *, #96544, .F. ) ;
#29982 = CARTESIAN_POINT ( 'NONE',  ( 206.3907062969896060, 273.1678058140250300, 11.56942460516550675 ) ) ;
#29983 = DIRECTION ( 'NONE',  ( 0.8660254037844373753, 0.5000000000000021094, 0.000000000000000000 ) ) ;
#29984 = ORIENTED_EDGE ( 'NONE', *, *, #48746, .T. ) ;
#29985 = CARTESIAN_POINT ( 'NONE',  ( 190.2318383114841254, 301.1557861577188078, 3.177919994438449525 ) ) ;
#29986 = DIRECTION ( 'NONE',  ( 0.000000000000000000, 0.000000000000000000, 1.000000000000000000 ) ) ;
#29987 = ORIENTED_EDGE ( 'NONE', *, *, #79857, .T. ) ;
#29988 = CARTESIAN_POINT ( 'NONE',  ( -17.45610439730315733, 75.77995691783453935, 13.40053368761685704 ) ) ;
#29989 = CARTESIAN_POINT ( 'NONE',  ( 33.59574554791263523, 38.13478043621391578, 8.090169943749478065 ) ) ;
#29990 = CARTESIAN_POINT ( 'NONE',  ( 78.18060451095965391, 47.59931466318645477, -14.43139321312144219 ) ) ;
#29991 = CARTESIAN_POINT ( 'NONE',  ( 103.3262782077763120, 218.9155109091896065, 2.679491924311254714 ) ) ;
#29992 = ORIENTED_EDGE ( 'NONE', *, *, #27289, .F. ) ;
#29993 = VERTEX_POINT ( 'NONE', #50478 ) ;
#29994 = CARTESIAN_POINT ( 'NONE',  ( 73.09460200958936582, 69.68087498946766800, 9.152088038772804524 ) ) ;
#29995 = CARTESIAN_POINT ( 'NONE',  ( 147.5498377207569263, 275.0831797495432056, 4.097967709737811326 ) ) ;
#29996 = CARTESIAN_POINT ( 'NONE',  ( 147.6430623265936219, 274.9217099957185155, 8.258152514891218487 ) ) ;
#29997 = CARTESIAN_POINT ( 'NONE',  ( 149.1903793729515257, 272.2416782560088677, 12.95958987445043675 ) ) ;
#29998 = CARTESIAN_POINT ( 'NONE',  ( 192.6224552386041182, 297.0151161785129261, 12.49354144254605181 ) ) ;
#29999 = CARTESIAN_POINT ( 'NONE',  ( 147.1749864263339020, 275.7324412367667605, 0.5903044561608349339 ) ) ;
#30000 = CARTESIAN_POINT ( 'NONE',  ( 191.8456210280128005, 298.3606325003146367, -9.135603544929113085 ) ) ;
#30001 = CARTESIAN_POINT ( 'NONE',  ( 159.9040744856012850, 255.4269131533854420, 16.38690128260775936 ) ) ;
#30002 = CARTESIAN_POINT ( 'NONE',  ( 70.34102847698805761, 68.37141199246802614, 8.639829021907296180 ) ) ;
#30004 = DIRECTION ( 'NONE',  ( -0.9377374661009826307, -0.3473448497826164827, 0.000000000000000000 ) ) ;
#30003 = CARTESIAN_POINT ( 'NONE',  ( 149.4965729687386045, 271.7113353911534546, -11.48413836595348059 ) ) ;
#30005 = CARTESIAN_POINT ( 'NONE',  ( 66.96692701909594803, 66.98780766957318633, 8.644895272513664963 ) ) ;
#30006 = CARTESIAN_POINT ( 'NONE',  ( 168.1440244810862055, 286.5563420518730027, 3.650993266842447849 ) ) ;
#30007 = CARTESIAN_POINT ( 'NONE',  ( 78.69402153464497474, 47.55556487758106954, 14.25945737374057742 ) ) ;
#30008 = ORIENTED_EDGE ( 'NONE', *, *, #58416, .T. ) ;
#30009 = CIRCLE ( 'NONE', #2790, 15.60714546451148799 ) ;
#30010 = CARTESIAN_POINT ( 'NONE',  ( 190.3243315981879107, 300.9955830857887236, -4.786543493425554630 ) ) ;
#30011 = CARTESIAN_POINT ( 'NONE',  ( 75.37844399319210709, 54.42689092199589851, -16.12112201184755733 ) ) ;
#30012 = CARTESIAN_POINT ( 'NONE',  ( 202.9053066868392818, 278.8211341806578503, 15.06259384972848636 ) ) ;
#30013 = CARTESIAN_POINT ( 'NONE',  ( 78.88938659514667506, 46.33750193266715911, 12.91880430790163281 ) ) ;
#30014 = CIRCLE ( 'NONE', #68841, 70.00000000000001421 ) ;
#30015 = CARTESIAN_POINT ( 'NONE',  ( 190.8763451968731886, 298.2172932904716731, -9.609917527147246119 ) ) ;
#30016 = CARTESIAN_POINT ( 'NONE',  ( 75.78590872935743050, 56.04690169322937265, -16.60533866342026244 ) ) ;
#30017 = CARTESIAN_POINT ( 'NONE',  ( 169.1095075563655143, 285.5585736834383965, -7.565734909916525197 ) ) ;
#30018 = ORIENTED_EDGE ( 'NONE', *, *, #60232, .T. ) ;
#30019 = DIRECTION ( 'NONE',  ( 1.000000000000000000, 0.000000000000000000, 0.000000000000000000 ) ) ;
#30020 = CARTESIAN_POINT ( 'NONE',  ( 206.8851632406098702, 272.3113812655195716, -9.957011741946159233 ) ) ;
#30021 = CARTESIAN_POINT ( 'NONE',  ( 72.49672817265226854, 71.70303783552662935, 5.966909785267820787 ) ) ;
#30022 = CARTESIAN_POINT ( 'NONE',  ( 42.80017141841058503, 185.5177522451417929, 5.000000000000051514 ) ) ;
#30023 = CARTESIAN_POINT ( 'NONE',  ( 112.9213393807382886, 229.8768266524160140, 9.188101187500096856 ) ) ;
#30024 = EDGE_CURVE ( 'NONE', #58166, #10592, #58088, .T. ) ;
#30025 = CARTESIAN_POINT ( 'NONE',  ( 199.1944722252943905, 285.6320488493591938, -18.17555833707144686 ) ) ;
#30026 = CARTESIAN_POINT ( 'NONE',  ( 79.14312167556931854, 57.64441083166269664, 0.000000000000000000 ) ) ;
#30027 = CARTESIAN_POINT ( 'NONE',  ( 157.3412122618683497, 258.1240215684019290, 16.75554199904894048 ) ) ;
#30028 = CARTESIAN_POINT ( 'NONE',  ( 172.2604035111071994, 250.9201653963260696, -4.030415234405903213 ) ) ;
#30029 = CARTESIAN_POINT ( 'NONE',  ( 30.29666933122289407, 197.4869531367911293, 4.594050593750046652 ) ) ;
#30030 = DIRECTION ( 'NONE',  ( -0.5369817302126803638, 0.8435938723211520163, 0.000000000000000000 ) ) ;
#30031 = VERTEX_POINT ( 'NONE', #95651 ) ;
#30032 = CARTESIAN_POINT ( 'NONE',  ( 176.7754569686200625, 262.2288517614920238, -15.26617267356994567 ) ) ;
#30033 = CARTESIAN_POINT ( 'NONE',  ( 177.9063225670694521, 265.5284957633090244, 15.62507714768716305 ) ) ;
#30034 = EDGE_CURVE ( 'NONE', #71782, #85768, #64310, .T. ) ;
#30035 = CARTESIAN_POINT ( 'NONE',  ( 73.60582443374298123, 62.09963750435122165, 15.23117417853161548 ) ) ;
#30036 = EDGE_CURVE ( 'NONE', #26501, #99967, #83677, .T. ) ;
#30037 = LINE ( 'NONE', #37626, #74304 ) ;
#30038 = CARTESIAN_POINT ( 'NONE',  ( 81.65512716465181597, 41.52065711327874453, -5.350319245000699553 ) ) ;
#30039 = LINE ( 'NONE', #22932, #41436 ) ;
#30040 = CARTESIAN_POINT ( 'NONE',  ( 25.96864935082048831, 154.0458036431183189, 21.50000000000008527 ) ) ;
#30041 = CARTESIAN_POINT ( 'NONE',  ( 104.3601438707544133, 224.3927522451418213, -10.00000000000009059 ) ) ;
#30042 = CARTESIAN_POINT ( 'NONE',  ( 65.88310562893971678, 69.02589174555536999, 1.996831191813055240 ) ) ;
#30043 = ORIENTED_EDGE ( 'NONE', *, *, #21952, .T. ) ;
#30044 = DIRECTION ( 'NONE',  ( 0.4755282581475757664, -0.8236391035463335175, -0.3090169943749448977 ) ) ;
#30045 = CARTESIAN_POINT ( 'NONE',  ( 155.4838159167009906, 279.7196639355038883, -1.614956184126561611 ) ) ;
#30046 = CARTESIAN_POINT ( 'NONE',  ( -27.42236680055714260, 166.5217562850347406, 1.224646799147364892E-15 ) ) ;
#30047 = TOROIDAL_SURFACE ( 'NONE', #86743, 16.10714546451156437, 0.5000000000000000000 ) ;
#30048 = CARTESIAN_POINT ( 'NONE',  ( 12.00188267627663308, 186.9244531367911293, -4.594050593750046652 ) ) ;
#30049 = CARTESIAN_POINT ( 'NONE',  ( 72.09295132551602592, 68.68266118357180972, -10.22840576930964396 ) ) ;
#30050 = CARTESIAN_POINT ( 'NONE',  ( 192.2734905965078553, 272.0667696282540646, 14.25396137523372886 ) ) ;
#30051 = CARTESIAN_POINT ( 'NONE',  ( 192.4867975473904949, 297.2500821921321972, -13.04960750009181325 ) ) ;
#30052 = CARTESIAN_POINT ( 'NONE',  ( -52.33464467766007999, 32.58262665401804270, -10.00000000000000000 ) ) ;
#30054 = CARTESIAN_POINT ( 'NONE',  ( 57.27886009182306282, 210.0024278399160949, -9.188101187500093303 ) ) ;
#30053 = CARTESIAN_POINT ( 'NONE',  ( 174.4584291273796453, 286.7546150749506637, 10.19462971651400807 ) ) ;
#30055 = CARTESIAN_POINT ( 'NONE',  ( 200.3414094930810165, 283.6454952284590263, 16.87912319229835489 ) ) ;
#30056 = CARTESIAN_POINT ( 'NONE',  ( 72.87126216515173383, 57.15041428312686378, 15.90107093336461475 ) ) ;
#30057 = CARTESIAN_POINT ( 'NONE',  ( -32.67881874348327642, 96.08878909247250988, 44.13137598596502187 ) ) ;
#30058 = CARTESIAN_POINT ( 'NONE',  ( 66.26881226693740246, 68.72770711070297978, -4.319471721241867179 ) ) ;
#30059 =( BOUNDED_CURVE ( )  B_SPLINE_CURVE ( 2, ( #73093, #35054, #11788, #81704, #4669, #10783, #2690, #96407, #88838 ),
 .UNSPECIFIED., .F., .T. ) 
 B_SPLINE_CURVE_WITH_KNOTS ( ( 3, 2, 2, 2, 3 ),
 ( 0.5766129032258064946, 0.5779569892473118697, 0.5806451612903226200, 0.5833333333333333703, 0.5846774193548387455 ),
 .UNSPECIFIED. ) 
 CURVE ( )  GEOMETRIC_REPRESENTATION_ITEM ( )  RATIONAL_B_SPLINE_CURVE ( ( 0.9330127018922194093, 0.9330127018922194093, 1.000000000000000000, 0.8660254037844387076, 1.000000000000000000, 0.8660254037844387076, 1.000000000000000000, 0.9330127018922194093, 0.9330127018922194093 ) ) 
 REPRESENTATION_ITEM ( '' )  );
#30060 = ORIENTED_EDGE ( 'NONE', *, *, #96231, .T. ) ;
#30061 = AXIS2_PLACEMENT_3D ( 'NONE', #71392, #70367, #48065 ) ;
#30062 = EDGE_CURVE ( 'NONE', #24937, #64281, #3895, .T. ) ;
#30063 = CARTESIAN_POINT ( 'NONE',  ( 165.4943819508360434, 269.3512166473536809, 17.11647148302431631 ) ) ;
#30064 = CARTESIAN_POINT ( 'NONE',  ( 10.91961124514380366, 177.1115022471902307, 10.00000000000009592 ) ) ;
#30065 = CARTESIAN_POINT ( 'NONE',  ( 163.9354095869165633, 246.7025367662834014, -7.289870401565430313 ) ) ;
#30066 = CARTESIAN_POINT ( 'NONE',  ( 134.1114646098825176, 257.4244531367911577, -4.594050593750046652 ) ) ;
#30067 = CARTESIAN_POINT ( 'NONE',  ( 33.38390286057418166, 24.98920272979928470, 7.433330006724137462 ) ) ;
#30068 = B_SPLINE_CURVE_WITH_KNOTS ( 'NONE', 3,
 ( #9141, #30934, #61817, #7129, #68926, #8143, #62826, #77555, #53718, #1556, #31424, #53237, #61324, #78553, #7634, #54718, #39017, #93782, #62314, #93269, #77028, #39506, #38013, #70433, #85700, #16236, #47626, #92769, #31922, #30435, #84189, #47127, #24341, #70954, #78050, #50, #32440, #92286, #55216, #91774, #22339, #14738, #45621, #99851, #84678, #22833 ),
 .UNSPECIFIED., .F., .F.,
 ( 4, 2, 2, 2, 2, 2, 2, 2, 2, 2, 2, 2, 2, 2, 2, 2, 2, 2, 2, 2, 2, 2, 4 ),
 ( 0.0005579239295771397551, 0.001560669089151106408, 0.002062041668938070435, 0.002187384813884852858, 0.002312727958831635282, 0.002438071103778417272, 0.002563414248725199695, 0.002814100538618904621, 0.003064786828512609980, 0.003566159408300144298, 0.004568904567875151784, 0.005571649727450158837, 0.006073022307237618128, 0.006323708597131346906, 0.006574394887025075684, 0.006699738031971940941, 0.006762409604445303313, 0.006825081176918663950, 0.007075767466812139458, 0.007577140046599087006, 0.008078512626386038023, 0.008329198916279562104, 0.008579885206173084450 ),
 .UNSPECIFIED. ) ;
#30069 = CARTESIAN_POINT ( 'NONE',  ( -31.49356256989596758, 94.88921800892812541, 36.50000000000000000 ) ) ;
#30070 = ADVANCED_FACE ( 'NONE', ( #2410 ), #57579, .T. ) ;
#30071 = LINE ( 'NONE', #6278, #10917 ) ;
#30073 = CARTESIAN_POINT ( 'NONE',  ( 73.12133584826474930, 57.41764960941905116, -15.88333458976553381 ) ) ;
#30072 = FACE_OUTER_BOUND ( 'NONE', #76340, .T. ) ;
#30074 = ADVANCED_FACE ( 'NONE', ( #56584 ), #57076, .F. ) ;
#30075 = CARTESIAN_POINT ( 'NONE',  ( -58.21247931993242730, 56.66826942632778241, 59.99999999999999289 ) ) ;
#30076 = VERTEX_POINT ( 'NONE', #80440 ) ;
#30077 = B_SPLINE_CURVE_WITH_KNOTS ( 'NONE', 3,
 ( #95484, #73141, #10830, #41710 ),
 .UNSPECIFIED., .F., .F.,
 ( 4, 4 ),
 ( 0.01048155653827781073, 0.01885456469717847194 ),
 .UNSPECIFIED. ) ;
#30078 = PLANE ( 'NONE',  #1869 ) ;
#30079 = CARTESIAN_POINT ( 'NONE',  ( 151.8246416459486738, 268.5104669391655534, -14.87942003997596352 ) ) ;
#30080 = PLANE ( 'NONE',  #7871 ) ;
#30081 = CARTESIAN_POINT ( 'NONE',  ( 3.104905098483929482, 23.83396525600387506, -2.839279412974133887 ) ) ;
#30082 = ORIENTED_EDGE ( 'NONE', *, *, #42120, .T. ) ;
#30083 = FACE_OUTER_BOUND ( 'NONE', #77605, .T. ) ;
#30084 = CARTESIAN_POINT ( 'NONE',  ( -19.79397322353313271, 93.08167340080578356, 59.99999999999999289 ) ) ;
#30085 = VECTOR ( 'NONE', #97959, 1000.000000000000000 ) ;
#30086 = EDGE_CURVE ( 'NONE', #27367, #95983, #59310, .T. ) ;
#30087 = CARTESIAN_POINT ( 'NONE',  ( 71.49724145223210314, 72.36708001998830753, 1.062265253749112626 ) ) ;
#30088 = ADVANCED_FACE ( 'NONE', ( #96136 ), #11013, .T. ) ;
#30089 = DIRECTION ( 'NONE',  ( -0.8660254037844387076, -0.4999999999999998890, -0.000000000000000000 ) ) ;
#30090 = CARTESIAN_POINT ( 'NONE',  ( 204.2441997346916480, 270.1807567755661807, -7.723805382780020601 ) ) ;
#30091 = VECTOR ( 'NONE', #6751, 1000.000000000000000 ) ;
#30092 = DIRECTION ( 'NONE',  ( 0.4999999999999992784, -0.8660254037844390407, 0.000000000000000000 ) ) ;
#30093 = CARTESIAN_POINT ( 'NONE',  ( 68.70380343559517655, 69.96303083712633963, 3.047589648568798104 ) ) ;
#30094 = CARTESIAN_POINT ( 'NONE',  ( 152.8651171364917900, 265.8768457450651113, -16.25664868183201861 ) ) ;
#30095 = ORIENTED_EDGE ( 'NONE', *, *, #85133, .T. ) ;
#30096 = CARTESIAN_POINT ( 'NONE',  ( 190.7801068464975742, 281.0515339637562420, 16.66579443870669053 ) ) ;
#30097 = CARTESIAN_POINT ( 'NONE',  ( 15.58658660100807580, 11.12755873383624561, -6.180339887498949025 ) ) ;
#30098 = DIRECTION ( 'NONE',  ( -0.5000000000000014433, 0.8660254037844379305, -0.000000000000000000 ) ) ;
#30099 = EDGE_LOOP ( 'NONE', ( #35257, #85635, #21132, #78208 ) ) ;
#30100 = CARTESIAN_POINT ( 'NONE',  ( 149.7162292714551199, 271.3308795146458010, 12.12826134257344357 ) ) ;
#30101 = CARTESIAN_POINT ( 'NONE',  ( 200.3293654959697392, 273.7156512906800572, 13.98704503334941229 ) ) ;
#30102 = CARTESIAN_POINT ( 'NONE',  ( 80.60014811170655946, 45.61340808052423768, -11.68284267982980751 ) ) ;
#30103 = ORIENTED_EDGE ( 'NONE', *, *, #62630, .T. ) ;
#30104 = CARTESIAN_POINT ( 'NONE',  ( 191.5521510896938935, 298.8689373439769952, -9.847378829740700112 ) ) ;
#30105 = CARTESIAN_POINT ( 'NONE',  ( 79.28866853763614131, 59.92453731934288896, -16.49803216704724207 ) ) ;
#30106 = CARTESIAN_POINT ( 'NONE',  ( 204.5133713884061706, 276.4194452585140311, 14.87364779308245843 ) ) ;
#30107 = CARTESIAN_POINT ( 'NONE',  ( 69.44126986223525932, 62.66889528608714244, 13.25115268555880377 ) ) ;
#30108 = ORIENTED_EDGE ( 'NONE', *, *, #28815, .T. ) ;
#30109 = CARTESIAN_POINT ( 'NONE',  ( 96.08779704679574252, 226.2833772461660260, -9.188101187500095079 ) ) ;
#30110 = CARTESIAN_POINT ( 'NONE',  ( 203.1594176127779861, 278.7645619890024591, 16.51125172500342231 ) ) ;
#30111 = CARTESIAN_POINT ( 'NONE',  ( 178.0116618716515973, 269.0027435595893053, -16.91056692113554760 ) ) ;
#30112 = CARTESIAN_POINT ( 'NONE',  ( 81.77397856916392982, 42.34590070723890420, -7.979864230673365810 ) ) ;
#30113 = ORIENTED_EDGE ( 'NONE', *, *, #30036, .T. ) ;
#30114 = ORIENTED_EDGE ( 'NONE', *, *, #49674, .F. ) ;
#30115 = ORIENTED_EDGE ( 'NONE', *, *, #53722, .F. ) ;
#30116 = CARTESIAN_POINT ( 'NONE',  ( 81.96106570470071517, 53.04313638909700046, 15.32626709879401616 ) ) ;
#30117 = ORIENTED_EDGE ( 'NONE', *, *, #77542, .F. ) ;
#30118 = CARTESIAN_POINT ( 'NONE',  ( 70.05430382187989835, 70.68195646498267593, 3.459074501075599883 ) ) ;
#30119 = VERTEX_POINT ( 'NONE', #19117 ) ;
#30120 = CARTESIAN_POINT ( 'NONE',  ( 207.5570596878370679, 271.1476224814971374, 2.444960520848353358 ) ) ;
#30122 = EDGE_CURVE ( 'NONE', #69482, #35722, #34291, .T. ) ;
#30121 = CARTESIAN_POINT ( 'NONE',  ( -22.42236680055709641, 157.8615022471902591, 0.000000000000000000 ) ) ;
#30123 = CARTESIAN_POINT ( 'NONE',  ( -23.45395869395431632, 99.79046250668140772, 45.19943155085691444 ) ) ;
#30124 = CARTESIAN_POINT ( 'NONE',  ( 82.74279437798169567, 53.94163497425878262, -15.46549534628083400 ) ) ;
#30125 = CARTESIAN_POINT ( 'NONE',  ( 73.42314397212541621, 57.50016318312121655, -16.38349303661395950 ) ) ;
#30126 = CARTESIAN_POINT ( 'NONE',  ( 21.04482852044473162, 14.01110640527291906, 2.839279412974134775 ) ) ;
#30127 = AXIS2_PLACEMENT_3D ( 'NONE', #97464, #49843, #11378 ) ;
#30128 = FACE_OUTER_BOUND ( 'NONE', #59722, .T. ) ;
#30129 = CARTESIAN_POINT ( 'NONE',  ( 80.25249281668115486, 57.81819139295712517, 16.60223264289302847 ) ) ;
#30131 = ORIENTED_EDGE ( 'NONE', *, *, #35562, .F. ) ;
#30130 = CARTESIAN_POINT ( 'NONE',  ( -22.42236680055709641, 157.8615022471902591, 0.000000000000000000 ) ) ;
#30132 = CARTESIAN_POINT ( 'NONE',  ( 202.2603678735342214, 280.3217618159037556, 16.49712126737133744 ) ) ;
#30133 = CARTESIAN_POINT ( 'NONE',  ( 185.5178088754986732, 257.9886162347545451, 3.053422304497617645 ) ) ;
#30134 = CARTESIAN_POINT ( 'NONE',  ( 165.7096765433480243, 246.6079469402106668, -2.628825658309415836 ) ) ;
#30135 = VECTOR ( 'NONE', #505, 1000.000000000000114 ) ;
#30136 = CARTESIAN_POINT ( 'NONE',  ( 79.98071600351464383, 46.30330387653911828, -12.47010283063279878 ) ) ;
#30137 = CARTESIAN_POINT ( 'NONE',  ( 168.4964275335260879, 253.5783752955648822, 11.53270701355078742 ) ) ;
#30138 = CARTESIAN_POINT ( 'NONE',  ( 192.8389457671851801, 263.0020653644326103, -0.7569367516056485501 ) ) ;
#30139 = ORIENTED_EDGE ( 'NONE', *, *, #25276, .T. ) ;
#30140 = CARTESIAN_POINT ( 'NONE',  ( 181.6867268255581678, 270.7552855298207533, -16.03927706080179760 ) ) ;
#30141 = CARTESIAN_POINT ( 'NONE',  ( 75.01383350950912643, 67.34328350408775066, -12.89590634041037909 ) ) ;
#30142 = DIRECTION ( 'NONE',  ( 0.000000000000000000, 0.000000000000000000, -1.000000000000000000 ) ) ;
#30143 = CARTESIAN_POINT ( 'NONE',  ( 0.4370954166216904357, 184.3927522451419350, 2.944929066748280225E-16 ) ) ;
#30144 = EDGE_CURVE ( 'NONE', #67223, #50031, #248, .T. ) ;
#30145 = CARTESIAN_POINT ( 'NONE',  ( 193.1774878905343371, 266.9097302922900781, -11.44520343211384983 ) ) ;
#30146 = FACE_OUTER_BOUND ( 'NONE', #32259, .T. ) ;
#30147 = CARTESIAN_POINT ( 'NONE',  ( 203.5750579584898219, 278.0446517925538501, -15.66676355934540332 ) ) ;
#30148 = CARTESIAN_POINT ( 'NONE',  ( 25.96864935082043857, 154.0458036431183473, -22.49999999999983658 ) ) ;
#30149 = CARTESIAN_POINT ( 'NONE',  ( 72.45510692969175182, 70.78848362686431983, 7.675293421552848550 ) ) ;
#30151 = CARTESIAN_POINT ( 'NONE',  ( 4.599382176350318652, 161.9155109091896350, 2.679491924311254714 ) ) ;
#30150 = CARTESIAN_POINT ( 'NONE',  ( -9.729855525997876953, 171.3149278399160664, 9.188101187500093303 ) ) ;
#30152 = CARTESIAN_POINT ( 'NONE',  ( 188.9734557794317595, 297.2153733544514012, 9.139690452204975557 ) ) ;
#30153 = ORIENTED_EDGE ( 'NONE', *, *, #5832, .F. ) ;
#30154 = ORIENTED_EDGE ( 'NONE', *, *, #63678, .T. ) ;
#30155 = FACE_OUTER_BOUND ( 'NONE', #19019, .T. ) ;
#30156 = CARTESIAN_POINT ( 'NONE',  ( 161.5266078408477597, 251.3399204103630211, 13.01505764280997468 ) ) ;
#30157 = EDGE_CURVE ( 'NONE', #46058, #60977, #90909, .T. ) ;
#30158 = CARTESIAN_POINT ( 'NONE',  ( 200.1233510698300222, 282.0231834965481994, 17.42297826929840809 ) ) ;
#30159 = AXIS2_PLACEMENT_3D ( 'NONE', #84607, #15146, #46043 ) ;
#30160 = CARTESIAN_POINT ( 'NONE',  ( 85.52188629250015595, 42.69847903795108124, 1.431352116385852469 ) ) ;
#30161 = EDGE_CURVE ( 'NONE', #93933, #78755, #91509, .T. ) ;
#30162 = CARTESIAN_POINT ( 'NONE',  ( 162.7471009177916130, 248.7607477562823703, -10.22904224531126438 ) ) ;
#30163 = CARTESIAN_POINT ( 'NONE',  ( 68.22205435738101187, 65.90345407221148832, 10.80313017757570826 ) ) ;
#30164 = CARTESIAN_POINT ( 'NONE',  ( 152.5937463967839847, 278.0176957858930678, 3.715656952871561280 ) ) ;
#30165 = CARTESIAN_POINT ( 'NONE',  ( 13.97758990260114231, 185.0024278399160949, 9.188101187500095079 ) ) ;
#30166 = CARTESIAN_POINT ( 'NONE',  ( 125.2893514524760548, 233.9548013555409796, -4.594050593750042211 ) ) ;
#30167 = CYLINDRICAL_SURFACE ( 'NONE', #96890, 70.00000000000002842 ) ;
#30168 = LINE ( 'NONE', #22571, #78701 ) ;
#30169 = PLANE ( 'NONE',  #39941 ) ;
#30170 = CARTESIAN_POINT ( 'NONE',  ( 81.96547941067910870, 41.17040324926905015, 3.814626384468428721 ) ) ;
#30171 = CARTESIAN_POINT ( 'NONE',  ( 190.5526305594705434, 299.9695577504274979, -4.324655322867677398 ) ) ;
#30172 = CARTESIAN_POINT ( 'NONE',  ( 157.2333142128019858, 258.3109064714224132, 16.87956768598436597 ) ) ;
#30173 = CARTESIAN_POINT ( 'NONE',  ( 193.7118145980225279, 295.1282904202991517, 14.61271143546694162 ) ) ;
#30174 = CARTESIAN_POINT ( 'NONE',  ( 161.6755750489535046, 250.6166850027345276, -13.01404233079112061 ) ) ;
#30175 = CARTESIAN_POINT ( 'NONE',  ( 189.8944967759784390, 284.6695464243575771, 16.74947250714170011 ) ) ;
#30176 = CARTESIAN_POINT ( 'NONE',  ( 167.7287949414774744, 278.2917028285691003, 14.65232981943655588 ) ) ;
#30177 = CARTESIAN_POINT ( 'NONE',  ( 189.8280524984248530, 300.0247317190094236, -0.5815489268893287989 ) ) ;
#30178 = CARTESIAN_POINT ( 'NONE',  ( 70.92518752925752779, 71.21820892678006487, 3.335809568748416165 ) ) ;
#30179 = LINE ( 'NONE', #89189, #3183 ) ;
#30180 = CARTESIAN_POINT ( 'NONE',  ( 184.4418290349794347, 268.6877477094485585, -15.38013229235870583 ) ) ;
#30181 = VERTEX_POINT ( 'NONE', #45363 ) ;
#30182 = DIRECTION ( 'NONE',  ( -0.5104483989331149996, -0.8599083858334093389, 0.000000000000000000 ) ) ;
#30183 = ADVANCED_FACE ( 'NONE', ( #76296 ), #30169, .T. ) ;
#30184 = CARTESIAN_POINT ( 'NONE',  ( 163.7012083107868534, 247.1081852757374975, -6.544933039329257518 ) ) ;
#30185 = CARTESIAN_POINT ( 'NONE',  ( 185.1206366404793471, 269.5993361517367362, 15.81333004430259948 ) ) ;
#30186 = CARTESIAN_POINT ( 'NONE',  ( 99.98491136382573075, 228.5333772461660828, 9.188101187500095079 ) ) ;
#30187 = CARTESIAN_POINT ( 'NONE',  ( 9.185703322462060783, 20.70171378149917629, -9.188101187500004485 ) ) ;
#30188 = CARTESIAN_POINT ( 'NONE',  ( 191.4044787581200069, 299.1247133251352466, 7.435199718141230818 ) ) ;
#30189 = CARTESIAN_POINT ( 'NONE',  ( 177.1347673595945764, 262.9921672455169528, 15.53478677465993485 ) ) ;
#30191 = CARTESIAN_POINT ( 'NONE',  ( 103.4219496833212162, 240.5177522451419350, 5.000000000000046185 ) ) ;
#30190 = FACE_OUTER_BOUND ( 'NONE', #95625, .T. ) ;
#30192 = B_SPLINE_CURVE_WITH_KNOTS ( 'NONE', 3,
 ( #80162, #19350, #11730, #34432 ),
 .UNSPECIFIED., .F., .F.,
 ( 4, 4 ),
 ( 0.009240307309658310833, 0.01507866790100597862 ),
 .UNSPECIFIED. ) ;
#30193 = CARTESIAN_POINT ( 'NONE',  ( 201.7550856928311589, 271.1410374022044607, -9.839847481188424894 ) ) ;
#30194 = CARTESIAN_POINT ( 'NONE',  ( 198.5970767652345899, 286.6667681383942181, -17.17073100918929640 ) ) ;
#30195 = DIRECTION ( 'NONE',  ( -0.8660254037844387076, -0.4999999999999998890, -0.000000000000000000 ) ) ;
#30196 = CARTESIAN_POINT ( 'NONE',  ( 39.01788588657935719, 31.03085787977765975, 9.188101187500006262 ) ) ;
#30197 = CYLINDRICAL_SURFACE ( 'NONE', #96866, 70.00000000000002842 ) ;
#30198 = CARTESIAN_POINT ( 'NONE',  ( 4.767222435543962078, 166.8927522451418213, 10.00000000000009948 ) ) ;
#30199 = ORIENTED_EDGE ( 'NONE', *, *, #94964, .T. ) ;
#30200 = CARTESIAN_POINT ( 'NONE',  ( 24.61059131263772670, 35.18502408145592852, 5.678558825948277544 ) ) ;
#30201 = CARTESIAN_POINT ( 'NONE',  ( 178.5316424161641748, 280.3506190370360400, 15.79244575417478735 ) ) ;
#30202 = VECTOR ( 'NONE', #3482, 1000.000000000000000 ) ;
#30203 = CARTESIAN_POINT ( 'NONE',  ( 147.5749398328735822, 275.0397016159798227, -4.620786157167191099 ) ) ;
#30204 = CARTESIAN_POINT ( 'NONE',  ( 149.1486417047969155, 272.3139700178423368, -11.47583619705022606 ) ) ;
#30205 = EDGE_CURVE ( 'NONE', #45578, #34461, #53703, .T. ) ;
#30206 = ORIENTED_EDGE ( 'NONE', *, *, #62312, .F. ) ;
#30207 = B_SPLINE_SURFACE_WITH_KNOTS ( 'NONE', 3, 1, ( 
 ( #32006, #77644 ),
 ( #7214, #8228 ),
 ( #39097, #24424 ),
 ( #41101, #87304 ),
 ( #2135, #17837 ),
 ( #79169, #24916 ),
 ( #3638, #25416 ),
 ( #41608, #79670 ),
 ( #57312, #72551 ),
 ( #88785, #56815 ),
 ( #34041, #19355 ),
 ( #18835, #56308 ),
 ( #2640, #55790 ),
 ( #72037, #73532 ),
 ( #49233, #26432 ),
 ( #11248, #32529 ),
 ( #63423, #9748 ),
 ( #48737, #18339 ),
 ( #94362, #10232 ),
 ( #95875, #86783 ),
 ( #33528, #64930 ),
 ( #87797, #50216 ),
 ( #49716, #94856 ),
 ( #34519, #64424 ),
 ( #3156, #63917 ),
 ( #88282, #80167 ),
 ( #81170, #11734 ),
 ( #80671, #17317 ),
 ( #95387, #42598 ),
 ( #25939, #10734 ),
 ( #42111, #73045 ) ),
 .UNSPECIFIED., .F., .F., .F.,
 ( 4, 3, 3, 3, 3, 3, 3, 3, 3, 3, 4 ),
 ( 2, 2 ),
 ( 0.000000000000000000, 0.1333490885032447282, 0.3007194338854389248, 0.4699862290245251373, 0.5844252810809574816, 0.6686540514502947730, 0.7354980260655736846, 0.8028463152565851191, 0.8633854507757401375, 0.9437142632667373521, 1.000000000000000000 ),
 ( 0.000000000000000000, 1.000000000000000000 ),
 .UNSPECIFIED. ) ;
#30208 = AXIS2_PLACEMENT_3D ( 'NONE', #12575, #45438, #43452 ) ;
#30209 = CARTESIAN_POINT ( 'NONE',  ( 84.76617582037141574, 50.00026310130547813, -13.66906362199170921 ) ) ;
#30210 = LINE ( 'NONE', #76805, #43928 ) ;
#30211 = CARTESIAN_POINT ( 'NONE',  ( 182.9169972424188586, 263.6770152411878598, -13.86124712002487236 ) ) ;
#30212 = CARTESIAN_POINT ( 'NONE',  ( 169.9766547505107894, 252.5201543592683322, -8.760183188246276842 ) ) ;
#30213 = CARTESIAN_POINT ( 'NONE',  ( 171.0458462729697260, 282.1216204770890386, -14.11865471209823930 ) ) ;
#30214 = EDGE_LOOP ( 'NONE', ( #80498, #37205, #85482 ) ) ;
#30215 = CARTESIAN_POINT ( 'NONE',  ( 73.30631488696991482, 69.89686749726290316, 9.630897265116471928 ) ) ;
#30216 = CARTESIAN_POINT ( 'NONE',  ( 38.36533659613348846, 24.01110640527295104, 2.839279412974134775 ) ) ;
#30217 = VERTEX_POINT ( 'NONE', #8374 ) ;
#30218 = CARTESIAN_POINT ( 'NONE',  ( 168.1909178643507232, 248.9330331115285162, 6.596560970029747395 ) ) ;
#30219 = CARTESIAN_POINT ( 'NONE',  ( 182.3561040761404968, 291.0252386590130413, -10.82420555737414247 ) ) ;
#30220 = ORIENTED_EDGE ( 'NONE', *, *, #58439, .T. ) ;
#30221 = DIRECTION ( 'NONE',  ( -0.3940053768033626169, 0.6824373310787468228, 0.6156614753256509642 ) ) ;
#30222 = CARTESIAN_POINT ( 'NONE',  ( 33.63888670793727442, 47.67824751478842416, 177.5919119679930134 ) ) ;
#30223 = CARTESIAN_POINT ( 'NONE',  ( 190.8872452503548232, 277.9998427814335855, -17.37787329346898346 ) ) ;
#30224 = CARTESIAN_POINT ( 'NONE',  ( 192.7446300355631479, 296.8035032227751913, -13.50572488576995411 ) ) ;
#30225 = CARTESIAN_POINT ( 'NONE',  ( 152.7691010214056462, 266.0431505347400503, -16.40662330462167162 ) ) ;
#30226 = EDGE_CURVE ( 'NONE', #29132, #50553, #39238, .T. ) ;
#30227 = DIRECTION ( 'NONE',  ( -0.000000000000000000, 0.000000000000000000, -1.000000000000000000 ) ) ;
#30228 = CIRCLE ( 'NONE', #48001, 70.00000000000001421 ) ;
#30229 = CARTESIAN_POINT ( 'NONE',  ( 34.13026518906141860, 41.74646525600392977, 2.839279412974139660 ) ) ;
#30230 = VECTOR ( 'NONE', #54668, 1000.000000000000000 ) ;
#30231 = CARTESIAN_POINT ( 'NONE',  ( 73.60933432321982650, 55.64367109616565443, 16.10230547196763595 ) ) ;
#30232 = CARTESIAN_POINT ( 'NONE',  ( -32.86949478547433046, 94.43171332246730287, 43.89948692389422291 ) ) ;
#30233 = ORIENTED_EDGE ( 'NONE', *, *, #69475, .T. ) ;
#30234 = CARTESIAN_POINT ( 'NONE',  ( 175.3460070743044810, 258.5034201212096718, 13.02170940230438667 ) ) ;
#30235 = VECTOR ( 'NONE', #9164, 1000.000000000000114 ) ;
#30236 = VERTEX_POINT ( 'NONE', #1275 ) ;
#30237 = ORIENTED_EDGE ( 'NONE', *, *, #12607, .T. ) ;
#30238 = CARTESIAN_POINT ( 'NONE',  ( 72.13293662478744750, 72.32175006689249130, -1.141440976623812942 ) ) ;
#30239 = CARTESIAN_POINT ( 'NONE',  ( 86.81641918289878390, 45.77657501471897916, -8.750901752256119437 ) ) ;
#30241 = CARTESIAN_POINT ( 'NONE',  ( 190.6324986747941068, 299.9733286590040962, -4.183702684017944762 ) ) ;
#30240 = CARTESIAN_POINT ( 'NONE',  ( 174.4482263059820468, 257.3207558651999989, -11.99955440495903858 ) ) ;
#30242 = CARTESIAN_POINT ( 'NONE',  ( 165.0424088038023456, 244.7851578786982145, -1.332161216135762105 ) ) ;
#30243 = CARTESIAN_POINT ( 'NONE',  ( 197.5277397434883255, 272.9434654477590243, -13.23775816460648080 ) ) ;
#30244 = CARTESIAN_POINT ( 'NONE',  ( 77.29684513673267077, 59.91861738668672643, -15.97104762766038810 ) ) ;
#30245 = CARTESIAN_POINT ( 'NONE',  ( 147.9748066657072627, 274.3471119452502762, 9.387104374042873900 ) ) ;
#30246 = CARTESIAN_POINT ( 'NONE',  ( 171.6332223966747392, 250.6993909615997609, -5.719266321659834063 ) ) ;
#30247 = CARTESIAN_POINT ( 'NONE',  ( 165.8055607888911709, 266.0341751366186713, 17.30635120499955804 ) ) ;
#30248 = CARTESIAN_POINT ( 'NONE',  ( 185.1069551167274199, 285.7384112475837696, -15.13345330922732401 ) ) ;
#30249 = CARTESIAN_POINT ( 'NONE',  ( 113.4086522182495145, 224.0327760586659451, 1.948934522072303157E-15 ) ) ;
#30250 = ORIENTED_EDGE ( 'NONE', *, *, #75038, .T. ) ;
#30251 = DIRECTION ( 'NONE',  ( -1.000000000000000000, -4.892646582057367384E-14, 0.000000000000000000 ) ) ;
#30252 = CARTESIAN_POINT ( 'NONE',  ( 160.9978133751494624, 283.8066770274658666, 2.192527523246561749 ) ) ;
#30253 = CARTESIAN_POINT ( 'NONE',  ( 187.9688059934449313, 273.8547072571687409, 16.05218478527549308 ) ) ;
#30254 = ORIENTED_EDGE ( 'NONE', *, *, #9254, .F. ) ;
#30255 = CARTESIAN_POINT ( 'NONE',  ( 74.00349760290353629, 68.31608301643910863, -11.67389511724663009 ) ) ;
#30256 = CARTESIAN_POINT ( 'NONE',  ( 180.1453383632374994, 295.1715722599841456, -2.140036363759055149 ) ) ;
#30257 = CARTESIAN_POINT ( 'NONE',  ( 196.0727848089514964, 291.0389700598140621, 17.56388901715066808 ) ) ;
#30258 = CARTESIAN_POINT ( 'NONE',  ( 159.3995226465659982, 254.5589234043588078, -16.81133486613867234 ) ) ;
#30259 = CARTESIAN_POINT ( 'NONE',  ( 16.38795500122288473, 25.16454794089041158, -10.00000000000000355 ) ) ;
#30260 = ORIENTED_EDGE ( 'NONE', *, *, #43573, .T. ) ;
#30261 = CARTESIAN_POINT ( 'NONE',  ( 194.7222134385861807, 293.3782282925342884, 16.03497216414424997 ) ) ;
#30262 = VERTEX_POINT ( 'NONE', #760 ) ;
#30263 = CARTESIAN_POINT ( 'NONE',  ( 45.80758703142363686, 72.03864405183792030, -10.00000000000000000 ) ) ;
#30264 = ORIENTED_EDGE ( 'NONE', *, *, #79664, .T. ) ;
#30265 = CARTESIAN_POINT ( 'NONE',  ( 191.7763301340909265, 267.4862631225445853, -12.60863414139059735 ) ) ;
#30266 = B_SPLINE_CURVE_WITH_KNOTS ( 'NONE', 3,
 ( #44091, #74034, #98331, #50217, #21319, #81171, #27434, #89763, #43092, #36003, #75035, #11736, #27912, #58308, #5612, #42600, #13714, #4624, #20837, #4115, #51729, #75524, #89285, #36504, #81658, #59798, #82168, #67407, #66908, #44589 ),
 .UNSPECIFIED., .F., .F.,
 ( 4, 2, 2, 2, 2, 2, 2, 2, 2, 2, 2, 2, 2, 2, 4 ),
 ( 0.001616355120345336219, 0.002274024124150745597, 0.002931693127956154325, 0.004247031135566920607, 0.004904700139372303314, 0.005233534641275029362, 0.005397951892226427080, 0.005439056204964282798, 0.005480160517702137649, 0.005521264830439992499, 0.005562369143177847350, 0.005726786394129246803, 0.005891203645080646256, 0.006220038146983454704, 0.006877707150789046445 ),
 .UNSPECIFIED. ) ;
#30267 = CARTESIAN_POINT ( 'NONE',  ( 193.6139411566157378, 262.7946681891672256, 4.750614067181518685 ) ) ;
#30268 = CARTESIAN_POINT ( 'NONE',  ( -11.32641631811692662, 174.2677522451419350, -5.000000000000047962 ) ) ;
#30269 = CARTESIAN_POINT ( 'NONE',  ( 202.8211298556536804, 279.3504935719197988, 17.07914446815911447 ) ) ;
#30271 = CARTESIAN_POINT ( 'NONE',  ( 69.80192404618573221, 63.14541187278000223, -13.66695019165900149 ) ) ;
#30270 = CARTESIAN_POINT ( 'NONE',  ( 184.3160629641438106, 288.6786004691003882, -13.34280541894466765 ) ) ;
#30272 = CARTESIAN_POINT ( 'NONE',  ( -44.74834796241764678, 29.05375577536863929, -10.00000000000000000 ) ) ;
#30273 = ORIENTED_EDGE ( 'NONE', *, *, #99722, .F. ) ;
#30275 = CARTESIAN_POINT ( 'NONE',  ( 147.5813496936708020, 275.0285994114094592, 4.516581957185684004 ) ) ;
#30274 = CIRCLE ( 'NONE', #54546, 1.449999999999993072 ) ;
#30276 = CARTESIAN_POINT ( 'NONE',  ( -13.11024591527723615, 27.99999999999999645, -32.50000000000017053 ) ) ;
#30277 = CARTESIAN_POINT ( 'NONE',  ( 189.7845653727764272, 264.2201878795776224, -9.220148691588715195 ) ) ;
#30278 = CARTESIAN_POINT ( 'NONE',  ( 192.9083073729183582, 270.9347064964478022, 14.76982790152045055 ) ) ;
#30279 = CARTESIAN_POINT ( 'NONE',  ( 192.3260883533780259, 271.6660879014408465, -14.49459676434517164 ) ) ;
#30280 = EDGE_CURVE ( 'NONE', #27141, #23710, #47974, .T. ) ;
#30281 = DIRECTION ( 'NONE',  ( 0.8660254037844375974, 0.5000000000000017764, 3.252519625699413953E-16 ) ) ;
#30282 = DIRECTION ( 'NONE',  ( -1.000000000000000000, 0.000000000000000000, 0.000000000000000000 ) ) ;
#30283 = ADVANCED_FACE ( 'NONE', ( #16954 ), #53459, .T. ) ;
#30284 = DIRECTION ( 'NONE',  ( -3.817860598523670672E-18, -1.090355031989287297E-16, -1.000000000000000000 ) ) ;
#30285 = CIRCLE ( 'NONE', #7636, 70.00000000000001421 ) ;
#30286 = CARTESIAN_POINT ( 'NONE',  ( 155.6435836392643637, 261.0644005951349982, 17.58841156286628049 ) ) ;
#30287 = CARTESIAN_POINT ( 'NONE',  ( 32.20940242151128530, 182.7365022471902876, 10.00000000000009948 ) ) ;
#30288 = CARTESIAN_POINT ( 'NONE',  ( 82.64074333392795779, 53.51963485226765016, -15.73164264726942285 ) ) ;
#30289 = ADVANCED_FACE ( 'NONE', ( #47845 ), #38245, .T. ) ;
#30290 = CARTESIAN_POINT ( 'NONE',  ( 77.41429782557628414, 209.3768266524159571, -9.188101187500091527 ) ) ;
#30291 = CARTESIAN_POINT ( 'NONE',  ( 206.1798448551755598, 273.5330285446045195, -10.53862763475382813 ) ) ;
#30292 = CARTESIAN_POINT ( 'NONE',  ( 192.5284579606305613, 297.1779242397361713, -13.15228012403107272 ) ) ;
#30293 = CARTESIAN_POINT ( 'NONE',  ( 207.8446715390582540, 270.6494641423232679, -2.429516028743652800 ) ) ;
#30294 = EDGE_CURVE ( 'NONE', #90439, #57797, #14780, .T. ) ;
#30295 = CARTESIAN_POINT ( 'NONE',  ( 196.2506489124965299, 288.9087261997057112, -17.23880585552221234 ) ) ;
#30296 = CARTESIAN_POINT ( 'NONE',  ( 161.3773209892555371, 251.1332761876949746, -14.50043705923759241 ) ) ;
#30297 = DIRECTION ( 'NONE',  ( -0.3535533905932676246, 0.6123724356957830350, 0.7071067811865604513 ) ) ;
#30298 = AXIS2_PLACEMENT_3D ( 'NONE', #95381, #73524, #56806 ) ;
#30299 = B_SPLINE_CURVE_WITH_KNOTS ( 'NONE', 3,
 ( #54125, #47048, #8557, #85087 ),
 .UNSPECIFIED., .F., .F.,
 ( 4, 4 ),
 ( 0.04103871331059693456, 0.04887120950165270428 ),
 .UNSPECIFIED. ) ;
#30301 = CARTESIAN_POINT ( 'NONE',  ( 76.58496548142363736, 51.27307132485643137, 16.05712343730097658 ) ) ;
#30300 = CARTESIAN_POINT ( 'NONE',  ( 73.72691027005377862, 69.52791761355244660, -9.770281360779824453 ) ) ;
#30302 = CARTESIAN_POINT ( 'NONE',  ( 33.92686603480522223, 41.36126292948897998, 6.180339887498949913 ) ) ;
#30303 = CARTESIAN_POINT ( 'NONE',  ( 205.4651907542742890, 274.7708457572024940, -12.42986464854210027 ) ) ;
#30305 = CARTESIAN_POINT ( 'NONE',  ( 195.6974783896144174, 291.6890198465123945, 16.70600479393688431 ) ) ;
#30304 = B_SPLINE_CURVE_WITH_KNOTS ( 'NONE', 3,
 ( #60462, #84326, #93419, #21980, #37665, #52874, #91927, #83825, #45275, #68575, #38154, #69072, #30582, #92418, #22968, #53855, #46252, #77176, #78697, #39649, #9284, #16873, #10789, #32064, #33587, #26489, #72096, #80221, #63479, #56370, #17897, #1699, #2696, #18897, #71600, #40159, #71100, #86841, #57366, #86336, #17376, #88340, #55358, #32582, #24477, #34095, #94416, #24969 ),
 .UNSPECIFIED., .F., .F.,
 ( 4, 2, 2, 2, 2, 2, 2, 2, 2, 2, 2, 2, 2, 2, 2, 2, 2, 2, 2, 2, 2, 2, 2, 4 ),
 ( 0.002501527887315633213, 0.002918846236623728971, 0.003127505411277738470, 0.003231834998604704405, 0.003336164585931669906, 0.003440494173258635408, 0.003544823760585601342, 0.003753482935239675460, 0.004170801284547748233, 0.005005437983164006538, 0.005840074681780264843, 0.006674711380396523147, 0.007092029729704573369, 0.007509348079012624459, 0.007613677666339734376, 0.007665842460003294105, 0.007718007253666853834, 0.007770172047330414430, 0.007822336840993975027, 0.007926666428321096219, 0.008135325602975338605, 0.008343984777629584459, 0.008761303126938145558, 0.009178621476246706656 ),
 .UNSPECIFIED. ) ;
#30306 = CARTESIAN_POINT ( 'NONE',  ( 71.88653196722606253, 72.25570330380722339, 3.269911192557288793 ) ) ;
#30307 = CARTESIAN_POINT ( 'NONE',  ( 27.59033994439653270, 195.9244531367911293, -4.594050593750046652 ) ) ;
#30308 = VECTOR ( 'NONE', #47384, 1000.000000000000000 ) ;
#30309 = CARTESIAN_POINT ( 'NONE',  ( 60.22919299317007358, 196.3923013555409796, 4.594050593750050204 ) ) ;
#30310 = LINE ( 'NONE', #97735, #32086 ) ;
#30311 = CARTESIAN_POINT ( 'NONE',  ( 199.4509464742678801, 277.6162209133078704, 15.23248329428225389 ) ) ;
#30312 = CARTESIAN_POINT ( 'NONE',  ( 79.92971505533115817, 50.62409585498646436, -14.80966530455547847 ) ) ;
#30313 = CARTESIAN_POINT ( 'NONE',  ( -13.68994397906405602, 176.2365022471903444, 2.944929066748280225E-16 ) ) ;
#30314 = CARTESIAN_POINT ( 'NONE',  ( 50.64826632015721231, 209.2369531367911293, -4.594050593750048428 ) ) ;
#30315 = B_SPLINE_CURVE_WITH_KNOTS ( 'NONE', 3,
 ( #11437, #81353, #41795, #2836, #42290, #42780, #95570, #35702, #18024, #73714, #97052, #27620, #10417, #81843, #43286, #74232, #4818, #66601, #58969, #45284, #45770, #90454, #75215, #28591, #89941, #30093, #52390, #59977, #74730, #29599, #6298, #12927, #67591, #60471, #82358, #22492, #98521, #76692, #21023, #75713, #14880, #36682, #37189, #59473, #53384, #84334 ),
 .UNSPECIFIED., .F., .F.,
 ( 4, 1, 2, 2, 1, 2, 2, 1, 1, 2, 2, 1, 1, 2, 2, 1, 1, 2, 2, 1, 1, 1, 2, 2, 1, 1, 1, 2, 2, 4 ),
 ( 0.000000000000000000, 0.06250000000000309475, 0.09375000000000353884, 0.1250000000000039968, 0.1875000000000036637, 0.2187500000000034972, 0.2500000000000033307, 0.3125000000000037192, 0.3437500000000049960, 0.3593750000000063838, 0.3750000000000077161, 0.4375000000000158207, 0.4687500000000199285, 0.4843750000000218159, 0.5000000000000236478, 0.5625000000000337508, 0.5937500000000368594, 0.6093750000000365263, 0.6250000000000361933, 0.6875000000000408562, 0.7187500000000411893, 0.7343750000000422995, 0.7421875000000427436, 0.7500000000000434097, 0.8125000000000350830, 0.8437500000000320854, 0.8593750000000306422, 0.8671875000000300870, 0.8750000000000294209, 1.000000000000000000 ),
 .UNSPECIFIED. ) ;
#30316 = CARTESIAN_POINT ( 'NONE',  ( 17.24455747906367264, 28.14336893147755347, 7.433330006724141015 ) ) ;
#30317 = CARTESIAN_POINT ( 'NONE',  ( -14.62813816649718213, 172.3615022471903160, 5.000000000000046185 ) ) ;
#30318 = CARTESIAN_POINT ( 'NONE',  ( -7.699934936221591641, 156.3615022471902023, 5.000000000000051514 ) ) ;
#30319 = CARTESIAN_POINT ( 'NONE',  ( 6.194340351808173217, 26.68290643055185285, 3.479690158560446702E-15 ) ) ;
#30320 = CARTESIAN_POINT ( 'NONE',  ( 205.2391015854675516, 275.1624436846170738, -14.01434138479280911 ) ) ;
#30321 = CARTESIAN_POINT ( 'NONE',  ( 158.9583395483327308, 256.9617481484739869, -16.95571191692422275 ) ) ;
#30322 = CARTESIAN_POINT ( 'NONE',  ( 175.6268470825654049, 291.0373744556468409, 2.379281674685343351 ) ) ;
#30323 = CARTESIAN_POINT ( 'NONE',  ( 159.6898930778639283, 254.0559870643349143, 16.90891900388599822 ) ) ;
#30324 = CARTESIAN_POINT ( 'NONE',  ( 72.42236640908883771, 60.72463564107695788, 14.97540514082750640 ) ) ;
#30325 = CARTESIAN_POINT ( 'NONE',  ( 201.3244920114063063, 281.9427463586865201, 17.21113171619803595 ) ) ;
#30326 = CARTESIAN_POINT ( 'NONE',  ( -19.15453390681661716, 24.31945705462846163, -10.00000000000000000 ) ) ;
#30327 = CARTESIAN_POINT ( 'NONE',  ( 114.8426596992764388, 237.1115022471902307, 10.00000000000009592 ) ) ;
#30328 = LINE ( 'NONE', #60701, #23136 ) ;
#30329 = FACE_OUTER_BOUND ( 'NONE', #32865, .T. ) ;
#30330 = VERTEX_POINT ( 'NONE', #26078 ) ;
#30331 = CARTESIAN_POINT ( 'NONE',  ( 77.01122693365802263, 49.58419032010621663, 15.00892541147910286 ) ) ;
#30332 = VERTEX_POINT ( 'NONE', #50358 ) ;
#30333 = CARTESIAN_POINT ( 'NONE',  ( 206.3423291502491566, 273.2515974901050413, -10.76717883871977577 ) ) ;
#30334 = CARTESIAN_POINT ( 'NONE',  ( 190.0974356945988575, 279.3567963776670240, -17.44568797921136039 ) ) ;
#30335 = CARTESIAN_POINT ( 'NONE',  ( 189.5255948787495015, 270.7606473226053367, 15.83079519377715627 ) ) ;
#30336 = ORIENTED_EDGE ( 'NONE', *, *, #40477, .F. ) ;
#30337 = DIRECTION ( 'NONE',  ( -0.8660254037844387076, -0.4999999999999998890, -0.000000000000000000 ) ) ;
#30338 = CARTESIAN_POINT ( 'NONE',  ( 164.9779129355220562, 244.8968679994381148, -1.771286574179712803 ) ) ;
#30339 = CARTESIAN_POINT ( 'NONE',  ( 147.6264044922760377, 274.9505622111005323, -8.841872555777701592 ) ) ;
#30340 = CARTESIAN_POINT ( 'NONE',  ( 73.10133336124690118, 70.55037490275843481, -7.932148607956638564 ) ) ;
#30341 = CYLINDRICAL_SURFACE ( 'NONE', #76458, 17.82106496071139645 ) ;
#30343 = EDGE_CURVE ( 'NONE', #27875, #91598, #22068, .T. ) ;
#30342 = VECTOR ( 'NONE', #50444, 1000.000000000000000 ) ;
#30344 = EDGE_LOOP ( 'NONE', ( #73433, #57511, #89949 ) ) ;
#30345 = VECTOR ( 'NONE', #28103, 1000.000000000000114 ) ;
#30346 = CARTESIAN_POINT ( 'NONE',  ( 17.52119783388728180, 25.51421378149919050, -9.188101187500004485 ) ) ;
#30347 = CARTESIAN_POINT ( 'NONE',  ( 75.84489191139213915, 59.04817673520474131, 15.93577818499344545 ) ) ;
#30348 = CARTESIAN_POINT ( 'NONE',  ( 67.11274794702013935, 69.23909389306264472, -1.736299782362168642 ) ) ;
#30349 = CARTESIAN_POINT ( 'NONE',  ( -22.42236680055709641, 157.8615022471902591, 0.000000000000000000 ) ) ;
#30350 = ORIENTED_EDGE ( 'NONE', *, *, #77873, .T. ) ;
#30351 = CARTESIAN_POINT ( 'NONE',  ( -22.23917875008777756, 35.17836123037032792, 59.99999999999999289 ) ) ;
#30352 = CARTESIAN_POINT ( 'NONE',  ( -6.130263895410251962, 167.2677522451418781, 10.00000000000009592 ) ) ;
#30353 = VERTEX_POINT ( 'NONE', #11397 ) ;
#30354 = CARTESIAN_POINT ( 'NONE',  ( 174.8261646120922421, 286.1039399097584806, 11.04222616188278749 ) ) ;
#30355 =( BOUNDED_CURVE ( )  B_SPLINE_CURVE ( 2, ( #18244, #532, #24823, #39500, #16231, #93263, #54710, #78044, #95289, #33433, #94762, #64330, #56211 ),
 .UNSPECIFIED., .F., .T. ) 
 B_SPLINE_CURVE_WITH_KNOTS ( ( 3, 2, 2, 2, 2, 2, 3 ),
 ( 0.5625000000000000000, 0.5649999999999999467, 0.5699999999999999512, 0.5749999999999999556, 0.5799999999999999600, 0.5849999999999999645, 0.5875000000000000222 ),
 .UNSPECIFIED. ) 
 CURVE ( )  GEOMETRIC_REPRESENTATION_ITEM ( )  RATIONAL_B_SPLINE_CURVE ( ( 0.9755282581475768211, 0.9755282581475768211, 1.000000000000000000, 0.9510565162951535312, 1.000000000000000000, 0.9510565162951535312, 1.000000000000000000, 0.9510565162951535312, 1.000000000000000000, 0.9510565162951535312, 1.000000000000000000, 0.9755282581475761550, 0.9755282581475767101 ) ) 
 REPRESENTATION_ITEM ( '' )  );
#30357 = CARTESIAN_POINT ( 'NONE',  ( 67.87119603988516303, 66.02582195971199042, -10.46564531199834924 ) ) ;
#30356 = CARTESIAN_POINT ( 'NONE',  ( 160.1224120645151174, 282.3532393352595591, -3.187131287737694052 ) ) ;
#30358 = CARTESIAN_POINT ( 'NONE',  ( 163.2742264920156572, 247.8477394797576778, -9.850275379362519956 ) ) ;
#30359 = CARTESIAN_POINT ( 'NONE',  ( 204.2457645315488719, 276.8829539310449945, 14.53406579917280261 ) ) ;
#30360 = CARTESIAN_POINT ( 'NONE',  ( 188.7060284211345618, 295.2753450948700902, -11.24849810963761776 ) ) ;
#30361 = CARTESIAN_POINT ( 'NONE',  ( 204.0604753336787667, 271.4817813032398703, 9.862283393711939183 ) ) ;
#30362 = EDGE_CURVE ( 'NONE', #29851, #77944, #99307, .T. ) ;
#30363 = CARTESIAN_POINT ( 'NONE',  ( 137.1160976468485728, 237.7202760586660020, -5.415160957724236172E-17 ) ) ;
#30364 = CARTESIAN_POINT ( 'NONE',  ( 160.1889510292459704, 254.1022327335691955, -15.33409651099172777 ) ) ;
#30365 = AXIS2_PLACEMENT_3D ( 'NONE', #21161, #35339, #89596 ) ;
#30366 = CARTESIAN_POINT ( 'NONE',  ( 181.9407744531946491, 260.3728692333327785, 9.471612455673151132 ) ) ;
#30367 = CARTESIAN_POINT ( 'NONE',  ( 71.43287601098374751, 221.2369531367911293, -4.594050593750048428 ) ) ;
#30368 = ORIENTED_EDGE ( 'NONE', *, *, #98725, .T. ) ;
#30369 = FACE_OUTER_BOUND ( 'NONE', #13666, .T. ) ;
#30370 = DIRECTION ( 'NONE',  ( 1.000000000000000000, 0.000000000000000000, 0.000000000000000000 ) ) ;
#30371 = ORIENTED_EDGE ( 'NONE', *, *, #13923, .F. ) ;
#30372 = CARTESIAN_POINT ( 'NONE',  ( 167.2515702596184042, 262.0622343731731689, -17.21809106051008342 ) ) ;
#30373 = ORIENTED_EDGE ( 'NONE', *, *, #69795, .T. ) ;
#30374 = ORIENTED_EDGE ( 'NONE', *, *, #31964, .T. ) ;
#30375 = LINE ( 'NONE', #92228, #68159 ) ;
#30376 = CARTESIAN_POINT ( 'NONE',  ( 67.03472654747955062, 67.61602409160271066, 6.661883959231219343 ) ) ;
#30377 = DIRECTION ( 'NONE',  ( 0.8660254037844339337, 0.5000000000000081046, -0.000000000000000000 ) ) ;
#30378 = CARTESIAN_POINT ( 'NONE',  ( 146.9456733906991417, 276.1296230653242105, -0.7988785540157754550 ) ) ;
#30379 = CARTESIAN_POINT ( 'NONE',  ( 81.19301662773271744, 55.65398007790845014, 16.37810844063417548 ) ) ;
#30380 = CARTESIAN_POINT ( 'NONE',  ( 155.4216552449402684, 261.4487918497463284, 18.51722274565528892 ) ) ;
#30381 = CARTESIAN_POINT ( 'NONE',  ( 79.84079962965540744, 210.2365022471901739, -10.00000000000009237 ) ) ;
#30382 = ORIENTED_EDGE ( 'NONE', *, *, #49755, .T. ) ;
#30383 = AXIS2_PLACEMENT_3D ( 'NONE', #45983, #76430, #76899 ) ;
#30384 = CARTESIAN_POINT ( 'NONE',  ( 161.9818314276490128, 250.0862333946917602, -13.01265917937909045 ) ) ;
#30385 = VERTEX_POINT ( 'NONE', #52844 ) ;
#30386 = CARTESIAN_POINT ( 'NONE',  ( 76.25939620287860521, 51.63842756541252044, -16.17602125672954116 ) ) ;
#30387 = CARTESIAN_POINT ( 'NONE',  ( 76.03824915322937272, 65.38513206480712370, -14.40956150002899783 ) ) ;
#30388 = CARTESIAN_POINT ( 'NONE',  ( 164.4261001824251878, 245.8526357240660900, 1.583002802772015549 ) ) ;
#30389 = CARTESIAN_POINT ( 'NONE',  ( 161.7518432240285620, 284.4801498230883112, 0.5359932121324623155 ) ) ;
#30390 = CARTESIAN_POINT ( 'NONE',  ( 198.9721957120447655, 281.0613474150461570, 17.36564602955951386 ) ) ;
#30391 = FACE_OUTER_BOUND ( 'NONE', #4173, .T. ) ;
#30392 = ORIENTED_EDGE ( 'NONE', *, *, #79415, .F. ) ;
#30393 = CARTESIAN_POINT ( 'NONE',  ( 88.22177397292790602, 44.42207723138842113, 4.484962078095955818 ) ) ;
#30394 = CARTESIAN_POINT ( 'NONE',  ( 156.8463053224485009, 274.3823876006896398, 13.73651536856081989 ) ) ;
#30395 = DIRECTION ( 'NONE',  ( 1.000000000000000000, 0.000000000000000000, -1.082076799516502204E-16 ) ) ;
#30396 = CARTESIAN_POINT ( 'NONE',  ( 153.2283961777204695, 265.2476279883323400, -17.66880461074566000 ) ) ;
#30397 = CARTESIAN_POINT ( 'NONE',  ( 72.74690663434007831, 70.81824800135888154, 7.160589954729633000 ) ) ;
#30398 = CARTESIAN_POINT ( 'NONE',  ( 45.80758703142363686, 72.03864405183792030, 10.00000000000000000 ) ) ;
#30399 = ORIENTED_EDGE ( 'NONE', *, *, #50966, .F. ) ;
#30400 = CARTESIAN_POINT ( 'NONE',  ( 197.5221644013859645, 266.2761734353669567, 4.458159567591970962 ) ) ;
#30401 = CARTESIAN_POINT ( 'NONE',  ( 148.3745023213073750, 276.3025496145838815, -3.856079141225808637 ) ) ;
#30402 = CARTESIAN_POINT ( 'NONE',  ( 82.10590413265644827, 40.80812859821141103, 1.532309608727412398 ) ) ;
#30403 = CIRCLE ( 'NONE', #25573, 17.82106496071138224 ) ;
#30404 = CARTESIAN_POINT ( 'NONE',  ( 184.5990297707867001, 263.7127329470384325, -12.27809941363454271 ) ) ;
#30405 = CARTESIAN_POINT ( 'NONE',  ( 83.53052282221433700, 51.97849157102297113, 15.01265415031365436 ) ) ;
#30406 = CARTESIAN_POINT ( 'NONE',  ( 198.3987358442466586, 266.1842203803777238, 0.8103656318469341091 ) ) ;
#30407 = EDGE_CURVE ( 'NONE', #47882, #4221, #45242, .T. ) ;
#30408 = ORIENTED_EDGE ( 'NONE', *, *, #69967, .F. ) ;
#30409 = CARTESIAN_POINT ( 'NONE',  ( 190.8907028847385448, 300.0145992415348815, -5.421341690443150618 ) ) ;
#30410 = CARTESIAN_POINT ( 'NONE',  ( 186.4922146040686357, 282.5459359838986302, 16.18330935361411349 ) ) ;
#30411 = VECTOR ( 'NONE', #56318, 1000.000000000000114 ) ;
#30412 = AXIS2_PLACEMENT_3D ( 'NONE', #59502, #98546, #22015 ) ;
#30413 = CARTESIAN_POINT ( 'NONE',  ( 164.2723164851102808, 246.1189969011916503, -1.993789335506892302 ) ) ;
#30415 = CARTESIAN_POINT ( 'NONE',  ( 192.8080529993486039, 268.3314956550081547, 12.47957376853008959 ) ) ;
#30414 = CARTESIAN_POINT ( 'NONE',  ( 193.9844289374573520, 294.6561085335266625, 15.49818881749970245 ) ) ;
#30416 = CARTESIAN_POINT ( 'NONE',  ( 22.87232021560678064, 28.90829794293881960, 10.00000000000000355 ) ) ;
#30417 = CARTESIAN_POINT ( 'NONE',  ( 21.07736754015083491, 189.6427522451419350, -10.00000000000009592 ) ) ;
#30418 = CARTESIAN_POINT ( 'NONE',  ( 165.4384176284148964, 285.1150933481030165, -3.137621857651547330 ) ) ;
#30419 = CARTESIAN_POINT ( 'NONE',  ( 68.05994358318133663, 69.15766078933415884, -5.932084911600773225 ) ) ;
#30420 = CARTESIAN_POINT ( 'NONE',  ( 198.6742831389107096, 286.5330427765190393, 17.60232614297041565 ) ) ;
#30421 = VECTOR ( 'NONE', #65797, 1000.000000000000000 ) ;
#30422 = CARTESIAN_POINT ( 'NONE',  ( -10.27112140336314994, 171.0024278399161233, -9.188101187500093303 ) ) ;
#30423 = CARTESIAN_POINT ( 'NONE',  ( 78.30721297357251842, 216.0177522451418497, -10.00000000000009592 ) ) ;
#30424 = ORIENTED_EDGE ( 'NONE', *, *, #90628, .F. ) ;
#30425 = CARTESIAN_POINT ( 'NONE',  ( 67.15772368909351542, 67.74692886573922124, -6.548511843863578541 ) ) ;
#30426 = CARTESIAN_POINT ( 'NONE',  ( 72.71813417941987723, 70.76084006159409512, -7.966439650937866546 ) ) ;
#30427 = CARTESIAN_POINT ( 'NONE',  ( -22.42236680055709641, 157.8615022471902591, 0.000000000000000000 ) ) ;
#30428 = CARTESIAN_POINT ( 'NONE',  ( 6.913983429043053519, 183.9869531367911009, 4.594050593750046652 ) ) ;
#30429 = CARTESIAN_POINT ( 'NONE',  ( 28.31825578742223115, 28.30066082961423390, -10.00000000000000533 ) ) ;
#30430 = DIRECTION ( 'NONE',  ( -0.1963739994383812415, 0.9805290675673896672, 0.000000000000000000 ) ) ;
#30431 = CARTESIAN_POINT ( 'NONE',  ( 204.9463377925012253, 275.6695254486514841, -14.15865086131798378 ) ) ;
#30432 = PLANE ( 'NONE',  #23225 ) ;
#30433 = B_SPLINE_SURFACE_WITH_KNOTS ( 'NONE', 3, 1, ( 
 ( #95485, #81264 ),
 ( #35109, #66019 ),
 ( #41202, #2745 ),
 ( #18439, #96968 ),
 ( #27534, #89378 ),
 ( #33634, #48327 ),
 ( #40707, #17940 ),
 ( #26038, #79273 ),
 ( #56908, #87894 ),
 ( #51296, #68005 ),
 ( #98929, #29024 ),
 ( #82268, #37100 ),
 ( #52300, #83238 ),
 ( #75131, #67000 ),
 ( #97927, #81756 ),
 ( #59895, #28502 ),
 ( #19933, #68497 ),
 ( #12841, #90863 ),
 ( #6205, #74138 ),
 ( #35614, #20430 ),
 ( #75617, #90359 ),
 ( #89855, #21415 ),
 ( #43701, #60880 ),
 ( #20940, #99421 ),
 ( #58886, #28009 ),
 ( #83746, #13806 ),
 ( #29998, #36099 ),
 ( #74644, #4731 ),
 ( #29507, #60384 ),
 ( #5219, #14309 ),
 ( #91340, #21900 ),
 ( #45195, #44685 ),
 ( #5706, #98433 ),
 ( #51821, #36597 ) ),
 .UNSPECIFIED., .T., .F., .F.,
 ( 4, 2, 2, 2, 2, 2, 2, 2, 2, 2, 2, 2, 2, 2, 2, 2, 4 ),
 ( 2, 2 ),
 ( 0.000000000000000000, 0.06250000000000000000, 0.1250000000000000000, 0.1875000000000000000, 0.2500000000000000000, 0.3125000000000000000, 0.3750000000000000000, 0.4375000000000000000, 0.5000000000000000000, 0.5625000000000000000, 0.6250000000000000000, 0.6875000000000000000, 0.7500000000000000000, 0.8125000000000000000, 0.8750000000000000000, 0.9375000000000000000, 1.000000000000000000 ),
 ( 0.000000000000000000, 1.000000000000000000 ),
 .UNSPECIFIED. ) ;
#30434 = CARTESIAN_POINT ( 'NONE',  ( 175.8155514549374914, 252.9580239610218371, -3.267414397889120359 ) ) ;
#30435 = CARTESIAN_POINT ( 'NONE',  ( 190.6298455067565101, 261.9054759779421602, -0.7664710513680175197 ) ) ;
#30436 = CARTESIAN_POINT ( 'NONE',  ( 183.0585217367469681, 295.7022925660351689, 1.036231964973731490 ) ) ;
#30437 = CARTESIAN_POINT ( 'NONE',  ( 72.04657099559547362, 205.7365022471902023, -10.00000000000009059 ) ) ;
#30438 = CARTESIAN_POINT ( 'NONE',  ( 82.01460820302004606, 41.19402847427713255, 5.465372724684262273 ) ) ;
#30439 = VECTOR ( 'NONE', #85474, 1000.000000000000000 ) ;
#30440 = CARTESIAN_POINT ( 'NONE',  ( 147.6618183892331331, 274.8892235422768522, 8.990680574201936892 ) ) ;
#30441 = CARTESIAN_POINT ( 'NONE',  ( 36.52174756457106497, 182.7048013555409796, 4.594050593750051981 ) ) ;
#30442 = CARTESIAN_POINT ( 'NONE',  ( 66.43767850218320348, 67.94397599821699885, 6.523424134266977426 ) ) ;
#30443 = DIRECTION ( 'NONE',  ( -0.8278489937552534483, 0.5609510170580086497, 0.000000000000000000 ) ) ;
#30444 = CARTESIAN_POINT ( 'NONE',  ( 40.83172133312034191, 29.28920272979929962, -7.433330006724141015 ) ) ;
#30445 = B_SPLINE_CURVE_WITH_KNOTS ( 'NONE', 3,
 ( #79744, #10808, #34591, #95947, #18919, #65990, #87867, #65490, #56388, #79248, #65004, #96439, #96943, #57386, #95461, #27509, #87384, #27003, #81240, #26508, #49792, #17391, #3711, #10306, #88360, #50287, #88866, #71619, #19431, #2215, #63992, #41178, #33096, #72114, #2718, #64501, #94934, #17913, #26013, #33606, #9820, #56884, #18413, #49304, #80755, #80241 ),
 .UNSPECIFIED., .F., .F.,
 ( 4, 1, 1, 1, 2, 2, 1, 1, 1, 2, 2, 1, 1, 2, 2, 1, 1, 2, 2, 1, 1, 2, 2, 1, 2, 2, 1, 2, 2, 4 ),
 ( 0.000000000000000000, 0.06249999999997297995, 0.09374999999995986544, 0.1093749999999537453, 0.1171874999999507477, 0.1249999999999477640, 0.1874999999999338307, 0.2187499999999278633, 0.2343749999999247824, 0.2421874999999236722, 0.2499999999999225064, 0.3124999999999218403, 0.3437499999999210631, 0.3593749999999211187, 0.3749999999999211742, 0.4374999999999245048, 0.4687499999999255040, 0.4843749999999260591, 0.4999999999999266143, 0.5624999999999341638, 0.5937499999999384936, 0.6093749999999407141, 0.6249999999999429345, 0.6874999999999559241, 0.7187499999999609201, 0.7499999999999659162, 0.8124999999999746869, 0.8437499999999790168, 0.8749999999999834577, 1.000000000000000000 ),
 .UNSPECIFIED. ) ;
#30446 = CARTESIAN_POINT ( 'NONE',  ( 151.1811967613751335, 268.7934813906678642, -15.79361349403328418 ) ) ;
#30447 = CARTESIAN_POINT ( 'NONE',  ( 207.6918009085542849, 270.9142438413412037, 7.009114282139513818 ) ) ;
#30448 = CARTESIAN_POINT ( 'NONE',  ( 188.8867764286892452, 268.2031459771304753, 13.62204560104310502 ) ) ;
#30449 = CARTESIAN_POINT ( 'NONE',  ( 159.9437897750486570, 278.5723957854588662, -9.797752282130973711 ) ) ;
#30450 = CARTESIAN_POINT ( 'NONE',  ( 179.9845513519039741, 262.5466105634188239, -14.24360566215998958 ) ) ;
#30451 = ITEM_DEFINED_TRANSFORMATION ( 'NONE', 'NONE', #13833,  #68784 ) ;
#30452 = CARTESIAN_POINT ( 'NONE',  ( 17.52119783388727825, 25.51421378149919050, -9.188101187500004485 ) ) ;
#30453 = CARTESIAN_POINT ( 'NONE',  ( 190.6084209867335915, 300.5035258309363826, -0.5505750481748228342 ) ) ;
#30454 = CARTESIAN_POINT ( 'NONE',  ( 71.59150237832598407, 59.07131284048556807, 15.33293140476554228 ) ) ;
#30455 = EDGE_CURVE ( 'NONE', #17810, #65477, #66066, .T. ) ;
#30456 = CARTESIAN_POINT ( 'NONE',  ( 155.1376601545389917, 261.9406857754215707, 18.55063430030667959 ) ) ;
#30457 = ORIENTED_EDGE ( 'NONE', *, *, #39740, .T. ) ;
#30458 = FACE_OUTER_BOUND ( 'NONE', #34610, .T. ) ;
#30459 = CARTESIAN_POINT ( 'NONE',  ( 75.27202081363431319, 53.54715819699419654, -16.04939499529041669 ) ) ;
#30460 = CARTESIAN_POINT ( 'NONE',  ( 148.5405002604136939, 273.7531191599721865, -8.243767320729981307 ) ) ;
#30461 = CARTESIAN_POINT ( 'NONE',  ( 81.88875743029853993, 42.19903267382473189, 7.633282463442304433 ) ) ;
#30462 = ORIENTED_EDGE ( 'NONE', *, *, #82998, .F. ) ;
#30463 = FACE_OUTER_BOUND ( 'NONE', #23935, .T. ) ;
#30464 = CARTESIAN_POINT ( 'NONE',  ( 72.61981592835454080, 71.39147990323394311, -5.869544098407574850 ) ) ;
#30465 = CARTESIAN_POINT ( 'NONE',  ( 72.60664467684684098, 57.18896317022895914, 16.35683965500042802 ) ) ;
#30466 = CARTESIAN_POINT ( 'NONE',  ( 180.6905943096166993, 256.8005298396895455, -7.802981789431568060 ) ) ;
#30467 = VERTEX_POINT ( 'NONE', #98480 ) ;
#30468 = VERTEX_POINT ( 'NONE', #35159 ) ;
#30470 = CARTESIAN_POINT ( 'NONE',  ( 83.36585540513543435, 42.45426523848973943, -5.297942810992300799 ) ) ;
#30469 = CARTESIAN_POINT ( 'NONE',  ( 202.4652556304803852, 279.1494446843323658, 15.55728013657999398 ) ) ;
#30471 = ORIENTED_EDGE ( 'NONE', *, *, #23587, .F. ) ;
#30472 = CARTESIAN_POINT ( 'NONE',  ( 150.8359915840788688, 269.3913942967808453, 15.73449616766854575 ) ) ;
#30473 = AXIS2_PLACEMENT_3D ( 'NONE', #7099, #93234, #23793 ) ;
#30474 = CARTESIAN_POINT ( 'NONE',  ( 33.29350273542976879, 95.92556709114796831, 59.99999999999999289 ) ) ;
#30475 = CARTESIAN_POINT ( 'NONE',  ( 79.89992946763821635, 58.05382247932297446, 16.26787594119393532 ) ) ;
#30476 = CARTESIAN_POINT ( 'NONE',  ( 67.09773762330524960, 69.34340978576997827, -3.906684184505462731 ) ) ;
#30478 = EDGE_CURVE ( 'NONE', #82087, #16991, #41326, .T. ) ;
#30477 = ORIENTED_EDGE ( 'NONE', *, *, #52947, .F. ) ;
#30479 = CARTESIAN_POINT ( 'NONE',  ( 147.7870527676176948, 274.6723112360602386, 9.257357958194809555 ) ) ;
#30480 = VECTOR ( 'NONE', #60708, 1000.000000000000000 ) ;
#30481 = AXIS2_PLACEMENT_3D ( 'NONE', #57046, #34261, #65156 ) ;
#30482 = ORIENTED_EDGE ( 'NONE', *, *, #99485, .T. ) ;
#30483 = CARTESIAN_POINT ( 'NONE',  ( 195.9713281756800427, 291.2146981034049418, 17.52210387885178022 ) ) ;
#30484 = AXIS2_PLACEMENT_3D ( 'NONE', #22275, #76970, #38460 ) ;
#30485 = CARTESIAN_POINT ( 'NONE',  ( 158.1038083475960718, 265.1254946056319000, 17.35475346825555931 ) ) ;
#30486 = ORIENTED_EDGE ( 'NONE', *, *, #85239, .T. ) ;
#30487 = CARTESIAN_POINT ( 'NONE',  ( 148.9232972370683399, 272.7042780851529642, 12.27045554427055940 ) ) ;
#30488 = CARTESIAN_POINT ( 'NONE',  ( 78.18897306460242191, 47.59851855797241171, -14.42851076044696335 ) ) ;
#30489 = EDGE_LOOP ( 'NONE', ( #68714, #23584, #96579, #4458 ) ) ;
#30490 = CARTESIAN_POINT ( 'NONE',  ( -13.56329049382775231, 72.36584674931148697, 14.11802994067470074 ) ) ;
#30491 = EDGE_CURVE ( 'NONE', #38493, #60445, #99467, .T. ) ;
#30492 = CARTESIAN_POINT ( 'NONE',  ( 190.8264243556038195, 300.1259329198319961, 8.466983560044813117 ) ) ;
#30493 = DIRECTION ( 'NONE',  ( 0.1266907948509091442, -0.9919422576440851680, 0.000000000000000000 ) ) ;
#30494 = CARTESIAN_POINT ( 'NONE',  ( 41.21417716447173518, 24.76426979415093044, 3.090169943749476733 ) ) ;
#30495 = ORIENTED_EDGE ( 'NONE', *, *, #89381, .T. ) ;
#30496 = VERTEX_POINT ( 'NONE', #33422 ) ;
#30497 = AXIS2_PLACEMENT_3D ( 'NONE', #32501, #40574, #63392 ) ;
#30498 = CARTESIAN_POINT ( 'NONE',  ( 86.64388902346107102, 46.39093904164906945, 9.083131486035911806 ) ) ;
#30499 = CARTESIAN_POINT ( 'NONE',  ( 147.1199024702499969, 275.8278494473859723, 5.224467159276165340 ) ) ;
#30500 = FACE_OUTER_BOUND ( 'NONE', #36710, .T. ) ;
#30501 = CARTESIAN_POINT ( 'NONE',  ( 190.1519139143167081, 301.2942192743771557, 4.481136594690903863 ) ) ;
#30502 = DIRECTION ( 'NONE',  ( 0.000000000000000000, 0.000000000000000000, 1.000000000000000000 ) ) ;
#30503 = CARTESIAN_POINT ( 'NONE',  ( 146.6045776406848802, 276.7204182345944901, 0.5293868638167662510 ) ) ;
#30504 = CARTESIAN_POINT ( 'NONE',  ( 146.9235493515124062, 276.1679430252639804, 0.7994986043261682607 ) ) ;
#30505 = CARTESIAN_POINT ( 'NONE',  ( 162.5659316022686482, 257.3233763081025813, 15.61851065589861243 ) ) ;
#30506 = CARTESIAN_POINT ( 'NONE',  ( 71.97959222828325210, 71.25346787330545340, 5.319870175860073935 ) ) ;
#30507 = CARTESIAN_POINT ( 'NONE',  ( 42.55121439978241682, 60.39930420098813357, 10.00000000000000000 ) ) ;
#30508 = CARTESIAN_POINT ( 'NONE',  ( 66.99733635639957186, 66.90869551988777175, 8.780753403809187674 ) ) ;
#30509 = CARTESIAN_POINT ( 'NONE',  ( 170.0120225124279330, 288.8437964431653313, 4.419511376178223649 ) ) ;
#30510 = CARTESIAN_POINT ( 'NONE',  ( 78.16621118571123361, 47.55685362076941658, 14.41442218299236622 ) ) ;
#30511 = VERTEX_POINT ( 'NONE', #48116 ) ;
#30512 = CARTESIAN_POINT ( 'NONE',  ( 190.7355618834574500, 300.2833113380910959, -3.494153871398564259 ) ) ;
#30513 = EDGE_CURVE ( 'NONE', #62347, #4089, #77202, .T. ) ;
#30514 = CARTESIAN_POINT ( 'NONE',  ( 75.72842597690201671, 54.31630180662983065, -16.10729176078631752 ) ) ;
#30515 = EDGE_CURVE ( 'NONE', #93599, #81863, #86079, .T. ) ;
#30516 = LINE ( 'NONE', #61405, #14013 ) ;
#30517 = CARTESIAN_POINT ( 'NONE',  ( 79.19657612229403298, 45.81917910958111406, 13.05272374772707700 ) ) ;
#30518 = CARTESIAN_POINT ( 'NONE',  ( 40.72531889205820477, 200.9865022471903160, -10.00000000000009592 ) ) ;
#30519 = CARTESIAN_POINT ( 'NONE',  ( 82.00351712801760584, 53.66420159836799542, -15.87819945195018789 ) ) ;
#30520 = CARTESIAN_POINT ( 'NONE',  ( -16.76269525828470464, 104.2312461070085021, 36.50000000000000000 ) ) ;
#30521 = VERTEX_POINT ( 'NONE', #79568 ) ;
#30523 = EDGE_CURVE ( 'NONE', #28922, #58170, #37732, .T. ) ;
#30522 = CARTESIAN_POINT ( 'NONE',  ( 163.4218292706009095, 247.5920839679097014, -10.44611490715852042 ) ) ;
#30524 = CARTESIAN_POINT ( 'NONE',  ( 206.2041691044954348, 273.4908977089264113, -9.455375957961031474 ) ) ;
#30525 = CARTESIAN_POINT ( 'NONE',  ( 72.48412649147189768, 71.58981433514404102, 5.211472423265571585 ) ) ;
#30526 = CARTESIAN_POINT ( 'NONE',  ( 45.83126033165607538, 197.2677522451418781, 10.00000000000009592 ) ) ;
#30527 = CARTESIAN_POINT ( 'NONE',  ( 127.8874276638293850, 235.4548013555409796, -4.594050593750042211 ) ) ;
#30528 = B_SPLINE_CURVE_WITH_KNOTS ( 'NONE', 3,
 ( #73171, #80292, #11864, #74669, #26560, #89405, #97468, #73658, #43224, #34158, #34642, #65541, #96488, #88922, #4236, #19482, #28035, #51329, #74166, #96994, #4757, #35136, #82296, #18972, #66541, #28528, #66047, #49847, #12866, #67028, #36125, #27564, #43726, #5246, #97955, #18464, #10863, #41737, #80806, #135, #53320, #68526, #52817, #84277, #61416, #98458, #6230, #46203, #52326, #77120, #38103, #90890 ),
 .UNSPECIFIED., .F., .F.,
 ( 4, 2, 2, 2, 2, 2, 2, 2, 2, 2, 2, 2, 2, 2, 2, 2, 2, 2, 2, 2, 2, 2, 2, 2, 2, 4 ),
 ( 0.0006745074493109526727, 0.0008837329331894130339, 0.001092958417067873503, 0.001197571159007103630, 0.001302183900946333756, 0.001406796642885563883, 0.001511409384824794009, 0.001929860352581865435, 0.002348311320338936862, 0.003185213255853080582, 0.004022115191367223869, 0.004859017126881367589, 0.005277468094638439015, 0.005486693578516984270, 0.005591306320456222202, 0.005643612691425760504, 0.005695919062395299673, 0.005748225433364837975, 0.005800531804334376276, 0.005905144546273446808, 0.006114370030151567922, 0.006323595514029689904, 0.006532820997907811018, 0.006742046481785933000, 0.006951271965664054114, 0.007369722933420295476 ),
 .UNSPECIFIED. ) ;
#30529 = CARTESIAN_POINT ( 'NONE',  ( 199.2299651681423143, 285.5705732690366858, -17.65328173313980642 ) ) ;
#30530 = EDGE_CURVE ( 'NONE', #48310, #33772, #16220, .T. ) ;
#30531 = DIRECTION ( 'NONE',  ( -0.9008877160804935613, -0.4340522123146846045, 0.000000000000000000 ) ) ;
#30532 = CARTESIAN_POINT ( 'NONE',  ( 157.7529601300917363, 257.4108533407307959, 16.91445305439664892 ) ) ;
#30533 = CARTESIAN_POINT ( 'NONE',  ( 175.4516086236820342, 253.5594085358976884, -4.077166357663031704 ) ) ;
#30534 = CARTESIAN_POINT ( 'NONE',  ( 41.74435586355720318, 207.1589784336661637, -6.496448406907675876E-16 ) ) ;
#30535 = CARTESIAN_POINT ( 'NONE',  ( 27.19136022205111658, 198.0530062829863311, -4.648177544792955347E-16 ) ) ;
#30536 = CARTESIAN_POINT ( 'NONE',  ( 85.70574795423719650, 48.48025216897318046, -12.24584271313006312 ) ) ;
#30537 = ORIENTED_EDGE ( 'NONE', *, *, #63705, .T. ) ;
#30539 = EDGE_CURVE ( 'NONE', #24506, #42773, #64320, .T. ) ;
#30538 = CARTESIAN_POINT ( 'NONE',  ( 70.94537046311441486, 63.12358859840954040, 13.51887736991167621 ) ) ;
#30541 = CARTESIAN_POINT ( 'NONE',  ( 74.37357505727348439, 67.95923626955014640, -11.68566301663373963 ) ) ;
#30540 = B_SPLINE_CURVE_WITH_KNOTS ( 'NONE', 3,
 ( #229, #31114, #75756, #99057, #60512, #22028, #23854, #86224, #94801, #95328, #18281, #94307, #24859, #16262, #17261, #48165, #63862, #40550, #1074, #25886, #78586, #71979, #86724, #2585 ),
 .UNSPECIFIED., .F., .F.,
 ( 4, 2, 2, 2, 2, 2, 2, 2, 2, 2, 2, 4 ),
 ( 0.000000000000000000, 0.1250000000000129896, 0.2500000000000259792, 0.3750000000000389688, 0.4375000000000411338, 0.5000000000000432987, 0.5625000000000454081, 0.6250000000000476286, 0.6875000000000497380, 0.7500000000000519584, 0.8750000000000259792, 1.000000000000000000 ),
 .UNSPECIFIED. ) ;
#30542 = EDGE_CURVE ( 'NONE', #62846, #43149, #6043, .T. ) ;
#30543 = CARTESIAN_POINT ( 'NONE',  ( 15.66239703771868719, 191.3967562850346837, -4.648177544792955347E-16 ) ) ;
#30544 = CARTESIAN_POINT ( 'NONE',  ( 190.9498149295421570, 299.9122141765958531, -5.138500224925297566 ) ) ;
#30545 = PLANE ( 'NONE',  #59572 ) ;
#30546 = DIRECTION ( 'NONE',  ( -1.000000000000000000, 0.000000000000000000, 0.000000000000000000 ) ) ;
#30547 = CARTESIAN_POINT ( 'NONE',  ( 164.8398358111874415, 250.3986661409049361, 10.19718004758793484 ) ) ;
#30548 = B_SPLINE_CURVE_WITH_KNOTS ( 'NONE', 3,
 ( #50937, #74771, #90985, #44820, #98058, #98566, #51438, #82405, #5349, #81886, #36230, #4865, #67136, #66641, #28635, #29638, #97571, #91467, #59518, #51946, #82886, #44326, #75258, #36727, #67633, #29150, #60021, #52927, #83879, #75755, #21546, #52428, #41456, #83375, #4347, #97095, #13940, #6341, #35243, #66149, #27663, #24021, #8331, #38715, #69621, #38203, #54399, #91982 ),
 .UNSPECIFIED., .F., .F.,
 ( 4, 2, 2, 2, 2, 2, 2, 2, 2, 2, 2, 2, 2, 2, 2, 2, 2, 2, 2, 2, 2, 2, 2, 4 ),
 ( 0.0006698723108304612634, 0.001653363054844869239, 0.001899235740848491481, 0.002145108426852113722, 0.002268044769853887546, 0.002390981112855661370, 0.002513917455857435628, 0.002636853798859209452, 0.002882726484862757534, 0.003128599170866305616, 0.003620344542873517139, 0.004603835286888004370, 0.005587326030902491601, 0.006079071402909690981, 0.006570816774916890361, 0.006693753117918673293, 0.006755221289419565192, 0.006816689460920456224, 0.006939625803922164562, 0.007062562146923872033, 0.007308434832927166412, 0.007554307518930460791, 0.008046052890937049548, 0.008537798262943638306 ),
 .UNSPECIFIED. ) ;
#30549 = CARTESIAN_POINT ( 'NONE',  ( 118.5773942495489592, 229.2677522451417929, -5.000000000000041744 ) ) ;
#30550 = AXIS2_PLACEMENT_3D ( 'NONE', #40840, #40346, #79910 ) ;
#30551 = CARTESIAN_POINT ( 'NONE',  ( 194.6550018378799507, 292.9242970792882943, -14.88548128926688463 ) ) ;
#30552 = ORIENTED_EDGE ( 'NONE', *, *, #67692, .F. ) ;
#30553 = AXIS2_PLACEMENT_3D ( 'NONE', #56632, #25753, #98522 ) ;
#30554 = CARTESIAN_POINT ( 'NONE',  ( 203.0507839702407580, 278.9527209772879814, 16.21318481136342626 ) ) ;
#30555 = CARTESIAN_POINT ( 'NONE',  ( 84.88474621580253654, 46.65668362480882791, -11.06339629709468042 ) ) ;
#30556 = AXIS2_PLACEMENT_3D ( 'NONE', #61407, #15807, #68516 ) ;
#30557 = CARTESIAN_POINT ( 'NONE',  ( 26.48065812185646806, 198.3464784336661637, 1.353441290958777327E-15 ) ) ;
#30558 = CARTESIAN_POINT ( 'NONE',  ( 7.350711452622367581, 26.01751292744054567, 6.180339887498949913 ) ) ;
#30559 = CARTESIAN_POINT ( 'NONE',  ( -14.22851846967002487, 105.1940860163543476, 43.89948692389422291 ) ) ;
#30560 = CARTESIAN_POINT ( 'NONE',  ( 71.97397978244890737, 59.31999651994269840, -15.32424238813479889 ) ) ;
#30561 = CARTESIAN_POINT ( 'NONE',  ( 179.4408063581041688, 277.4340371255875652, 17.62723233342114071 ) ) ;
#30563 = CARTESIAN_POINT ( 'NONE',  ( 71.05451054047556170, 202.6423013555409796, -4.594050593750043987 ) ) ;
#30562 = CARTESIAN_POINT ( 'NONE',  ( 194.9775624055715468, 275.3010545703284038, -15.63051501613322003 ) ) ;
#30564 = CARTESIAN_POINT ( 'NONE',  ( 12.74041337322552891, 7.759783934591623300, -1.583844403245364241 ) ) ;
#30565 = CARTESIAN_POINT ( 'NONE',  ( -23.51620074007619010, 60.05598660948531631, -10.00000000000000000 ) ) ;
#30566 = CARTESIAN_POINT ( 'NONE',  ( 17.73406340791407843, 11.20801979619927558, -3.090169943749474069 ) ) ;
#30567 = ORIENTED_EDGE ( 'NONE', *, *, #86359, .F. ) ;
#30568 = B_SPLINE_CURVE_WITH_KNOTS ( 'NONE', 3,
 ( #50672, #82644, #65879, #13202, #73015, #12198, #36471, #65386, #81625, #67375, #98301, #28890, #59768, #11216, #34485, #42083, #3607, #14187, #61261, #478, #14681, #37955, #69373, #60257 ),
 .UNSPECIFIED., .F., .F.,
 ( 4, 2, 2, 2, 2, 2, 2, 2, 2, 2, 2, 4 ),
 ( 1.437624280391282253E-16, 0.0003245379161388591786, 0.0006490758322775745919, 0.0009736137484162901137, 0.001298151664555005419, 0.001947227496832436462, 0.002271765412971152309, 0.002596303329109868590, 0.003245379161387301151, 0.003894454993664734146, 0.004543530825942166708, 0.005192606658219600137 ),
 .UNSPECIFIED. ) ;
#30569 = VECTOR ( 'NONE', #63115, 1000.000000000000000 ) ;
#30570 = CARTESIAN_POINT ( 'NONE',  ( 13.51768745649711789, 178.6115022471902591, 10.00000000000009592 ) ) ;
#30571 = CARTESIAN_POINT ( 'NONE',  ( 208.1415148974628266, 270.1353163636768500, 3.453641150550738725 ) ) ;
#30572 = CARTESIAN_POINT ( 'NONE',  ( 135.5998589986957086, 261.3464784336661637, 1.353441290958777327E-15 ) ) ;
#30573 = CARTESIAN_POINT ( 'NONE',  ( 37.13125039574066477, 23.29860640527294535, -2.839279412974138328 ) ) ;
#30574 = CARTESIAN_POINT ( 'NONE',  ( -31.49356256989596758, 94.88921800892812541, 43.89948692389422291 ) ) ;
#30576 = CARTESIAN_POINT ( 'NONE',  ( 189.4731981977795101, 299.9930995634677515, 4.873517838202077179 ) ) ;
#30575 = CARTESIAN_POINT ( 'NONE',  ( 82.75711436980199665, 40.78606491925197730, -2.625374872848795782 ) ) ;
#30577 = CARTESIAN_POINT ( 'NONE',  ( 69.02699102946681364, 64.47626555514762003, 12.46414397747164671 ) ) ;
#30578 = ORIENTED_EDGE ( 'NONE', *, *, #97085, .F. ) ;
#30579 = CARTESIAN_POINT ( 'NONE',  ( 81.31146485538788227, 51.54224463187279071, 15.34331897028426717 ) ) ;
#30580 = CARTESIAN_POINT ( 'NONE',  ( 183.2347291344400730, 286.2791671247540535, 15.72992646725049326 ) ) ;
#30581 = DIRECTION ( 'NONE',  ( -0.000000000000000000, -0.000000000000000000, -1.000000000000000000 ) ) ;
#30582 = CARTESIAN_POINT ( 'NONE',  ( 156.6575251390178209, 280.1398687009162245, -5.349388280191599954 ) ) ;
#30583 = CARTESIAN_POINT ( 'NONE',  ( 6.569006713621681648, 25.83396525600388216, -2.839279412974133887 ) ) ;
#30585 = ORIENTED_EDGE ( 'NONE', *, *, #60881, .F. ) ;
#30584 = VECTOR ( 'NONE', #28934, 1000.000000000000114 ) ;
#30586 = CARTESIAN_POINT ( 'NONE',  ( 206.5536402976238151, 272.8855958466460265, 8.283930970375774194 ) ) ;
#30587 = ADVANCED_FACE ( 'NONE', ( #6755 ), #53659, .F. ) ;
#30588 = DIRECTION ( 'NONE',  ( -1.000000000000000000, -1.156482317317871133E-15, 0.000000000000000000 ) ) ;
#30589 = CARTESIAN_POINT ( 'NONE',  ( 69.39586509779915957, 62.82256197253910557, 13.14397930765713163 ) ) ;
#30590 = EDGE_CURVE ( 'NONE', #69830, #59778, #77416, .T. ) ;
#30591 = DIRECTION ( 'NONE',  ( -0.000000000000000000, 0.000000000000000000, -1.000000000000000000 ) ) ;
#30592 = LINE ( 'NONE', #77183, #11014 ) ;
#30593 = CARTESIAN_POINT ( 'NONE',  ( 149.8172510487983402, 272.9568577616375364, 11.41474127177868425 ) ) ;
#30594 = CARTESIAN_POINT ( 'NONE',  ( 163.4055107321044318, 247.6203485056908846, -10.24153090796238530 ) ) ;
#30595 = CARTESIAN_POINT ( 'NONE',  ( 201.3053499423511425, 281.9759013948520874, -16.75960365258566398 ) ) ;
#30596 = ORIENTED_EDGE ( 'NONE', *, *, #81673, .T. ) ;
#30597 = CARTESIAN_POINT ( 'NONE',  ( 191.8019569549158518, 281.4351414054034990, 16.70232326611636964 ) ) ;
#30598 = CARTESIAN_POINT ( 'NONE',  ( 72.49881181205529401, 70.63619014701561127, 7.225229806400220056 ) ) ;
#30599 = ORIENTED_EDGE ( 'NONE', *, *, #34639, .T. ) ;
#30600 = CARTESIAN_POINT ( 'NONE',  ( 148.9694607950094394, 272.6243204573405592, 11.81236034532910573 ) ) ;
#30601 = CARTESIAN_POINT ( 'NONE',  ( 1.638219116881074022, 26.38162155862025671, -10.00000000000000000 ) ) ;
#30602 = CARTESIAN_POINT ( 'NONE',  ( 83.25213841147557048, 45.25846362796585964, -9.926727695915893435 ) ) ;
#30604 = EDGE_CURVE ( 'NONE', #17646, #39570, #32796, .T. ) ;
#30603 = ORIENTED_EDGE ( 'NONE', *, *, #76353, .T. ) ;
#30605 = DIRECTION ( 'NONE',  ( -0.000000000000000000, -0.000000000000000000, -1.000000000000000000 ) ) ;
#30606 = CARTESIAN_POINT ( 'NONE',  ( 167.4011299790239775, 281.5488363183706042, 12.98604958840868662 ) ) ;
#30607 = CARTESIAN_POINT ( 'NONE',  ( 15.49551970000783996, 14.11029122506293021, -8.090169943749478065 ) ) ;
#30608 = CARTESIAN_POINT ( 'NONE',  ( -52.57320609282758994, 32.70376883311633520, 10.00000000000000000 ) ) ;
#30609 = CARTESIAN_POINT ( 'NONE',  ( 69.60809846375656207, 62.55097647278505235, 13.37551271588222690 ) ) ;
#30610 = ORIENTED_EDGE ( 'NONE', *, *, #96899, .F. ) ;
#30611 = CARTESIAN_POINT ( 'NONE',  ( 103.7198194655286017, 224.5643266524159856, -9.188101187500093303 ) ) ;
#30612 = FACE_OUTER_BOUND ( 'NONE', #66835, .T. ) ;
#30613 = CARTESIAN_POINT ( 'NONE',  ( 73.27146650943220152, 69.63413511619549467, -9.919440617956860606 ) ) ;
#30614 = CARTESIAN_POINT ( 'NONE',  ( 151.0778907302193943, 268.9724126853576536, 15.84769371787143832 ) ) ;
#30615 = CARTESIAN_POINT ( 'NONE',  ( 136.7639277290221571, 249.7677522451418497, 10.00000000000009592 ) ) ;
#30616 = ORIENTED_EDGE ( 'NONE', *, *, #50036, .T. ) ;
#30617 = EDGE_CURVE ( 'NONE', #46146, #30076, #31295, .T. ) ;
#30618 = VERTEX_POINT ( 'NONE', #23683 ) ;
#30619 = EDGE_CURVE ( 'NONE', #25393, #16493, #63157, .T. ) ;
#30620 = ORIENTED_EDGE ( 'NONE', *, *, #72159, .T. ) ;
#30621 = CARTESIAN_POINT ( 'NONE',  ( 81.41849629226379648, 50.07632656148466310, 14.25717219674097791 ) ) ;
#30622 = VERTEX_POINT ( 'NONE', #78931 ) ;
#30623 = CARTESIAN_POINT ( 'NONE',  ( 67.79074041082746760, 67.79995302995581596, 7.165554312747186572 ) ) ;
#30624 = CARTESIAN_POINT ( 'NONE',  ( 87.89296955652562815, 44.95200477618789137, 6.297572492595292282 ) ) ;
#30625 = ORIENTED_EDGE ( 'NONE', *, *, #95425, .F. ) ;
#30626 = CARTESIAN_POINT ( 'NONE',  ( 163.7587049410067266, 247.0085981909329576, -6.137518685179130351 ) ) ;
#30627 = CARTESIAN_POINT ( 'NONE',  ( 195.7944228926560868, 283.4259135625417798, 17.81926924524233868 ) ) ;
#30628 = CARTESIAN_POINT ( 'NONE',  ( 170.9271208801252158, 283.6173671677598236, 12.30198536427989353 ) ) ;
#30629 = CARTESIAN_POINT ( 'NONE',  ( 147.8163551302855296, 274.6215580551378821, -9.286329195885331345 ) ) ;
#30631 = CARTESIAN_POINT ( 'NONE',  ( 82.44310520575160695, 54.28011738120409291, -15.96781897959228758 ) ) ;
#30630 = VECTOR ( 'NONE', #43119, 1000.000000000000227 ) ;
#30632 = CARTESIAN_POINT ( 'NONE',  ( 166.6760794757555288, 247.0815379807098964, 1.916300026573462878 ) ) ;
#30633 = CARTESIAN_POINT ( 'NONE',  ( 15.73863525846626032, 14.80170272979925272, 7.433330006724137462 ) ) ;
#30634 = DIRECTION ( 'NONE',  ( 0.4999999999999998890, -0.8660254037844385966, 0.000000000000000000 ) ) ;
#30635 = CARTESIAN_POINT ( 'NONE',  ( 79.99999999999998579, 9.999999999999985789, -54.99999999999999289 ) ) ;
#30636 = AXIS2_PLACEMENT_3D ( 'NONE', #51972, #75288, #74309 ) ;
#30638 = ORIENTED_EDGE ( 'NONE', *, *, #40866, .T. ) ;
#30637 = CARTESIAN_POINT ( 'NONE',  ( 50.33970617970973649, 92.06352491358971690, 10.00000000000000000 ) ) ;
#30639 = EDGE_CURVE ( 'NONE', #76828, #39058, #78866, .T. ) ;
#30640 = CARTESIAN_POINT ( 'NONE',  ( -27.42236680055714260, 166.5217562850347406, 1.224646799147364892E-15 ) ) ;
#30641 = CARTESIAN_POINT ( 'NONE',  ( 186.9301476837522671, 260.0195029309103916, 2.866143204992003479 ) ) ;
#30642 = DIRECTION ( 'NONE',  ( -0.8660254037844378194, -0.5000000000000014433, -0.000000000000000000 ) ) ;
#30643 = CARTESIAN_POINT ( 'NONE',  ( 81.66383133520196225, 46.03416481792814352, -11.52458638852417572 ) ) ;
#30644 = CARTESIAN_POINT ( 'NONE',  ( 200.5810378487751393, 283.2304467414622877, 18.38516374632547112 ) ) ;
#30645 = CARTESIAN_POINT ( 'NONE',  ( 157.9878497072205050, 281.0327258848784595, 1.976071138188537635 ) ) ;
#30646 = AXIS2_PLACEMENT_3D ( 'NONE', #22856, #36186, #76570 ) ;
#30647 =( BOUNDED_CURVE ( )  B_SPLINE_CURVE ( 2, ( #46572, #70385, #40473, #9610, #79021, #93221, #94228, #71405, #32881 ),
 .UNSPECIFIED., .F., .F. ) 
 B_SPLINE_CURVE_WITH_KNOTS ( ( 3, 2, 2, 2, 3 ),
 ( 0.7298387096774193727, 0.7311827956989247479, 0.7338709677419354982, 0.7365591397849462485, 0.7379032258064516236 ),
 .UNSPECIFIED. ) 
 CURVE ( )  GEOMETRIC_REPRESENTATION_ITEM ( )  RATIONAL_B_SPLINE_CURVE ( ( 0.9330127018922194093, 0.9330127018922194093, 1.000000000000000000, 0.8660254037844387076, 1.000000000000000000, 0.8660254037844387076, 1.000000000000000000, 0.9330127018922194093, 0.9330127018922194093 ) ) 
 REPRESENTATION_ITEM ( '' )  );
#30648 = ORIENTED_EDGE ( 'NONE', *, *, #23073, .F. ) ;
#30650 = EDGE_CURVE ( 'NONE', #69000, #74125, #87542, .T. ) ;
#30649 = CARTESIAN_POINT ( 'NONE',  ( 155.3605053979525223, 261.5547064916044064, -18.59460972482254704 ) ) ;
#30651 = CARTESIAN_POINT ( 'NONE',  ( 74.89378789817061488, 62.29972416502009480, -14.99401956569568561 ) ) ;
#30652 = DIRECTION ( 'NONE',  ( 1.000000000000000000, 0.000000000000000000, 0.000000000000000000 ) ) ;
#30653 = CARTESIAN_POINT ( 'NONE',  ( 6.860117161356328097, 174.7677522451418781, 10.00000000000009592 ) ) ;
#30654 = CARTESIAN_POINT ( 'NONE',  ( 192.8656348049960059, 266.9067490818276269, -11.31435781342206504 ) ) ;
#30655 = EDGE_CURVE ( 'NONE', #73229, #28615, #64711, .T. ) ;
#30656 = DIRECTION ( 'NONE',  ( 0.000000000000000000, 0.000000000000000000, -1.000000000000000000 ) ) ;
#30657 = CARTESIAN_POINT ( 'NONE',  ( 169.0081789574249456, 280.3483017457910478, -14.43549772046353574 ) ) ;
#30658 = CARTESIAN_POINT ( 'NONE',  ( 72.87908800440395396, 70.94240749453250316, 7.824389999597029188 ) ) ;
#30660 = CARTESIAN_POINT ( 'NONE',  ( 76.22741562560636908, 65.24129761985034293, 14.53304928680089958 ) ) ;
#30659 = CARTESIAN_POINT ( 'NONE',  ( -12.81524457486244550, 175.6589784336661353, -6.496448406907675876E-16 ) ) ;
#30661 = AXIS2_PLACEMENT_3D ( 'NONE', #44267, #29093, #82340 ) ;
#30662 = CARTESIAN_POINT ( 'NONE',  ( 187.2498241109438197, 296.0094539997018046, 8.138855039951142345 ) ) ;
#30663 = EDGE_LOOP ( 'NONE', ( #54894, #54906, #83862, #33710 ) ) ;
#30664 = EDGE_CURVE ( 'NONE', #81112, #18408, #23817, .T. ) ;
#30665 = VERTEX_POINT ( 'NONE', #29202 ) ;
#30666 = DIRECTION ( 'NONE',  ( 1.000000000000000000, 0.000000000000000000, 0.000000000000000000 ) ) ;
#30667 =( BOUNDED_CURVE ( )  B_SPLINE_CURVE ( 2, ( #54831, #70032, #24446, #646, #31532, #15322, #22935 ),
 .UNSPECIFIED., .F., .T. ) 
 B_SPLINE_CURVE_WITH_KNOTS ( ( 3, 2, 2, 3 ),
 ( 0.9875000000000000444, 0.9899999999999999911, 0.9949999999999999956, 1.000000000000000000 ),
 .UNSPECIFIED. ) 
 CURVE ( )  GEOMETRIC_REPRESENTATION_ITEM ( )  RATIONAL_B_SPLINE_CURVE ( ( 0.9755282581475767101, 0.9755282581475772652, 1.000000000000000000, 0.9510565162951535312, 1.000000000000000000, 0.9510565162951535312, 1.000000000000000000 ) ) 
 REPRESENTATION_ITEM ( '' )  );
#30668 = CARTESIAN_POINT ( 'NONE',  ( 84.02246009045383346, 46.28810143914654418, -10.58215992841521391 ) ) ;
#30669 = CARTESIAN_POINT ( 'NONE',  ( -17.42236680055705023, 149.2012482093457777, 0.000000000000000000 ) ) ;
#30670 = FACE_OUTER_BOUND ( 'NONE', #51180, .T. ) ;
#30671 = CARTESIAN_POINT ( 'NONE',  ( 81.83475763163420424, 42.02284892325379673, 6.270888180158195269 ) ) ;
#30672 = CARTESIAN_POINT ( 'NONE',  ( 167.1443788062580609, 247.6230354218334924, 5.209738392609174262 ) ) ;
#30673 = CARTESIAN_POINT ( 'NONE',  ( 21.28450569914983248, 195.3464784336661637, 1.353441290958777525E-15 ) ) ;
#30674 = CARTESIAN_POINT ( 'NONE',  ( 117.5758788303146076, 244.8149278399160664, 9.188101187500093303 ) ) ;
#30675 = CARTESIAN_POINT ( 'NONE',  ( 180.0968189326222557, 292.5754757235382613, -6.169244772567886947 ) ) ;
#30676 = CARTESIAN_POINT ( 'NONE',  ( 183.0802513414319606, 257.7480130289799831, -2.340672193140110657 ) ) ;
#30677 = CARTESIAN_POINT ( 'NONE',  ( 153.3843775842402124, 274.2552327709109932, -12.20347941078255616 ) ) ;
#30678 = CARTESIAN_POINT ( 'NONE',  ( 178.2729695640300349, 283.8809743909798158, -15.09020537081628888 ) ) ;
#30679 = CARTESIAN_POINT ( 'NONE',  ( 189.7838259857693686, 299.9317662682615833, -5.554424272425116271 ) ) ;
#30680 = CARTESIAN_POINT ( 'NONE',  ( 195.8627871995700502, 291.4026965887302936, 17.41145040657729481 ) ) ;
#30681 = CARTESIAN_POINT ( 'NONE',  ( 194.2321518193436987, 294.2270399159019121, 13.98132384850917020 ) ) ;
#30682 = CARTESIAN_POINT ( 'NONE',  ( 207.8570869662935365, 270.6279599915536664, -5.669188455878507504 ) ) ;
#30683 = DIRECTION ( 'NONE',  ( -0.000000000000000000, -0.000000000000000000, 1.000000000000000000 ) ) ;
#30684 = CARTESIAN_POINT ( 'NONE',  ( 193.0673599610802569, 264.3079050832715211, 7.416874666535670180 ) ) ;
#30685 = CARTESIAN_POINT ( 'NONE',  ( 171.4993218643381852, 279.8819833531975974, 13.90609482443614908 ) ) ;
#30686 = LINE ( 'NONE', #23062, #50704 ) ;
#30687 = CARTESIAN_POINT ( 'NONE',  ( 71.33995758461628611, 71.62702440093282519, 2.627031368899047870 ) ) ;
#30688 = CARTESIAN_POINT ( 'NONE',  ( 80.68240590561059378, 44.01878066398630551, 10.12792899481129894 ) ) ;
#30689 = CARTESIAN_POINT ( 'NONE',  ( 180.8455629192530125, 266.6468860283634967, -14.68397486445532252 ) ) ;
#30690 = ORIENTED_EDGE ( 'NONE', *, *, #52570, .T. ) ;
#30691 = CARTESIAN_POINT ( 'NONE',  ( -13.86269525828471849, 104.2312461070085021, 45.19948692389422717 ) ) ;
#30692 = CARTESIAN_POINT ( 'NONE',  ( 185.1323751026578464, 269.6436051631800979, 15.74023217557582477 ) ) ;
#30693 = CARTESIAN_POINT ( 'NONE',  ( 90.89164462408909628, 223.2833772461660260, -9.188101187500095079 ) ) ;
#30694 = CARTESIAN_POINT ( 'NONE',  ( 20.18540868186541459, 12.44966523072493914, -2.296566073217252530E-15 ) ) ;
#30695 = CARTESIAN_POINT ( 'NONE',  ( 77.56874017944556954, 59.32837778823116537, -16.45541604924300927 ) ) ;
#30696 = VECTOR ( 'NONE', #64022, 1000.000000000000114 ) ;
#30697 = CARTESIAN_POINT ( 'NONE',  ( 92.93017357788669131, 158.0650415295850735, 36.50000000000000000 ) ) ;
#30699 = CARTESIAN_POINT ( 'NONE',  ( 192.0737711319585230, 277.0892155713485181, 17.32299324414631414 ) ) ;
#30698 = FACE_OUTER_BOUND ( 'NONE', #27391, .T. ) ;
#30700 = CARTESIAN_POINT ( 'NONE',  ( 201.2026048815914692, 270.3487196048755550, -10.12796269912754710 ) ) ;
#30701 = CARTESIAN_POINT ( 'NONE',  ( 190.6420043223797620, 261.1713590208896107, -4.660055732604916123 ) ) ;
#30702 = DIRECTION ( 'NONE',  ( 0.000000000000000000, 0.000000000000000000, 1.000000000000000000 ) ) ;
#30703 = CARTESIAN_POINT ( 'NONE',  ( 52.48883062679684741, 201.1115022471902591, 10.00000000000009592 ) ) ;
#30704 = CARTESIAN_POINT ( 'NONE',  ( 192.4335622838504207, 297.3422883733380786, -12.83044365323471325 ) ) ;
#30705 = CARTESIAN_POINT ( 'NONE',  ( 66.13428293896411958, 69.21728233722956247, 1.665249920595609501 ) ) ;
#30706 = ORIENTED_EDGE ( 'NONE', *, *, #69637, .F. ) ;
#30707 = CARTESIAN_POINT ( 'NONE',  ( 24.06271987006732616, 35.93396525600390845, 2.839279412974139660 ) ) ;
#30708 = DIRECTION ( 'NONE',  ( 0.000000000000000000, 0.000000000000000000, 1.000000000000000000 ) ) ;
#30709 = CARTESIAN_POINT ( 'NONE',  ( 199.8990292968633469, 270.1221403762914406, 9.242915985417027969 ) ) ;
#30710 = CARTESIAN_POINT ( 'NONE',  ( 196.5475899070771675, 290.2165835061676944, -17.89382743182097002 ) ) ;
#30711 = EDGE_LOOP ( 'NONE', ( #54037, #2720, #79310, #55627 ) ) ;
#30712 = DIRECTION ( 'NONE',  ( -0.000000000000000000, 0.000000000000000000, -1.000000000000000000 ) ) ;
#30713 = CARTESIAN_POINT ( 'NONE',  ( 175.1271263694729328, 272.4273639404348728, 17.81557788710851042 ) ) ;
#30714 = CARTESIAN_POINT ( 'NONE',  ( 180.0421887822893439, 262.9451233745447780, -12.84000619916867159 ) ) ;
#30715 = CARTESIAN_POINT ( 'NONE',  ( 173.0587134762232324, 253.8503347386293854, -9.001391358779716967 ) ) ;
#30716 = AXIS2_PLACEMENT_3D ( 'NONE', #61171, #21692, #30282 ) ;
#30717 = CARTESIAN_POINT ( 'NONE',  ( 152.6992418905140028, 266.1641500988167763, 17.27767170937316621 ) ) ;
#30718 = ORIENTED_EDGE ( 'NONE', *, *, #75807, .T. ) ;
#30719 = CARTESIAN_POINT ( 'NONE',  ( 187.1956594725295417, 278.7701613363302044, 17.25881440492993590 ) ) ;
#30720 = CARTESIAN_POINT ( 'NONE',  ( 27.74993340135631215, 36.99752408145592852, 5.678558825948277544 ) ) ;
#30721 = VERTEX_POINT ( 'NONE', #5403 ) ;
#30722 = CARTESIAN_POINT ( 'NONE',  ( 66.57026871561890857, 68.76443072695623471, 4.738950751700697239 ) ) ;
#30723 = CARTESIAN_POINT ( 'NONE',  ( -55.59287931351117606, 32.99562883703961091, -10.00000000000000000 ) ) ;
#30726 = ADVANCED_FACE ( 'NONE', ( #51489 ), #60070, .T. ) ;
#30725 = EDGE_LOOP ( 'NONE', ( #65560, #40465, #29411, #16151, #92685, #77370 ) ) ;
#30724 = B_SPLINE_CURVE_WITH_KNOTS ( 'NONE', 3,
 ( #99289, #97800, #15149, #60743 ),
 .UNSPECIFIED., .F., .F.,
 ( 4, 4 ),
 ( 0.006074498585399344674, 0.01174373323087292767 ),
 .UNSPECIFIED. ) ;
#30727 = CARTESIAN_POINT ( 'NONE',  ( 86.37995054896607883, 46.98508828575033647, -10.52062608394496479 ) ) ;
#30728 = CARTESIAN_POINT ( 'NONE',  ( 159.0141149511101446, 255.2264691145165330, 17.40381185983830292 ) ) ;
#30729 = CARTESIAN_POINT ( 'NONE',  ( 190.6321288753560736, 278.4426617264936112, -16.55712034464263027 ) ) ;
#30730 = CARTESIAN_POINT ( 'NONE',  ( 192.6535100158423290, 296.9613277265186184, -13.39826475700667174 ) ) ;
#30731 = CARTESIAN_POINT ( 'NONE',  ( 46.88368875251778434, 110.3874725885333135, -10.00000000000000000 ) ) ;
#30732 = AXIS2_PLACEMENT_3D ( 'NONE', #64615, #88984, #28098 ) ;
#30733 = CARTESIAN_POINT ( 'NONE',  ( 115.9793180381956148, 237.7677522451418497, 10.00000000000009592 ) ) ;
#30734 = CARTESIAN_POINT ( 'NONE',  ( 81.63547489262985835, 55.73921394657421757, -16.35272683298455121 ) ) ;
#30736 = EDGE_CURVE ( 'NONE', #82113, #3476, #91520, .T. ) ;
#30735 = DIRECTION ( 'NONE',  ( -0.000000000000000000, 1.000000000000000000, 0.000000000000000000 ) ) ;
#30737 = ORIENTED_EDGE ( 'NONE', *, *, #61054, .F. ) ;
#30738 = FACE_OUTER_BOUND ( 'NONE', #92338, .T. ) ;
#30739 = EDGE_CURVE ( 'NONE', #70875, #45464, #82458, .T. ) ;
#30740 = VERTEX_POINT ( 'NONE', #29690 ) ;
#30741 = ORIENTED_EDGE ( 'NONE', *, *, #12128, .T. ) ;
#30742 = CARTESIAN_POINT ( 'NONE',  ( 172.7634016531041539, 271.0112792648602635, 16.42974606472167665 ) ) ;
#30743 = CARTESIAN_POINT ( 'NONE',  ( 84.38175156668881982, 50.02035787987339432, 13.81135446509517628 ) ) ;
#30744 = ORIENTED_EDGE ( 'NONE', *, *, #29335, .F. ) ;
#30746 = DIRECTION ( 'NONE',  ( 0.000000000000000000, 0.000000000000000000, 1.000000000000000000 ) ) ;
#30745 = CARTESIAN_POINT ( 'NONE',  ( 154.9032082715209810, 280.6326124547101699, -2.389722542998433230 ) ) ;
#30747 = CARTESIAN_POINT ( 'NONE',  ( 206.6093111437328957, 272.7891711126852101, -9.934261249647553527 ) ) ;
#30748 = CARTESIAN_POINT ( 'NONE',  ( 148.1846401255833996, 275.9836697316168284, -5.368268268079755323 ) ) ;
#30749 = CARTESIAN_POINT ( 'NONE',  ( 71.19320197529700067, 61.90671673094616523, -14.21225849412795306 ) ) ;
#30750 = CARTESIAN_POINT ( 'NONE',  ( 82.72861693379122983, 40.56744065827609802, 0.9164833145372243139 ) ) ;
#30751 = CARTESIAN_POINT ( 'NONE',  ( 178.6782777294722848, 260.6412425082613709, 13.57969907341511551 ) ) ;
#30752 = CARTESIAN_POINT ( 'NONE',  ( 77.00376392975798012, 63.39239755058648029, -15.46687034352795109 ) ) ;
#30753 = CARTESIAN_POINT ( 'NONE',  ( 186.7621306400879462, 287.1057732871925623, -15.90520287716750225 ) ) ;
#30754 = CARTESIAN_POINT ( 'NONE',  ( 103.0428032491157779, 239.4869531367911293, 4.594050593750046652 ) ) ;
#30755 = ORIENTED_EDGE ( 'NONE', *, *, #94882, .T. ) ;
#30756 = CARTESIAN_POINT ( 'NONE',  ( 186.7511758073848682, 262.6631644945539392, -10.04217688415225496 ) ) ;
#30757 = CARTESIAN_POINT ( 'NONE',  ( 41.44395331530407844, 35.87878583063845639, -9.188101187500006262 ) ) ;
#30758 = CARTESIAN_POINT ( 'NONE',  ( 188.0217479200190382, 273.7640949189246840, 16.90097692181329236 ) ) ;
#30759 = ORIENTED_EDGE ( 'NONE', *, *, #48568, .T. ) ;
#30760 = CARTESIAN_POINT ( 'NONE',  ( 74.15402199957247831, 68.42859570829774896, -11.65141325894000879 ) ) ;
#30761 = CARTESIAN_POINT ( 'NONE',  ( 72.74506803476772632, 63.63576506029848190, -13.82193098727775649 ) ) ;
#30762 = FACE_OUTER_BOUND ( 'NONE', #53261, .T. ) ;
#30763 = CARTESIAN_POINT ( 'NONE',  ( 192.7699314614395689, 296.7596798676532899, 11.34673828722139177 ) ) ;
#30764 = CARTESIAN_POINT ( 'NONE',  ( 72.85138575605425615, 64.91499728177296902, 13.16331341298753088 ) ) ;
#30765 = CARTESIAN_POINT ( 'NONE',  ( 33.63407072503001416, 49.62913085183823370, 10.00000000000000000 ) ) ;
#30766 = CARTESIAN_POINT ( 'NONE',  ( 88.86189758574322184, 232.1115022471902876, -5.000000000000047962 ) ) ;
#30767 = VERTEX_POINT ( 'NONE', #76309 ) ;
#30768 = CARTESIAN_POINT ( 'NONE',  ( 148.0737445431542767, 274.1757465147189237, 10.26368672933362980 ) ) ;
#30769 = ORIENTED_EDGE ( 'NONE', *, *, #85209, .F. ) ;
#30771 = EDGE_CURVE ( 'NONE', #18450, #27245, #91033, .T. ) ;
#30770 = CARTESIAN_POINT ( 'NONE',  ( 194.9757425430702824, 292.9391030023704161, -15.21392314336593365 ) ) ;
#30772 = ORIENTED_EDGE ( 'NONE', *, *, #61047, .T. ) ;
#30773 = CARTESIAN_POINT ( 'NONE',  ( 188.1032490429140580, 266.2180392766005639, -11.82133915774577559 ) ) ;
#30774 = ADVANCED_FACE ( 'NONE', ( #21598 ), #75813, .F. ) ;
#30775 = CARTESIAN_POINT ( 'NONE',  ( 190.7104275908211264, 284.0216516728820011, -16.91638317915403533 ) ) ;
#30776 = CARTESIAN_POINT ( 'NONE',  ( 193.0146740725342056, 262.6358330379304107, 4.705848471798295130 ) ) ;
#30777 = CARTESIAN_POINT ( 'NONE',  ( 158.4506253844079708, 263.4166843688063295, 17.67374169831186848 ) ) ;
#30778 = CARTESIAN_POINT ( 'NONE',  ( 204.6053525328498779, 273.0989532408518130, -10.15815190134183332 ) ) ;
#30780 = CARTESIAN_POINT ( 'NONE',  ( 160.8008004585890376, 281.5710333326640580, 5.628202240593611627 ) ) ;
#30779 = CARTESIAN_POINT ( 'NONE',  ( 184.3757908040668099, 288.5642296694110769, -13.61842078453970295 ) ) ;
#30781 = CARTESIAN_POINT ( 'NONE',  ( 153.2583947049096764, 265.1956690150883560, -17.64103123457563882 ) ) ;
#30782 = ORIENTED_EDGE ( 'NONE', *, *, #94225, .T. ) ;
#30783 = CARTESIAN_POINT ( 'NONE',  ( 204.7259617510281942, 272.8945987308273970, -9.650000825374167590 ) ) ;
#30784 = DIRECTION ( 'NONE',  ( 0.000000000000000000, -0.000000000000000000, 1.000000000000000000 ) ) ;
#30785 = CARTESIAN_POINT ( 'NONE',  ( 163.7898901466472523, 247.5855377128527834, -7.511645082746166047 ) ) ;
#30786 = EDGE_CURVE ( 'NONE', #69106, #40327, #64084, .T. ) ;
#30787 = CARTESIAN_POINT ( 'NONE',  ( 141.9699493749754140, 259.7505386000626686, -7.968025677899344572 ) ) ;
#30788 = CARTESIAN_POINT ( 'NONE',  ( 189.0756608774803453, 270.0634534580582908, -14.06871611248690890 ) ) ;
#30789 = CARTESIAN_POINT ( 'NONE',  ( 185.1141009223508149, 296.8708822037961568, -4.333820615423671363 ) ) ;
#30790 = CARTESIAN_POINT ( 'NONE',  ( 82.93017357788667709, 175.3855496052738374, -36.50000000000000000 ) ) ;
#30791 = CARTESIAN_POINT ( 'NONE',  ( 28.07773955407504118, 197.0177522451419350, 5.000000000000046185 ) ) ;
#30792 = VECTOR ( 'NONE', #72428, 1000.000000000000227 ) ;
#30793 = CARTESIAN_POINT ( 'NONE',  ( 191.4411680433141214, 282.7668619920169135, -17.27576285388926536 ) ) ;
#30794 = CARTESIAN_POINT ( 'NONE',  ( 74.27315540778812419, 65.63952288200199803, -13.71985095672392774 ) ) ;
#30795 = CARTESIAN_POINT ( 'NONE',  ( 76.27746593522670082, 214.8458772461660544, 9.188101187500095079 ) ) ;
#30796 = LINE ( 'NONE', #24682, #57283 ) ;
#30797 = CARTESIAN_POINT ( 'NONE',  ( 147.4271219180435253, 275.2957297547342819, -3.800519706258907782 ) ) ;
#30798 = CARTESIAN_POINT ( 'NONE',  ( 207.9743173328493526, 270.4249110404894054, -2.481515874287090639 ) ) ;
#30799 = CARTESIAN_POINT ( 'NONE',  ( 78.75297625639956323, 47.66336229257159118, 14.29739783539339371 ) ) ;
#30800 = CARTESIAN_POINT ( 'NONE',  ( 207.8431546909062320, 270.6520914003897360, -6.441273666418043220 ) ) ;
#30801 = CARTESIAN_POINT ( 'NONE',  ( 84.67010498191464762, 49.80963328464838469, -13.17095790170508174 ) ) ;
#30802 = CARTESIAN_POINT ( 'NONE',  ( 48.88270317314112390, 187.4824982072973967, 3.021315404115420679E-15 ) ) ;
#30804 = CARTESIAN_POINT ( 'NONE',  ( 76.10825311040436247, 51.34890012828683581, 15.64337078650107671 ) ) ;
#30803 = CARTESIAN_POINT ( 'NONE',  ( 73.36014537180697914, 69.17374614814826828, -9.939646048807338374 ) ) ;
#30805 = CARTESIAN_POINT ( 'NONE',  ( 165.9714824136468394, 249.3895961940136488, -9.198834327378280662 ) ) ;
#30806 = CARTESIAN_POINT ( 'NONE',  ( 163.9665205130568495, 246.6486510615381178, -4.977134839185944237 ) ) ;
#30807 = CARTESIAN_POINT ( 'NONE',  ( 157.8562613713738472, 257.2319303423452652, 17.81420683562559404 ) ) ;
#30808 = DIRECTION ( 'NONE',  ( -0.8660254037844387076, -0.4999999999999998890, -0.000000000000000000 ) ) ;
#30809 = EDGE_CURVE ( 'NONE', #55246, #93711, #75312, .T. ) ;
#30810 = EDGE_CURVE ( 'NONE', #6582, #51970, #37282, .T. ) ;
#30811 = CARTESIAN_POINT ( 'NONE',  ( 50.62146334811270521, 200.0333772461660544, 9.188101187500095079 ) ) ;
#30812 = CARTESIAN_POINT ( 'NONE',  ( 164.3815567799200039, 246.8702290586211632, -5.719362487965026887 ) ) ;
#30813 = CARTESIAN_POINT ( 'NONE',  ( 87.94829491887652750, 43.95349485838026027, 0.4967466087338212044 ) ) ;
#30814 = CARTESIAN_POINT ( 'NONE',  ( 76.47316661484272515, 51.61210842333346704, -15.65491330287230376 ) ) ;
#30815 = CARTESIAN_POINT ( 'NONE',  ( -14.62813816649718213, 172.3615022471903160, 5.000000000000046185 ) ) ;
#30816 = CARTESIAN_POINT ( 'NONE',  ( 66.61806446105697432, 69.58935570732562326, -0.3124497180235544791 ) ) ;
#30817 = CARTESIAN_POINT ( 'NONE',  ( 196.6129024267879402, 268.7927177136375576, -10.56481122998096289 ) ) ;
#30818 = CARTESIAN_POINT ( 'NONE',  ( 26.97531487256933858, 21.28920272979927830, -7.433330006724141015 ) ) ;
#30819 = CARTESIAN_POINT ( 'NONE',  ( 150.7691137448031213, 269.5072301123068428, -15.63821625702598084 ) ) ;
#30820 = CARTESIAN_POINT ( 'NONE',  ( 196.5475899070771675, 290.2165835061676944, -17.89382743182097002 ) ) ;
#30821 = CARTESIAN_POINT ( 'NONE',  ( 10.03310832875943603, 27.83396525600388571, -2.839279412974133887 ) ) ;
#30822 = CARTESIAN_POINT ( 'NONE',  ( 60.95981515367195414, 199.8768266524160140, 9.188101187500096856 ) ) ;
#30823 = CARTESIAN_POINT ( 'NONE',  ( 76.77756057274272905, 63.67496528870245243, 15.32214893988671101 ) ) ;
#30824 = CARTESIAN_POINT ( 'NONE',  ( 76.19481306539471177, 60.31832523138206170, 16.18231617239213094 ) ) ;
#30825 = CARTESIAN_POINT ( 'NONE',  ( 198.2819808855875863, 287.2125302111982705, 18.53535247371401695 ) ) ;
#30826 = FACE_OUTER_BOUND ( 'NONE', #2107, .T. ) ;
#30827 = CARTESIAN_POINT ( 'NONE',  ( 76.48733475582915275, 56.37564448157380781, -16.15952532856388046 ) ) ;
#30828 = CARTESIAN_POINT ( 'NONE',  ( 99.68721513304873838, 238.3615022471903160, 5.000000000000046185 ) ) ;
#30829 = CARTESIAN_POINT ( 'NONE',  ( 161.5875797534026219, 250.7690973254556468, 12.95526170413129030 ) ) ;
#30830 = CARTESIAN_POINT ( 'NONE',  ( 165.0509870607838252, 244.7702999017660375, -2.356357909806504392 ) ) ;
#30831 = VERTEX_POINT ( 'NONE', #22086 ) ;
#30832 = CARTESIAN_POINT ( 'NONE',  ( 77.13981730435806128, 49.50565677253940322, 14.95469319025198196 ) ) ;
#30833 = CARTESIAN_POINT ( 'NONE',  ( 202.8371121491529152, 271.7102578477088173, 10.98807562330369869 ) ) ;
#30834 = ORIENTED_EDGE ( 'NONE', *, *, #94923, .F. ) ;
#30835 = CARTESIAN_POINT ( 'NONE',  ( 159.9531724557437826, 253.5999738052623229, -15.71074128491364874 ) ) ;
#30836 = CARTESIAN_POINT ( 'NONE',  ( 187.5118225138183163, 276.9259439731086445, -17.64892817816586756 ) ) ;
#30837 = CARTESIAN_POINT ( 'NONE',  ( 69.01668676381960665, 68.81684766018636878, -6.622719373402289555 ) ) ;
#30838 = VERTEX_POINT ( 'NONE', #35794 ) ;
#30839 = B_SPLINE_CURVE_WITH_KNOTS ( 'NONE', 3,
 ( #85982, #16509, #47404, #78331, #99136, #29722, #60596, #22120, #83966, #2843, #96062, #71739, #18530, #9418, #63112, #48924, #49413, #26621, #41297, #79367, #11444, #80360, #65114, #10424, #33733, #56508, #79861, #10931, #40793, #25624, #87497 ),
 .UNSPECIFIED., .F., .F.,
 ( 4, 3, 3, 3, 3, 3, 3, 3, 3, 3, 4 ),
 ( 0.000000000000000000, 0.1333490885032345696, 0.3007194338854333737, 0.4699862290245237495, 0.5844252810809289489, 0.6686540514502742338, 0.7354980260655397117, 0.8028463152565420424, 0.8633854507756993923, 0.9437142632667149256, 1.000000000000000000 ),
 .UNSPECIFIED. ) ;
#30840 = ORIENTED_EDGE ( 'NONE', *, *, #11154, .F. ) ;
#30841 = CARTESIAN_POINT ( 'NONE',  ( 207.6900289502458179, 270.9173129631602706, 7.178327969100043227 ) ) ;
#30842 = CARTESIAN_POINT ( 'NONE',  ( 147.7112127936102866, 274.8036699242858276, -9.124700685424272706 ) ) ;
#30843 = ORIENTED_EDGE ( 'NONE', *, *, #2938, .T. ) ;
#30844 = CARTESIAN_POINT ( 'NONE',  ( 23.93942162470478507, 34.79752408145593279, -5.678558825948271327 ) ) ;
#30845 = CARTESIAN_POINT ( 'NONE',  ( 74.83966849089097195, 54.13869872289780005, 16.11807719370478864 ) ) ;
#30846 = DIRECTION ( 'NONE',  ( -0.000000000000000000, -0.000000000000000000, -1.000000000000000000 ) ) ;
#30847 = CARTESIAN_POINT ( 'NONE',  ( 74.93756780616696744, 67.42216207915814152, -12.80861374294490318 ) ) ;
#30848 = ORIENTED_EDGE ( 'NONE', *, *, #48882, .T. ) ;
#30850 = EDGE_CURVE ( 'NONE', #22043, #94679, #67186, .T. ) ;
#30849 = FACE_OUTER_BOUND ( 'NONE', #17763, .T. ) ;
#30851 = DIRECTION ( 'NONE',  ( -0.6625377181876315191, -0.7490285521785713385, 0.000000000000000000 ) ) ;
#30852 = EDGE_CURVE ( 'NONE', #48169, #55924, #98110, .T. ) ;
#30853 = ORIENTED_EDGE ( 'NONE', *, *, #10882, .F. ) ;
#30854 = AXIS2_PLACEMENT_3D ( 'NONE', #15250, #84224, #91311 ) ;
#30855 = CARTESIAN_POINT ( 'NONE',  ( 174.3506819931331506, 286.9267872025895940, 11.76311152586403885 ) ) ;
#30857 = CARTESIAN_POINT ( 'NONE',  ( 67.96557359005117860, 65.23838819696450742, -10.59734309696486143 ) ) ;
#30856 = CARTESIAN_POINT ( 'NONE',  ( 71.17266338141718052, 64.03727702359581997, 13.60747010924504607 ) ) ;
#30858 = CARTESIAN_POINT ( 'NONE',  ( 208.2874212803407090, 269.8825990953837390, -1.143705256421198690 ) ) ;
#30859 = CARTESIAN_POINT ( 'NONE',  ( 163.7010375032499212, 247.1084811230698506, 6.649922295230481950 ) ) ;
#30860 = EDGE_CURVE ( 'NONE', #3474, #88681, #6882, .T. ) ;
#30861 = CARTESIAN_POINT ( 'NONE',  ( 188.4191156127841964, 294.8423196679893294, -11.05441416046296510 ) ) ;
#30862 = CARTESIAN_POINT ( 'NONE',  ( 157.0978663001774862, 258.5455091378672137, -17.31223197570816552 ) ) ;
#30863 = EDGE_CURVE ( 'NONE', #99756, #17862, #29211, .T. ) ;
#30864 = CARTESIAN_POINT ( 'NONE',  ( 143.3676317564762144, 244.3923013555409511, 4.594050593750050204 ) ) ;
#30865 = CARTESIAN_POINT ( 'NONE',  ( 159.5827168731687209, 254.9346697425724528, -15.70473076143803759 ) ) ;
#30866 = CARTESIAN_POINT ( 'NONE',  ( 182.5138934050887940, 259.5598872865875251, 9.236875158659382024 ) ) ;
#30867 = CARTESIAN_POINT ( 'NONE',  ( 65.12704176573704729, 220.6589784336661637, -6.496448406907675876E-16 ) ) ;
#30868 = EDGE_LOOP ( 'NONE', ( #45675, #97921, #85353, #96788 ) ) ;
#30869 = CARTESIAN_POINT ( 'NONE',  ( 151.3560786774222322, 268.4905770267490652, 15.54402364351346932 ) ) ;
#30870 = CYLINDRICAL_SURFACE ( 'NONE', #73891, 17.82106496071139645 ) ;
#30871 = ORIENTED_EDGE ( 'NONE', *, *, #60254, .F. ) ;
#30872 = CARTESIAN_POINT ( 'NONE',  ( 196.1154025625812380, 290.9651539452228235, -16.59765440650598478 ) ) ;
#30873 = ORIENTED_EDGE ( 'NONE', *, *, #93523, .F. ) ;
#30874 = CARTESIAN_POINT ( 'NONE',  ( 80.17557668363483003, 44.21690606740114049, -11.32705747359858073 ) ) ;
#30875 = CARTESIAN_POINT ( 'NONE',  ( 197.6872697694112162, 287.3145487930856916, 17.07396129458168232 ) ) ;
#30876 = CARTESIAN_POINT ( 'NONE',  ( 191.6723191112861855, 298.6608002251342100, -9.737039817265848995 ) ) ;
#30877 = LINE ( 'NONE', #77989, #92012 ) ;
#30878 = CARTESIAN_POINT ( 'NONE',  ( 193.7901930790854976, 294.9925349088783264, 14.24765323155741115 ) ) ;
#30879 = CARTESIAN_POINT ( 'NONE',  ( 71.34493322773809609, 66.48664206392754750, 11.31262581298163106 ) ) ;
#30880 = CARTESIAN_POINT ( 'NONE',  ( 85.15457341978220995, 207.7202760586659167, -5.415160957724236172E-17 ) ) ;
#30881 = VERTEX_POINT ( 'NONE', #90034 ) ;
#30882 = ORIENTED_EDGE ( 'NONE', *, *, #91423, .T. ) ;
#30883 = EDGE_CURVE ( 'NONE', #7334, #71477, #65916, .T. ) ;
#30884 = CARTESIAN_POINT ( 'NONE',  ( 24.86476902620765728, 14.75978393459164373, -1.583844403245362020 ) ) ;
#30885 = CARTESIAN_POINT ( 'NONE',  ( 162.0148977879440508, 250.0289607786390604, -13.13131188671606786 ) ) ;
#30886 = ORIENTED_EDGE ( 'NONE', *, *, #26525, .F. ) ;
#30887 = CARTESIAN_POINT ( 'NONE',  ( 83.72772921281246283, 41.65051315404114263, 0.2546602532276703301 ) ) ;
#30888 = CARTESIAN_POINT ( 'NONE',  ( 183.7401645296863819, 275.5702118650854686, 17.68276783697519505 ) ) ;
#30889 = CARTESIAN_POINT ( 'NONE',  ( -29.89096190292416821, 93.77824852085353768, 44.39154330738892895 ) ) ;
#30890 = CARTESIAN_POINT ( 'NONE',  ( 185.1790142135946837, 260.5378326486920741, -9.806357480331048038 ) ) ;
#30891 = PLANE ( 'NONE',  #7589 ) ;
#30892 = VERTEX_POINT ( 'NONE', #44873 ) ;
#30893 = CARTESIAN_POINT ( 'NONE',  ( 82.27584197377750286, 43.65791533439266203, -8.572228566050736021 ) ) ;
#30894 = CARTESIAN_POINT ( 'NONE',  ( 186.0348036264326481, 259.0250182415348945, 6.435743254585703177 ) ) ;
#30895 = CARTESIAN_POINT ( 'NONE',  ( 31.97641226934276659, 34.16454794089042935, -10.00000000000000355 ) ) ;
#30896 = CARTESIAN_POINT ( 'NONE',  ( 200.6680263064462792, 283.0797783131037022, -17.21821073473145347 ) ) ;
#30897 = CARTESIAN_POINT ( 'NONE',  ( 72.67131491517322672, 70.78719139597193077, 7.139508363488885401 ) ) ;
#30898 = CARTESIAN_POINT ( 'NONE',  ( 41.37327796571899796, 124.7191351846657028, 10.00000000000000000 ) ) ;
#30899 = VERTEX_POINT ( 'NONE', #7377 ) ;
#30900 = CARTESIAN_POINT ( 'NONE',  ( 198.9991959707468538, 266.7910966233320664, 4.538875652460267140 ) ) ;
#30901 = CARTESIAN_POINT ( 'NONE',  ( 75.43017357788674815, 188.3759306620403891, 30.52142883766498827 ) ) ;
#30902 = CARTESIAN_POINT ( 'NONE',  ( 199.0746189151364831, 265.2438329385483939, 1.559867394473611002 ) ) ;
#30903 = CARTESIAN_POINT ( 'NONE',  ( 79.83962644441906775, 47.32072031626830722, 13.19797558408899008 ) ) ;
#30904 = CARTESIAN_POINT ( 'NONE',  ( 83.78524573913310292, 52.15075186824800824, 14.63520302633205361 ) ) ;
#30905 = CARTESIAN_POINT ( 'NONE',  ( 152.9518609051173996, 270.9304444175188564, 13.97502339724686138 ) ) ;
#30906 = ORIENTED_EDGE ( 'NONE', *, *, #21787, .F. ) ;
#30907 = CARTESIAN_POINT ( 'NONE',  ( -110.0000000000000142, -8.000000000000000000, -9.212605237762117483 ) ) ;
#30908 = CARTESIAN_POINT ( 'NONE',  ( -17.46030756596911360, 103.9795007202521475, 44.59709923157863187 ) ) ;
#30909 = EDGE_CURVE ( 'NONE', #45951, #39202, #2663, .T. ) ;
#30910 = CARTESIAN_POINT ( 'NONE',  ( 205.2391015854675516, 275.1624436846170738, -14.01434138479280911 ) ) ;
#30912 = CARTESIAN_POINT ( 'NONE',  ( 73.68661752955311783, 55.32924942141305280, 16.59143442441305538 ) ) ;
#30911 = CARTESIAN_POINT ( 'NONE',  ( -47.47812815766307182, 47.92838303172833037, 59.99999999999999289 ) ) ;
#30913 = CARTESIAN_POINT ( 'NONE',  ( 23.20344070249937829, 32.13478043621388736, 8.090169943749478065 ) ) ;
#30914 = CARTESIAN_POINT ( 'NONE',  ( 171.1711017573581159, 274.6214328870215695, 17.23018440474811186 ) ) ;
#30915 = CARTESIAN_POINT ( 'NONE',  ( 165.9702209435083944, 286.5350195535361877, -3.323153172973990266 ) ) ;
#30916 = CARTESIAN_POINT ( 'NONE',  ( 32.30839531297598910, 123.0650415295850593, 203.6502102582797420 ) ) ;
#30917 = DIRECTION ( 'NONE',  ( -0.8660254037844387076, -0.4999999999999998890, -0.000000000000000000 ) ) ;
#30918 = AXIS2_PLACEMENT_3D ( 'NONE', #95441, #63970, #94913 ) ;
#30919 = CARTESIAN_POINT ( 'NONE',  ( -7.997457622663985966, 160.0643266524160140, -9.188101187500093303 ) ) ;
#30920 = B_SPLINE_CURVE_WITH_KNOTS ( 'NONE', 3,
 ( #49604, #95270, #3532, #65309 ),
 .UNSPECIFIED., .F., .F.,
 ( 4, 4 ),
 ( 0.008171099580468714138, 0.01417519103088871364 ),
 .UNSPECIFIED. ) ;
#30921 = CARTESIAN_POINT ( 'NONE',  ( 188.4688990864094080, 295.3997683978527675, -11.43812978727723717 ) ) ;
#30922 = ORIENTED_EDGE ( 'NONE', *, *, #59504, .T. ) ;
#30923 = CARTESIAN_POINT ( 'NONE',  ( 66.71451521809625262, 67.43874277882086687, -6.652223803815810577 ) ) ;
#30924 = CARTESIAN_POINT ( 'NONE',  ( 72.86429505109983040, 70.96802964124921687, -7.768747002037665439 ) ) ;
#30925 = CARTESIAN_POINT ( 'NONE',  ( 81.85952891566994083, 41.18668495682469910, 5.665119147071315808 ) ) ;
#30926 = CARTESIAN_POINT ( 'NONE',  ( 18.84898279888859918, 187.8149278399161233, 9.188101187500093303 ) ) ;
#30927 = CARTESIAN_POINT ( 'NONE',  ( 176.0882202740374964, 265.4570366886316037, -16.33249936588881823 ) ) ;
#30928 = CARTESIAN_POINT ( 'NONE',  ( 178.4436848606596300, 273.6446589788789083, -17.07804873076608843 ) ) ;
#30929 = CARTESIAN_POINT ( 'NONE',  ( 25.81463925578599117, 37.83705186507755514, 3.090169943749475401 ) ) ;
#30930 = CARTESIAN_POINT ( 'NONE',  ( 85.32181490816766711, 42.56115037135857904, -1.119015723361847181 ) ) ;
#30931 = DIRECTION ( 'NONE',  ( -0.000000000000000000, -1.000000000000000000, -0.000000000000000000 ) ) ;
#30932 = FACE_OUTER_BOUND ( 'NONE', #70022, .T. ) ;
#30933 = CARTESIAN_POINT ( 'NONE',  ( 82.08779928828076322, 42.49253994542575441, 7.931423503822311538 ) ) ;
#30934 = CARTESIAN_POINT ( 'NONE',  ( 188.9729628992022867, 259.4128536004376997, -0.8123650975293817966 ) ) ;
#30936 =( BOUNDED_CURVE ( )  B_SPLINE_CURVE ( 2, ( #71567, #2163, #79695, #10257, #2662, #4645, #43112, #11272, #19378, #41632, #87821, #19860, #3664, #88309, #57335, #18360, #5145, #4137, #49253, #88812, #57832, #34065, #64956, #18862, #49745, #95409, #80190, #74567, #74057, #42624, #50237, #73066, #80697, #3181, #35031, #95901, #10757, #72574, #81192, #26459, #82192, #65935, #42135, #34542, #65440, #96385, #26948, #11760, #58816, #73553, #96889, #27459, #43628, #64450, #58330, #89305, #25966, #56836, #50726, #81682, #12255, #35538, #66441, #27932, #97367, #89778, #20354, #51223, #12763, #59309, #75055, #52225, #29435, #60310, #13733, #44611, #90789, #68423, #5631, #21340, #44118, #75547, #67425, #91267, #6132, #76063, #83170, #91763, #6642, #99350, #37029, #36525, #67937, #28946, #37516, #98859, #21832, #97857, #14239, #52717, #14731, #68919, #83676, #45125, #99844, #7122, #29929, #98357, #60804, #76543, #59824, #22329, #30428, #53229, #84181, #45612, #77020, #61317, #38006, #92280, #22827, #53711, #13258, #84667, #15210, #46106, #36026, #66926, #90289, #28427, #20858, #51750, #82692, #78041, #79068, #38516, #16230, #17741, #70426, #78545, #39010, #1035, #94760, #41, #25324, #2034, #40511, #70944, #71446, #31913, #77547, #94266, #62818, #9133, #61811, #93774, #69916, #40004, #47618, #48123, #48641, #30926, #85691, #1548, #92761, #32921, #47120, #63825, #8137, #55209, #24332, #54709, #56210, #8632, #86190, #16726, #32431, #63326, #24822, #39499, #531, #69427, #55696, #62306, #86685, #9653, #17217, #87207, #7624, #23316, #54203, #85171, #15714, #46616, #31418, #93262, #23816, #2547, #20233, #19258, #33430, #42994, #18240, #49135, #80069, #72456, #64836, #10135, #64327, #89673, #89194, #57709, #72956, #88188, #95783, #10640, #50125, #41514, #95287, #87706, #34426, #79576, #42022, #81078, #3062, #25847, #65326, #81562, #11644, #41002, #18737, #11153, #71944, #49621, #26830, #3548, #56724, #33949, #26335, #57212, #19743, #96768, #88688, #80574, #96263, #42503, #73440, #4024, #34908, #12131, #65808, #35417, #27334, #58216, #50607, #73931, #4517, #66324, #97256, #27822, #58698, #92168, #67820, #21715, #75946, #22212, #43995, #6523, #99728, #82575, #68304, #37399, #14620, #35912, #99227, #53110, #74937, #44499, #74450, #90163, #67309, #66811, #45499, #29814, #83054, #5030, #29322, #51106, #60687, #91645, #28821, #13138, #6014, #21228, #91150, #5520, #84066, #52598, #83555, #59705, #20735, #14120, #45000, #52107, #51621, #76432, #7005, #90671, #59187, #13627, #37892, #75430, #36907, #68800, #30314, #98743, #36403, #61200, #82071, #98236, #60189, #97741, #12639, #43511, #28308, #77932, #47017, #55102, #53603, #15100, #9538, #30822, #8032, #24710, #54095, #38905, #39889, #7506, #62196, #61702, #92654, #85051, #76908, #23204, #8523, #69316, #71336, #84561, #39392, #15598, #70309, #40399, #45991, #1928, #48006, #86576, #16613, #17109, #922, #46498, #70824, #77434, #69809, #38403, #94157, #16119, #1433, #62700, #419, #100238, #31308, #93147, #93657, #23698, #78950, #54593, #32814, #85575, #31798, #24222, #86089, #47509, #78436, #63719, #94657, #32314, #9017, #63215, #55593, #41914, #26721, #95167, #72849, #42398, #64216, #3441, #34318, #88583, #79466, #11037, #57603, #10528, #2439, #87089, #18125, #10030, #40892, #19145, #65216, #72347, #17625, #26225, #25212, #96158, #50019, #79960, #25735, #64729, #41403, #71841, #80973, #11538, #73332, #3919, #56096, #18633, #48529, #33317, #56615, #57101, #87599, #49026, #2952, #33841, #95678, #88083, #49512, #80466, #86909, #8349, #8840, #7851, #62521, #62020, #31127, #9871, #63539, #47335, #38734, #93987, #15423, #71168, #1764, #93483, #46842, #70639, #85913, #55418, #70126, #32644, #86403, #24537, #16935, #63042, #47822, #78761, #16440, #85392, #9348, #71674, #24038, #23526, #78260, #48352, #39711, #54937, #79302, #17446, #1253, #54416, #40224, #32134, #39219, #739, #69638, #56441, #94481, #246, #25036, #55916, #40728, #46320, #77246, #2264, #92971, #31623, #33146, #15938, #64046, #94991, #77765, #25553, #26059, #27057, #18463, #10361, #95513, #42231, #2773, #4756, #87435, #11381, #56935, #80805, #74164, #79795, #35638, #81781, #19955, #50338, #50832, #34641, #73170, #41227, #10862, #87920, #17968, #27563, #49846, #4235, #96487, #49351, #72168, #33662, #65049, #57938, #64552, #12357, #95999, #43223, #80290, #26559, #57433, #41736, #48863, #58428, #3760, #35135, #88921, #72680, #3274, #34157, #88412, #19481, #18970, #66540, #65539, #97467, #81290, #11863, #42719, #73656, #66046, #96992, #28034, #89404, #45222, #99944, #75643, #29535, #83773, #30023, #51847, #14334, #7218, #90390, #76160, #6737, #22428, #43725, #37613, #21438, #59920, #28527, #51328, #5731, #5244, #74667, #53319, #68525, #90889, #82295, #37123, #58910, #99447, #60908, #36619, #20964, #13832, #29051, #98952, #67528, #76633, #98457, #68031, #60408, #6229, #91363, #21927, #52324, #59410, #52816, #14821, #83266, #67027, #44710, #91873, #84276, #45709, #38102, #69014, #36124, #12865, #89880, #20454, #82788, #13352, #97954, #44218, #75155, #84767, #85793, #23917, #32011, #30527, #92368, #86787, #7724, #85269, #1649, #31017, #8727, #16325, #39100, #46719, #69520, #70519, #61908, #53802, #134, #47218, #46202, #48226, #61415, #78140, #92857, #39599, #17321, #22916, #79173, #24920, #93360, #15303, #629, #1134, #62921, #77119, #54301, #77647, #93871, #23411, #15815, #86284, #70013, #8233, #31509, #24428, #71546, #55304, #16820, #47707, #78645, #9228, #40107, #71047, #32533, #63427, #94366, #40612, #55794, #80678, #95880, #10738, #18343, #41106, #42116, #33533, #25420, #10237, #57317, #17842, #64936, #73050, #64430, #48743, #88288, #4117, #3643, #63921, #41612, #34046, #94860, #72557, #49721, #26438, #56313, #25944, #72041, #2140, #42602, #18841, #34524, #73536, #12235, #96869, #56819, #35012, #87309, #11253, #3161, #65423, #96366, #2645, #26932, #89288 ),
 .UNSPECIFIED., .F., .T. ) 
 B_SPLINE_CURVE_WITH_KNOTS ( ( 3, 2, 2, 2, 2, 2, 2, 2, 2, 2, 2, 2, 2, 2, 2, 2, 2, 2, 2, 2, 2, 2, 2, 2, 2, 2, 2, 2, 2, 2, 2, 2, 2, 2, 2, 2, 2, 2, 2, 2, 2, 2, 2, 2, 2, 2, 2, 2, 2, 2, 2, 2, 2, 2, 2, 2, 2, 2, 2, 2, 2, 2, 2, 2, 2, 2, 2, 2, 2, 2, 2, 2, 2, 2, 2, 2, 2, 2, 2, 2, 2, 2, 2, 2, 2, 2, 2, 2, 2, 2, 2, 2, 2, 2, 2, 2, 2, 2, 2, 2, 2, 2, 2, 2, 2, 2, 2, 2, 2, 2, 2, 2, 2, 2, 2, 2, 2, 2, 2, 2, 2, 2, 2, 2, 2, 2, 2, 2, 2, 2, 2, 2, 2, 2, 2, 2, 2, 2, 2, 2, 2, 2, 2, 2, 2, 2, 2, 2, 2, 2, 2, 2, 2, 2, 2, 2, 2, 2, 2, 2, 2, 2, 2, 2, 2, 2, 2, 2, 2, 2, 2, 2, 2, 2, 2, 2, 2, 2, 2, 2, 2, 2, 2, 2, 2, 2, 2, 2, 2, 2, 2, 2, 2, 2, 2, 2, 2, 2, 2, 2, 2, 2, 2, 2, 2, 2, 2, 2, 2, 2, 2, 2, 2, 2, 2, 2, 2, 2, 2, 2, 2, 2, 2, 2, 2, 2, 2, 2, 2, 2, 2, 2, 2, 2, 2, 2, 2, 2, 2, 2, 2, 2, 2, 2, 2, 2, 2, 2, 2, 2, 2, 2, 2, 2, 2, 2, 2, 2, 2, 2, 2, 2, 2, 2, 2, 2, 2, 2, 2, 2, 2, 2, 2, 2, 2, 2, 2, 2, 2, 2, 2, 2, 2, 2, 2, 2, 2, 2, 2, 2, 2, 2, 2, 2, 2, 2, 2, 2, 2, 2, 2, 2, 2, 2, 2, 2, 2, 2, 2, 2, 2, 2, 2, 2, 2, 2, 2, 2, 2, 2, 2, 2, 2, 2, 2, 2, 2, 2, 2, 2, 2, 2, 2, 2, 2, 2, 2, 2, 2, 2, 2, 2, 2, 2, 2, 2, 2, 2, 2, 2, 2, 2, 2, 2, 2, 2, 2, 2, 2, 2, 2, 2, 2, 2, 2, 2, 2, 3 ),
 ( 0.000000000000000000, 0.002688172043010752903, 0.005376344086021505805, 0.008064516129032257841, 0.01075268817204301161, 0.01344086021505376365, 0.01612903225806451568, 0.01881720430107526945, 0.02150537634408602322, 0.02419354838709677352, 0.02688172043010752729, 0.02956989247311828106, 0.03225806451612903136, 0.03494623655913978166, 0.03763440860215053890, 0.04032258064516128920, 0.04301075268817204644, 0.04569892473118279674, 0.04838709677419354704, 0.05107526881720430428, 0.05376344086021505458, 0.05645161290322580488, 0.05913978494623656212, 0.06182795698924731242, 0.06451612903225806273, 0.06720430107526881303, 0.06989247311827956333, 0.07258064516129032751, 0.07526881720430107781, 0.07795698924731182811, 0.08064516129032257841, 0.08333333333333332871, 0.08602150537634409289, 0.08870967741935484319, 0.09139784946236559349, 0.09408602150537634379, 0.09677419354838709409, 0.09946236559139784439, 0.1021505376344086086, 0.1048387096774193589, 0.1075268817204301092, 0.1102150537634408595, 0.1129032258064516098, 0.1155913978494623601, 0.1182795698924731242, 0.1209677419354838745, 0.1236559139784946248, 0.1263440860215053752, 0.1290322580645161255, 0.1317204301075268758, 0.1344086021505376261, 0.1370967741935483764, 0.1397849462365591267, 0.1424731182795699047, 0.1451612903225806550, 0.1478494623655914053, 0.1505376344086021556, 0.1532258064516129059, 0.1559139784946236562, 0.1586021505376344065, 0.1612903225806451568, 0.1639784946236559071, 0.1666666666666666574, 0.1693548387096774077, 0.1720430107526881858, 0.1747311827956989361, 0.1774193548387096864, 0.1801075268817204367, 0.1827956989247311870, 0.1854838709677419373, 0.1881720430107526876, 0.1908602150537634379, 0.1935483870967741882, 0.1962365591397849385, 0.1989247311827956888, 0.2016129032258064391, 0.2043010752688172171, 0.2069892473118279674, 0.2096774193548387177, 0.2123655913978494680, 0.2150537634408602183, 0.2177419354838709686, 0.2204301075268817189, 0.2231182795698924692, 0.2258064516129032195, 0.2284946236559139698, 0.2311827956989247201, 0.2338709677419354704, 0.2365591397849462485, 0.2392473118279569988, 0.2419354838709677491, 0.2446236559139784994, 0.2473118279569892497, 0.2500000000000000000, 0.2526881720430107503, 0.2553763440860215006, 0.2580645161290322509, 0.2607526881720430012, 0.2634408602150537515, 0.2661290322580645018, 0.2688172043010752521, 0.2715053763440860024, 0.2741935483870967527, 0.2768817204301075030, 0.2795698924731182533, 0.2822580645161290591, 0.2849462365591398094, 0.2876344086021505597, 0.2903225806451613100, 0.2930107526881720603, 0.2956989247311828106, 0.2983870967741935609, 0.3010752688172043112, 0.3037634408602150615, 0.3064516129032258118, 0.3091397849462365621, 0.3118279569892473124, 0.3145161290322580627, 0.3172043010752688130, 0.3198924731182795633, 0.3225806451612903136, 0.3252688172043010639, 0.3279569892473118142, 0.3306451612903225645, 0.3333333333333333148, 0.3360215053763440651, 0.3387096774193548154, 0.3413978494623655657, 0.3440860215053763715, 0.3467741935483871218, 0.3494623655913978721, 0.3521505376344086224, 0.3548387096774193727, 0.3575268817204301230, 0.3602150537634408733, 0.3629032258064516236, 0.3655913978494623739, 0.3682795698924731242, 0.3709677419354838745, 0.3736559139784946248, 0.3763440860215053752, 0.3790322580645161255, 0.3817204301075268758, 0.3844086021505376261, 0.3870967741935483764, 0.3897849462365591267, 0.3924731182795698770, 0.3951612903225806273, 0.3978494623655913776, 0.4005376344086021279, 0.4032258064516128782, 0.4059139784946236285, 0.4086021505376344343, 0.4112903225806451846, 0.4139784946236559349, 0.4166666666666666852, 0.4193548387096774355, 0.4220430107526881858, 0.4247311827956989361, 0.4274193548387096864, 0.4301075268817204367, 0.4327956989247311870, 0.4354838709677419373, 0.4381720430107526876, 0.4408602150537634379, 0.4435483870967741882, 0.4462365591397849385, 0.4489247311827956888, 0.4516129032258064391, 0.4543010752688171894, 0.4569892473118279397, 0.4596774193548386900, 0.4623655913978494403, 0.4650537634408601906, 0.4677419354838709409, 0.4704301075268817467, 0.4731182795698924970, 0.4758064516129032473, 0.4784946236559139976, 0.4811827956989247479, 0.4838709677419354982, 0.4865591397849462485, 0.4892473118279569988, 0.4919354838709677491, 0.4946236559139784994, 0.4973118279569892497, 0.5000000000000000000, 0.5026881720430107503, 0.5053763440860215006, 0.5080645161290322509, 0.5107526881720430012, 0.5134408602150537515, 0.5161290322580645018, 0.5188172043010752521, 0.5215053763440860024, 0.5241935483870967527, 0.5268817204301075030, 0.5295698924731182533, 0.5322580645161290036, 0.5349462365591397539, 0.5376344086021505042, 0.5403225806451612545, 0.5430107526881720048, 0.5456989247311827551, 0.5483870967741935054, 0.5510752688172042557, 0.5537634408602150060, 0.5564516129032257563, 0.5591397849462365066, 0.5618279569892472569, 0.5645161290322581182, 0.5672043010752688685, 0.5698924731182796188, 0.5725806451612903691, 0.5752688172043011194, 0.5779569892473118697, 0.5806451612903226200, 0.5833333333333333703, 0.5860215053763441206, 0.5887096774193548709, 0.5913978494623656212, 0.5940860215053763715, 0.5967741935483871218, 0.5994623655913978721, 0.6021505376344086224, 0.6048387096774193727, 0.6075268817204301230, 0.6102150537634408733, 0.6129032258064516236, 0.6155913978494623739, 0.6182795698924731242, 0.6209677419354838745, 0.6236559139784946248, 0.6263440860215053752, 0.6290322580645161255, 0.6317204301075268758, 0.6344086021505376261, 0.6370967741935483764, 0.6397849462365591267, 0.6424731182795698770, 0.6451612903225806273, 0.6478494623655913776, 0.6505376344086021279, 0.6532258064516128782, 0.6559139784946236285, 0.6586021505376343788, 0.6612903225806451291, 0.6639784946236558794, 0.6666666666666666297, 0.6693548387096773800, 0.6720430107526881303, 0.6747311827956988806, 0.6774193548387096309, 0.6801075268817203812, 0.6827956989247311315, 0.6854838709677418818, 0.6881720430107527431, 0.6908602150537634934, 0.6935483870967742437, 0.6962365591397849940, 0.6989247311827957443, 0.7016129032258064946, 0.7043010752688172449, 0.7069892473118279952, 0.7096774193548387455, 0.7123655913978494958, 0.7150537634408602461, 0.7177419354838709964, 0.7204301075268817467, 0.7231182795698924970, 0.7258064516129032473, 0.7284946236559139976, 0.7311827956989247479, 0.7338709677419354982, 0.7365591397849462485, 0.7392473118279569988, 0.7419354838709677491, 0.7446236559139784994, 0.7473118279569892497, 0.7500000000000000000, 0.7526881720430107503, 0.7553763440860215006, 0.7580645161290322509, 0.7607526881720430012, 0.7634408602150537515, 0.7661290322580645018, 0.7688172043010752521, 0.7715053763440860024, 0.7741935483870967527, 0.7768817204301075030, 0.7795698924731182533, 0.7822580645161290036, 0.7849462365591397539, 0.7876344086021505042, 0.7903225806451612545, 0.7930107526881720048, 0.7956989247311827551, 0.7983870967741935054, 0.8010752688172042557, 0.8037634408602150060, 0.8064516129032257563, 0.8091397849462365066, 0.8118279569892472569, 0.8145161290322581182, 0.8172043010752688685, 0.8198924731182796188, 0.8225806451612903691, 0.8252688172043011194, 0.8279569892473118697, 0.8306451612903226200, 0.8333333333333333703, 0.8360215053763441206, 0.8387096774193548709, 0.8413978494623656212, 0.8440860215053763715, 0.8467741935483871218, 0.8494623655913978721, 0.8521505376344086224, 0.8548387096774193727, 0.8575268817204301230, 0.8602150537634408733, 0.8629032258064516236, 0.8655913978494623739, 0.8682795698924731242, 0.8709677419354838745, 0.8736559139784946248, 0.8763440860215053752, 0.8790322580645161255, 0.8817204301075268758, 0.8844086021505376261, 0.8870967741935483764, 0.8897849462365591267, 0.8924731182795698770, 0.8951612903225806273, 0.8978494623655913776, 0.9005376344086021279, 0.9032258064516128782, 0.9059139784946236285, 0.9086021505376343788, 0.9112903225806451291, 0.9139784946236558794, 0.9166666666666666297, 0.9193548387096773800, 0.9220430107526881303, 0.9247311827956988806, 0.9274193548387096309, 0.9301075268817203812, 0.9327956989247311315, 0.9354838709677418818, 0.9381720430107527431, 0.9408602150537634934, 0.9435483870967742437, 0.9462365591397849940, 0.9489247311827957443, 0.9516129032258064946, 0.9543010752688172449, 0.9569892473118279952, 0.9596774193548387455, 0.9623655913978494958, 0.9650537634408602461, 0.9677419354838709964, 0.9704301075268817467, 0.9731182795698924970, 0.9758064516129032473, 0.9784946236559139976, 0.9811827956989247479, 0.9838709677419354982, 0.9855363728105643872 ),
 .UNSPECIFIED. ) 
 CURVE ( )  GEOMETRIC_REPRESENTATION_ITEM ( )  RATIONAL_B_SPLINE_CURVE ( ( 1.000000000000000000, 0.8660254037844387076, 1.000000000000000000, 0.8660254037844387076, 1.000000000000000000, 0.8660254037844387076, 1.000000000000000000, 0.8660254037844387076, 1.000000000000000000, 0.8660254037844387076, 1.000000000000000000, 0.8660254037844387076, 1.000000000000000000, 0.8660254037844387076, 1.000000000000000000, 0.8660254037844387076, 1.000000000000000000, 0.8660254037844387076, 1.000000000000000000, 0.8660254037844387076, 1.000000000000000000, 0.8660254037844387076, 1.000000000000000000, 0.8660254037844387076, 1.000000000000000000, 0.8660254037844387076, 1.000000000000000000, 0.8660254037844387076, 1.000000000000000000, 0.8660254037844387076, 1.000000000000000000, 0.8660254037844387076, 1.000000000000000000, 0.8660254037844387076, 1.000000000000000000, 0.8660254037844387076, 1.000000000000000000, 0.8660254037844387076, 1.000000000000000000, 0.8660254037844387076, 1.000000000000000000, 0.8660254037844387076, 1.000000000000000000, 0.8660254037844387076, 1.000000000000000000, 0.8660254037844387076, 1.000000000000000000, 0.8660254037844387076, 1.000000000000000000, 0.8660254037844387076, 1.000000000000000000, 0.8660254037844387076, 1.000000000000000000, 0.8660254037844387076, 1.000000000000000000, 0.8660254037844387076, 1.000000000000000000, 0.8660254037844387076, 1.000000000000000000, 0.8660254037844387076, 1.000000000000000000, 0.8660254037844387076, 1.000000000000000000, 0.8660254037844387076, 1.000000000000000000, 0.8660254037844387076, 1.000000000000000000, 0.8660254037844387076, 1.000000000000000000, 0.8660254037844387076, 1.000000000000000000, 0.8660254037844387076, 1.000000000000000000, 0.8660254037844387076, 1.000000000000000000, 0.8660254037844387076, 1.000000000000000000, 0.8660254037844387076, 1.000000000000000000, 0.8660254037844387076, 1.000000000000000000, 0.8660254037844387076, 1.000000000000000000, 0.8660254037844387076, 1.000000000000000000, 0.8660254037844387076, 1.000000000000000000, 0.8660254037844387076, 1.000000000000000000, 0.8660254037844387076, 1.000000000000000000, 0.8660254037844387076, 1.000000000000000000, 0.8660254037844387076, 1.000000000000000000, 0.8660254037844387076, 1.000000000000000000, 0.8660254037844387076, 1.000000000000000000, 0.8660254037844387076, 1.000000000000000000, 0.8660254037844387076, 1.000000000000000000, 0.8660254037844387076, 1.000000000000000000, 0.8660254037844387076, 1.000000000000000000, 0.8660254037844387076, 1.000000000000000000, 0.8660254037844387076, 1.000000000000000000, 0.8660254037844387076, 1.000000000000000000, 0.8660254037844387076, 1.000000000000000000, 0.8660254037844387076, 1.000000000000000000, 0.8660254037844387076, 1.000000000000000000, 0.8660254037844387076, 1.000000000000000000, 0.8660254037844387076, 1.000000000000000000, 0.8660254037844387076, 1.000000000000000000, 0.8660254037844387076, 1.000000000000000000, 0.8660254037844387076, 1.000000000000000000, 0.8660254037844387076, 1.000000000000000000, 0.8660254037844387076, 1.000000000000000000, 0.8660254037844387076, 1.000000000000000000, 0.8660254037844387076, 1.000000000000000000, 0.8660254037844387076, 1.000000000000000000, 0.8660254037844387076, 1.000000000000000000, 0.8660254037844387076, 1.000000000000000000, 0.8660254037844387076, 1.000000000000000000, 0.8660254037844387076, 1.000000000000000000, 0.8660254037844387076, 1.000000000000000000, 0.8660254037844387076, 1.000000000000000000, 0.8660254037844387076, 1.000000000000000000, 0.8660254037844387076, 1.000000000000000000, 0.8660254037844387076, 1.000000000000000000, 0.8660254037844387076, 1.000000000000000000, 0.8660254037844387076, 1.000000000000000000, 0.8660254037844387076, 1.000000000000000000, 0.8660254037844387076, 1.000000000000000000, 0.8660254037844387076, 1.000000000000000000, 0.8660254037844387076, 1.000000000000000000, 0.8660254037844387076, 1.000000000000000000, 0.8660254037844387076, 1.000000000000000000, 0.8660254037844387076, 1.000000000000000000, 0.8660254037844387076, 1.000000000000000000, 0.8660254037844387076, 1.000000000000000000, 0.8660254037844387076, 1.000000000000000000, 0.8660254037844387076, 1.000000000000000000, 0.8660254037844387076, 1.000000000000000000, 0.8660254037844387076, 1.000000000000000000, 0.8660254037844387076, 1.000000000000000000, 0.8660254037844387076, 1.000000000000000000, 0.8660254037844387076, 1.000000000000000000, 0.8660254037844387076, 1.000000000000000000, 0.8660254037844387076, 1.000000000000000000, 0.8660254037844387076, 1.000000000000000000, 0.8660254037844387076, 1.000000000000000000, 0.8660254037844387076, 1.000000000000000000, 0.8660254037844387076, 1.000000000000000000, 0.8660254037844387076, 1.000000000000000000, 0.8660254037844387076, 1.000000000000000000, 0.8660254037844387076, 1.000000000000000000, 0.8660254037844387076, 1.000000000000000000, 0.8660254037844387076, 1.000000000000000000, 0.8660254037844387076, 1.000000000000000000, 0.8660254037844387076, 1.000000000000000000, 0.8660254037844387076, 1.000000000000000000, 0.8660254037844387076, 1.000000000000000000, 0.8660254037844387076, 1.000000000000000000, 0.8660254037844387076, 1.000000000000000000, 0.8660254037844387076, 1.000000000000000000, 0.8660254037844387076, 1.000000000000000000, 0.8660254037844387076, 1.000000000000000000, 0.8660254037844387076, 1.000000000000000000, 0.8660254037844387076, 1.000000000000000000, 0.8660254037844387076, 1.000000000000000000, 0.8660254037844387076, 1.000000000000000000, 0.8660254037844387076, 1.000000000000000000, 0.8660254037844387076, 1.000000000000000000, 0.8660254037844387076, 1.000000000000000000, 0.8660254037844387076, 1.000000000000000000, 0.8660254037844387076, 1.000000000000000000, 0.8660254037844387076, 1.000000000000000000, 0.8660254037844387076, 1.000000000000000000, 0.8660254037844387076, 1.000000000000000000, 0.8660254037844387076, 1.000000000000000000, 0.8660254037844387076, 1.000000000000000000, 0.8660254037844387076, 1.000000000000000000, 0.8660254037844387076, 1.000000000000000000, 0.8660254037844387076, 1.000000000000000000, 0.8660254037844387076, 1.000000000000000000, 0.8660254037844387076, 1.000000000000000000, 0.8660254037844387076, 1.000000000000000000, 0.8660254037844387076, 1.000000000000000000, 0.8660254037844387076, 1.000000000000000000, 0.8660254037844387076, 1.000000000000000000, 0.8660254037844387076, 1.000000000000000000, 0.8660254037844387076, 1.000000000000000000, 0.8660254037844387076, 1.000000000000000000, 0.8660254037844387076, 1.000000000000000000, 0.8660254037844387076, 1.000000000000000000, 0.8660254037844387076, 1.000000000000000000, 0.8660254037844387076, 1.000000000000000000, 0.8660254037844387076, 1.000000000000000000, 0.8660254037844387076, 1.000000000000000000, 0.8660254037844387076, 1.000000000000000000, 0.8660254037844387076, 1.000000000000000000, 0.8660254037844387076, 1.000000000000000000, 0.8660254037844387076, 1.000000000000000000, 0.8660254037844387076, 1.000000000000000000, 0.8660254037844387076, 1.000000000000000000, 0.8660254037844387076, 1.000000000000000000, 0.8660254037844387076, 1.000000000000000000, 0.8660254037844387076, 1.000000000000000000, 0.8660254037844387076, 1.000000000000000000, 0.8660254037844387076, 1.000000000000000000, 0.8660254037844387076, 1.000000000000000000, 0.8660254037844387076, 1.000000000000000000, 0.8660254037844387076, 1.000000000000000000, 0.8660254037844387076, 1.000000000000000000, 0.8660254037844387076, 1.000000000000000000, 0.8660254037844387076, 1.000000000000000000, 0.8660254037844387076, 1.000000000000000000, 0.8660254037844387076, 1.000000000000000000, 0.8660254037844387076, 1.000000000000000000, 0.8660254037844387076, 1.000000000000000000, 0.8660254037844387076, 1.000000000000000000, 0.8660254037844387076, 1.000000000000000000, 0.8660254037844387076, 1.000000000000000000, 0.8660254037844387076, 1.000000000000000000, 0.8660254037844387076, 1.000000000000000000, 0.8660254037844387076, 1.000000000000000000, 0.8660254037844387076, 1.000000000000000000, 0.8660254037844387076, 1.000000000000000000, 0.8660254037844387076, 1.000000000000000000, 0.8660254037844387076, 1.000000000000000000, 0.8660254037844387076, 1.000000000000000000, 0.8660254037844387076, 1.000000000000000000, 0.8660254037844387076, 1.000000000000000000, 0.8660254037844387076, 1.000000000000000000, 0.8660254037844387076, 1.000000000000000000, 0.8660254037844387076, 1.000000000000000000, 0.8660254037844387076, 1.000000000000000000, 0.8660254037844387076, 1.000000000000000000, 0.8660254037844387076, 1.000000000000000000, 0.8660254037844387076, 1.000000000000000000, 0.8660254037844387076, 1.000000000000000000, 0.8660254037844387076, 1.000000000000000000, 0.8660254037844387076, 1.000000000000000000, 0.8660254037844387076, 1.000000000000000000, 0.8660254037844387076, 1.000000000000000000, 0.8660254037844387076, 1.000000000000000000, 0.8660254037844387076, 1.000000000000000000, 0.8660254037844387076, 1.000000000000000000, 0.8660254037844387076, 1.000000000000000000, 0.8660254037844387076, 1.000000000000000000, 0.8660254037844387076, 1.000000000000000000, 0.8660254037844387076, 1.000000000000000000, 0.8660254037844387076, 1.000000000000000000, 0.8660254037844387076, 1.000000000000000000, 0.8660254037844387076, 1.000000000000000000, 0.8660254037844387076, 1.000000000000000000, 0.8660254037844387076, 1.000000000000000000, 0.8660254037844387076, 1.000000000000000000, 0.8660254037844387076, 1.000000000000000000, 0.8660254037844387076, 1.000000000000000000, 0.8660254037844387076, 1.000000000000000000, 0.8660254037844387076, 1.000000000000000000, 0.8660254037844387076, 1.000000000000000000, 0.8660254037844387076, 1.000000000000000000, 0.8660254037844387076, 1.000000000000000000, 0.8660254037844387076, 1.000000000000000000, 0.8660254037844387076, 1.000000000000000000, 0.8660254037844387076, 1.000000000000000000, 0.8660254037844387076, 1.000000000000000000, 0.8660254037844387076, 1.000000000000000000, 0.8660254037844387076, 1.000000000000000000, 0.8660254037844387076, 1.000000000000000000, 0.8660254037844387076, 1.000000000000000000, 0.8660254037844387076, 1.000000000000000000, 0.8660254037844387076, 1.000000000000000000, 0.8660254037844387076, 1.000000000000000000, 0.8660254037844387076, 1.000000000000000000, 0.8660254037844387076, 1.000000000000000000, 0.8660254037844387076, 1.000000000000000000, 0.8660254037844387076, 1.000000000000000000, 0.8660254037844387076, 1.000000000000000000, 0.8660254037844387076, 1.000000000000000000, 0.8660254037844387076, 1.000000000000000000, 0.8660254037844387076, 1.000000000000000000, 0.8660254037844387076, 1.000000000000000000, 0.8660254037844387076, 1.000000000000000000, 0.8660254037844387076, 1.000000000000000000, 0.8660254037844387076, 1.000000000000000000, 0.8660254037844387076, 1.000000000000000000, 0.8660254037844387076, 1.000000000000000000, 0.8660254037844387076, 1.000000000000000000, 0.8660254037844387076, 1.000000000000000000, 0.8660254037844387076, 1.000000000000000000, 0.8660254037844387076, 1.000000000000000000, 0.8660254037844387076, 1.000000000000000000, 0.8660254037844387076, 1.000000000000000000, 0.8660254037844387076, 1.000000000000000000, 0.8660254037844387076, 1.000000000000000000, 0.8660254037844387076, 1.000000000000000000, 0.8660254037844387076, 1.000000000000000000, 0.8660254037844387076, 1.000000000000000000, 0.8660254037844387076, 1.000000000000000000, 0.8660254037844387076, 1.000000000000000000, 0.8660254037844387076, 1.000000000000000000, 0.8660254037844387076, 1.000000000000000000, 0.8660254037844387076, 1.000000000000000000, 0.8660254037844387076, 1.000000000000000000, 0.8660254037844387076, 1.000000000000000000, 0.8660254037844387076, 1.000000000000000000, 0.8660254037844387076, 1.000000000000000000, 0.8660254037844387076, 1.000000000000000000, 0.8660254037844387076, 1.000000000000000000, 0.8660254037844387076, 1.000000000000000000, 0.8660254037844387076, 1.000000000000000000, 0.8660254037844387076, 1.000000000000000000, 0.8660254037844387076, 1.000000000000000000, 0.8660254037844387076, 1.000000000000000000, 0.8660254037844387076, 1.000000000000000000, 0.8660254037844387076, 1.000000000000000000, 0.8660254037844387076, 1.000000000000000000, 0.8660254037844387076, 1.000000000000000000, 0.8660254037844387076, 1.000000000000000000, 0.8660254037844387076, 1.000000000000000000, 0.8660254037844387076, 1.000000000000000000, 0.8660254037844387076, 1.000000000000000000, 0.8660254037844387076, 1.000000000000000000, 0.8660254037844387076, 1.000000000000000000, 0.8660254037844387076, 1.000000000000000000, 0.8660254037844387076, 1.000000000000000000, 0.8660254037844387076, 1.000000000000000000, 0.8660254037844387076, 1.000000000000000000, 0.8660254037844387076, 1.000000000000000000, 0.8660254037844387076, 1.000000000000000000, 0.8660254037844387076, 1.000000000000000000, 0.8660254037844387076, 1.000000000000000000, 0.8660254037844387076, 1.000000000000000000, 0.8660254037844387076, 1.000000000000000000, 0.8660254037844387076, 1.000000000000000000, 0.8660254037844387076, 1.000000000000000000, 0.8660254037844387076, 1.000000000000000000, 0.8660254037844387076, 1.000000000000000000, 0.8660254037844387076, 1.000000000000000000, 0.8660254037844387076, 1.000000000000000000, 0.8660254037844387076, 1.000000000000000000, 0.8660254037844387076, 1.000000000000000000, 0.8660254037844387076, 1.000000000000000000, 0.8660254037844387076, 1.000000000000000000, 0.8660254037844387076, 1.000000000000000000, 0.8660254037844387076, 1.000000000000000000, 0.8660254037844387076, 1.000000000000000000, 0.8660254037844387076, 1.000000000000000000, 0.8660254037844387076, 1.000000000000000000, 0.8660254037844387076, 1.000000000000000000, 0.8660254037844387076, 1.000000000000000000, 0.8660254037844387076, 1.000000000000000000, 0.8660254037844387076, 1.000000000000000000, 0.8660254037844387076, 1.000000000000000000, 0.8660254037844387076, 1.000000000000000000, 0.8660254037844387076, 1.000000000000000000, 0.8660254037844387076, 1.000000000000000000, 0.8660254037844387076, 1.000000000000000000, 0.8660254037844387076, 1.000000000000000000, 0.8660254037844387076, 1.000000000000000000, 0.8660254037844387076, 1.000000000000000000, 0.8660254037844387076, 1.000000000000000000, 0.8660254037844387076, 1.000000000000000000, 0.8660254037844387076, 1.000000000000000000, 0.8660254037844387076, 1.000000000000000000, 0.8660254037844387076, 1.000000000000000000, 0.8660254037844387076, 1.000000000000000000, 0.8660254037844387076, 1.000000000000000000, 0.8660254037844387076, 1.000000000000000000, 0.8660254037844387076, 1.000000000000000000, 0.8660254037844387076, 1.000000000000000000, 0.8660254037844387076, 1.000000000000000000, 0.8660254037844387076, 1.000000000000000000, 0.8660254037844387076, 1.000000000000000000, 0.8660254037844387076, 1.000000000000000000, 0.8660254037844387076, 1.000000000000000000, 0.8660254037844387076, 1.000000000000000000, 0.8660254037844387076, 1.000000000000000000, 0.8660254037844387076, 1.000000000000000000, 0.8660254037844387076, 1.000000000000000000, 0.8660254037844387076, 1.000000000000000000, 0.8660254037844387076, 1.000000000000000000, 0.8660254037844387076, 1.000000000000000000, 0.8660254037844387076, 1.000000000000000000, 0.8660254037844387076, 1.000000000000000000, 0.8660254037844387076, 1.000000000000000000, 0.8660254037844387076, 1.000000000000000000, 0.8660254037844387076, 1.000000000000000000, 0.8660254037844387076, 1.000000000000000000, 0.8660254037844387076, 1.000000000000000000, 0.8660254037844387076, 1.000000000000000000, 0.8660254037844387076, 1.000000000000000000, 0.8660254037844387076, 1.000000000000000000, 0.8660254037844387076, 1.000000000000000000, 0.8660254037844387076, 1.000000000000000000, 0.8660254037844387076, 1.000000000000000000, 0.8660254037844387076, 1.000000000000000000, 0.8660254037844387076, 1.000000000000000000, 0.8660254037844387076, 1.000000000000000000, 0.8660254037844387076, 1.000000000000000000, 0.8660254037844387076, 1.000000000000000000, 0.8660254037844387076, 1.000000000000000000, 0.8660254037844387076, 1.000000000000000000, 0.8660254037844387076, 1.000000000000000000, 0.8660254037844387076, 1.000000000000000000, 0.8660254037844387076, 1.000000000000000000, 0.8660254037844387076, 1.000000000000000000, 0.8660254037844387076, 1.000000000000000000, 0.8660254037844387076, 1.000000000000000000, 0.8660254037844387076, 1.000000000000000000, 0.8660254037844387076, 1.000000000000000000, 0.8660254037844387076, 1.000000000000000000, 0.8660254037844387076, 1.000000000000000000, 0.8660254037844387076, 1.000000000000000000, 0.9169986265629754829, 0.9368410486966849415 ) ) 
 REPRESENTATION_ITEM ( '' )  );
#30935 = CARTESIAN_POINT ( 'NONE',  ( 65.98439316910437924, 202.2365022471902023, 10.00000000000009592 ) ) ;
#30937 = CARTESIAN_POINT ( 'NONE',  ( 167.9496373820661290, 248.6204696539478789, -6.517719931589019744 ) ) ;
#30938 = CARTESIAN_POINT ( 'NONE',  ( 72.41389820116259557, 70.72247311216293042, 7.745007521649655224 ) ) ;
#30939 = CARTESIAN_POINT ( 'NONE',  ( 33.57141466322406131, 196.3149278399160949, -9.188101187500095079 ) ) ;
#30940 = CARTESIAN_POINT ( 'NONE',  ( 72.62340041749851594, 70.70648146094340802, -7.965908336710430859 ) ) ;
#30941 = CARTESIAN_POINT ( 'NONE',  ( 32.37774987120970849, 30.64441083166263269, -10.00000000000000533 ) ) ;
#30942 = CARTESIAN_POINT ( 'NONE',  ( 203.3114313796560282, 269.4513687231070662, -5.937407854999036338 ) ) ;
#30943 = DIRECTION ( 'NONE',  ( -0.000000000000000000, -0.000000000000000000, -1.000000000000000000 ) ) ;
#30944 = DIRECTION ( 'NONE',  ( -0.000000000000000000, 0.000000000000000000, -1.000000000000000000 ) ) ;
#30945 = DIRECTION ( 'NONE',  ( -0.4999999999999982792, 0.8660254037844398178, 0.000000000000000000 ) ) ;
#30946 = CARTESIAN_POINT ( 'NONE',  ( 159.8715144876434238, 278.4871566375445582, -9.860745765539576269 ) ) ;
#30947 = DIRECTION ( 'NONE',  ( -0.3402761906661169178, -0.9403255362191097477, 0.000000000000000000 ) ) ;
#30948 = CARTESIAN_POINT ( 'NONE',  ( 24.30746885452586525, 16.96004757982090183, -5.678558825948276656 ) ) ;
#30949 = CARTESIAN_POINT ( 'NONE',  ( 44.28334795397206847, 122.1950543691075808, 10.00000000000000000 ) ) ;
#30950 = CARTESIAN_POINT ( 'NONE',  ( 72.02510489751692546, 59.23144522310215621, 15.85746550207202077 ) ) ;
#30951 = CARTESIAN_POINT ( 'NONE',  ( 188.8167911736601354, 269.9502213024455841, -14.08247674505766867 ) ) ;
#30952 = ORIENTED_EDGE ( 'NONE', *, *, #22000, .F. ) ;
#30953 = CARTESIAN_POINT ( 'NONE',  ( 3.154811933878272523, 22.79752408145589371, -5.678558825948271327 ) ) ;
#30954 = CARTESIAN_POINT ( 'NONE',  ( 71.71174882302004505, 58.93038559421764688, -15.88944412480316970 ) ) ;
#30955 = CARTESIAN_POINT ( 'NONE',  ( 88.24655134174822990, 44.28719395207696863, 2.070298746488927755 ) ) ;
#30956 = ORIENTED_EDGE ( 'NONE', *, *, #39468, .T. ) ;
#30957 = CARTESIAN_POINT ( 'NONE',  ( 207.8575108622103755, 270.6272257822888037, -6.381720258959569847 ) ) ;
#30959 = EDGE_CURVE ( 'NONE', #95124, #25119, #46041, .T. ) ;
#30958 = CARTESIAN_POINT ( 'NONE',  ( 174.6066048939933921, 262.0940252294753918, 15.79829227059981278 ) ) ;
#30960 = CARTESIAN_POINT ( 'NONE',  ( 72.52865609843787809, 57.51546068812135815, 16.29679984377914437 ) ) ;
#30961 = CARTESIAN_POINT ( 'NONE',  ( 181.2335612792182076, 257.5653981390558442, -7.611125781952750025 ) ) ;
#30962 = EDGE_CURVE ( 'NONE', #33084, #47394, #70168, .T. ) ;
#30963 = VERTEX_POINT ( 'NONE', #282 ) ;
#30964 = EDGE_LOOP ( 'NONE', ( #53773, #60367, #38575, #24233, #75980, #60507, #33091, #37118, #75665, #95309, #84891, #58327 ) ) ;
#30965 = DIRECTION ( 'NONE',  ( -0.9879014915521923124, 0.1550826972584425645, 0.000000000000000000 ) ) ;
#30966 = VERTEX_POINT ( 'NONE', #62058 ) ;
#30967 = CARTESIAN_POINT ( 'NONE',  ( 153.3544108199959908, 265.0293642254135307, -17.49105661178601423 ) ) ;
#30968 = DIRECTION ( 'NONE',  ( -0.6681572590663601430, 0.7440200784635646603, 0.000000000000000000 ) ) ;
#30969 = CARTESIAN_POINT ( 'NONE',  ( 201.1945576647943312, 267.4339689888946054, -5.629323321537795799 ) ) ;
#30970 = CARTESIAN_POINT ( 'NONE',  ( 44.85937643310610667, 116.8208962945185050, -10.00000000000000000 ) ) ;
#30971 = EDGE_LOOP ( 'NONE', ( #6031, #70977, #85231, #76588 ) ) ;
#30973 = EDGE_CURVE ( 'NONE', #43772, #20667, #93009, .T. ) ;
#30972 = CARTESIAN_POINT ( 'NONE',  ( 147.6121581866023007, 274.9752375363476631, 8.700660424766859080 ) ) ;
#30974 = ORIENTED_EDGE ( 'NONE', *, *, #30909, .F. ) ;
#30975 = CARTESIAN_POINT ( 'NONE',  ( 157.2168982216852555, 258.3393398020932636, 18.09635675623264106 ) ) ;
#30976 = B_SPLINE_CURVE_WITH_KNOTS ( 'NONE', 3,
 ( #8440, #60616, #46935, #23120, #37823, #15515, #55023, #86004, #47427, #39309, #38822, #99655, #30241, #38323 ),
 .UNSPECIFIED., .F., .F.,
 ( 4, 2, 2, 2, 2, 2, 4 ),
 ( 2.792110050598545343E-17, 0.0004826660903813697365, 0.0007239991355720011264, 0.0009653321807626326790, 0.001206665225953264123, 0.001447998271143895567, 0.001930664361525126363 ),
 .UNSPECIFIED. ) ;
#30977 = CARTESIAN_POINT ( 'NONE',  ( 158.2129804214947058, 265.2348010298870236, 17.61986633405762603 ) ) ;
#30978 = ORIENTED_EDGE ( 'NONE', *, *, #1583, .F. ) ;
#30979 = CARTESIAN_POINT ( 'NONE',  ( 33.05914333415502426, 24.80170272979928470, 7.433330006724137462 ) ) ;
#30980 = CARTESIAN_POINT ( 'NONE',  ( 149.4539134692060145, 271.7852238117696402, 12.95627816374690688 ) ) ;
#30981 = CARTESIAN_POINT ( 'NONE',  ( 78.32728443519724237, 47.41824214893080836, -13.74674985590325171 ) ) ;
#30982 = ORIENTED_EDGE ( 'NONE', *, *, #66201, .F. ) ;
#30983 = B_SPLINE_CURVE_WITH_KNOTS ( 'NONE', 3,
 ( #18861, #64449, #95408, #26458, #56835, #87820, #88308 ),
 .UNSPECIFIED., .F., .F.,
 ( 4, 3, 4 ),
 ( 0.000000000000000000, 0.001498044985889790620, 0.001795433657425995512 ),
 .UNSPECIFIED. ) ;
#30984 = CARTESIAN_POINT ( 'NONE',  ( -9.237615305844807168, 72.36688712545108615, 14.94757194756781793 ) ) ;
#30985 = CARTESIAN_POINT ( 'NONE',  ( 143.0969038086192597, 260.4263049900483225, -7.951529393128359935 ) ) ;
#30986 = CARTESIAN_POINT ( 'NONE',  ( 30.05588850504797449, 78.74034736131613954, 59.99999999999999289 ) ) ;
#30987 = CARTESIAN_POINT ( 'NONE',  ( 31.59942275858663407, 40.01751292744058475, 6.180339887498949913 ) ) ;
#30988 = ORIENTED_EDGE ( 'NONE', *, *, #77016, .F. ) ;
#30989 = AXIS2_PLACEMENT_3D ( 'NONE', #61825, #83692, #22841 ) ;
#30990 = ORIENTED_EDGE ( 'NONE', *, *, #43523, .T. ) ;
#30991 = CARTESIAN_POINT ( 'NONE',  ( 190.6384534477846557, 299.7466497614934156, 5.268453997566757252 ) ) ;
#30992 = CARTESIAN_POINT ( 'NONE',  ( 82.61830983956946284, 42.72265058836246254, -6.751676072530465866 ) ) ;
#30993 = CARTESIAN_POINT ( 'NONE',  ( 37.13585574571499848, 81.55128318896728956, 59.99999999999999289 ) ) ;
#30994 = CARTESIAN_POINT ( 'NONE',  ( 148.9275518150011806, 272.6969089400084272, 12.34519124974546500 ) ) ;
#30995 = CARTESIAN_POINT ( 'NONE',  ( 173.8450891585409011, 276.9012038130899214, -15.64775106871585031 ) ) ;
#30996 = FACE_OUTER_BOUND ( 'NONE', #44569, .T. ) ;
#30997 = CARTESIAN_POINT ( 'NONE',  ( 146.9370072200009645, 276.1446333132804511, -3.799807221059707363 ) ) ;
#30998 = DIRECTION ( 'NONE',  ( -0.8660254037844387076, -0.4999999999999998890, -0.000000000000000000 ) ) ;
#30999 = CARTESIAN_POINT ( 'NONE',  ( 69.50090580276174990, 66.60780273872985902, 10.14006215365368924 ) ) ;
#31000 = DIRECTION ( 'NONE',  ( 0.000000000000000000, 0.000000000000000000, 1.000000000000000000 ) ) ;
#31001 = CARTESIAN_POINT ( 'NONE',  ( 75.73213429733796431, 65.60614264062904510, 13.80850863069982992 ) ) ;
#31002 = CARTESIAN_POINT ( 'NONE',  ( 154.7926630903251350, 264.2811358641517927, -17.33176059627759358 ) ) ;
#31003 = CARTESIAN_POINT ( 'NONE',  ( 78.46010992227571990, 47.82667959050288431, 13.91303883740862624 ) ) ;
#31004 = CARTESIAN_POINT ( 'NONE',  ( 106.3178956768819319, 226.0643266524159856, -9.188101187500093303 ) ) ;
#31005 = ORIENTED_EDGE ( 'NONE', *, *, #6401, .T. ) ;
#31006 = CARTESIAN_POINT ( 'NONE',  ( 191.7187529716733820, 298.5803744197520473, -8.487597704798396592 ) ) ;
#31007 = DIRECTION ( 'NONE',  ( 0.8660254037844363761, 0.5000000000000039968, 0.000000000000000000 ) ) ;
#31008 = DIRECTION ( 'NONE',  ( 0.000000000000000000, 0.000000000000000000, 1.000000000000000000 ) ) ;
#31009 = CARTESIAN_POINT ( 'NONE',  ( 203.5555343017997529, 278.0784677578903370, -15.71723084798551362 ) ) ;
#31010 = CARTESIAN_POINT ( 'NONE',  ( 181.2388288815258477, 283.4805243373127723, -15.08248537652952059 ) ) ;
#31011 = CARTESIAN_POINT ( 'NONE',  ( 147.9595119098395060, 274.3736032395026427, -9.979693660141967015 ) ) ;
#31012 = CARTESIAN_POINT ( 'NONE',  ( 165.4948777162425131, 284.0002391267994994, -8.475767388502914557 ) ) ;
#31013 = ORIENTED_EDGE ( 'NONE', *, *, #95052, .T. ) ;
#31014 = CARTESIAN_POINT ( 'NONE',  ( 207.6837091943624785, 270.9282591014416539, -1.156610046911421552 ) ) ;
#31015 = CARTESIAN_POINT ( 'NONE',  ( 72.46511837996447980, 71.56249752072032777, 6.234640293157911017 ) ) ;
#31016 = CARTESIAN_POINT ( 'NONE',  ( 54.13067045125697518, 195.3927522451418213, 10.00000000000009592 ) ) ;
#31017 = CARTESIAN_POINT ( 'NONE',  ( 121.2293367285889616, 249.9869531367911293, 4.594050593750046652 ) ) ;
#31018 = DIRECTION ( 'NONE',  ( -0.6139877827364832452, 0.7893155279419866721, 0.000000000000000000 ) ) ;
#31019 = DIRECTION ( 'NONE',  ( 0.4999999999999998890, -0.8660254037844385966, 0.000000000000000000 ) ) ;
#31020 = CARTESIAN_POINT ( 'NONE',  ( 157.3988263959001870, 258.0242309610243865, 16.72376558639979294 ) ) ;
#31021 = DIRECTION ( 'NONE',  ( -1.000000000000000000, 0.000000000000000000, 0.000000000000000000 ) ) ;
#31022 = CARTESIAN_POINT ( 'NONE',  ( 49.51212862133765213, 190.2048013555409796, 4.594050593750051981 ) ) ;
#31023 = EDGE_CURVE ( 'NONE', #57165, #30262, #95041, .T. ) ;
#31024 = CARTESIAN_POINT ( 'NONE',  ( 85.76025348255959102, 48.54612661500244997, -11.80603267945767954 ) ) ;
#31026 = ORIENTED_EDGE ( 'NONE', *, *, #4992, .T. ) ;
#31025 = B_SPLINE_CURVE_WITH_KNOTS ( 'NONE', 3,
 ( #82894, #5852, #97580, #29158, #89993, #75266, #11971, #58057, #4357, #20569, #43841, #74780, #3865, #80918, #22041, #30137, #37239, #31121, #84378, #6352, #7332, #68137, #14925, #15930, #52936, #54409, #7843, #46313, #14451, #92964, #91476, #52437, #83889, #45332, #76265, #92474, #62012, #61021, #99554, #31616, #91991, #239, #6837, #77237, #99065, #46835, #23516, #37723, #22543, #90993 ),
 .UNSPECIFIED., .F., .F.,
 ( 4, 2, 2, 2, 2, 2, 2, 2, 2, 2, 2, 2, 2, 2, 2, 2, 2, 2, 2, 2, 2, 2, 2, 2, 4 ),
 ( 0.0007513920313679374680, 0.0009574642477403361596, 0.001060500355926582722, 0.001163536464112829068, 0.001266572572299075414, 0.001369608680485322194, 0.001575680896857799057, 0.001987825329602752999, 0.002399969762347706724, 0.003224258627837614175, 0.004048547493327522492, 0.004872836358817429943, 0.005284980791562383234, 0.005491053007934861181, 0.005594089116121140487, 0.005645607170214243277, 0.005697125224307346067, 0.005800161332493488330, 0.005903197440679630592, 0.006109269657051875219, 0.006521414089796225694, 0.006727486306168400064, 0.006933558522540574434, 0.007139630738912749672, 0.007345702955284924042 ),
 .UNSPECIFIED. ) ;
#31027 = CARTESIAN_POINT ( 'NONE',  ( -19.53030666862117215, 93.13595298606905715, 59.99999999999999289 ) ) ;
#31028 = LINE ( 'NONE', #23420, #7502 ) ;
#31029 = B_SPLINE_SURFACE_WITH_KNOTS ( 'NONE', 3, 1, ( 
 ( #22166, #29765 ),
 ( #30261, #14575 ),
 ( #65888, #29277 ),
 ( #58288, #27409 ),
 ( #89264, #35491 ),
 ( #34985, #6959 ),
 ( #45451, #73509 ),
 ( #53551, #88761 ),
 ( #65397, #50196 ),
 ( #75896, #19814 ),
 ( #81148, #11715 ),
 ( #98696, #99678 ),
 ( #53058, #4093 ),
 ( #74012, #14069 ),
 ( #37846, #61147 ),
 ( #92119, #96842 ),
 ( #22671, #84016 ),
 ( #11225, #6474 ),
 ( #60145, #50682 ),
 ( #42576, #81637 ),
 ( #43069, #83507 ),
 ( #37353, #44955 ),
 ( #4598, #73024 ),
 ( #91107, #21673 ),
 ( #94595, #39334 ),
 ( #15047, #45938 ),
 ( #92598, #76856 ),
 ( #78883, #93083 ),
 ( #100183, #32254 ),
 ( #85511, #54038 ),
 ( #31249, #30768 ),
 ( #62136, #23639 ),
 ( #16553, #84993 ),
 ( #54530, #61649 ) ),
 .UNSPECIFIED., .T., .F., .F.,
 ( 4, 2, 2, 2, 2, 2, 2, 2, 2, 2, 2, 2, 2, 2, 2, 2, 4 ),
 ( 2, 2 ),
 ( 0.000000000000000000, 0.06250000000000000000, 0.1250000000000000000, 0.1875000000000000000, 0.2500000000000000000, 0.3125000000000000000, 0.3750000000000000000, 0.4375000000000000000, 0.5000000000000000000, 0.5625000000000000000, 0.6250000000000000000, 0.6875000000000000000, 0.7500000000000000000, 0.8125000000000000000, 0.8750000000000000000, 0.9375000000000000000, 1.000000000000000000 ),
 ( 0.000000000000000000, 1.000000000000000000 ),
 .UNSPECIFIED. ) ;
#31030 = CARTESIAN_POINT ( 'NONE',  ( 72.94085775465440236, 59.22282884362820710, 16.00814023073137093 ) ) ;
#31031 = CARTESIAN_POINT ( 'NONE',  ( 147.5813496936708020, 275.0285994114094592, 4.516581957185684004 ) ) ;
#31032 = PLANE ( 'NONE',  #80691 ) ;
#31033 = EDGE_CURVE ( 'NONE', #34720, #3513, #77482, .T. ) ;
#31034 = CARTESIAN_POINT ( 'NONE',  ( 198.2505066714982149, 285.2670451491296149, 0.000000000000000000 ) ) ;
#31035 = CARTESIAN_POINT ( 'NONE',  ( 157.3948608031964511, 270.9082508132711382, -14.72219542052569885 ) ) ;
#31036 = CARTESIAN_POINT ( 'NONE',  ( 114.6081111488702931, 223.6427522451417644, 1.119607411625061291E-15 ) ) ;
#31037 = CARTESIAN_POINT ( 'NONE',  ( 15.09101445147005727, 32.21091486745859811, -1.111400068045478839E-16 ) ) ;
#31038 = ORIENTED_EDGE ( 'NONE', *, *, #97788, .F. ) ;
#31039 = EDGE_CURVE ( 'NONE', #93933, #51005, #78740, .T. ) ;
#31040 = CARTESIAN_POINT ( 'NONE',  ( 202.8787628851569593, 279.2506702366259788, 17.01435431865322556 ) ) ;
#31041 = CARTESIAN_POINT ( 'NONE',  ( 86.46651626576456806, 46.39758167564458802, -9.828513499124806430 ) ) ;
#31042 = CARTESIAN_POINT ( 'NONE',  ( 32.43492986863949312, 189.5333772461660544, 9.188101187500095079 ) ) ;
#31043 = CARTESIAN_POINT ( 'NONE',  ( 18.87072174683323666, 11.86426979415088745, -3.090169943749474069 ) ) ;
#31044 = CARTESIAN_POINT ( 'NONE',  ( -17.23615303860155379, 104.9140057318794703, 44.48293588312308344 ) ) ;
#31045 = CARTESIAN_POINT ( 'NONE',  ( 39.49844957003031709, 183.6115022471902023, -5.000000000000041744 ) ) ;
#31046 = CARTESIAN_POINT ( 'NONE',  ( 73.21379494821863432, 69.78953872660252955, 9.103517464032861994 ) ) ;
#31048 = CARTESIAN_POINT ( 'NONE',  ( 56.16917826928300883, 212.4244531367911577, -4.594050593750046652 ) ) ;
#31047 = CARTESIAN_POINT ( 'NONE',  ( 177.3741080081426844, 288.0714115368494959, 10.68489811804565726 ) ) ;
#31049 = CARTESIAN_POINT ( 'NONE',  ( 161.2799361541916028, 251.3019516699124836, 14.40628917569557110 ) ) ;
#31050 = CARTESIAN_POINT ( 'NONE',  ( 73.00502472597065662, 57.20524681399147227, 15.90417734607904876 ) ) ;
#31051 = CARTESIAN_POINT ( 'NONE',  ( -30.34080891622166121, 96.68806665343463180, 44.58230547404211563 ) ) ;
#31052 = ORIENTED_EDGE ( 'NONE', *, *, #10699, .T. ) ;
#31053 = CARTESIAN_POINT ( 'NONE',  ( 33.86928444543146810, 180.3615022471902023, 5.000000000000051514 ) ) ;
#31054 = CARTESIAN_POINT ( 'NONE',  ( 163.7183543885751078, 247.0784873978576854, -6.786164904910574336 ) ) ;
#31055 = CARTESIAN_POINT ( 'NONE',  ( 0.1486806056246424423, 161.7048013555410080, 4.594050593750051981 ) ) ;
#31056 = CARTESIAN_POINT ( 'NONE',  ( 30.58134869734400851, 35.84336893147758474, -7.433330006724137462 ) ) ;
#31057 = CARTESIAN_POINT ( 'NONE',  ( 167.6362108137774669, 262.4817980704067395, -16.57735221840392725 ) ) ;
#31058 = CARTESIAN_POINT ( 'NONE',  ( 185.3427542040608387, 260.2457244105148675, 7.085506836970698608 ) ) ;
#31059 = CARTESIAN_POINT ( 'NONE',  ( 164.9103019330012216, 245.0139736909548560, 2.841678961959298810 ) ) ;
#31060 = CARTESIAN_POINT ( 'NONE',  ( 88.46324942983896733, 43.96425106107526659, 1.817931795122161631 ) ) ;
#31061 = CARTESIAN_POINT ( 'NONE',  ( 65.81518118656045147, 68.94946510510605719, 2.247327669414935780 ) ) ;
#31062 = ORIENTED_EDGE ( 'NONE', *, *, #98811, .T. ) ;
#31063 = CARTESIAN_POINT ( 'NONE',  ( 187.4171132689631634, 261.5282790321019206, -9.397869408254909018 ) ) ;
#31064 = CARTESIAN_POINT ( 'NONE',  ( -19.65312891409030271, 93.06504152958497400, -10.00000000000000888 ) ) ;
#31065 = CARTESIAN_POINT ( 'NONE',  ( 83.42542119994750749, 51.64995580955420706, -14.90072893730332027 ) ) ;
#31066 = CARTESIAN_POINT ( 'NONE',  ( 17.35761498915574563, 12.94754757982088478, 5.678558825948272215 ) ) ;
#31067 = ORIENTED_EDGE ( 'NONE', *, *, #73888, .F. ) ;
#31068 = CARTESIAN_POINT ( 'NONE',  ( 159.8912210074807945, 253.7072768612558775, 15.17831030338107112 ) ) ;
#31069 = CARTESIAN_POINT ( 'NONE',  ( 205.2121761402296443, 275.2090799237855094, -14.05269615702442465 ) ) ;
#31070 = EDGE_CURVE ( 'NONE', #52312, #54608, #66697, .T. ) ;
#31071 = CARTESIAN_POINT ( 'NONE',  ( 71.57943482431289794, 72.41997303871666247, 0.9858917062509267026 ) ) ;
#31072 = CARTESIAN_POINT ( 'NONE',  ( 153.2712411579340426, 265.1734183057532732, 16.26687330118495467 ) ) ;
#31073 = DIRECTION ( 'NONE',  ( 1.000000000000000000, 0.000000000000000000, 0.000000000000000000 ) ) ;
#31074 = CARTESIAN_POINT ( 'NONE',  ( 48.92549481379852949, 97.87922363803308201, 10.00000000000000000 ) ) ;
#31075 = CARTESIAN_POINT ( 'NONE',  ( 207.6067494229581314, 271.0615573356529353, -1.924113146155245868 ) ) ;
#31076 = FACE_BOUND ( 'NONE', #34143, .T. ) ;
#31077 = EDGE_LOOP ( 'NONE', ( #65239, #10656, #53868, #74867 ) ) ;
#31078 = CARTESIAN_POINT ( 'NONE',  ( -42.72532191160158987, 28.29708160126036987, -10.00000000000000000 ) ) ;
#31079 = CARTESIAN_POINT ( 'NONE',  ( 169.3716973832724761, 248.0780012208689982, 1.470315277928950781 ) ) ;
#31080 = ORIENTED_EDGE ( 'NONE', *, *, #77029, .F. ) ;
#31082 = ADVANCED_FACE ( 'NONE', ( #1291 ), #98940, .T. ) ;
#31081 = CARTESIAN_POINT ( 'NONE',  ( 21.98544502579644799, 24.64441083166261137, -10.00000000000000533 ) ) ;
#31083 = CARTESIAN_POINT ( 'NONE',  ( 86.94567315205141256, 44.99287267174491234, -6.599641438898517620 ) ) ;
#31084 = ORIENTED_EDGE ( 'NONE', *, *, #44110, .F. ) ;
#31086 = EDGE_CURVE ( 'NONE', #8862, #25798, #69001, .T. ) ;
#31085 = DIRECTION ( 'NONE',  ( -0.2588190451025027539, -0.9659258262890730862, -9.720431063823805450E-17 ) ) ;
#31087 = FACE_OUTER_BOUND ( 'NONE', #50181, .T. ) ;
#31088 = CARTESIAN_POINT ( 'NONE',  ( 184.2795938587219382, 282.7716313920612379, -17.16491284908262216 ) ) ;
#31089 = CARTESIAN_POINT ( 'NONE',  ( 74.93017357788674815, 189.2419560658248940, 17.47570218321536117 ) ) ;
#31090 = CARTESIAN_POINT ( 'NONE',  ( 69.89538980332476115, 62.79524207331544972, 13.90205096215579950 ) ) ;
#31091 = ORIENTED_EDGE ( 'NONE', *, *, #73514, .T. ) ;
#31092 = CARTESIAN_POINT ( 'NONE',  ( 200.1103929410127762, 284.0456276340304953, 17.67835211026828901 ) ) ;
#31093 = B_SPLINE_CURVE_WITH_KNOTS ( 'NONE', 3,
 ( #38995, #83661, #45111, #61797 ),
 .UNSPECIFIED., .F., .F.,
 ( 4, 4 ),
 ( 2.098622547487930532E-15, 0.004943534199230881221 ),
 .UNSPECIFIED. ) ;
#31094 = CARTESIAN_POINT ( 'NONE',  ( 66.10228174255657052, 68.64626758096548542, 4.271897712742703135 ) ) ;
#31095 = CARTESIAN_POINT ( 'NONE',  ( 141.5270674498366077, 242.5177522451417929, 5.000000000000051514 ) ) ;
#31096 = ORIENTED_EDGE ( 'NONE', *, *, #66550, .F. ) ;
#31097 = ORIENTED_EDGE ( 'NONE', *, *, #13650, .F. ) ;
#31098 = ORIENTED_EDGE ( 'NONE', *, *, #13163, .T. ) ;
#31099 = CARTESIAN_POINT ( 'NONE',  ( 74.50658829527574767, 66.53799963998996247, 12.80246580919608235 ) ) ;
#31100 = ORIENTED_EDGE ( 'NONE', *, *, #97454, .F. ) ;
#31101 = CARTESIAN_POINT ( 'NONE',  ( 70.85244465605627795, 71.45066637977274127, 2.090713904591689598 ) ) ;
#31102 = ORIENTED_EDGE ( 'NONE', *, *, #95793, .T. ) ;
#31103 = CARTESIAN_POINT ( 'NONE',  ( 164.3545367017254364, 245.9765873086048487, -5.942639963102972267 ) ) ;
#31104 = CARTESIAN_POINT ( 'NONE',  ( 81.47863721931979342, 44.48187038564707052, 10.12635968134262399 ) ) ;
#31105 = CARTESIAN_POINT ( 'NONE',  ( 165.6431331270639760, 271.4262817979627584, 17.22401055456362684 ) ) ;
#31106 = CARTESIAN_POINT ( 'NONE',  ( 167.0646487823995585, 282.1497282158676398, 11.94391941918240185 ) ) ;
#31107 = CARTESIAN_POINT ( 'NONE',  ( 194.8067605455144076, 293.2317884077015151, -16.00245909155922774 ) ) ;
#31108 = CARTESIAN_POINT ( 'NONE',  ( 82.87162244869749372, 53.63483014063397292, -15.36256874745430245 ) ) ;
#31109 = CARTESIAN_POINT ( 'NONE',  ( 198.2505066714982149, 285.2670451491296149, 0.000000000000000000 ) ) ;
#31110 = ORIENTED_EDGE ( 'NONE', *, *, #1638, .T. ) ;
#31111 = CARTESIAN_POINT ( 'NONE',  ( 167.0648401017704430, 247.0325385398216440, 1.942792713102396762 ) ) ;
#31112 = CARTESIAN_POINT ( 'NONE',  ( 17.90851666933368236, 18.84335787977762777, 9.188101187500006262 ) ) ;
#31113 = CARTESIAN_POINT ( 'NONE',  ( -22.42236680055709641, 157.8615022471902591, 0.000000000000000000 ) ) ;
#31114 = CARTESIAN_POINT ( 'NONE',  ( 85.69555808373030459, 48.70564388484159224, 11.94729400084767157 ) ) ;
#31116 = ORIENTED_EDGE ( 'NONE', *, *, #50862, .F. ) ;
#31115 = DIRECTION ( 'NONE',  ( -0.5000000000000011102, -0.8660254037844380415, 0.000000000000000000 ) ) ;
#31117 = CARTESIAN_POINT ( 'NONE',  ( 168.3105211781452795, 256.9082286493703009, -14.73656021653829384 ) ) ;
#31118 = CARTESIAN_POINT ( 'NONE',  ( 159.2102594322688844, 254.8867369075254885, -16.13039487917589199 ) ) ;
#31119 = CARTESIAN_POINT ( 'NONE',  ( -17.42236680055705023, 149.2012482093457777, 0.000000000000000000 ) ) ;
#31120 = CARTESIAN_POINT ( 'NONE',  ( 82.21697353817442888, 45.95328030435120326, -11.18469232000785496 ) ) ;
#31121 = CARTESIAN_POINT ( 'NONE',  ( 168.9042932422607919, 253.9312568212353085, 11.43877001047246189 ) ) ;
#31122 = CARTESIAN_POINT ( 'NONE',  ( 161.0249958932952552, 283.1118547020287224, 2.115121692784775576 ) ) ;
#31123 = CARTESIAN_POINT ( 'NONE',  ( 193.9307011644069973, 294.7491677662272878, -14.33994679320232990 ) ) ;
#31124 = DIRECTION ( 'NONE',  ( 0.4999999999999992784, -0.8660254037844390407, 0.000000000000000000 ) ) ;
#31125 = LINE ( 'NONE', #52943, #51596 ) ;
#31126 = CARTESIAN_POINT ( 'NONE',  ( 8.159155267032986103, 175.5177522451418781, -10.00000000000009592 ) ) ;
#31127 = CARTESIAN_POINT ( 'NONE',  ( 82.77265646360999085, 218.5958772461660544, -9.188101187500095079 ) ) ;
#31128 = CARTESIAN_POINT ( 'NONE',  ( 196.0257901730189474, 269.4247523037524275, -10.81113306140426999 ) ) ;
#31129 = CARTESIAN_POINT ( 'NONE',  ( 16.00201260034520345, 10.20801979619927380, -3.090169943749474069 ) ) ;
#31130 = CARTESIAN_POINT ( 'NONE',  ( 163.8240215689833690, 246.8954664726980184, -8.949281535847481095 ) ) ;
#31131 = LINE ( 'NONE', #62024, #82406 ) ;
#31133 = CARTESIAN_POINT ( 'NONE',  ( -22.42236680055709641, 157.8615022471902591, 0.000000000000000000 ) ) ;
#31132 = CARTESIAN_POINT ( 'NONE',  ( -1.313257906909115480, 179.2369531367911293, -4.594050593750048428 ) ) ;
#31134 = ADVANCED_FACE ( 'NONE', ( #13341 ), #56155, .F. ) ;
#31135 = CARTESIAN_POINT ( 'NONE',  ( 200.1782072557437857, 283.9281697954355650, 18.05177561285849208 ) ) ;
#31136 = ORIENTED_EDGE ( 'NONE', *, *, #36694, .F. ) ;
#31137 = VERTEX_POINT ( 'NONE', #31999 ) ;
#31138 = CARTESIAN_POINT ( 'NONE',  ( 49.80235952159635815, 85.00000000000000000, -10.00000000000000000 ) ) ;
#31139 = ADVANCED_FACE ( 'NONE', ( #86271 ), #84450, .F. ) ;
#31140 = CARTESIAN_POINT ( 'NONE',  ( 82.17887713766984348, 46.62351855337478668, -11.80422335332041328 ) ) ;
#31141 = CARTESIAN_POINT ( 'NONE',  ( 157.6036818288543486, 257.6694109429415107, -16.73826488331764395 ) ) ;
#31142 = CARTESIAN_POINT ( 'NONE',  ( 162.8917261183091227, 248.5102495609312143, -11.80346065365840680 ) ) ;
#31143 = CARTESIAN_POINT ( 'NONE',  ( 106.8138825148102740, 239.1427522451419065, -10.00000000000009592 ) ) ;
#31144 = CARTESIAN_POINT ( 'NONE',  ( 176.8408657501080654, 282.3818803302173137, -15.82416175011198689 ) ) ;
#31145 = CARTESIAN_POINT ( 'NONE',  ( 18.65997361151702449, 172.3923013555409796, 4.594050593750050204 ) ) ;
#31146 = CARTESIAN_POINT ( 'NONE',  ( 130.4855038751826726, 236.9548013555409796, -4.594050593750042211 ) ) ;
#31147 = CARTESIAN_POINT ( 'NONE',  ( 183.5021136046642596, 257.1513431580297038, -3.213728371295248465 ) ) ;
#31148 = ORIENTED_EDGE ( 'NONE', *, *, #80431, .T. ) ;
#31149 = EDGE_CURVE ( 'NONE', #89481, #41262, #33521, .T. ) ;
#31150 = DIRECTION ( 'NONE',  ( -0.5000000000000019984, 0.8660254037844374864, 0.000000000000000000 ) ) ;
#31151 = LINE ( 'NONE', #92995, #32379 ) ;
#31152 = AXIS2_PLACEMENT_3D ( 'NONE', #66076, #81321, #3788 ) ;
#31153 = AXIS2_PLACEMENT_3D ( 'NONE', #84677, #83685, #14246 ) ;
#31154 = CARTESIAN_POINT ( 'NONE',  ( 34.10980067877857635, 31.64441083166263269, -10.00000000000000533 ) ) ;
#31155 = CARTESIAN_POINT ( 'NONE',  ( 195.9713281756800427, 291.2146981034049418, 17.52210387885178022 ) ) ;
#31156 = CARTESIAN_POINT ( 'NONE',  ( 194.4165969972361552, 293.9075714965812267, 14.23342188338008718 ) ) ;
#31157 = CARTESIAN_POINT ( 'NONE',  ( 207.2167723318516153, 271.7370174712370954, -6.606038862010207957 ) ) ;
#31158 = CARTESIAN_POINT ( 'NONE',  ( 81.08332877246739656, 43.92371124442119168, 10.53733257259109735 ) ) ;
#31159 = CARTESIAN_POINT ( 'NONE',  ( 148.1829914015846157, 273.9865254053503349, -9.304102644963160529 ) ) ;
#31161 = EDGE_CURVE ( 'NONE', #11833, #97853, #48596, .T. ) ;
#31160 = CIRCLE ( 'NONE', #21498, 70.00000000000001421 ) ;
#31162 = CARTESIAN_POINT ( 'NONE',  ( 187.1736806720859647, 299.3961564376974138, 1.305121339064515551 ) ) ;
#31163 = CARTESIAN_POINT ( 'NONE',  ( 168.4104533980780900, 278.9328176548356168, 14.99313165221212252 ) ) ;
#31164 = CARTESIAN_POINT ( 'NONE',  ( 192.5170171266991304, 265.2796291261559531, 8.180105463325700654 ) ) ;
#31165 = CARTESIAN_POINT ( 'NONE',  ( 67.78251950854047436, 66.97470367889792442, 8.421653629368158533 ) ) ;
#31166 = CARTESIAN_POINT ( 'NONE',  ( 189.8314329296643450, 301.8493086226544619, -0.8085564604676659384 ) ) ;
#31167 = CARTESIAN_POINT ( 'NONE',  ( 180.8012419246406353, 266.7401795635341273, -14.70472759341407709 ) ) ;
#31168 = EDGE_CURVE ( 'NONE', #42726, #28514, #44580, .T. ) ;
#31169 = ORIENTED_EDGE ( 'NONE', *, *, #99358, .F. ) ;
#31170 = CARTESIAN_POINT ( 'NONE',  ( 151.9556655013304862, 274.5278385319554104, -11.22762646749768756 ) ) ;
#31171 = CARTESIAN_POINT ( 'NONE',  ( 185.2582332437331445, 272.4808076714297727, 17.23139995252659773 ) ) ;
#31172 = CARTESIAN_POINT ( 'NONE',  ( 111.8384605302426991, 241.5024278399160664, -9.188101187500093303 ) ) ;
#31173 = CARTESIAN_POINT ( 'NONE',  ( 14.76917458061509514, 17.03085787977762067, 9.188101187500006262 ) ) ;
#31174 = CARTESIAN_POINT ( 'NONE',  ( 151.0778907302193943, 268.9724126853576536, 15.84769371787143832 ) ) ;
#31175 = CARTESIAN_POINT ( 'NONE',  ( -58.02784037451009880, 34.21088073648085981, -10.00000000000000000 ) ) ;
#31176 = AXIS2_PLACEMENT_3D ( 'NONE', #86899, #94472, #17434 ) ;
#31178 = CARTESIAN_POINT ( 'NONE',  ( 191.6230175057792451, 276.9742630895800630, 16.77582784212352252 ) ) ;
#31177 = CARTESIAN_POINT ( 'NONE',  ( 18.52134341065868384, 22.64441083166259716, 0.000000000000000000 ) ) ;
#31179 = CARTESIAN_POINT ( 'NONE',  ( 196.7941661740290158, 289.7895008838662534, 17.93043241841150959 ) ) ;
#31180 = DIRECTION ( 'NONE',  ( 0.4999999999999992784, -0.8660254037844390407, 0.000000000000000000 ) ) ;
#31181 = PLANE ( 'NONE',  #86645 ) ;
#31182 = CARTESIAN_POINT ( 'NONE',  ( 123.3201800421238090, 253.5530062829863311, -4.648177544792955347E-16 ) ) ;
#31183 = CARTESIAN_POINT ( 'NONE',  ( 86.43642008611649885, 47.55668332166565904, 10.53568000035417995 ) ) ;
#31184 = ORIENTED_EDGE ( 'NONE', *, *, #28905, .T. ) ;
#31185 = CARTESIAN_POINT ( 'NONE',  ( 163.7565952011062507, 255.1539107282341092, -15.17543724475343048 ) ) ;
#31186 = CARTESIAN_POINT ( 'NONE',  ( 27.63686232447692603, 34.14336893147756768, 7.433330006724141015 ) ) ;
#31187 = DIRECTION ( 'NONE',  ( 0.4493970231495826861, -0.7783784768652872721, -0.4383711467890751834 ) ) ;
#31188 = CARTESIAN_POINT ( 'NONE',  ( 200.1795251174064560, 269.7820628003561296, 8.922369943785961155 ) ) ;
#31189 = CARTESIAN_POINT ( 'NONE',  ( 149.4908848037268001, 271.7211875819559737, -12.92288068979413573 ) ) ;
#31190 = EDGE_CURVE ( 'NONE', #91064, #91993, #5604, .T. ) ;
#31191 = ORIENTED_EDGE ( 'NONE', *, *, #55279, .F. ) ;
#31192 = B_SPLINE_CURVE_WITH_KNOTS ( 'NONE', 3,
 ( #40015, #63833, #55215, #33439, #87715, #18250, #1555, #86197, #80080, #39016, #538, #31423, #81086, #72467, #89203, #65335, #89684, #82081, #66333, #19751, #35922, #18749, #88197, #33958 ),
 .UNSPECIFIED., .F., .F.,
 ( 4, 2, 2, 2, 2, 2, 2, 2, 2, 2, 2, 4 ),
 ( 0.000000000000000000, 0.1250000000000164591, 0.2500000000000329181, 0.3750000000000494049, 0.4375000000000497935, 0.5000000000000501821, 0.5625000000000506262, 0.6250000000000510703, 0.6875000000000515143, 0.7500000000000519584, 0.8750000000000260902, 1.000000000000000000 ),
 .UNSPECIFIED. ) ;
#31193 = LINE ( 'NONE', #2703, #24328 ) ;
#31194 = CARTESIAN_POINT ( 'NONE',  ( 78.82603149318642011, 48.82109720856274748, 14.29823851343999941 ) ) ;
#31195 = CARTESIAN_POINT ( 'NONE',  ( 181.9559929377375056, 291.6402902057536721, -11.43735378946719372 ) ) ;
#31196 = DIRECTION ( 'NONE',  ( -0.8660254037844377084, -0.5000000000000014433, -0.000000000000000000 ) ) ;
#31197 = CARTESIAN_POINT ( 'NONE',  ( 74.90541669563339156, 53.37575215131342077, -16.53204517015438313 ) ) ;
#31198 = CARTESIAN_POINT ( 'NONE',  ( 153.1745822862813498, 265.3408363824576668, 16.18092354043443493 ) ) ;
#31199 = EDGE_CURVE ( 'NONE', #31328, #44296, #61835, .T. ) ;
#31200 = VERTEX_POINT ( 'NONE', #14204 ) ;
#31201 = CARTESIAN_POINT ( 'NONE',  ( 73.36774340952439388, 69.90371635966560859, 9.665654898056800448 ) ) ;
#31202 = CARTESIAN_POINT ( 'NONE',  ( 42.00264329202813229, 26.11110640527295601, -2.839279412974138328 ) ) ;
#31203 = ORIENTED_EDGE ( 'NONE', *, *, #3295, .T. ) ;
#31204 = CARTESIAN_POINT ( 'NONE',  ( 164.3996301846870267, 247.3020492865104529, 7.248807534621905191 ) ) ;
#31205 = B_SPLINE_CURVE_WITH_KNOTS ( 'NONE', 3,
 ( #32267, #56048, #55550, #86534, #41358, #17064, #48480, #2907, #9483, #40354, #79422, #62150, #71291, #9988, #81416, #20582, #81910, #51463, #73287, #58556, #58072, #28166, #34275, #89054, #73781, #43854, #4370, #80934, #3879, #35268, #19604, #82430, #12489, #65171, #43356, #27687, #50464, #11987, #57561, #34763 ),
 .UNSPECIFIED., .F., .F.,
 ( 4, 2, 2, 2, 2, 2, 2, 2, 2, 2, 2, 2, 2, 2, 2, 2, 2, 2, 2, 4 ),
 ( 0.002905659672395857849, 0.003105746374355510941, 0.003305833076315163599, 0.003405876427294977568, 0.003505919778274790670, 0.003605963129254604639, 0.003706006480234417741, 0.003906093182194044378, 0.004106179884153671016, 0.004506353288073101232, 0.005306700095912135137, 0.006107046903751169042, 0.007707740519429236853, 0.007907827221389052141, 0.007957848896878968667, 0.008007870572368885193, 0.008107913923348666202, 0.008508087327267866568, 0.008908260731187066933, 0.009308434135106267299 ),
 .UNSPECIFIED. ) ;
#31207 = ADVANCED_FACE ( 'NONE', ( #60767 ), #74534, .F. ) ;
#31206 = DIRECTION ( 'NONE',  ( -0.5000000000000013323, 0.8660254037844380415, 0.000000000000000000 ) ) ;
#31208 = VERTEX_POINT ( 'NONE', #97827 ) ;
#31210 = EDGE_CURVE ( 'NONE', #45557, #29501, #74464, .T. ) ;
#31209 = CARTESIAN_POINT ( 'NONE',  ( 86.23632586776285791, 46.97348825937578454, -10.05460913028329450 ) ) ;
#31211 = CARTESIAN_POINT ( 'NONE',  ( 205.9755752649865315, 273.8868338532529378, 12.31646113325132674 ) ) ;
#31212 = PLANE ( 'NONE',  #75283 ) ;
#31213 = CARTESIAN_POINT ( 'NONE',  ( 80.81722803126136512, 44.69323391722993932, -11.42900611749914219 ) ) ;
#31214 = CARTESIAN_POINT ( 'NONE',  ( 111.2161783173811500, 245.0177522451419065, 5.000000000000046185 ) ) ;
#31215 = CARTESIAN_POINT ( 'NONE',  ( 81.62115332376640708, 55.85468755722441614, -16.37141313285761157 ) ) ;
#31216 = EDGE_CURVE ( 'NONE', #6854, #36578, #90759, .T. ) ;
#31217 = EDGE_CURVE ( 'NONE', #86029, #20189, #4993, .T. ) ;
#31218 = VERTEX_POINT ( 'NONE', #83136 ) ;
#31219 = CARTESIAN_POINT ( 'NONE',  ( 195.8729049011480470, 290.8691304563884614, 15.97541058376903855 ) ) ;
#31220 = VERTEX_POINT ( 'NONE', #24782 ) ;
#31221 = CARTESIAN_POINT ( 'NONE',  ( 77.36600796148924530, 49.13692148722834929, -14.77749963168139935 ) ) ;
#31222 = EDGE_LOOP ( 'NONE', ( #29160, #7748, #53931, #62389 ) ) ;
#31223 = CARTESIAN_POINT ( 'NONE',  ( 170.1342846507165518, 269.5121279834121992, 16.76028639438306911 ) ) ;
#31225 = EDGE_LOOP ( 'NONE', ( #62721, #49320, #8926, #4875, #9836 ) ) ;
#31224 =( BOUNDED_CURVE ( )  B_SPLINE_CURVE ( 2, ( #21547, #22029, #15409, #83376, #84372, #44327, #52929, #90986, #76732 ),
 .UNSPECIFIED., .F., .T. ) 
 B_SPLINE_CURVE_WITH_KNOTS ( ( 3, 2, 2, 2, 3 ),
 ( 0.1653225806451612823, 0.1666666666666666574, 0.1693548387096774077, 0.1720430107526881858, 0.1733870967741935609 ),
 .UNSPECIFIED. ) 
 CURVE ( )  GEOMETRIC_REPRESENTATION_ITEM ( )  RATIONAL_B_SPLINE_CURVE ( ( 0.9330127018922194093, 0.9330127018922194093, 1.000000000000000000, 0.8660254037844387076, 1.000000000000000000, 0.8660254037844387076, 1.000000000000000000, 0.9330127018922194093, 0.9330127018922194093 ) ) 
 REPRESENTATION_ITEM ( '' )  );
#31226 = CARTESIAN_POINT ( 'NONE',  ( 164.5519675908388422, 246.2604196026755687, 2.628616105114974122 ) ) ;
#31227 = CARTESIAN_POINT ( 'NONE',  ( 206.7182525013508041, 272.6004791462452204, -10.42767927275168205 ) ) ;
#31228 = CARTESIAN_POINT ( 'NONE',  ( 67.70770923549420672, 67.39958653419566303, 8.673274222080605611 ) ) ;
#31229 = CARTESIAN_POINT ( 'NONE',  ( 197.7385643933960750, 285.3845219642180382, -17.06910720252511027 ) ) ;
#31230 = CARTESIAN_POINT ( 'NONE',  ( 82.57037383359188709, 41.04081928364340115, 1.106021355371193282 ) ) ;
#31231 = CARTESIAN_POINT ( 'NONE',  ( 167.7191586515327231, 249.2659981153678359, -5.464437866973313795 ) ) ;
#31232 = CARTESIAN_POINT ( 'NONE',  ( 24.69086998626515594, 38.90223361192551010, 177.5919119679930134 ) ) ;
#31233 = CARTESIAN_POINT ( 'NONE',  ( 186.1263547150109900, 286.8862237501084564, -16.18252752151998308 ) ) ;
#31234 = CARTESIAN_POINT ( 'NONE',  ( 137.8467198073504107, 241.2048013555409796, 4.594050593750051981 ) ) ;
#31235 = CARTESIAN_POINT ( 'NONE',  ( 186.7214803242468122, 262.7147121518711401, -9.981163800224575056 ) ) ;
#31236 = CARTESIAN_POINT ( 'NONE',  ( 42.85004829832550399, 33.24335787977766188, -9.188101187500008038 ) ) ;
#31237 = CARTESIAN_POINT ( 'NONE',  ( 179.9513890298225078, 291.5425348745724818, -10.01420112412196772 ) ) ;
#31238 = ORIENTED_EDGE ( 'NONE', *, *, #95684, .T. ) ;
#31239 = AXIS2_PLACEMENT_3D ( 'NONE', #25171, #63676, #17578 ) ;
#31240 = CARTESIAN_POINT ( 'NONE',  ( 86.89657730260137214, 45.77512320498411214, -8.683907937581334835 ) ) ;
#31241 = CARTESIAN_POINT ( 'NONE',  ( 178.5998364833490939, 254.7693240753903297, 1.328249545842869139 ) ) ;
#31242 = VECTOR ( 'NONE', #1935, 1000.000000000000114 ) ;
#31243 = CARTESIAN_POINT ( 'NONE',  ( 171.1538413615039360, 287.7943309346417209, -4.649139628941194147 ) ) ;
#31244 = CARTESIAN_POINT ( 'NONE',  ( 146.6671492545637534, 276.6120410202449307, 3.340372238077111255 ) ) ;
#31245 = FACE_OUTER_BOUND ( 'NONE', #44907, .T. ) ;
#31246 = CARTESIAN_POINT ( 'NONE',  ( 201.0844796915553161, 282.3584598911111812, -16.59562674965125950 ) ) ;
#31247 = CARTESIAN_POINT ( 'NONE',  ( 177.2389597949545248, 288.8581041804060874, -9.261545317147978906 ) ) ;
#31248 = EDGE_LOOP ( 'NONE', ( #38566, #23735, #34834, #39617, #89275 ) ) ;
#31249 = CARTESIAN_POINT ( 'NONE',  ( 194.7900099568305166, 293.2608012783592812, 16.38313017464638932 ) ) ;
#31250 = CARTESIAN_POINT ( 'NONE',  ( 164.8624568345837531, 246.3845970976477417, 4.092954484416948979 ) ) ;
#31251 = EDGE_LOOP ( 'NONE', ( #63547, #20393, #22560, #58374 ) ) ;
#31252 = CARTESIAN_POINT ( 'NONE',  ( 194.2223991963907963, 294.2439319543634610, -14.97294938100067441 ) ) ;
#31253 = CARTESIAN_POINT ( 'NONE',  ( 167.9496373820661290, 248.6204696539478789, -6.517719931589019744 ) ) ;
#31254 = ORIENTED_EDGE ( 'NONE', *, *, #50987, .T. ) ;
#31255 = CARTESIAN_POINT ( 'NONE',  ( 188.1709242600894925, 266.2605123816134665, -11.82625739451866131 ) ) ;
#31256 = CIRCLE ( 'NONE', #37688, 17.82106496071138935 ) ;
#31257 = CARTESIAN_POINT ( 'NONE',  ( 156.9511562921923939, 276.6036013291395079, 10.24360920285362653 ) ) ;
#31258 = CARTESIAN_POINT ( 'NONE',  ( 193.1664498718385232, 262.6697469753432870, 4.718537006446267945 ) ) ;
#31259 = CARTESIAN_POINT ( 'NONE',  ( 190.6893905452545823, 300.3632824417117604, 3.294993852933539191 ) ) ;
#31260 = CARTESIAN_POINT ( 'NONE',  ( -46.74660806181546491, 29.87360136034011049, -10.00000000000000000 ) ) ;
#31262 = CARTESIAN_POINT ( 'NONE',  ( 156.8144410367226840, 280.3425935702447305, 5.941698292227072464 ) ) ;
#31261 = CARTESIAN_POINT ( 'NONE',  ( 163.3456309634439663, 283.9452505866142928, -7.113541931128232854 ) ) ;
#31263 = CARTESIAN_POINT ( 'NONE',  ( 160.4258337542706272, 283.3657075219940680, -4.450354451773817388 ) ) ;
#31264 = ORIENTED_EDGE ( 'NONE', *, *, #18828, .F. ) ;
#31265 = CARTESIAN_POINT ( 'NONE',  ( 190.5541309856500050, 300.5975588711562523, -4.167177996129430184 ) ) ;
#31267 = CARTESIAN_POINT ( 'NONE',  ( 72.85462391432039908, 67.11347816504185460, 11.56953996784876715 ) ) ;
#31266 = B_SPLINE_SURFACE_WITH_KNOTS ( 'NONE', 3, 1, ( 
 ( #22710, #15579 ),
 ( #62682, #39374 ),
 ( #53588, #70807 ),
 ( #47001, #54572 ),
 ( #402, #86069 ),
 ( #30303, #7491 ),
 ( #61686, #23680 ),
 ( #61189, #100221 ),
 ( #84543, #15086 ),
 ( #92638, #85556 ),
 ( #31780, #16595 ),
 ( #14611, #46482 ),
 ( #68790, #70289 ),
 ( #93635, #8016 ),
 ( #38384, #45974 ),
 ( #76891, #24202 ),
 ( #47491, #31291 ),
 ( #78416, #23187 ),
 ( #69297, #30806 ),
 ( #8998, #85033 ),
 ( #54080, #91635 ),
 ( #22203, #93131 ),
 ( #38889, #69792 ),
 ( #16097, #49007 ),
 ( #25714, #88560 ),
 ( #96141, #17600 ),
 ( #3424, #26700 ),
 ( #32791, #72327 ),
 ( #19125, #42379 ),
 ( #71317, #34299 ),
 ( #11021, #2417 ),
 ( #57584, #33819 ),
 ( #3903, #11521 ),
 ( #1910, #17091 ) ),
 .UNSPECIFIED., .T., .F., .F.,
 ( 4, 2, 2, 2, 2, 2, 2, 2, 2, 2, 2, 2, 2, 2, 2, 2, 4 ),
 ( 2, 2 ),
 ( 0.000000000000000000, 0.06250000000000000000, 0.1250000000000000000, 0.1875000000000000000, 0.2500000000000000000, 0.3125000000000000000, 0.3750000000000000000, 0.4375000000000000000, 0.5000000000000000000, 0.5625000000000000000, 0.6250000000000000000, 0.6875000000000000000, 0.7500000000000000000, 0.8125000000000000000, 0.8750000000000000000, 0.9375000000000000000, 1.000000000000000000 ),
 ( 0.000000000000000000, 1.000000000000000000 ),
 .UNSPECIFIED. ) ;
#31268 = CARTESIAN_POINT ( 'NONE',  ( 186.7629878510455512, 262.7841317527147567, -8.999996197527845965 ) ) ;
#31269 = CARTESIAN_POINT ( 'NONE',  ( -28.04097607764120781, 24.82386083235214969, -10.00000000000000000 ) ) ;
#31270 = CARTESIAN_POINT ( 'NONE',  ( 12.89700858264996164, 45.12712377379325801, 59.99999999999999289 ) ) ;
#31271 = CARTESIAN_POINT ( 'NONE',  ( 184.7908904391260592, 296.8361954622408234, -4.367935385452441643 ) ) ;
#31272 = CARTESIAN_POINT ( 'NONE',  ( 204.3073682595353091, 276.3816438339565593, 13.21529881594027422 ) ) ;
#31273 = CARTESIAN_POINT ( 'NONE',  ( 27.19136022205111658, 198.0530062829863311, -4.648177544792955347E-16 ) ) ;
#31274 = CARTESIAN_POINT ( 'NONE',  ( 155.0197698005585494, 262.1448778582381465, 18.42918111182112284 ) ) ;
#31275 = CARTESIAN_POINT ( 'NONE',  ( 191.2333131753503892, 283.1309561651182776, -16.66095403317861923 ) ) ;
#31276 = CARTESIAN_POINT ( 'NONE',  ( 70.56242779276917076, 66.53244391737094077, -11.50149545576417864 ) ) ;
#31277 = CARTESIAN_POINT ( 'NONE',  ( 82.61045024828291616, 212.3768266524159856, -9.188101187500091527 ) ) ;
#31278 = CARTESIAN_POINT ( 'NONE',  ( 67.35448364888117112, 66.58801464723161700, 8.610823906226203306 ) ) ;
#31279 = CARTESIAN_POINT ( 'NONE',  ( 147.1603453755519695, 275.7578002805973370, -5.230822882238410187 ) ) ;
#31280 = CARTESIAN_POINT ( 'NONE',  ( 7.454216751344177716, 28.24511763804003195, -10.00000000000000000 ) ) ;
#31281 = EDGE_CURVE ( 'NONE', #34720, #97734, #6234, .T. ) ;
#31282 = CARTESIAN_POINT ( 'NONE',  ( 203.0026270830780675, 279.0361311525880978, -16.61345826058821373 ) ) ;
#31283 = CARTESIAN_POINT ( 'NONE',  ( 52.72569090598241104, 189.7012482093459766, 4.692658452248458818E-14 ) ) ;
#31284 = CARTESIAN_POINT ( 'NONE',  ( -16.14350997085658790, 56.98620320469874656, 0.000000000000000000 ) ) ;
#31285 = CARTESIAN_POINT ( 'NONE',  ( 66.57026871561892278, 68.76443072695623471, 4.738950751700696351 ) ) ;
#31287 = CARTESIAN_POINT ( 'NONE',  ( 76.01988506423570868, 51.27439951277732177, 16.12938561522662440 ) ) ;
#31286 = CARTESIAN_POINT ( 'NONE',  ( 73.72251996588057921, 69.48154048452748555, -9.822749744319873244 ) ) ;
#31288 = CARTESIAN_POINT ( 'NONE',  ( 207.6777884554021512, 270.9385141221390541, 6.417167147861016829 ) ) ;
#31289 = EDGE_CURVE ( 'NONE', #30119, #86428, #50906, .T. ) ;
#31290 = CARTESIAN_POINT ( 'NONE',  ( 166.0155133103885703, 249.5026163374074599, -9.152316162654148712 ) ) ;
#31291 = CARTESIAN_POINT ( 'NONE',  ( 163.9864329842212953, 246.6141616497770030, -4.773827767272011080 ) ) ;
#31292 = CARTESIAN_POINT ( 'NONE',  ( 196.1573359623355088, 290.8925231663144473, 17.55680092534192482 ) ) ;
#31293 = DIRECTION ( 'NONE',  ( -0.2165469281463391349, 0.9762722099447388446, 0.000000000000000000 ) ) ;
#31294 = ADVANCED_FACE ( 'NONE', ( #95243 ), #85281, .F. ) ;
#31295 = LINE ( 'NONE', #55579, #33537 ) ;
#31296 = CARTESIAN_POINT ( 'NONE',  ( 39.95835201613431309, 200.0024278399160949, 9.188101187500095079 ) ) ;
#31297 = CARTESIAN_POINT ( 'NONE',  ( 55.05949644674294774, 214.8464784336661637, 1.353441290958777327E-15 ) ) ;
#31298 = CARTESIAN_POINT ( 'NONE',  ( 57.11559101558731300, 215.3297689869269220, -2.679491924311252493 ) ) ;
#31299 = CARTESIAN_POINT ( 'NONE',  ( 88.28592015977812935, 44.16006502160690417, -0.2344584660016976740 ) ) ;
#31300 = CARTESIAN_POINT ( 'NONE',  ( 163.6320872669321602, 257.9766140902174243, 15.55573320749642896 ) ) ;
#31301 = CARTESIAN_POINT ( 'NONE',  ( -7.699934936221591641, 156.3615022471902023, 5.000000000000051514 ) ) ;
#31302 = CARTESIAN_POINT ( 'NONE',  ( 77.71695824120645568, 49.45779813244274692, 15.33409790704233977 ) ) ;
#31303 = CARTESIAN_POINT ( 'NONE',  ( 196.4096156673327869, 269.1445197880362343, -10.54851971483136630 ) ) ;
#31304 = CARTESIAN_POINT ( 'NONE',  ( 31.21402144970675252, 20.94754757982090609, 5.678558825948272215 ) ) ;
#31305 = CARTESIAN_POINT ( 'NONE',  ( 81.58050098450105736, 59.42274603127592769, -0.3830222215594929480 ) ) ;
#31306 = CARTESIAN_POINT ( 'NONE',  ( 81.70770681640576072, 47.33369484184763820, -12.52618337250604519 ) ) ;
#31307 = CARTESIAN_POINT ( 'NONE',  ( 9.658441966945924051, 28.68290643055185996, 3.479690158560446702E-15 ) ) ;
#31308 = CARTESIAN_POINT ( 'NONE',  ( 70.72975101405640430, 202.4548013555409796, -4.594050593750042211 ) ) ;
#31309 = CARTESIAN_POINT ( 'NONE',  ( 77.20294869268629157, 63.53692916728167006, 15.07858399788869797 ) ) ;
#31310 = CARTESIAN_POINT ( 'NONE',  ( 154.8579861482817535, 262.4250953638155011, -17.69813260923097786 ) ) ;
#31311 = CARTESIAN_POINT ( 'NONE',  ( 198.3449891235413531, 287.1033967417670283, 16.95540786497457120 ) ) ;
#31312 = CARTESIAN_POINT ( 'NONE',  ( 66.77376812102318127, 68.41195941748605946, -4.433129028897194068 ) ) ;
#31313 = CARTESIAN_POINT ( 'NONE',  ( 153.6005803596509054, 264.6029860754553056, 18.07864614867099462 ) ) ;
#31314 = AXIS2_PLACEMENT_3D ( 'NONE', #6275, #37170, #68068 ) ;
#31315 = CARTESIAN_POINT ( 'NONE',  ( 81.12641806927595667, 54.67637760867621211, -15.82913326966788681 ) ) ;
#31316 = CARTESIAN_POINT ( 'NONE',  ( 103.9451733683222443, 237.4865022471903160, 10.00000000000009237 ) ) ;
#31317 = CARTESIAN_POINT ( 'NONE',  ( 18.62362889609498851, 174.8927522451418213, -10.00000000000009237 ) ) ;
#31318 = EDGE_CURVE ( 'NONE', #57035, #42320, #85346, .T. ) ;
#31319 = CARTESIAN_POINT ( 'NONE',  ( 164.2723164851102808, 246.1189969011916503, -1.993789335506892302 ) ) ;
#31320 = ORIENTED_EDGE ( 'NONE', *, *, #61576, .T. ) ;
#31321 = VECTOR ( 'NONE', #100120, 1000.000000000000000 ) ;
#31322 = CARTESIAN_POINT ( 'NONE',  ( 76.93135750435078535, 49.70919492771366777, 15.06818509151668195 ) ) ;
#31323 = CARTESIAN_POINT ( 'NONE',  ( 82.62974588365311490, 53.86145749464595411, 15.83045060744369970 ) ) ;
#31324 = EDGE_LOOP ( 'NONE', ( #37563, #99329, #87977, #94808 ) ) ;
#31325 = CARTESIAN_POINT ( 'NONE',  ( 206.8775514429320026, 272.3245652858344670, -9.838455694836268250 ) ) ;
#31326 = CARTESIAN_POINT ( 'NONE',  ( 186.8361490887116645, 276.6032954149434886, -17.09107860825236713 ) ) ;
#31327 = CARTESIAN_POINT ( 'NONE',  ( 68.60042634697137487, 68.76562077347861646, -6.227687874156614178 ) ) ;
#31328 = VERTEX_POINT ( 'NONE', #20696 ) ;
#31329 = CARTESIAN_POINT ( 'NONE',  ( 173.4028078701637696, 251.4564948467337047, 0.3090336303432728027 ) ) ;
#31331 = ORIENTED_EDGE ( 'NONE', *, *, #8357, .T. ) ;
#31330 = VECTOR ( 'NONE', #44618, 1000.000000000000227 ) ;
#31333 = ADVANCED_FACE ( 'NONE', ( #68271 ), #51584, .T. ) ;
#31332 = DIRECTION ( 'NONE',  ( -0.3766285016932175989, 0.9263643838751153270, 0.000000000000000000 ) ) ;
#31334 = CARTESIAN_POINT ( 'NONE',  ( 148.1632261683078013, 274.0207597936089883, -7.853210555358286271 ) ) ;
#31335 = B_SPLINE_CURVE_WITH_KNOTS ( 'NONE', 3,
 ( #80917, #3863, #11488, #19083 ),
 .UNSPECIFIED., .F., .F.,
 ( 4, 4 ),
 ( 0.007733555512259023858, 0.01590650797624234419 ),
 .UNSPECIFIED. ) ;
#31336 = CARTESIAN_POINT ( 'NONE',  ( -44.74834796241764678, 29.05375577536864995, -10.00000000000000000 ) ) ;
#31337 = ORIENTED_EDGE ( 'NONE', *, *, #48446, .T. ) ;
#31338 = CARTESIAN_POINT ( 'NONE',  ( 19.72598728594001116, 34.49540643055188127, 3.479690158560446702E-15 ) ) ;
#31339 = CARTESIAN_POINT ( 'NONE',  ( 75.04415442720188878, 55.04612442798951832, 16.14546943093221287 ) ) ;
#31340 = DIRECTION ( 'NONE',  ( -0.8660254037844387076, -0.4999999999999998890, -0.000000000000000000 ) ) ;
#31341 = CARTESIAN_POINT ( 'NONE',  ( 75.17086645518898536, 66.39979144248444243, -13.15673120748005154 ) ) ;
#31342 = EDGE_CURVE ( 'NONE', #71334, #8428, #35674, .T. ) ;
#31343 = ORIENTED_EDGE ( 'NONE', *, *, #2190, .T. ) ;
#31344 = CARTESIAN_POINT ( 'NONE',  ( 130.0937757410490576, 257.4637435831425023, 2.679491924311251605 ) ) ;
#31345 = CARTESIAN_POINT ( 'NONE',  ( -9.233521592304517966, 172.1427522451419065, 10.00000000000009415 ) ) ;
#31346 = VERTEX_POINT ( 'NONE', #21686 ) ;
#31347 = CARTESIAN_POINT ( 'NONE',  ( 170.8837800509748490, 284.6422579550419982, 10.91543698957328701 ) ) ;
#31349 = CARTESIAN_POINT ( 'NONE',  ( 67.70479547160532263, 65.84759395738886667, -10.55275263577380862 ) ) ;
#31348 = CARTESIAN_POINT ( 'NONE',  ( 67.78299301307349367, 65.68149062186182618, 10.02826371555679152 ) ) ;
#31350 = CARTESIAN_POINT ( 'NONE',  ( 81.63285811411603277, 55.18114913913488806, -15.91372994156266962 ) ) ;
#31351 = CARTESIAN_POINT ( 'NONE',  ( 204.2799274532736433, 276.8237820148827950, 13.55359442435934803 ) ) ;
#31352 = CARTESIAN_POINT ( 'NONE',  ( 185.4129985849131401, 292.6123411851212381, -10.72120707279806417 ) ) ;
#31353 = CARTESIAN_POINT ( 'NONE',  ( 204.7519188734507622, 276.0062688943993408, -12.76027478560537531 ) ) ;
#31354 = CARTESIAN_POINT ( 'NONE',  ( 131.5133883985292016, 255.9244531367911293, -4.594050593750046652 ) ) ;
#31355 = CARTESIAN_POINT ( 'NONE',  ( 203.2786752506974040, 268.5145164534344531, 2.480206815910183771 ) ) ;
#31356 = CARTESIAN_POINT ( 'NONE',  ( 182.0609731580854316, 260.3214751816357193, 9.357376519101284984 ) ) ;
#31357 = CARTESIAN_POINT ( 'NONE',  ( 77.03558525930309031, 203.0327760586659451, 1.948934522072303157E-15 ) ) ;
#31358 = ORIENTED_EDGE ( 'NONE', *, *, #10713, .F. ) ;
#31359 = CARTESIAN_POINT ( 'NONE',  ( 150.8359915840788688, 269.3913942967808453, 15.73449616766854575 ) ) ;
#31360 = CARTESIAN_POINT ( 'NONE',  ( -132.5954152546898115, 108.6868197944956478, 37.50000000000002132 ) ) ;
#31361 = ORIENTED_EDGE ( 'NONE', *, *, #21352, .F. ) ;
#31362 = CARTESIAN_POINT ( 'NONE',  ( 157.4853229503657133, 257.8744145340106684, -17.61474390190301165 ) ) ;
#31363 = EDGE_LOOP ( 'NONE', ( #33776, #10562, #44793, #33425 ) ) ;
#31364 = VERTEX_POINT ( 'NONE', #22181 ) ;
#31365 = CARTESIAN_POINT ( 'NONE',  ( 80.20857538931046804, 44.21345027830163588, -11.30608575784165026 ) ) ;
#31366 = CARTESIAN_POINT ( 'NONE',  ( 7.864685750751951865, 30.05722773587472219, -10.00000000000000000 ) ) ;
#31367 = CARTESIAN_POINT ( 'NONE',  ( 147.3047606266276546, 275.5076657283461827, -0.02269072295920609994 ) ) ;
#31368 = DIRECTION ( 'NONE',  ( -0.8660254037844378194, -0.5000000000000014433, -0.000000000000000000 ) ) ;
#31369 = DIRECTION ( 'NONE',  ( -0.8660254037844387076, -0.4999999999999998890, -0.000000000000000000 ) ) ;
#31370 = CARTESIAN_POINT ( 'NONE',  ( 162.4263297320084121, 249.3163397476629086, 11.18012070315788087 ) ) ;
#31371 = CARTESIAN_POINT ( 'NONE',  ( 85.53328598605538957, 214.0643266524159856, -9.188101187500093303 ) ) ;
#31372 = ORIENTED_EDGE ( 'NONE', *, *, #63416, .F. ) ;
#31373 = EDGE_LOOP ( 'NONE', ( #27613, #15634, #36070, #36755 ) ) ;
#31374 = CARTESIAN_POINT ( 'NONE',  ( 200.3152516538017380, 283.6908019351069470, -17.43933074397117977 ) ) ;
#31375 = ORIENTED_EDGE ( 'NONE', *, *, #12355, .F. ) ;
#31376 = ADVANCED_FACE ( 'NONE', ( #12606 ), #60921, .F. ) ;
#31377 = B_SPLINE_CURVE_WITH_KNOTS ( 'NONE', 3,
 ( #61428, #92381, #22930, #29063 ),
 .UNSPECIFIED., .F., .F.,
 ( 4, 4 ),
 ( 0.0001207921824033371633, 0.005340818303214702259 ),
 .UNSPECIFIED. ) ;
#31378 = CARTESIAN_POINT ( 'NONE',  ( 76.01947567912945658, 65.31078134063972129, -14.44091581795174051 ) ) ;
#31379 = CARTESIAN_POINT ( 'NONE',  ( 165.0308887387863876, 244.8051112166122891, 1.948365933089477808 ) ) ;
#31380 = CARTESIAN_POINT ( 'NONE',  ( 161.5731931013706628, 284.2088213097117091, 0.5314451569754123916 ) ) ;
#31381 = CARTESIAN_POINT ( 'NONE',  ( 207.3988330342936877, 270.8564699888902396, -1.301389719878858875 ) ) ;
#31382 = CARTESIAN_POINT ( 'NONE',  ( 200.0394048839106347, 267.9517317495682960, -8.074306449384252460 ) ) ;
#31383 = ORIENTED_EDGE ( 'NONE', *, *, #14166, .T. ) ;
#31384 = CARTESIAN_POINT ( 'NONE',  ( 83.53255499166944276, 43.67462638228406036, -7.537004589607056104 ) ) ;
#31385 = CARTESIAN_POINT ( 'NONE',  ( -27.42236680055714260, 166.5217562850347406, 1.224646799147364892E-15 ) ) ;
#31386 = CARTESIAN_POINT ( 'NONE',  ( 157.2948870673828026, 280.9759411348209142, 6.053012778684776940 ) ) ;
#31387 = CARTESIAN_POINT ( 'NONE',  ( 152.6740002182599767, 266.2078699576288159, -17.16212636348624088 ) ) ;
#31388 = CARTESIAN_POINT ( 'NONE',  ( 43.25185672232382217, 62.35734246106904521, -10.00000000000000000 ) ) ;
#31389 = AXIS2_PLACEMENT_3D ( 'NONE', #10277, #33067, #25985 ) ;
#31390 = CARTESIAN_POINT ( 'NONE',  ( 68.89583508828081904, 67.43123359013807772, -8.727553619782785432 ) ) ;
#31391 = ORIENTED_EDGE ( 'NONE', *, *, #36249, .F. ) ;
#31392 = CARTESIAN_POINT ( 'NONE',  ( 196.3606441383045649, 265.7307755575039323, 4.429610383328119738 ) ) ;
#31393 = LINE ( 'NONE', #76517, #64469 ) ;
#31394 = CARTESIAN_POINT ( 'NONE',  ( -75.57215499213535281, 50.95729256953105590, -10.00000000000000000 ) ) ;
#31395 = CARTESIAN_POINT ( 'NONE',  ( 187.8316118507717079, 266.3710757443984107, -12.34398216243838320 ) ) ;
#31396 = CARTESIAN_POINT ( 'NONE',  ( 83.78171082742430542, 51.97306301863908828, 14.95037678041455109 ) ) ;
#31397 = PLANE ( 'NONE',  #73712 ) ;
#31398 = ORIENTED_EDGE ( 'NONE', *, *, #80226, .F. ) ;
#31399 = EDGE_CURVE ( 'NONE', #41212, #73983, #13431, .T. ) ;
#31400 = CARTESIAN_POINT ( 'NONE',  ( 162.6476498368881494, 248.9330020812748785, 10.75824100428386743 ) ) ;
#31401 = CARTESIAN_POINT ( 'NONE',  ( -30.62386769735030256, 61.69365454717127051, -10.00000000000000000 ) ) ;
#31404 = CARTESIAN_POINT ( 'NONE',  ( 73.61770819056830817, 55.44860389765071318, 16.11080357623078640 ) ) ;
#31403 = B_SPLINE_CURVE_WITH_KNOTS ( 'NONE', 3,
 ( #96600, #89985, #51441, #49954, #27666, #89032, #80911, #19581, #4351, #5352, #20066, #35246, #58534, #12974, #12466, #43835, #36233, #98061, #57036, #88019, #18568, #75759, #22032, #5844 ),
 .UNSPECIFIED., .F., .F.,
 ( 4, 2, 2, 2, 2, 2, 2, 2, 2, 2, 2, 4 ),
 ( 1.440969542111313559E-17, 0.0003279589196580527753, 0.0006559178393160911306, 0.0009838767589741292691, 0.001311835678632167733, 0.001639794598290206197, 0.001967753517948244227, 0.002623671357264322455, 0.003279589196580400684, 0.003935507035896478045, 0.004591424875212556274, 0.005247342714528634502 ),
 .UNSPECIFIED. ) ;
#31402 = DIRECTION ( 'NONE',  ( -0.3473448497826262527, 0.9377374661009790779, 0.000000000000000000 ) ) ;
#31405 = CARTESIAN_POINT ( 'NONE',  ( 176.1389927384235534, 285.2568696065857239, -12.19707684924138036 ) ) ;
#31406 = EDGE_CURVE ( 'NONE', #57607, #42192, #39349, .T. ) ;
#31407 = CARTESIAN_POINT ( 'NONE',  ( 31.17504386912796477, 20.12755873383627758, -6.180339887498949025 ) ) ;
#31408 = CYLINDRICAL_SURFACE ( 'NONE', #87005, 70.00000000000002842 ) ;
#31409 = CARTESIAN_POINT ( 'NONE',  ( 86.13879346367242817, 46.95025718893441535, -10.63009676298478823 ) ) ;
#31410 = CARTESIAN_POINT ( 'NONE',  ( 192.2417256132786179, 262.2162190891563682, 3.002089893086772765 ) ) ;
#31411 = EDGE_CURVE ( 'NONE', #52271, #53961, #35641, .T. ) ;
#31412 = CARTESIAN_POINT ( 'NONE',  ( 5.317335864756744357, 180.0024278399160949, -9.188101187500093303 ) ) ;
#31413 = DIRECTION ( 'NONE',  ( -0.8903844177683323258, -0.4552093898365321412, 0.000000000000000000 ) ) ;
#31414 = ORIENTED_EDGE ( 'NONE', *, *, #33215, .F. ) ;
#31415 = DIRECTION ( 'NONE',  ( -0.8660254037844387076, -0.4999999999999998890, -0.000000000000000000 ) ) ;
#31416 = CARTESIAN_POINT ( 'NONE',  ( 198.0816276881963915, 264.5915495180347534, -1.723934393811154182E-14 ) ) ;
#31417 = CARTESIAN_POINT ( 'NONE',  ( -65.66987298107781612, 17.49999999999999645, 59.99999999999999289 ) ) ;
#31418 = CARTESIAN_POINT ( 'NONE',  ( 24.66750420662404508, 194.2369531367911293, -4.594050593750048428 ) ) ;
#31419 = CARTESIAN_POINT ( 'NONE',  ( 31.58830253577720626, 26.43677371833803846, -10.00000000000000355 ) ) ;
#31420 = CARTESIAN_POINT ( 'NONE',  ( 84.50369441069709353, 42.22801554421776160, -2.143854648006744856 ) ) ;
#31421 = CARTESIAN_POINT ( 'NONE',  ( 147.1259762202154207, 275.8173294038533641, -0.6716460511724978710 ) ) ;
#31422 = CARTESIAN_POINT ( 'NONE',  ( 140.7332108297008517, 245.3927522451417929, -10.00000000000009237 ) ) ;
#31423 = CARTESIAN_POINT ( 'NONE',  ( 87.17616255865019070, 46.12350222913486419, -8.288611607450606655 ) ) ;
#31424 = CARTESIAN_POINT ( 'NONE',  ( 187.5207547097004692, 259.2518634157261204, -0.7857520814055728442 ) ) ;
#31425 = CARTESIAN_POINT ( 'NONE',  ( 71.18054559181101126, 205.2365022471902023, 10.00000000000009592 ) ) ;
#31426 = CARTESIAN_POINT ( 'NONE',  ( 73.10444574000553075, 66.28578448752213603, -12.33233823302241028 ) ) ;
#31427 = EDGE_CURVE ( 'NONE', #99896, #88304, #32783, .T. ) ;
#31428 = CARTESIAN_POINT ( 'NONE',  ( 204.7788459716290390, 270.7538572138115569, 6.060631932661717514 ) ) ;
#31429 = CARTESIAN_POINT ( 'NONE',  ( 26.91401791951368949, 186.3458772461660544, 9.188101187500095079 ) ) ;
#31430 = CARTESIAN_POINT ( 'NONE',  ( 70.50721453739950562, 70.25575512013267598, -6.612918012354620068 ) ) ;
#31431 = CARTESIAN_POINT ( 'NONE',  ( 73.84283235153957037, 201.8932355074535963, -2.679491924311248496 ) ) ;
#31432 = DIRECTION ( 'NONE',  ( 0.9659258262891203817, -0.2588190451023261174, 0.000000000000000000 ) ) ;
#31433 = CARTESIAN_POINT ( 'NONE',  ( 67.41248320326424448, 66.37693208286884783, -8.946798147498737919 ) ) ;
#31434 = LINE ( 'NONE', #62328, #68546 ) ;
#31435 = B_SPLINE_CURVE_WITH_KNOTS ( 'NONE', 3,
 ( #67317, #68314, #29823, #76913, #91656, #90680, #21236, #22728, #60697, #22221 ),
 .UNSPECIFIED., .F., .F.,
 ( 4, 2, 2, 2, 4 ),
 ( 0.000000000000000000, 0.2499999999999997780, 0.4999999999999998890, 0.7500000000000000000, 1.000000000000000000 ),
 .UNSPECIFIED. ) ;
#31436 = CARTESIAN_POINT ( 'NONE',  ( 159.9092487632085238, 278.3844945790232828, -10.24712064432635472 ) ) ;
#31437 = FACE_OUTER_BOUND ( 'NONE', #49250, .T. ) ;
#31438 = CONTEXT_DEPENDENT_SHAPE_REPRESENTATION ( #75776, #3881 ) ;
#31439 = CARTESIAN_POINT ( 'NONE',  ( 16.63655203261577498, 31.64646525600389637, -2.839279412974133887 ) ) ;
#31440 = DIRECTION ( 'NONE',  ( -0.9414334852479518956, -0.3371987438498165734, 0.000000000000000000 ) ) ;
#31441 = CARTESIAN_POINT ( 'NONE',  ( 71.66445348058819320, 59.04578686578420132, 15.35137124261116348 ) ) ;
#31442 = CARTESIAN_POINT ( 'NONE',  ( 188.8930654812573380, 270.1357654272443938, -15.31858714226914486 ) ) ;
#31443 = ORIENTED_EDGE ( 'NONE', *, *, #16098, .F. ) ;
#31444 = CARTESIAN_POINT ( 'NONE',  ( 39.30595310148520838, 34.64441083166263979, -10.00000000000000533 ) ) ;
#31445 = CARTESIAN_POINT ( 'NONE',  ( 9.401013375279877238, 17.37878583063838889, 9.188101187500006262 ) ) ;
#31446 = CARTESIAN_POINT ( 'NONE',  ( 75.35748313534503495, 53.53391244244795644, -16.04435529155647089 ) ) ;
#31447 = CARTESIAN_POINT ( 'NONE',  ( 74.69440617789626913, 59.37262990323052492, -15.74149122071481699 ) ) ;
#31448 = CARTESIAN_POINT ( 'NONE',  ( 88.22748190676185231, 44.35111709898976784, 2.597852402453839638 ) ) ;
#31449 = VERTEX_POINT ( 'NONE', #43225 ) ;
#31450 = CARTESIAN_POINT ( 'NONE',  ( -27.42236680055714260, 166.5217562850347406, 1.224646799147364892E-15 ) ) ;
#31451 = CARTESIAN_POINT ( 'NONE',  ( 72.56229913925623976, 71.29878675843531255, -6.010006885656266284 ) ) ;
#31452 = CARTESIAN_POINT ( 'NONE',  ( 151.0715479399129606, 268.9833987204304435, 14.24612252017116987 ) ) ;
#31453 = CARTESIAN_POINT ( 'NONE',  ( 87.63170318219837895, 44.36446170533411504, -4.079950490519347106 ) ) ;
#31454 = VECTOR ( 'NONE', #35297, 1000.000000000000114 ) ;
#31455 = ORIENTED_EDGE ( 'NONE', *, *, #78752, .F. ) ;
#31456 = ORIENTED_EDGE ( 'NONE', *, *, #90945, .T. ) ;
#31458 = CARTESIAN_POINT ( 'NONE',  ( 84.26179751283029873, 42.61849302290659836, -4.369886972103340206 ) ) ;
#31457 = CARTESIAN_POINT ( 'NONE',  ( 67.11110063547383220, 69.33978020239571549, 3.973669838717296177 ) ) ;
#31459 = ORIENTED_EDGE ( 'NONE', *, *, #7409, .F. ) ;
#31460 = CARTESIAN_POINT ( 'NONE',  ( 190.8623743139412454, 300.0636657654615647, 8.577953960666059530 ) ) ;
#31461 = CARTESIAN_POINT ( 'NONE',  ( 72.41389820116259557, 70.72247311216293042, 7.745007521649655224 ) ) ;
#31462 = CARTESIAN_POINT ( 'NONE',  ( 72.85370133302119200, 56.82307610116442476, -15.94993432694561619 ) ) ;
#31463 = CARTESIAN_POINT ( 'NONE',  ( 76.62859868508415673, 63.47930858090246176, 15.36151106740648409 ) ) ;
#31464 = CARTESIAN_POINT ( 'NONE',  ( 148.1634546024981205, 274.0203641339852538, 9.324875965062235039 ) ) ;
#31465 = AXIS2_PLACEMENT_3D ( 'NONE', #11832, #4206, #66012 ) ;
#31466 = EDGE_CURVE ( 'NONE', #33264, #91209, #34066, .T. ) ;
#31467 = ORIENTED_EDGE ( 'NONE', *, *, #83687, .T. ) ;
#31468 = DIRECTION ( 'NONE',  ( 0.5000000000000014433, -0.8660254037844378194, 0.000000000000000000 ) ) ;
#31469 = CARTESIAN_POINT ( 'NONE',  ( 161.8330907632800404, 267.0924558059494416, 16.50031884935262028 ) ) ;
#31470 = VERTEX_POINT ( 'NONE', #54303 ) ;
#31471 = CARTESIAN_POINT ( 'NONE',  ( 25.29680607046014984, 36.64646525600391413, -2.839279412974133887 ) ) ;
#31472 = CARTESIAN_POINT ( 'NONE',  ( 190.7862358025146534, 300.1955415356651429, 3.573119809004446257 ) ) ;
#31473 = CARTESIAN_POINT ( 'NONE',  ( 78.23551423149454820, 47.47004208817780579, -13.80088926432411078 ) ) ;
#31474 = ORIENTED_EDGE ( 'NONE', *, *, #28507, .F. ) ;
#31475 = FACE_OUTER_BOUND ( 'NONE', #87869, .T. ) ;
#31476 = CARTESIAN_POINT ( 'NONE',  ( 159.6430037033188114, 255.2459832026828224, 16.03379434140432735 ) ) ;
#31477 = CARTESIAN_POINT ( 'NONE',  ( 150.6051381537932343, 269.7912441671369947, 13.72054362922755999 ) ) ;
#31478 = CARTESIAN_POINT ( 'NONE',  ( 83.80070905581447960, 52.11257540518899134, 14.61422408426159514 ) ) ;
#31479 = VERTEX_POINT ( 'NONE', #22918 ) ;
#31480 = ORIENTED_EDGE ( 'NONE', *, *, #25860, .T. ) ;
#31481 = CARTESIAN_POINT ( 'NONE',  ( 72.24154989827734141, 59.25143648895021897, -15.38920633486964462 ) ) ;
#31482 = B_SPLINE_CURVE_WITH_KNOTS ( 'NONE', 3,
 ( #26828, #4515, #57707, #35415 ),
 .UNSPECIFIED., .F., .F.,
 ( 4, 4 ),
 ( 0.005796625092869264924, 0.01143961042366389153 ),
 .UNSPECIFIED. ) ;
#31483 = CARTESIAN_POINT ( 'NONE',  ( 190.1635032421960148, 301.2741459696644029, -5.047660290019184259 ) ) ;
#31484 = CARTESIAN_POINT ( 'NONE',  ( 189.8147415777049218, 301.8782188922952514, -0.5019643756309712934 ) ) ;
#31485 = EDGE_LOOP ( 'NONE', ( #88479, #99763, #87898, #58493 ) ) ;
#31486 = CARTESIAN_POINT ( 'NONE',  ( 190.6094661480870798, 300.5017155583701083, 4.598210453186021951 ) ) ;
#31487 = CARTESIAN_POINT ( 'NONE',  ( 157.1378598138013558, 259.5494816622388612, -17.27281705625119912 ) ) ;
#31488 = CARTESIAN_POINT ( 'NONE',  ( 191.0626252760453383, 299.7168209248331436, 8.862249628642642207 ) ) ;
#31489 = CARTESIAN_POINT ( 'NONE',  ( 147.5749398328735822, 275.0397016159798227, -4.620786157167191099 ) ) ;
#31490 = CARTESIAN_POINT ( 'NONE',  ( 163.6900654399419466, 257.4571500704111600, 15.51179371342129620 ) ) ;
#31491 = CARTESIAN_POINT ( 'NONE',  ( 71.27261462778223233, 70.10394064289017990, 6.818682661097508202 ) ) ;
#31492 = CARTESIAN_POINT ( 'NONE',  ( 205.7639495959071212, 274.2533802642843170, 10.79039487422292432 ) ) ;
#31493 = CARTESIAN_POINT ( 'NONE',  ( 67.47735244041156477, 66.63445412725755546, 8.643438539336665727 ) ) ;
#31494 = CARTESIAN_POINT ( 'NONE',  ( 71.45656473000614994, 65.30002271808615433, -12.31008476486731418 ) ) ;
#31495 = CARTESIAN_POINT ( 'NONE',  ( 78.23831993261968876, 47.47892751676445755, 14.35468016619520881 ) ) ;
#31496 = CARTESIAN_POINT ( 'NONE',  ( 105.1810637865323628, 231.5333772461660828, 9.188101187500095079 ) ) ;
#31497 = EDGE_LOOP ( 'NONE', ( #60724, #5969, #99816, #46740 ) ) ;
#31498 = CARTESIAN_POINT ( 'NONE',  ( 146.6647111637776106, 276.6162639173599587, -0.6373001129109082674 ) ) ;
#31499 = CARTESIAN_POINT ( 'NONE',  ( 83.81364139273995306, 41.70719278157028498, -0.8692552194661639087 ) ) ;
#31500 = CARTESIAN_POINT ( 'NONE',  ( 192.9064638172013417, 270.9369261147751331, 14.92505667092759758 ) ) ;
#31501 = FACE_OUTER_BOUND ( 'NONE', #99416, .T. ) ;
#31502 = CARTESIAN_POINT ( 'NONE',  ( 183.2940791498508872, 284.7098848858684619, -14.97307289601423186 ) ) ;
#31503 = CARTESIAN_POINT ( 'NONE',  ( 83.82917762730355093, 51.97629592023758249, -14.94018958758825022 ) ) ;
#31504 = CARTESIAN_POINT ( 'NONE',  ( 165.6569603496038496, 284.1908122977653761, -8.522347108096667512 ) ) ;
#31505 = ORIENTED_EDGE ( 'NONE', *, *, #10886, .T. ) ;
#31506 = DIRECTION ( 'NONE',  ( 0.6758705274779382988, 0.2489746672676192429, 0.6936934806855775681 ) ) ;
#31507 = CARTESIAN_POINT ( 'NONE',  ( 72.29720748969889144, 71.75793896413090067, 5.568862843245728556 ) ) ;
#31508 = CARTESIAN_POINT ( 'NONE',  ( 206.3117289818846700, 272.0185653065639713, 8.038418397519199843 ) ) ;
#31509 = CARTESIAN_POINT ( 'NONE',  ( 127.4808708382166316, 256.6589784336661637, -6.496448406907676862E-16 ) ) ;
#31510 = CARTESIAN_POINT ( 'NONE',  ( 110.0000000000000000, 0.000000000000000000, -9.212605237762131694 ) ) ;
#31511 = CARTESIAN_POINT ( 'NONE',  ( 188.5613127796079880, 298.7266913302852345, 4.776745480473671535 ) ) ;
#31512 = CARTESIAN_POINT ( 'NONE',  ( 196.3519702320103590, 290.5554067223432639, 17.39042812051341969 ) ) ;
#31513 = DIRECTION ( 'NONE',  ( -0.5078630399532131356, -0.8614378286617561109, 0.000000000000000000 ) ) ;
#31514 = B_SPLINE_CURVE_WITH_KNOTS ( 'NONE', 3,
 ( #25823, #93749, #57186, #55674, #64304, #16701, #95255, #18713, #94241, #86661, #56699, #72933, #71919, #64811, #17193, #87680, #33403, #9627, #62792, #18215, #40973, #80550, #41487, #40488, #72433, #49107, #87177, #17713, #71418, #80044, #70915, #47593, #9106, #63801, #10611, #33926, #48614, #95759, #32894, #26311, #41997, #32402, #88165, #49595, #63299, #94735 ),
 .UNSPECIFIED., .F., .F.,
 ( 4, 1, 2, 2, 1, 2, 2, 1, 1, 2, 2, 1, 1, 2, 2, 1, 1, 2, 2, 1, 1, 1, 2, 2, 1, 1, 1, 2, 2, 4 ),
 ( 0.000000000000000000, 0.06249999999998799571, 0.09374999999998243072, 0.1249999999999768796, 0.1874999999999684974, 0.2187499999999658606, 0.2499999999999632516, 0.3124999999999567013, 0.3437499999999547029, 0.3593749999999529821, 0.3749999999999512057, 0.4374999999999458766, 0.4687499999999430456, 0.4843749999999430456, 0.4999999999999430456, 0.5624999999999473754, 0.5937499999999509281, 0.6093749999999535927, 0.6249999999999562572, 0.6874999999999649170, 0.7187499999999702460, 0.7343749999999733546, 0.7421874999999749090, 0.7499999999999764633, 0.8124999999999785727, 0.8437499999999796829, 0.8593749999999792388, 0.8671874999999796829, 0.8749999999999800160, 1.000000000000000000 ),
 .UNSPECIFIED. ) ;
#31515 = CARTESIAN_POINT ( 'NONE',  ( 41.36564329728401646, 200.8149278399160664, -9.188101187500095079 ) ) ;
#31516 = CARTESIAN_POINT ( 'NONE',  ( 69.37251848561912482, 66.28420332388499503, -10.39712879372465437 ) ) ;
#31517 = EDGE_LOOP ( 'NONE', ( #8826, #14343, #40836, #52800 ) ) ;
#31518 = DIRECTION ( 'NONE',  ( 0.000000000000000000, -0.000000000000000000, -1.000000000000000000 ) ) ;
#31519 = CARTESIAN_POINT ( 'NONE',  ( 87.70233365940427461, 44.37954158847006170, -4.000613605175061593 ) ) ;
#31520 = EDGE_CURVE ( 'NONE', #92543, #18551, #78894, .T. ) ;
#31521 = DIRECTION ( 'NONE',  ( -0.8660254037844378194, -0.5000000000000013323, -0.000000000000000000 ) ) ;
#31522 = CARTESIAN_POINT ( 'NONE',  ( 174.5201653990494322, 262.1690094913359985, 14.32490148041052258 ) ) ;
#31523 = CARTESIAN_POINT ( 'NONE',  ( 82.13606007655464225, 41.45974715720112869, -5.928773293604740147 ) ) ;
#31524 = CIRCLE ( 'NONE', #39539, 0.1418229129680897982 ) ;
#31525 = CARTESIAN_POINT ( 'NONE',  ( 202.8874463667715133, 279.2356300052831557, -15.29930322226033468 ) ) ;
#31526 = EDGE_CURVE ( 'NONE', #3615, #92554, #53805, .T. ) ;
#31527 = CARTESIAN_POINT ( 'NONE',  ( 10.68506269473756909, 183.6427522451419350, -10.00000000000009592 ) ) ;
#31528 =( BOUNDED_CURVE ( )  B_SPLINE_CURVE ( 2, ( #48292, #87374, #93425, #2204, #70070, #9810, #685, #48800, #32586, #79238, #92913, #71607, #23977 ),
 .UNSPECIFIED., .F., .T. ) 
 B_SPLINE_CURVE_WITH_KNOTS ( ( 3, 2, 2, 2, 2, 2, 3 ),
 ( 0.5875000000000000222, 0.5899999999999999689, 0.5949999999999999734, 0.5999999999999999778, 0.6049999999999999822, 0.6099999999999999867, 0.6125000000000000444 ),
 .UNSPECIFIED. ) 
 CURVE ( )  GEOMETRIC_REPRESENTATION_ITEM ( )  RATIONAL_B_SPLINE_CURVE ( ( 0.9755282581475767101, 0.9755282581475772652, 1.000000000000000000, 0.9510565162951535312, 1.000000000000000000, 0.9510565162951535312, 1.000000000000000000, 0.9510565162951535312, 1.000000000000000000, 0.9510565162951535312, 1.000000000000000000, 0.9755282581475761550, 0.9755282581475767101 ) ) 
 REPRESENTATION_ITEM ( '' )  );
#31529 = CARTESIAN_POINT ( 'NONE',  ( 100.8238734719678860, 239.0177522451419350, 5.000000000000046185 ) ) ;
#31530 = B_SPLINE_SURFACE_WITH_KNOTS ( 'NONE', 3, 1, ( 
 ( #56374, #2202 ),
 ( #1702, #86340 ),
 ( #79235, #95934 ),
 ( #87372, #64990 ),
 ( #72614, #63483 ),
 ( #32068, #64488 ),
 ( #10292, #41164 ),
 ( #94420, #2704 ),
 ( #9288, #18396 ),
 ( #57371, #72101 ),
 ( #70574, #56871 ),
 ( #40163, #62979 ),
 ( #16876, #3216 ),
 ( #34100, #71604 ),
 ( #33592, #39653 ),
 ( #88346, #71104 ),
 ( #95449, #9807 ),
 ( #26000, #40667 ),
 ( #18905, #49781 ),
 ( #55360, #93926 ),
 ( #1191, #80740 ),
 ( #24481, #47762 ),
 ( #32585, #24974 ),
 ( #55851, #86846 ),
 ( #82227, #59345 ),
 ( #28465, #4172 ),
 ( #34578, #50274 ),
 ( #19416, #42171 ),
 ( #19894, #65976 ),
 ( #81226, #65478 ),
 ( #97891, #42658 ),
 ( #81718, #51262 ),
 ( #66962, #12800 ),
 ( #50766, #11802 ) ),
 .UNSPECIFIED., .T., .F., .F.,
 ( 4, 2, 2, 2, 2, 2, 2, 2, 2, 2, 2, 2, 2, 2, 2, 2, 4 ),
 ( 2, 2 ),
 ( 0.000000000000000000, 0.06250000000000000000, 0.1250000000000000000, 0.1875000000000000000, 0.2500000000000000000, 0.3125000000000000000, 0.3750000000000000000, 0.4375000000000000000, 0.5000000000000000000, 0.5625000000000000000, 0.6250000000000000000, 0.6875000000000000000, 0.7500000000000000000, 0.8125000000000000000, 0.8750000000000000000, 0.9375000000000000000, 1.000000000000000000 ),
 ( 0.000000000000000000, 1.000000000000000000 ),
 .UNSPECIFIED. ) ;
#31531 = EDGE_CURVE ( 'NONE', #88359, #49527, #59922, .T. ) ;
#31532 = CARTESIAN_POINT ( 'NONE',  ( 43.80372508975956691, 30.45404122711137163, -8.090169943749478065 ) ) ;
#31533 = VERTEX_POINT ( 'NONE', #52327 ) ;
#31534 = EDGE_CURVE ( 'NONE', #62259, #72718, #48059, .T. ) ;
#31535 = CARTESIAN_POINT ( 'NONE',  ( 203.0398866899141126, 278.9715956204779559, 16.57839218037009132 ) ) ;
#31536 = LINE ( 'NONE', #46744, #26985 ) ;
#31537 = CARTESIAN_POINT ( 'NONE',  ( 27.59033994439653270, 195.9244531367911293, -4.594050593750046652 ) ) ;
#31538 = CARTESIAN_POINT ( 'NONE',  ( 15.30702494462977370, 17.03677371833801146, 10.00000000000000533 ) ) ;
#31539 = CARTESIAN_POINT ( 'NONE',  ( 72.52865609843787809, 57.51546068812135815, 16.29679984377914437 ) ) ;
#31540 = FACE_OUTER_BOUND ( 'NONE', #88751, .T. ) ;
#31541 = DIRECTION ( 'NONE',  ( 0.000000000000000000, -0.000000000000000000, -1.000000000000000000 ) ) ;
#31543 = CARTESIAN_POINT ( 'NONE',  ( 62.85372508080289577, 219.3464784336661637, 1.353441290958777327E-15 ) ) ;
#31542 = CARTESIAN_POINT ( 'NONE',  ( 185.9406580756425171, 265.4572926502605128, 14.02042132963198817 ) ) ;
#31544 = CARTESIAN_POINT ( 'NONE',  ( 200.5438717407500917, 283.2948203288816558, 18.39667691545567152 ) ) ;
#31545 = CARTESIAN_POINT ( 'NONE',  ( 73.15257707569458034, 57.27860612637811499, 16.38974116562414451 ) ) ;
#31546 = LINE ( 'NONE', #60443, #29448 ) ;
#31547 = CARTESIAN_POINT ( 'NONE',  ( 19.02883662497902861, 11.39040679176981996, 1.333680081654574804E-15 ) ) ;
#31548 = ORIENTED_EDGE ( 'NONE', *, *, #34475, .T. ) ;
#31549 = CARTESIAN_POINT ( 'NONE',  ( 31.19903945042937821, 195.4865022471903160, 10.00000000000009237 ) ) ;
#31550 = LINE ( 'NONE', #48266, #64402 ) ;
#31551 = CARTESIAN_POINT ( 'NONE',  ( -11.27255005043015856, 173.4869531367911293, 4.594050593750046652 ) ) ;
#31552 = CARTESIAN_POINT ( 'NONE',  ( 25.38519627463738715, 32.84336893147757053, -7.433330006724137462 ) ) ;
#31553 = CARTESIAN_POINT ( 'NONE',  ( 200.4119102014255134, 282.6799346856502098, 16.91998934435313728 ) ) ;
#31554 = CARTESIAN_POINT ( 'NONE',  ( 185.3347439640575658, 260.3534090642163505, 6.375270193058597989 ) ) ;
#31555 = CARTESIAN_POINT ( 'NONE',  ( 205.8918578537579833, 274.0318366629789466, 11.52627491423194250 ) ) ;
#31556 = CARTESIAN_POINT ( 'NONE',  ( 186.9626043371740707, 259.3098172291293508, -2.387369219704509327 ) ) ;
#31557 = CARTESIAN_POINT ( 'NONE',  ( 65.82094082657513923, 68.94627234734062426, 2.288258256726706907 ) ) ;
#31558 = ORIENTED_EDGE ( 'NONE', *, *, #2518, .T. ) ;
#31559 = DIRECTION ( 'NONE',  ( -0.8660254037844387076, -0.4999999999999998890, -0.000000000000000000 ) ) ;
#31560 = CARTESIAN_POINT ( 'NONE',  ( 179.1598829120495964, 285.8685653680148562, 13.04984300519404528 ) ) ;
#31561 = CARTESIAN_POINT ( 'NONE',  ( 196.1370092075112268, 290.1209220278959720, 16.40156295354631411 ) ) ;
#31562 = CARTESIAN_POINT ( 'NONE',  ( 14.98925625915878435, 9.449665230724930254, -2.296566073217252530E-15 ) ) ;
#31563 = ORIENTED_EDGE ( 'NONE', *, *, #60680, .T. ) ;
#31564 = CARTESIAN_POINT ( 'NONE',  ( 71.90400658755810070, 72.53437165389429708, 1.750395423964772990 ) ) ;
#31565 = AXIS2_PLACEMENT_3D ( 'NONE', #817, #93556, #83468 ) ;
#31566 = CARTESIAN_POINT ( 'NONE',  ( 157.7593757092099906, 257.3997412317380054, -18.08445832352326121 ) ) ;
#31567 = CARTESIAN_POINT ( 'NONE',  ( 192.1149248854976861, 297.8941845364767005, 12.26771790733441314 ) ) ;
#31568 = DIRECTION ( 'NONE',  ( -0.000000000000000000, -0.000000000000000000, -1.000000000000000000 ) ) ;
#31569 = FACE_OUTER_BOUND ( 'NONE', #8298, .T. ) ;
#31570 = CARTESIAN_POINT ( 'NONE',  ( 207.6875671281972870, 270.9215769640275653, -2.211577121115235300 ) ) ;
#31571 = CARTESIAN_POINT ( 'NONE',  ( 200.9445292274600092, 282.6008612054670266, -16.62830946367346741 ) ) ;
#31572 = ORIENTED_EDGE ( 'NONE', *, *, #40587, .F. ) ;
#31573 = VERTEX_POINT ( 'NONE', #13836 ) ;
#31574 = CARTESIAN_POINT ( 'NONE',  ( 190.5573062922015026, 281.4271296422851947, 16.94287472538490391 ) ) ;
#31575 = CARTESIAN_POINT ( 'NONE',  ( 73.06786641563543583, 70.68483820275014295, 7.671292531139269677 ) ) ;
#31576 = VERTEX_POINT ( 'NONE', #85271 ) ;
#31577 = PLANE ( 'NONE',  #41841 ) ;
#31578 = CARTESIAN_POINT ( 'NONE',  ( -17.42236680055705023, 149.2012482093457777, 0.000000000000000000 ) ) ;
#31579 = VERTEX_POINT ( 'NONE', #37126 ) ;
#31580 = CARTESIAN_POINT ( 'NONE',  ( 146.5157004908022031, 276.8743579738231233, -0.1877253132609108255 ) ) ;
#31581 = DIRECTION ( 'NONE',  ( -0.4924038765061016787, 0.8528685319524424990, -0.1736481776669404342 ) ) ;
#31582 = CARTESIAN_POINT ( 'NONE',  ( 149.6564118588553924, 271.4344863124460971, -11.76165597393390172 ) ) ;
#31583 = EDGE_CURVE ( 'NONE', #5590, #39677, #36621, .T. ) ;
#31584 = CARTESIAN_POINT ( 'NONE',  ( 21.35627990119762032, 12.73415679381821519, 1.333680081654574804E-15 ) ) ;
#31585 = ORIENTED_EDGE ( 'NONE', *, *, #40095, .T. ) ;
#31586 = CARTESIAN_POINT ( 'NONE',  ( 161.4025183475459073, 251.0896330829197041, 14.50747140106038735 ) ) ;
#31587 = FACE_OUTER_BOUND ( 'NONE', #87883, .T. ) ;
#31588 = CARTESIAN_POINT ( 'NONE',  ( 33.26462506102002692, 34.90829794293883026, 10.00000000000000355 ) ) ;
#31589 = ORIENTED_EDGE ( 'NONE', *, *, #78353, .F. ) ;
#31590 = EDGE_LOOP ( 'NONE', ( #5000, #63608, #30495, #74661 ) ) ;
#31591 = ORIENTED_EDGE ( 'NONE', *, *, #37146, .T. ) ;
#31592 = CARTESIAN_POINT ( 'NONE',  ( 72.81511981781955001, 58.90692562186728765, 15.57534130551175799 ) ) ;
#31593 = VECTOR ( 'NONE', #61374, 1000.000000000000000 ) ;
#31594 = ORIENTED_EDGE ( 'NONE', *, *, #6093, .T. ) ;
#31595 = CARTESIAN_POINT ( 'NONE',  ( -10.54235908185773418, 24.92402704602492847, -10.00000000000000000 ) ) ;
#31596 = ORIENTED_EDGE ( 'NONE', *, *, #83747, .T. ) ;
#31597 = CARTESIAN_POINT ( 'NONE',  ( 163.8398374448017591, 246.8680725722146008, -5.948785025486735378 ) ) ;
#31598 = CARTESIAN_POINT ( 'NONE',  ( 81.98982836076474712, 58.71377021865833257, 0.05226423163382854647 ) ) ;
#31600 = EDGE_CURVE ( 'NONE', #51782, #100286, #6739, .T. ) ;
#31599 = CARTESIAN_POINT ( 'NONE',  ( 167.1501680486316559, 282.0009818228157314, 11.65768677921798790 ) ) ;
#31601 = CARTESIAN_POINT ( 'NONE',  ( 194.7900911235093133, 293.2606606935473792, -14.66228443412922999 ) ) ;
#31602 =( GEOMETRIC_REPRESENTATION_CONTEXT ( 3 ) GLOBAL_UNCERTAINTY_ASSIGNED_CONTEXT ( ( #55426 ) ) GLOBAL_UNIT_ASSIGNED_CONTEXT ( ( #56367, #57864, #51251 ) ) REPRESENTATION_CONTEXT ( 'NONE', 'WORKASPACE' ) );
#31603 = CARTESIAN_POINT ( 'NONE',  ( 82.37373412059557154, 53.49834611899161985, -15.77010555883211929 ) ) ;
#31604 = CARTESIAN_POINT ( 'NONE',  ( 87.10115137904762150, 45.28340438443854055, 6.995308688534716879 ) ) ;
#31605 = VERTEX_POINT ( 'NONE', #83775 ) ;
#31606 = CARTESIAN_POINT ( 'NONE',  ( 75.08189823614961256, 56.99527856207666332, -16.54286807313852137 ) ) ;
#31607 = CARTESIAN_POINT ( 'NONE',  ( 9.333682440526761326, 28.49540643055185640, 3.479690158560446702E-15 ) ) ;
#31608 = CYLINDRICAL_SURFACE ( 'NONE', #929, 17.82106496071139645 ) ;
#31609 = DIRECTION ( 'NONE',  ( 0.4999999999999992784, -0.8660254037844390407, 0.000000000000000000 ) ) ;
#31611 = VERTEX_POINT ( 'NONE', #44220 ) ;
#31610 = CARTESIAN_POINT ( 'NONE',  ( 198.2819808855875863, 287.2125302111982705, 18.53535247371401695 ) ) ;
#31612 = DIRECTION ( 'NONE',  ( -0.9689885751534038638, -0.2471055264905585858, 0.000000000000000000 ) ) ;
#31613 = CARTESIAN_POINT ( 'NONE',  ( 159.2713554375903300, 254.7809155221686410, -15.70062444474382168 ) ) ;
#31614 = DIRECTION ( 'NONE',  ( 1.000000000000000000, 0.000000000000000000, 0.000000000000000000 ) ) ;
#31615 = CARTESIAN_POINT ( 'NONE',  ( 81.70878797397156745, 46.02746657646116546, -11.49744158306595310 ) ) ;
#31616 = CARTESIAN_POINT ( 'NONE',  ( 171.6554683614685075, 255.1804135649609577, 10.96344727419213072 ) ) ;
#31617 = CARTESIAN_POINT ( 'NONE',  ( 190.8112310826165867, 262.0020291435678246, -0.6932856109839961034 ) ) ;
#31618 = VERTEX_POINT ( 'NONE', #84278 ) ;
#31619 = CARTESIAN_POINT ( 'NONE',  ( 154.9949866785712231, 262.1878034846902779, -17.93766467320931213 ) ) ;
#31620 = CARTESIAN_POINT ( 'NONE',  ( 128.5163324648304410, 256.5530062829863027, -4.648177544792955347E-16 ) ) ;
#31621 = DIRECTION ( 'NONE',  ( -0.000000000000000000, -0.000000000000000000, -1.000000000000000000 ) ) ;
#31622 = CARTESIAN_POINT ( 'NONE',  ( 23.74761253515288217, 184.5177522451418497, -10.00000000000009592 ) ) ;
#31623 = CARTESIAN_POINT ( 'NONE',  ( 88.50972766791687718, 234.1589784336661353, -6.496448406907676862E-16 ) ) ;
#31624 = CARTESIAN_POINT ( 'NONE',  ( 82.16355652963139278, 40.77362396971211922, -0.6832070566406561740 ) ) ;
#31625 = CARTESIAN_POINT ( 'NONE',  ( -22.42236680055709641, 157.8615022471902591, 0.000000000000000000 ) ) ;
#31626 = CARTESIAN_POINT ( 'NONE',  ( 167.0149686599001200, 278.0521133782755214, -13.60968902122515090 ) ) ;
#31627 = CARTESIAN_POINT ( 'NONE',  ( -67.91103796225580425, 44.10201266000169795, -10.00000000000000000 ) ) ;
#31629 = CARTESIAN_POINT ( 'NONE',  ( 75.60765592493140730, 65.32810859375902623, 14.31319638027754593 ) ) ;
#31628 = CARTESIAN_POINT ( 'NONE',  ( 7.969365115964081703, 187.6589784336661637, -6.496448406907675876E-16 ) ) ;
#31630 = CARTESIAN_POINT ( 'NONE',  ( 161.1884843536000744, 251.4603508349806873, 13.21272898143761942 ) ) ;
#31631 = VERTEX_POINT ( 'NONE', #77121 ) ;
#31632 = ORIENTED_EDGE ( 'NONE', *, *, #73080, .F. ) ;
#31633 = DIRECTION ( 'NONE',  ( 0.8660254037844341557, 0.5000000000000082157, -0.000000000000000000 ) ) ;
#31634 = CARTESIAN_POINT ( 'NONE',  ( 197.8141251302497778, 265.6821229749213558, -2.897974208861140433 ) ) ;
#31635 = EDGE_CURVE ( 'NONE', #12301, #41077, #27933, .T. ) ;
#31636 = CARTESIAN_POINT ( 'NONE',  ( 83.55900032775279840, 46.36886482531775044, -10.91248212791196615 ) ) ;
#31637 = AXIS2_PLACEMENT_3D ( 'NONE', #53907, #47317, #85897 ) ;
#31638 = CARTESIAN_POINT ( 'NONE',  ( 201.9906765889849112, 280.7888808231018061, -16.23360557870388732 ) ) ;
#31639 = CARTESIAN_POINT ( 'NONE',  ( 105.0176211588661772, 242.9860189848785126, -2.679491924311252493 ) ) ;
#31640 = CARTESIAN_POINT ( 'NONE',  ( 74.43794370846053710, 68.05007506763284653, -11.63842094426022555 ) ) ;
#31641 = CARTESIAN_POINT ( 'NONE',  ( 29.07873433320978052, 199.8464784336661637, 1.353441290958777525E-15 ) ) ;
#31642 = CARTESIAN_POINT ( 'NONE',  ( 199.0369196554013627, 277.3085947641471876, 15.18055274685867673 ) ) ;
#31643 = VERTEX_POINT ( 'NONE', #75158 ) ;
#31644 = CARTESIAN_POINT ( 'NONE',  ( 153.3257670986663470, 273.8331553043774989, -11.88532112633179594 ) ) ;
#31645 = ADVANCED_FACE ( 'NONE', ( #68527 ), #90891, .T. ) ;
#31646 = APPLICATION_CONTEXT ( 'automotive_design' ) ;
#31647 = CARTESIAN_POINT ( 'NONE',  ( 182.5436984794861814, 260.5467356096382900, -10.91178052607559046 ) ) ;
#31648 = CARTESIAN_POINT ( 'NONE',  ( 35.64779661956466583, 28.78052372038643369, -10.00000000000000355 ) ) ;
#31649 = LINE ( 'NONE', #15966, #50846 ) ;
#31650 = CARTESIAN_POINT ( 'NONE',  ( 194.2669918475045279, 294.1666952169902629, 14.00965265288584050 ) ) ;
#31651 = CARTESIAN_POINT ( 'NONE',  ( 207.1019571622349815, 271.9358831784929293, -5.989975140547304733 ) ) ;
#31652 = AXIS2_PLACEMENT_3D ( 'NONE', #75163, #98958, #14342 ) ;
#31653 = DIRECTION ( 'NONE',  ( -0.7499999999999993339, -0.4330127018922203530, -0.4999999999999999445 ) ) ;
#31654 = CARTESIAN_POINT ( 'NONE',  ( 147.7467138384290308, 274.7421803109381813, -9.190172068879620682 ) ) ;
#31655 = CARTESIAN_POINT ( 'NONE',  ( 189.2703867623931728, 262.7700255369126694, 8.020027416226151118 ) ) ;
#31656 = CARTESIAN_POINT ( 'NONE',  ( 167.9135783974399772, 278.5162520875397831, 14.81510772495481554 ) ) ;
#31657 = CARTESIAN_POINT ( 'NONE',  ( 192.5295226464411371, 265.2521209099669477, 8.400182565873334894 ) ) ;
#31658 = CARTESIAN_POINT ( 'NONE',  ( 146.7818291168261453, 276.4134096722012828, -0.7617065417431535534 ) ) ;
#31659 = CARTESIAN_POINT ( 'NONE',  ( -17.42236680055705023, 149.2012482093457777, 0.000000000000000000 ) ) ;
#31660 = CARTESIAN_POINT ( 'NONE',  ( 180.7783084174795079, 266.7965790172731886, -14.72117180798574232 ) ) ;
#31661 = ORIENTED_EDGE ( 'NONE', *, *, #7075, .F. ) ;
#31662 = CARTESIAN_POINT ( 'NONE',  ( 186.3032856786115303, 294.1815019053933611, 11.41626773807880468 ) ) ;
#31663 = CARTESIAN_POINT ( 'NONE',  ( 207.5570596878370679, 271.1476224814971374, 2.444960520848353358 ) ) ;
#31664 = CARTESIAN_POINT ( 'NONE',  ( 189.0720805967732758, 299.7343203868808246, 4.955419684386629164 ) ) ;
#31665 = CARTESIAN_POINT ( 'NONE',  ( 108.1307024963493149, 242.4244531367911293, -4.594050593750046652 ) ) ;
#31666 = CARTESIAN_POINT ( 'NONE',  ( 8.474262601947446072, 26.93396525600388713, 2.839279412974139660 ) ) ;
#31667 = CARTESIAN_POINT ( 'NONE',  ( 191.4941427383744781, 298.9694107557253346, 8.584406880462095657 ) ) ;
#31668 = CARTESIAN_POINT ( 'NONE',  ( 73.52895665835218608, 59.09902088736443915, -16.10230406680008741 ) ) ;
#31670 = CARTESIAN_POINT ( 'NONE',  ( 195.2304193712978986, 279.0657389023923542, 16.29610427727775246 ) ) ;
#31669 = CARTESIAN_POINT ( 'NONE',  ( 136.3105610988903607, 261.0530062829863027, -4.648177544792955347E-16 ) ) ;
#31671 = CARTESIAN_POINT ( 'NONE',  ( 150.4957438262301253, 269.9807207005363807, -15.25519111672087114 ) ) ;
#31672 = CARTESIAN_POINT ( 'NONE',  ( 192.1929114410880288, 263.4101189793182698, -4.344445731632683660 ) ) ;
#31673 = CARTESIAN_POINT ( 'NONE',  ( 149.9475948592590839, 271.6738979692356111, -11.66626220284549298 ) ) ;
#31674 = CARTESIAN_POINT ( 'NONE',  ( 58.02232427585079222, 192.7592609112379876, 2.679491924311254714 ) ) ;
#31675 = DIRECTION ( 'NONE',  ( -0.8660254037844387076, -0.4999999999999998890, -0.000000000000000000 ) ) ;
#31676 = CARTESIAN_POINT ( 'NONE',  ( 86.46502256137985398, 47.49784904624871729, 10.45499499417849876 ) ) ;
#31677 = ORIENTED_EDGE ( 'NONE', *, *, #50555, .F. ) ;
#31678 = FACE_OUTER_BOUND ( 'NONE', #21510, .T. ) ;
#31679 = CARTESIAN_POINT ( 'NONE',  ( 199.9984457123739503, 270.0849612724584290, 9.145354784334640996 ) ) ;
#31680 = CARTESIAN_POINT ( 'NONE',  ( 82.67070653882738895, 41.17429230206336399, 4.398717897525028064 ) ) ;
#31681 = CARTESIAN_POINT ( 'NONE',  ( 180.1105033416455967, 262.3445359189764190, -12.66037080800385084 ) ) ;
#31682 = CARTESIAN_POINT ( 'NONE',  ( -36.26652983198115976, 26.35523046909639078, -10.00000000000000000 ) ) ;
#31683 = LINE ( 'NONE', #14996, #16103 ) ;
#31684 = VERTEX_POINT ( 'NONE', #14336 ) ;
#31685 = CARTESIAN_POINT ( 'NONE',  ( 73.17900167297862879, 69.84980244707995212, 9.598651498403647508 ) ) ;
#31686 = CARTESIAN_POINT ( 'NONE',  ( 33.80247542503471436, 34.91421378149921395, 9.188101187500008038 ) ) ;
#31687 = ORIENTED_EDGE ( 'NONE', *, *, #82290, .F. ) ;
#31688 = CARTESIAN_POINT ( 'NONE',  ( 181.4735074999749145, 292.1586133693310785, 10.55809797880889001 ) ) ;
#31689 = CARTESIAN_POINT ( 'NONE',  ( 194.4032909867620447, 293.9306181827685123, -16.05392006271526384 ) ) ;
#31690 = CARTESIAN_POINT ( 'NONE',  ( 156.6941734481478079, 259.2447256682348211, 17.84224415335075520 ) ) ;
#31691 = VERTEX_POINT ( 'NONE', #99947 ) ;
#31692 = CARTESIAN_POINT ( 'NONE',  ( 79.58917286194427732, 59.33460254692537461, 16.56081879078485741 ) ) ;
#31693 = CARTESIAN_POINT ( 'NONE',  ( 159.1215725138524704, 256.7057375585948193, 16.87965583163218142 ) ) ;
#31694 = CARTESIAN_POINT ( 'NONE',  ( 193.0105523955311355, 296.3429121844422980, -12.00165843972855839 ) ) ;
#31695 = CARTESIAN_POINT ( 'NONE',  ( 19.73933908736162124, 30.13478043621388380, 8.090169943749478065 ) ) ;
#31697 = EDGE_CURVE ( 'NONE', #87618, #55881, #46204, .T. ) ;
#31696 = VECTOR ( 'NONE', #37356, 1000.000000000000114 ) ;
#31698 = CARTESIAN_POINT ( 'NONE',  ( 85.07340834217973224, 44.94014711221131364, -9.007945491601892840 ) ) ;
#31699 = CARTESIAN_POINT ( 'NONE',  ( 155.1865148098964937, 261.8560670301561686, -16.99758927948949605 ) ) ;
#31700 = VERTEX_POINT ( 'NONE', #45712 ) ;
#31701 = EDGE_CURVE ( 'NONE', #73884, #41027, #92859, .T. ) ;
#31702 = ORIENTED_EDGE ( 'NONE', *, *, #61148, .F. ) ;
#31704 = CIRCLE ( 'NONE', #88424, 0.1418229129681557177 ) ;
#31703 = LINE ( 'NONE', #8929, #93445 ) ;
#31705 = VERTEX_POINT ( 'NONE', #6231 ) ;
#31706 = CARTESIAN_POINT ( 'NONE',  ( 77.16425012238860859, 49.51985965088922370, -15.46725698127323945 ) ) ;
#31707 = ORIENTED_EDGE ( 'NONE', *, *, #39513, .T. ) ;
#31708 = CARTESIAN_POINT ( 'NONE',  ( 86.89657730260137214, 45.77512320498411214, -8.683907937581334835 ) ) ;
#31709 = CARTESIAN_POINT ( 'NONE',  ( 155.5066938333533528, 261.3015006940112244, -18.40036130547566273 ) ) ;
#31710 = ORIENTED_EDGE ( 'NONE', *, *, #80937, .T. ) ;
#31711 = CARTESIAN_POINT ( 'NONE',  ( 207.3988330342936877, 270.8564699888902396, -1.301389719878858875 ) ) ;
#31712 = CARTESIAN_POINT ( 'NONE',  ( 164.4575000359379828, 245.7982495824318505, -1.032884424947213997 ) ) ;
#31713 = CARTESIAN_POINT ( 'NONE',  ( 190.3440926964027540, 300.9613558596673784, 1.920019422129680464 ) ) ;
#31714 = LINE ( 'NONE', #2356, #52905 ) ;
#31715 = CARTESIAN_POINT ( 'NONE',  ( 79.49951204047911801, 46.37032438487753438, 12.70281872619212926 ) ) ;
#31717 = ADVANCED_FACE ( 'NONE', ( #60410 ), #45225, .T. ) ;
#31716 = DIRECTION ( 'NONE',  ( -0.8098206029991054100, 0.5866775868892259993, 0.000000000000000000 ) ) ;
#31718 = CARTESIAN_POINT ( 'NONE',  ( 49.89075441544353851, 199.6115022471902591, 10.00000000000009592 ) ) ;
#31719 = FACE_OUTER_BOUND ( 'NONE', #86164, .T. ) ;
#31720 = CARTESIAN_POINT ( 'NONE',  ( 122.7720312530212396, 247.8149278399160949, 9.188101187500093303 ) ) ;
#31721 = CARTESIAN_POINT ( 'NONE',  ( 70.80322137413750738, 60.50400129575321984, -14.70302039727341636 ) ) ;
#31722 = CARTESIAN_POINT ( 'NONE',  ( 33.58239374649102871, 42.49540643055189548, 3.479690158560446702E-15 ) ) ;
#31723 = VERTEX_POINT ( 'NONE', #22430 ) ;
#31725 = EDGE_LOOP ( 'NONE', ( #55884, #16132, #41195, #68854 ) ) ;
#31724 = DIRECTION ( 'NONE',  ( 0.2633726137851616911, 0.9634420117996742583, 0.04913609882121805494 ) ) ;
#31726 = VECTOR ( 'NONE', #74148, 1000.000000000000114 ) ;
#31727 = CARTESIAN_POINT ( 'NONE',  ( 203.6388180714938301, 276.2575050999084283, 13.35755797172022952 ) ) ;
#31728 = DIRECTION ( 'NONE',  ( -0.3473448497826262527, 0.9377374661009790779, 0.000000000000000000 ) ) ;
#31729 = CARTESIAN_POINT ( 'NONE',  ( 173.7521259494088781, 289.6425462570808236, -4.709990374833325610 ) ) ;
#31730 = CARTESIAN_POINT ( 'NONE',  ( 157.4656258344471098, 257.9085309395441641, 18.30485740784190796 ) ) ;
#31731 = CARTESIAN_POINT ( 'NONE',  ( 71.41016749218992743, 59.45273978182970609, 15.19346469599747174 ) ) ;
#31732 = CARTESIAN_POINT ( 'NONE',  ( -27.64350997085663764, 76.90478749174087625, 0.000000000000000000 ) ) ;
#31733 = CARTESIAN_POINT ( 'NONE',  ( 173.3670856503965183, 287.2530419906886436, -9.722124389285141888 ) ) ;
#31734 = EDGE_CURVE ( 'NONE', #2508, #96690, #25632, .T. ) ;
#31735 = VECTOR ( 'NONE', #84657, 1000.000000000000000 ) ;
#31736 = CARTESIAN_POINT ( 'NONE',  ( 26.07871176553302917, 38.55466486950701466, 7.012934429366973338E-14 ) ) ;
#31737 = CARTESIAN_POINT ( 'NONE',  ( 77.97212537282862854, 53.69847124008602890, -16.36973322202745607 ) ) ;
#31738 = ORIENTED_EDGE ( 'NONE', *, *, #100054, .F. ) ;
#31739 = CARTESIAN_POINT ( 'NONE',  ( 148.4083960970861256, 273.5961130204771052, -8.574185186226726429 ) ) ;
#31740 = DIRECTION ( 'NONE',  ( -0.8600446134263897147, -0.5102188382608503492, 0.000000000000000000 ) ) ;
#31741 = ORIENTED_EDGE ( 'NONE', *, *, #26473, .F. ) ;
#31742 = CARTESIAN_POINT ( 'NONE',  ( 188.3092780937153350, 266.3409406274001299, -11.83214085844302943 ) ) ;
#31743 = CARTESIAN_POINT ( 'NONE',  ( 160.2261283380418035, 278.9007923701936420, 10.53197256397347203 ) ) ;
#31744 = CARTESIAN_POINT ( 'NONE',  ( 192.1948126989040873, 297.7558147847510099, -10.38004547301857272 ) ) ;
#31745 = CARTESIAN_POINT ( 'NONE',  ( 149.4491471355718772, 271.7934793437897270, 11.43912701239353780 ) ) ;
#31746 = CARTESIAN_POINT ( 'NONE',  ( 204.6742660055938643, 272.9835131625996496, -9.777367022634962268 ) ) ;
#31748 = CARTESIAN_POINT ( 'NONE',  ( 154.9259971922039938, 277.6026755967128565, -8.943939257718048097 ) ) ;
#31747 = CARTESIAN_POINT ( 'NONE',  ( 164.4368094649636305, 283.5685030574936150, -6.732700809822128818 ) ) ;
#31749 = CARTESIAN_POINT ( 'NONE',  ( 200.8147387322574957, 282.8256649374973790, -18.02438097732020239 ) ) ;
#31750 = EDGE_LOOP ( 'NONE', ( #44607, #47418, #87963, #5914, #46934, #91670 ) ) ;
#31751 = CARTESIAN_POINT ( 'NONE',  ( 190.8683709797118411, 300.0532792356709706, -4.461919767133968762 ) ) ;
#31752 = CARTESIAN_POINT ( 'NONE',  ( 193.8848781386269309, 267.1185884883711879, -11.59377028749509364 ) ) ;
#31753 = EDGE_CURVE ( 'NONE', #28265, #86867, #40110, .T. ) ;
#31754 = CARTESIAN_POINT ( 'NONE',  ( 163.5128695541682191, 247.8493887573044105, -7.994499776565081817 ) ) ;
#31755 = DIRECTION ( 'NONE',  ( -0.5000000000000002220, 0.8660254037844385966, 0.000000000000000000 ) ) ;
#31756 = DIRECTION ( 'NONE',  ( -0.8660254037844387076, -0.4999999999999998890, -0.000000000000000000 ) ) ;
#31757 = EDGE_CURVE ( 'NONE', #37198, #21557, #38881, .T. ) ;
#31758 = CARTESIAN_POINT ( 'NONE',  ( 184.5615956163028955, 297.0763260467899158, -4.452223854632125999 ) ) ;
#31759 = CARTESIAN_POINT ( 'NONE',  ( 192.5254593562406171, 297.1831179748913314, 11.00703791256144015 ) ) ;
#31760 = DIRECTION ( 'NONE',  ( -0.3766285016932175433, 0.9263643838751153270, 0.000000000000000000 ) ) ;
#31761 = ADVANCED_FACE ( 'NONE', ( #47709 ), #48229, .T. ) ;
#31762 = CARTESIAN_POINT ( 'NONE',  ( 73.76584831522595209, 68.38082682530665579, 10.99424229391075514 ) ) ;
#31763 = CARTESIAN_POINT ( 'NONE',  ( 69.65059073173789272, 70.85594054465668989, -0.7120434053404213204 ) ) ;
#31764 = CARTESIAN_POINT ( 'NONE',  ( 0.4734401320438119676, 161.8923013555410080, 4.594050593750050204 ) ) ;
#31765 = CARTESIAN_POINT ( 'NONE',  ( 97.82019495012963262, 215.0327760586659451, 1.948934522072303157E-15 ) ) ;
#31766 = CARTESIAN_POINT ( 'NONE',  ( 37.35373998880870516, 180.8262482093457493, 3.021315404115420679E-15 ) ) ;
#31767 = CARTESIAN_POINT ( 'NONE',  ( 192.9633865298379476, 296.4246058602058156, -11.85717392250713864 ) ) ;
#31768 = DIRECTION ( 'NONE',  ( 0.000000000000000000, 0.000000000000000000, 1.000000000000000000 ) ) ;
#31769 = LINE ( 'NONE', #62673, #4310 ) ;
#31770 = ADVANCED_FACE ( 'NONE', ( #77650 ), #1651, .T. ) ;
#31771 = AXIS2_PLACEMENT_3D ( 'NONE', #39054, #17276, #24383 ) ;
#31772 = CARTESIAN_POINT ( 'NONE',  ( -22.42236680055709641, 157.8615022471902591, 0.000000000000000000 ) ) ;
#31773 = CARTESIAN_POINT ( 'NONE',  ( 163.1008115941903895, 248.1481028935802442, 11.25332017433677834 ) ) ;
#31774 = CARTESIAN_POINT ( 'NONE',  ( 163.3718935141138786, 265.0702796956427392, 17.82925771866536735 ) ) ;
#31775 = CARTESIAN_POINT ( 'NONE',  ( -19.65312891409030271, 93.06504152958497400, -10.00000000000000888 ) ) ;
#31776 = EDGE_CURVE ( 'NONE', #90496, #47930, #75161, .T. ) ;
#31777 = CARTESIAN_POINT ( 'NONE',  ( 177.8610022267205863, 290.0596117902207425, 9.769913558664320874 ) ) ;
#31778 = EDGE_CURVE ( 'NONE', #61485, #97002, #87311, .T. ) ;
#31779 = LINE ( 'NONE', #78415, #94502 ) ;
#31780 = CARTESIAN_POINT ( 'NONE',  ( 205.0423986797212592, 275.5031431113662279, -12.28496450925721462 ) ) ;
#31781 = CARTESIAN_POINT ( 'NONE',  ( 196.4351339088274813, 290.4113630087520050, 17.20526457544535504 ) ) ;
#31782 = AXIS2_PLACEMENT_3D ( 'NONE', #18060, #3375, #4345 ) ;
#31783 = PLANE ( 'NONE',  #2636 ) ;
#31784 = CARTESIAN_POINT ( 'NONE',  ( 72.87540168778714644, 56.79582781200069519, -15.95562737981789603 ) ) ;
#31785 = CARTESIAN_POINT ( 'NONE',  ( 40.49996498926459765, 188.0643266524160140, 9.188101187500095079 ) ) ;
#31786 = CARTESIAN_POINT ( 'NONE',  ( 77.73905735199544154, 209.5643266524159571, -9.188101187500093303 ) ) ;
#31787 = PLANE ( 'NONE',  #67679 ) ;
#31788 = CARTESIAN_POINT ( 'NONE',  ( 88.17148522932362198, 43.68169873549415883, 0.1729226289268753214 ) ) ;
#31789 = CARTESIAN_POINT ( 'NONE',  ( 84.86738834342773430, 49.16326195102271868, -12.63241503557467205 ) ) ;
#31790 = CARTESIAN_POINT ( 'NONE',  ( 147.7245617474428911, 256.0958772461660828, -9.188101187500095079 ) ) ;
#31792 = CARTESIAN_POINT ( 'NONE',  ( 68.97600843347925093, 70.62407868326711480, -3.116157198528183514 ) ) ;
#31791 = CARTESIAN_POINT ( 'NONE',  ( -19.65312891409034179, 93.06504152958504505, 0.000000000000000000 ) ) ;
#31793 = CARTESIAN_POINT ( 'NONE',  ( 196.6461856324828830, 268.7375099474577951, -10.58772324698134604 ) ) ;
#31794 = CARTESIAN_POINT ( 'NONE',  ( 34.04181514241641793, 20.44966523072496400, -2.296566073217252530E-15 ) ) ;
#31795 = DIRECTION ( 'NONE',  ( -0.8660254037844379305, -0.5000000000000014433, -0.000000000000000000 ) ) ;
#31796 = CARTESIAN_POINT ( 'NONE',  ( 83.56384804551235845, 46.97371956187362940, -11.44051147514629818 ) ) ;
#31797 = CARTESIAN_POINT ( 'NONE',  ( 15.62556418158687244, 11.94754757982088123, 5.678558825948272215 ) ) ;
#31798 = CARTESIAN_POINT ( 'NONE',  ( 68.48323730116675279, 210.3458772461660544, 9.188101187500095079 ) ) ;
#31799 = CARTESIAN_POINT ( 'NONE',  ( 173.1933364606677799, 257.0593323752887045, -13.27564283692902691 ) ) ;
#31800 = CARTESIAN_POINT ( 'NONE',  ( 203.1526193585190470, 278.7763369107815379, -16.67658907091021447 ) ) ;
#31801 = AXIS2_PLACEMENT_3D ( 'NONE', #77752, #93473, #62506 ) ;
#31802 = CARTESIAN_POINT ( 'NONE',  ( 159.2554912534056939, 254.8083930951974878, 16.49944922174842432 ) ) ;
#31803 = CARTESIAN_POINT ( 'NONE',  ( 69.43616476765555490, 62.98053158445969757, -13.63934076488703795 ) ) ;
#31804 = CARTESIAN_POINT ( 'NONE',  ( 153.2249512918476455, 276.7798453101777341, 7.180601189652168870 ) ) ;
#31805 = VECTOR ( 'NONE', #10763, 1000.000000000000000 ) ;
#31807 =( BOUNDED_CURVE ( )  B_SPLINE_CURVE ( 2, ( #9888, #40746, #2288, #78277, #25574, #39728, #54782, #29991, #91332 ),
 .UNSPECIFIED., .F., .T. ) 
 B_SPLINE_CURVE_WITH_KNOTS ( ( 3, 2, 2, 2, 3 ),
 ( 0.6814516129032257563, 0.6827956989247311315, 0.6854838709677418818, 0.6881720430107527431, 0.6895161290322581182 ),
 .UNSPECIFIED. ) 
 CURVE ( )  GEOMETRIC_REPRESENTATION_ITEM ( )  RATIONAL_B_SPLINE_CURVE ( ( 0.9330127018922194093, 0.9330127018922194093, 1.000000000000000000, 0.8660254037844387076, 1.000000000000000000, 0.8660254037844387076, 1.000000000000000000, 0.9330127018922194093, 0.9330127018922194093 ) ) 
 REPRESENTATION_ITEM ( '' )  );
#31806 = CARTESIAN_POINT ( 'NONE',  ( 105.8215617431884539, 245.2365022471903444, 2.944929066748280225E-16 ) ) ;
#31808 = CARTESIAN_POINT ( 'NONE',  ( 200.8551880497955437, 282.7556046643899776, 18.00894873733387058 ) ) ;
#31809 = CARTESIAN_POINT ( 'NONE',  ( 164.3524132573224392, 245.9802652221976587, -2.749586949851067441 ) ) ;
#31810 = ORIENTED_EDGE ( 'NONE', *, *, #65744, .F. ) ;
#31811 = CARTESIAN_POINT ( 'NONE',  ( 77.29015577573032658, 49.49666603636313766, 14.91995587329190798 ) ) ;
#31812 = CARTESIAN_POINT ( 'NONE',  ( 184.7850555545515192, 271.2875256772542230, 16.11813442280277542 ) ) ;
#31813 = VERTEX_POINT ( 'NONE', #72043 ) ;
#31814 = CARTESIAN_POINT ( 'NONE',  ( 159.3586121662929713, 254.6297824347537642, -15.50090345830412630 ) ) ;
#31815 = CARTESIAN_POINT ( 'NONE',  ( 190.1758200331204876, 279.2204749713225169, -17.78067544974210890 ) ) ;
#31816 = CARTESIAN_POINT ( 'NONE',  ( 68.58230928772361779, 68.76319458306602428, -6.210401753971947159 ) ) ;
#31817 = ORIENTED_EDGE ( 'NONE', *, *, #41427, .F. ) ;
#31818 = CARTESIAN_POINT ( 'NONE',  ( 173.2954469512942239, 251.6588534220469739, -0.1071739093455414404 ) ) ;
#31819 = ORIENTED_EDGE ( 'NONE', *, *, #59647, .F. ) ;
#31820 = DIRECTION ( 'NONE',  ( -0.4999999999999987788, 0.8660254037844392627, 0.000000000000000000 ) ) ;
#31821 = CARTESIAN_POINT ( 'NONE',  ( 147.6095889327917803, 274.9796876144846465, -8.460961150142429332 ) ) ;
#31822 = B_SPLINE_CURVE_WITH_KNOTS ( 'NONE', 3,
 ( #17610, #47994, #30812, #78937, #63708, #94644, #7495, #23192, #100226, #69799, #61691, #92644, #85039, #85562, #25723, #64717 ),
 .UNSPECIFIED., .F., .F.,
 ( 4, 2, 2, 2, 2, 2, 2, 4 ),
 ( 0.0005957069887743393069, 0.0008992575955524882789, 0.001202808202330637143, 0.001506358809108786223, 0.001809909415886935304, 0.002113460022665083950, 0.002417010629443233465, 0.003024111842999524253 ),
 .UNSPECIFIED. ) ;
#31823 = CARTESIAN_POINT ( 'NONE',  ( 206.7951683401124399, 270.7576251107032590, -5.378181275766958258 ) ) ;
#31824 = VERTEX_POINT ( 'NONE', #33534 ) ;
#31825 = ADVANCED_FACE ( 'NONE', ( #64433 ), #8236, .T. ) ;
#31826 = CARTESIAN_POINT ( 'NONE',  ( 32.96772289237024012, 21.96004757982091959, -5.678558825948275768 ) ) ;
#31827 = CARTESIAN_POINT ( 'NONE',  ( 21.99520779934447745, 195.0530062829863311, -4.648177544792955347E-16 ) ) ;
#31828 = CARTESIAN_POINT ( 'NONE',  ( 74.97941504220045772, 66.36908880787137832, -13.10375872137871767 ) ) ;
#31829 = EDGE_CURVE ( 'NONE', #58437, #27033, #18844, .T. ) ;
#31830 = EDGE_LOOP ( 'NONE', ( #9368, #49025, #53281, #62337 ) ) ;
#31831 = CARTESIAN_POINT ( 'NONE',  ( 23.46864935082052739, 158.3759306620404743, 30.52142883766500603 ) ) ;
#31832 = CARTESIAN_POINT ( 'NONE',  ( 159.8597520197352537, 253.7617827468940277, -16.74905990210778839 ) ) ;
#31833 = ORIENTED_EDGE ( 'NONE', *, *, #5156, .T. ) ;
#31834 = CARTESIAN_POINT ( 'NONE',  ( 174.5161929735236583, 286.6389660134419159, 11.76074990303198220 ) ) ;
#31836 = CARTESIAN_POINT ( 'NONE',  ( 68.03198790762533577, 66.08726303867234719, -10.49906168697004816 ) ) ;
#31835 = CARTESIAN_POINT ( 'NONE',  ( 68.00841086724713591, 65.44229140645596488, 10.41124389034581199 ) ) ;
#31837 = CARTESIAN_POINT ( 'NONE',  ( 208.3699316049496133, 269.7396870210121733, -1.898463622294385811 ) ) ;
#31838 = CARTESIAN_POINT ( 'NONE',  ( 154.9344967692067598, 262.2925750810547356, 17.30210568643136781 ) ) ;
#31839 = CARTESIAN_POINT ( 'NONE',  ( 32.56963740530460427, 41.73705186507756082, -3.090169943749475845 ) ) ;
#31840 = CARTESIAN_POINT ( 'NONE',  ( 204.6475128369918082, 276.1871054541632020, -13.72068618491070779 ) ) ;
#31842 = ADVANCED_FACE ( 'NONE', ( #41614 ), #19361, .F. ) ;
#31841 = CARTESIAN_POINT ( 'NONE',  ( 208.0730008398676318, 270.2539861924646516, -3.911917750280078376 ) ) ;
#31843 = CARTESIAN_POINT ( 'NONE',  ( 206.5911069559201110, 270.4023401184283557, 3.160577138512981055 ) ) ;
#31844 = CARTESIAN_POINT ( 'NONE',  ( 195.6460486738788518, 290.5633724012552079, -16.40341345355467695 ) ) ;
#31845 = CARTESIAN_POINT ( 'NONE',  ( 90.02596631606967037, 210.5327760586659451, 1.948934522072303157E-15 ) ) ;
#31846 = EDGE_LOOP ( 'NONE', ( #10549, #40939, #60000, #23418 ) ) ;
#31847 = CARTESIAN_POINT ( 'NONE',  ( 150.6487462746963502, 269.7157126861102370, 15.18501655901553704 ) ) ;
#31848 = CARTESIAN_POINT ( 'NONE',  ( 195.2347945672775325, 277.4660317214627980, -17.03751719888963123 ) ) ;
#31849 = CARTESIAN_POINT ( 'NONE',  ( -77.74869931532474254, 54.01501336371526918, 10.00000000000000000 ) ) ;
#31850 = AXIS2_PLACEMENT_3D ( 'NONE', #73795, #18606, #27704 ) ;
#31851 = VERTEX_POINT ( 'NONE', #49723 ) ;
#31852 = CARTESIAN_POINT ( 'NONE',  ( 196.1005589118404373, 290.9908639024753825, -16.71343850857806501 ) ) ;
#31853 = AXIS2_PLACEMENT_3D ( 'NONE', #98901, #79118, #2594 ) ;
#31854 = VERTEX_POINT ( 'NONE', #50710 ) ;
#31855 = CARTESIAN_POINT ( 'NONE',  ( 80.16587651742513287, 44.65728575280898127, -11.72747585068735887 ) ) ;
#31856 = DIRECTION ( 'NONE',  ( -0.4999999999999987788, 0.8660254037844392627, 0.000000000000000000 ) ) ;
#31857 = EDGE_CURVE ( 'NONE', #30831, #93932, #95203, .T. ) ;
#31859 = B_SPLINE_SURFACE_WITH_KNOTS ( 'NONE', 3, 1, ( 
 ( #74922, #28801 ),
 ( #61182, #74432 ),
 ( #59682, #90654 ),
 ( #53090, #21212 ),
 ( #91137, #44984 ),
 ( #77490, #85109 ),
 ( #14679, #22272 ),
 ( #8084, #99294 ),
 ( #14185, #23758 ),
 ( #76009, #68861 ),
 ( #84614, #61759 ),
 ( #91710, #92708 ),
 ( #54145, #38457 ),
 ( #45560, #29386 ),
 ( #23258, #69863 ),
 ( #60253, #29875 ),
 ( #100290, #53656 ),
 ( #93202, #46051 ),
 ( #53176, #99786 ),
 ( #38958, #60747 ),
 ( #15659, #22779 ),
 ( #85627, #52663 ),
 ( #91211, #30376 ),
 ( #46555, #15153 ),
 ( #84130, #61259 ),
 ( #76489, #6587 ),
 ( #76966, #68370 ),
 ( #92229, #7068 ),
 ( #21773, #37952 ),
 ( #83617, #7567 ),
 ( #69371, #475 ) ),
 .UNSPECIFIED., .F., .F., .F.,
 ( 4, 3, 3, 3, 3, 3, 3, 3, 3, 3, 4 ),
 ( 2, 2 ),
 ( 0.000000000000000000, 0.1122669598086762505, 0.2243161639709597699, 0.3396355846219117347, 0.4553962076585177376, 0.5677860799922461732, 0.6749047109689493285, 0.7773884377078335017, 0.8775581155834230040, 0.9782364162377888972, 1.000000000000000000 ),
 ( 0.000000000000000000, 1.000000000000000000 ),
 .UNSPECIFIED. ) ;
#31858 = DIRECTION ( 'NONE',  ( -0.000000000000000000, 0.000000000000000000, -1.000000000000000000 ) ) ;
#31860 = CARTESIAN_POINT ( 'NONE',  ( -22.42236680055709641, 157.8615022471902591, 0.000000000000000000 ) ) ;
#31861 = CARTESIAN_POINT ( 'NONE',  ( 84.55469670542369443, 47.34764971695675229, -11.32901942273590379 ) ) ;
#31862 = CARTESIAN_POINT ( 'NONE',  ( 157.4883523481626639, 280.5151220735496622, 7.290131461700886106 ) ) ;
#31863 = EDGE_CURVE ( 'NONE', #33601, #3825, #95881, .T. ) ;
#31864 = CARTESIAN_POINT ( 'NONE',  ( 89.24104401994878799, 213.1423013555409796, -4.594050593750043987 ) ) ;
#31865 = VERTEX_POINT ( 'NONE', #49239 ) ;
#31866 = VECTOR ( 'NONE', #30395, 1000.000000000000000 ) ;
#31867 = ORIENTED_EDGE ( 'NONE', *, *, #30294, .T. ) ;
#31868 = CARTESIAN_POINT ( 'NONE',  ( 163.4178923001155681, 247.5989030008181260, -10.38047187240561442 ) ) ;
#31869 = VERTEX_POINT ( 'NONE', #66911 ) ;
#31870 = LINE ( 'NONE', #26169, #75860 ) ;
#31871 = CARTESIAN_POINT ( 'NONE',  ( 184.0702669486040008, 275.1941235734948918, 16.36998289429038067 ) ) ;
#31872 = CARTESIAN_POINT ( 'NONE',  ( -30.81750703737776220, 93.28907056446753643, 44.17799681287748115 ) ) ;
#31873 = CARTESIAN_POINT ( 'NONE',  ( 206.1823507212516802, 271.5286882572439140, -8.119960357998227352 ) ) ;
#31874 = CARTESIAN_POINT ( 'NONE',  ( 87.64772643527687990, 44.68358544867225390, 5.012156274856216953 ) ) ;
#31875 = ORIENTED_EDGE ( 'NONE', *, *, #46857, .F. ) ;
#31876 = AXIS2_PLACEMENT_3D ( 'NONE', #57140, #88121, #61123 ) ;
#31877 = CARTESIAN_POINT ( 'NONE',  ( 189.2891873318943396, 295.0123130764713437, 11.41301585810447783 ) ) ;
#31878 = CARTESIAN_POINT ( 'NONE',  ( 185.8275728834229596, 259.3864893694817511, 5.920843924932031932 ) ) ;
#31879 = PLANE ( 'NONE',  #70705 ) ;
#31880 = CARTESIAN_POINT ( 'NONE',  ( 71.88281838930642209, 59.56282477439597045, -15.74156321294393024 ) ) ;
#31881 = CARTESIAN_POINT ( 'NONE',  ( 111.3525576494051563, 223.5494855054051584, -2.679491924311248496 ) ) ;
#31882 = DIRECTION ( 'NONE',  ( 0.4999999999999998890, -0.8660254037844385966, 0.000000000000000000 ) ) ;
#31883 = ORIENTED_EDGE ( 'NONE', *, *, #19228, .F. ) ;
#31884 = CARTESIAN_POINT ( 'NONE',  ( 188.2145160130152419, 294.1882611685968527, -12.46123440450256936 ) ) ;
#31885 = ADVANCED_FACE ( 'NONE', ( #97841 ), #11741, .T. ) ;
#31886 = CARTESIAN_POINT ( 'NONE',  ( 200.1782072557437857, 283.9281697954355650, 18.05177561285849208 ) ) ;
#31887 = CARTESIAN_POINT ( 'NONE',  ( 82.08475017950465258, 40.77228884684495824, 1.269038889852737384 ) ) ;
#31888 = CARTESIAN_POINT ( 'NONE',  ( 187.7420758953736595, 266.0326380175162058, -11.83518821542502586 ) ) ;
#31889 = CARTESIAN_POINT ( 'NONE',  ( 83.75118553669710764, 52.20252726632157447, 14.66647926495056886 ) ) ;
#31890 = CARTESIAN_POINT ( 'NONE',  ( 153.2338012341922990, 270.4421391452444254, 13.91873268832451416 ) ) ;
#31891 = B_SPLINE_CURVE_WITH_KNOTS ( 'NONE', 3,
 ( #97076, #12445, #81379, #26139, #3838, #19057, #49931, #72767, #64643, #11946 ),
 .UNSPECIFIED., .F., .F.,
 ( 4, 2, 2, 2, 4 ),
 ( 0.000000000000000000, 0.2500000000000000000, 0.5000000000000000000, 0.7500000000000000000, 1.000000000000000000 ),
 .UNSPECIFIED. ) ;
#31892 = EDGE_LOOP ( 'NONE', ( #98515, #96360, #86637, #58760 ) ) ;
#31893 = CARTESIAN_POINT ( 'NONE',  ( 170.5373622343556690, 269.7751423367952270, 17.81562764448176850 ) ) ;
#31894 = EDGE_CURVE ( 'NONE', #19653, #62639, #36260, .T. ) ;
#31895 = CARTESIAN_POINT ( 'NONE',  ( -16.58100052909938071, 102.4826666393443304, 44.59494843596851155 ) ) ;
#31896 = EDGE_CURVE ( 'NONE', #30740, #63497, #70158, .T. ) ;
#31897 = CARTESIAN_POINT ( 'NONE',  ( 207.5686001603237116, 271.1276337968068333, 7.659944433763431704 ) ) ;
#31899 = CARTESIAN_POINT ( 'NONE',  ( -23.29562891409031522, 78.77562236714182120, 59.97499999999998721 ) ) ;
#31898 = CARTESIAN_POINT ( 'NONE',  ( 194.4459411895494725, 293.8567458645873103, 14.31012567920753042 ) ) ;
#31900 = CARTESIAN_POINT ( 'NONE',  ( 199.1671527971112141, 281.9112550430394322, -16.60146190726549165 ) ) ;
#31901 = CARTESIAN_POINT ( 'NONE',  ( 26.41003172443570790, 38.18080186712595037, 3.090169943749475401 ) ) ;
#31902 = CARTESIAN_POINT ( 'NONE',  ( 165.1772004350705458, 286.3187765620995151, -3.363692932437915228 ) ) ;
#31903 = DIRECTION ( 'NONE',  ( 1.000000000000000000, 0.000000000000000000, 0.000000000000000000 ) ) ;
#31904 = CARTESIAN_POINT ( 'NONE',  ( 188.2316138847417051, 260.8329576480458059, 3.008261098653536525 ) ) ;
#31905 = DIRECTION ( 'NONE',  ( -0.000000000000000000, -0.000000000000000000, 1.000000000000000000 ) ) ;
#31906 = CARTESIAN_POINT ( 'NONE',  ( -7.294332625736644538, 178.8464784336661637, 1.353441290958777327E-15 ) ) ;
#31907 = DIRECTION ( 'NONE',  ( 0.06958655048003267729, -0.1205274409548735270, -0.9902680687415703620 ) ) ;
#31908 = ORIENTED_EDGE ( 'NONE', *, *, #92720, .T. ) ;
#31909 = CARTESIAN_POINT ( 'NONE',  ( 160.1902186677070574, 253.5786389215288068, -14.79079237559988691 ) ) ;
#31910 = CARTESIAN_POINT ( 'NONE',  ( 26.23682664367882111, 38.08080186712594184, -3.090169943749475845 ) ) ;
#31911 = CARTESIAN_POINT ( 'NONE',  ( 208.3135187673106543, 269.8373969220020285, 2.829653198597726682 ) ) ;
#31912 = CARTESIAN_POINT ( 'NONE',  ( 176.5752601597114335, 288.5842064133888130, 11.38490813771325350 ) ) ;
#31913 = CARTESIAN_POINT ( 'NONE',  ( 16.25090658753528317, 186.3149278399161233, 9.188101187500093303 ) ) ;
#31914 = VECTOR ( 'NONE', #57587, 1000.000000000000000 ) ;
#31915 = CARTESIAN_POINT ( 'NONE',  ( 64.10800479423804177, 214.4865022471902876, -10.00000000000009592 ) ) ;
#31916 = CARTESIAN_POINT ( 'NONE',  ( 28.13532114344886992, 38.01751292744058475, 6.180339887498949913 ) ) ;
#31917 = CARTESIAN_POINT ( 'NONE',  ( 85.18851589652911116, 42.50252688496647835, -1.291714491316064306 ) ) ;
#31918 = CARTESIAN_POINT ( 'NONE',  ( 191.1192699377806719, 299.6187094927299199, -9.526914969203620132 ) ) ;
#31919 = AXIS2_PLACEMENT_3D ( 'NONE', #64761, #3473, #32843 ) ;
#31920 = CARTESIAN_POINT ( 'NONE',  ( 81.50416045441870949, 56.04869296950724333, 16.05856639404321129 ) ) ;
#31921 = CARTESIAN_POINT ( 'NONE',  ( 186.8377166567931909, 295.8024518766285382, -7.974395351236546858 ) ) ;
#31922 = CARTESIAN_POINT ( 'NONE',  ( 190.5217488035042379, 261.8431898049273059, -0.7587358768599492542 ) ) ;
#31923 = VECTOR ( 'NONE', #44722, 1000.000000000000000 ) ;
#31924 = CARTESIAN_POINT ( 'NONE',  ( 68.58246938045769525, 203.7365022471902023, 10.00000000000009592 ) ) ;
#31925 = CARTESIAN_POINT ( 'NONE',  ( 68.42498683509937507, 66.83623499972065929, -9.111695128013669986 ) ) ;
#31926 = CARTESIAN_POINT ( 'NONE',  ( -46.35039662390601478, 28.35603213498495023, 10.00000000000000000 ) ) ;
#31927 = CARTESIAN_POINT ( 'NONE',  ( 40.66251830035667325, 182.0327760586659451, 1.948934522072303157E-15 ) ) ;
#31928 = CARTESIAN_POINT ( 'NONE',  ( 71.39067424117821759, 70.28756797341888785, -7.485097133833798821 ) ) ;
#31929 = ADVANCED_FACE ( 'NONE', ( #66421 ), #77132, .F. ) ;
#31930 = CARTESIAN_POINT ( 'NONE',  ( 34.97213163436671124, 51.32435524152969464, -10.00000000000000000 ) ) ;
#31931 = CARTESIAN_POINT ( 'NONE',  ( 77.46075950540223687, 49.77948894799936852, -14.98483444581543722 ) ) ;
#31932 = CARTESIAN_POINT ( 'NONE',  ( 173.6088960567799120, 251.7861549345625178, -6.312679096147793878 ) ) ;
#31933 = PLANE ( 'NONE',  #51530 ) ;
#31934 = CARTESIAN_POINT ( 'NONE',  ( -5.122212653107841795, 179.3967562850347406, 2.649461200531984646E-14 ) ) ;
#31935 = CARTESIAN_POINT ( 'NONE',  ( 162.9249713293285424, 280.6004508475537023, -9.976534934921010844 ) ) ;
#31936 = CARTESIAN_POINT ( 'NONE',  ( 205.6544395269333165, 269.2573939850345255, -1.340776332317544339 ) ) ;
#31937 = CARTESIAN_POINT ( 'NONE',  ( 18.21401815691482895, 25.91421378149918198, 9.188101187500008038 ) ) ;
#31938 = CARTESIAN_POINT ( 'NONE',  ( 162.9796882977680639, 248.3578945969637743, 9.683801903336119565 ) ) ;
#31939 = CARTESIAN_POINT ( 'NONE',  ( 108.6902708896766114, 226.8927522451418213, 10.00000000000009948 ) ) ;
#31940 = CARTESIAN_POINT ( 'NONE',  ( 188.5189969585072731, 269.7688609434800924, -14.07648933449623208 ) ) ;
#31941 = EDGE_LOOP ( 'NONE', ( #41941, #32863, #97688, #49840 ) ) ;
#31942 = AXIS2_PLACEMENT_3D ( 'NONE', #83230, #57527, #88503 ) ;
#31943 = CARTESIAN_POINT ( 'NONE',  ( 35.31250668086031652, 42.16126292948898424, -6.180339887498951690 ) ) ;
#31944 = CARTESIAN_POINT ( 'NONE',  ( 10.26703877906431472, 17.87878583063839599, -9.188101187500006262 ) ) ;
#31945 = CARTESIAN_POINT ( 'NONE',  ( 75.25614561676577807, 53.63511853603917956, -16.53665762988984511 ) ) ;
#31946 = CARTESIAN_POINT ( 'NONE',  ( 161.5029716424245407, 251.3413373469583973, -13.00020995489466458 ) ) ;
#31947 = CARTESIAN_POINT ( 'NONE',  ( 71.91251904240313308, 72.63095699448832931, -0.6620033135626105514 ) ) ;
#31948 = CARTESIAN_POINT ( 'NONE',  ( 36.20694410119924811, 43.83705186507757645, 3.090169943749475401 ) ) ;
#31949 = ORIENTED_EDGE ( 'NONE', *, *, #83937, .F. ) ;
#31950 = DIRECTION ( 'NONE',  ( -0.6355427771210634402, 0.000000000000000000, 0.7720656568254065100 ) ) ;
#31951 = CARTESIAN_POINT ( 'NONE',  ( 72.52074056358647169, 71.25752213848458894, -6.049989122658143259 ) ) ;
#31952 = CARTESIAN_POINT ( 'NONE',  ( 191.2645787786270262, 299.3670271975948367, 7.309947121636420242 ) ) ;
#31953 = CARTESIAN_POINT ( 'NONE',  ( 180.9038145878475916, 257.6994971499530607, -7.472903516740896812 ) ) ;
#31954 = ORIENTED_EDGE ( 'NONE', *, *, #21506, .T. ) ;
#31955 = AXIS2_PLACEMENT_3D ( 'NONE', #89418, #33160, #72698 ) ;
#31957 = CARTESIAN_POINT ( 'NONE',  ( 86.45348570349138129, 43.24264366923927838, -1.738868482183878239 ) ) ;
#31956 = CARTESIAN_POINT ( 'NONE',  ( 79.14312167556931854, 57.64441083166269664, 0.000000000000000000 ) ) ;
#31958 = VERTEX_POINT ( 'NONE', #98335 ) ;
#31959 = CARTESIAN_POINT ( 'NONE',  ( 65.86357856937301847, 68.93032387894690771, -2.527662978207743549 ) ) ;
#31960 = CARTESIAN_POINT ( 'NONE',  ( 71.76465953926796715, 72.09915442159702081, -3.621776363507912766 ) ) ;
#31961 = CARTESIAN_POINT ( 'NONE',  ( 79.93705350559073963, 58.08899977657839031, 16.26815128937695576 ) ) ;
#31962 = CARTESIAN_POINT ( 'NONE',  ( 76.92045831404706746, 63.69682018499118925, 15.34400990693822564 ) ) ;
#31963 = CARTESIAN_POINT ( 'NONE',  ( 147.8465295590381743, 274.5692944114487091, 9.322947948439978205 ) ) ;
#31964 = EDGE_CURVE ( 'NONE', #26501, #934, #75040, .T. ) ;
#31965 = CARTESIAN_POINT ( 'NONE',  ( 149.1004267900891307, 272.3974806997987343, -12.86882154300063341 ) ) ;
#31966 = CARTESIAN_POINT ( 'NONE',  ( 83.50336539627915045, 219.0177522451418497, -10.00000000000009592 ) ) ;
#31967 = ORIENTED_EDGE ( 'NONE', *, *, #63685, .F. ) ;
#31968 = DIRECTION ( 'NONE',  ( -0.000000000000000000, -0.000000000000000000, -1.000000000000000000 ) ) ;
#31969 = CARTESIAN_POINT ( 'NONE',  ( -44.30466402961319972, 27.54938068083718861, 10.00000000000000000 ) ) ;
#31970 = ORIENTED_EDGE ( 'NONE', *, *, #52881, .F. ) ;
#31971 = CARTESIAN_POINT ( 'NONE',  ( 24.92213970864663963, 37.49540643055189548, 3.479690158560446702E-15 ) ) ;
#31972 = FACE_OUTER_BOUND ( 'NONE', #61989, .T. ) ;
#31973 = CARTESIAN_POINT ( 'NONE',  ( 78.28749215422203633, 47.38001368514189693, -14.28996306490787482 ) ) ;
#31974 = CARTESIAN_POINT ( 'NONE',  ( 54.68078388046973970, 208.5024278399160949, -9.188101187500093303 ) ) ;
#31975 = ORIENTED_EDGE ( 'NONE', *, *, #37993, .F. ) ;
#31976 = ADVANCED_FACE ( 'NONE', ( #67411 ), #13719, .T. ) ;
#31977 = CARTESIAN_POINT ( 'NONE',  ( 74.40608543823466903, 68.34271654374390437, 11.85151599582642312 ) ) ;
#31978 = CARTESIAN_POINT ( 'NONE',  ( 190.8094645593471341, 300.1553081486349015, 8.399847186519689757 ) ) ;
#31979 = DIRECTION ( 'NONE',  ( -0.5951734788405994570, 0.8035972437015812542, 0.000000000000000000 ) ) ;
#31980 = CARTESIAN_POINT ( 'NONE',  ( 172.8855825645377990, 271.3786399235225417, 16.45412496818341097 ) ) ;
#31981 = EDGE_CURVE ( 'NONE', #35343, #69104, #7105, .T. ) ;
#31982 = ORIENTED_EDGE ( 'NONE', *, *, #99902, .T. ) ;
#31983 = DIRECTION ( 'NONE',  ( 4.546899780356473057E-16, -0.000000000000000000, -1.000000000000000000 ) ) ;
#31984 = DIRECTION ( 'NONE',  ( -0.9879014915521923124, 0.1550826972584426755, 0.000000000000000000 ) ) ;
#31985 = CARTESIAN_POINT ( 'NONE',  ( 165.6039301651514961, 278.9421411211367285, 14.15335429374977139 ) ) ;
#31986 = ORIENTED_EDGE ( 'NONE', *, *, #73526, .T. ) ;
#31987 = CARTESIAN_POINT ( 'NONE',  ( 175.3038007714868058, 260.9809825493145468, -14.68767903443118605 ) ) ;
#31988 = CARTESIAN_POINT ( 'NONE',  ( 171.4076116757450450, 275.9429945178056869, -16.88996634460038848 ) ) ;
#31989 = FACE_OUTER_BOUND ( 'NONE', #86228, .T. ) ;
#31990 = CARTESIAN_POINT ( 'NONE',  ( 192.4212750754384160, 297.3635704425909125, -12.73704185013552248 ) ) ;
#31991 = CARTESIAN_POINT ( 'NONE',  ( 160.1876870865671947, 255.7147813180542073, 16.12179979881591407 ) ) ;
#31992 = DIRECTION ( 'NONE',  ( -0.4999999999999987788, 0.8660254037844392627, 0.000000000000000000 ) ) ;
#31993 = CARTESIAN_POINT ( 'NONE',  ( 76.18925827497564285, 65.27842891210502785, 14.09988157931024766 ) ) ;
#31994 = CARTESIAN_POINT ( 'NONE',  ( 76.32413911534708006, 63.96060367144042402, -14.71169841249486332 ) ) ;
#31995 = CARTESIAN_POINT ( 'NONE',  ( 207.7655736232174206, 270.7864657513322300, 3.530742899761726949 ) ) ;
#31996 = VECTOR ( 'NONE', #42297, 1000.000000000000000 ) ;
#31997 = CARTESIAN_POINT ( 'NONE',  ( 111.5140480995885497, 229.0643266524159856, -9.188101187500093303 ) ) ;
#31998 = ORIENTED_EDGE ( 'NONE', *, *, #73932, .F. ) ;
#31999 = CARTESIAN_POINT ( 'NONE',  ( 84.55537670905214043, 50.62155581810768012, -14.09136642048690291 ) ) ;
#32000 = CARTESIAN_POINT ( 'NONE',  ( 70.61866190243357266, 66.21379322135312862, 11.18361157626617874 ) ) ;
#32001 = CARTESIAN_POINT ( 'NONE',  ( 203.4696564630250464, 278.2272125378923988, -16.38980782817167636 ) ) ;
#32002 = CARTESIAN_POINT ( 'NONE',  ( 182.8969736784899567, 285.4463084877070287, -15.16533932269233986 ) ) ;
#32003 = CARTESIAN_POINT ( 'NONE',  ( 83.83319469606612984, 52.06770183867002544, -14.58843048856406099 ) ) ;
#32004 = CARTESIAN_POINT ( 'NONE',  ( 178.0214568497756886, 255.3923698286970705, 4.825899244335746019 ) ) ;
#32005 = ORIENTED_EDGE ( 'NONE', *, *, #98306, .F. ) ;
#32006 = CARTESIAN_POINT ( 'NONE',  ( 80.15404930735283529, 58.24487849859603017, -16.60713908503102232 ) ) ;
#32007 = ADVANCED_FACE ( 'NONE', ( #75528, #6622 ), #68898, .F. ) ;
#32008 = CARTESIAN_POINT ( 'NONE',  ( 85.83574890286925552, 44.62951015086210305, -6.991694815152513343 ) ) ;
#32009 = CARTESIAN_POINT ( 'NONE',  ( 182.1624531057215393, 260.1812964409709252, 10.65669563999669833 ) ) ;
#32010 = CARTESIAN_POINT ( 'NONE',  ( 205.9474858145129019, 272.6472302773099159, 9.310014741362042656 ) ) ;
#32011 = CARTESIAN_POINT ( 'NONE',  ( 128.9971094863694532, 233.0327760586659451, 1.948934522072302763E-15 ) ) ;
#32012 = CARTESIAN_POINT ( 'NONE',  ( 189.7310370775148840, 294.7812428202356614, -12.66668878006862364 ) ) ;
#32013 = VECTOR ( 'NONE', #69348, 1000.000000000000000 ) ;
#32014 = CARTESIAN_POINT ( 'NONE',  ( 189.1692022066353331, 299.6200726245371015, 4.912915616140450581 ) ) ;
#32015 = CARTESIAN_POINT ( 'NONE',  ( 195.9920715006079490, 291.1787696107118677, 15.99608784761372071 ) ) ;
#32016 = CARTESIAN_POINT ( 'NONE',  ( 47.32807415326523426, 108.5480133836684900, -10.00000000000000000 ) ) ;
#32017 = CARTESIAN_POINT ( 'NONE',  ( 53.16558651961199899, 195.3768266524160140, 9.188101187500098632 ) ) ;
#32018 = CARTESIAN_POINT ( 'NONE',  ( 85.55975315002648074, 48.35019831671618817, -12.20940535940758842 ) ) ;
#32019 = ORIENTED_EDGE ( 'NONE', *, *, #69849, .T. ) ;
#32020 = DIRECTION ( 'NONE',  ( 0.9186857246103528052, -0.3949892902309516951, 0.000000000000000000 ) ) ;
#32021 = DIRECTION ( 'NONE',  ( 0.000000000000000000, 0.000000000000000000, 1.000000000000000000 ) ) ;
#32022 = EDGE_CURVE ( 'NONE', #87147, #91470, #57970, .T. ) ;
#32023 = CARTESIAN_POINT ( 'NONE',  ( 175.0915097197001558, 261.2351211855327051, 15.18232397002616629 ) ) ;
#32024 = LINE ( 'NONE', #93885, #61175 ) ;
#32025 = CARTESIAN_POINT ( 'NONE',  ( 67.79725476218452229, 65.71048819351143777, 10.00598338191753101 ) ) ;
#32026 = CARTESIAN_POINT ( 'NONE',  ( 178.3743760340321387, 261.1640921747737139, 13.34356303130173949 ) ) ;
#32027 = AXIS2_PLACEMENT_3D ( 'NONE', #39417, #16636, #8545 ) ;
#32028 = CARTESIAN_POINT ( 'NONE',  ( 124.2787281577965075, 235.8927522451418213, 10.00000000000009592 ) ) ;
#32029 = CARTESIAN_POINT ( 'NONE',  ( 194.5514039441539751, 292.7602831052016086, -15.13274470691405149 ) ) ;
#32030 = ORIENTED_EDGE ( 'NONE', *, *, #16354, .F. ) ;
#32031 = CARTESIAN_POINT ( 'NONE',  ( 189.9462859318020946, 301.6503773875500087, -1.164147598593831656 ) ) ;
#32032 = CARTESIAN_POINT ( 'NONE',  ( 88.05223289789027774, 44.73115413622458902, 4.436861541472143067 ) ) ;
#32033 = CARTESIAN_POINT ( 'NONE',  ( 34.68144358152915174, 181.6423013555409796, -4.594050593750043987 ) ) ;
#32034 = CARTESIAN_POINT ( 'NONE',  ( 8.320926099340340443, 27.73705186507752174, -3.090169943749475845 ) ) ;
#32035 = DIRECTION ( 'NONE',  ( 0.000000000000000000, 0.000000000000000000, 1.000000000000000000 ) ) ;
#32036 = CARTESIAN_POINT ( 'NONE',  ( 71.87556436007473337, 59.56477266904413881, -15.73977692506605486 ) ) ;
#32037 = CARTESIAN_POINT ( 'NONE',  ( 66.76060919205468736, 68.13847131232218146, -6.506754398145753626 ) ) ;
#32039 = CARTESIAN_POINT ( 'NONE',  ( 62.79092448910136426, 200.3927522451417929, -10.00000000000009059 ) ) ;
#32038 = CARTESIAN_POINT ( 'NONE',  ( 168.9285091408607684, 266.8905904589466900, 17.77692745299157195 ) ) ;
#32040 = CARTESIAN_POINT ( 'NONE',  ( 12.53791098520745173, 8.208019796199266693, -3.090169943749474069 ) ) ;
#32041 = CARTESIAN_POINT ( 'NONE',  ( 184.7966971888043020, 257.5870176390811821, 1.382809315717336229 ) ) ;
#32042 = CARTESIAN_POINT ( 'NONE',  ( 204.7519188734507622, 276.0062688943993408, -12.76027478560537531 ) ) ;
#32043 = CARTESIAN_POINT ( 'NONE',  ( 16.70795526530605457, 14.81029122506293483, 8.090169943749479842 ) ) ;
#32044 = ORIENTED_EDGE ( 'NONE', *, *, #86860, .T. ) ;
#32045 = EDGE_CURVE ( 'NONE', #87128, #91430, #4463, .T. ) ;
#32046 = CARTESIAN_POINT ( 'NONE',  ( 27.73493783529162116, 193.4865022471903444, -10.00000000000009415 ) ) ;
#32047 = CARTESIAN_POINT ( 'NONE',  ( 32.84087927488944558, 199.7677522451419350, -5.000000000000047962 ) ) ;
#32048 = CARTESIAN_POINT ( 'NONE',  ( 162.6264071486809542, 248.9697954965390920, 10.36322805486644683 ) ) ;
#32049 = AXIS2_PLACEMENT_3D ( 'NONE', #10653, #42520, #34926 ) ;
#32050 = CARTESIAN_POINT ( 'NONE',  ( -3.504777292649704279, 156.5327760586659451, 1.948934522072303157E-15 ) ) ;
#32051 = CARTESIAN_POINT ( 'NONE',  ( 27.52682148520507965, 37.93396525600392266, 2.839279412974139660 ) ) ;
#32054 = EDGE_CURVE ( 'NONE', #54506, #4704, #44668, .T. ) ;
#32053 = CARTESIAN_POINT ( 'NONE',  ( 170.9051221141708083, 262.8660520292235674, 16.32175538396744230 ) ) ;
#32052 = CARTESIAN_POINT ( 'NONE',  ( 164.1204250983133477, 260.5664103406105028, -16.15875528054763421 ) ) ;
#32055 = CARTESIAN_POINT ( 'NONE',  ( 185.8626946602280441, 259.3471889805154547, 7.308832903665572367 ) ) ;
#32056 = DIRECTION ( 'NONE',  ( 0.5000000000000048850, -0.8660254037844358210, 0.000000000000000000 ) ) ;
#32058 = AXIS2_PLACEMENT_3D ( 'NONE', #49269, #18373, #88323 ) ;
#32057 = CYLINDRICAL_SURFACE ( 'NONE', #56512, 9.212605237762131694 ) ;
#32059 = CARTESIAN_POINT ( 'NONE',  ( 66.03987969823486992, 68.56027586650085937, 2.028142095923215482 ) ) ;
#32060 = EDGE_LOOP ( 'NONE', ( #42901, #59728, #45060, #48022 ) ) ;
#32061 = CARTESIAN_POINT ( 'NONE',  ( 82.87596643829704135, 41.15858874971023340, 0.1873015203630768732 ) ) ;
#32062 = VECTOR ( 'NONE', #77652, 1000.000000000000000 ) ;
#32063 = CARTESIAN_POINT ( 'NONE',  ( 181.8249261631527531, 287.9314247020339508, 13.64167460269014320 ) ) ;
#32064 = CARTESIAN_POINT ( 'NONE',  ( 154.0709734344990522, 278.1335148570522620, -5.205178880588171353 ) ) ;
#32065 = CARTESIAN_POINT ( 'NONE',  ( 14.44138481658839090, 10.19860640527290663, 2.839279412974134775 ) ) ;
#32066 = CARTESIAN_POINT ( 'NONE',  ( 159.0552039522962957, 259.4077134839495216, 16.69544169553007151 ) ) ;
#32067 = VECTOR ( 'NONE', #57777, 1000.000000000000000 ) ;
#32068 = CARTESIAN_POINT ( 'NONE',  ( 206.8851632406098702, 272.3113812655195716, -9.957011741946159233 ) ) ;
#32069 = CARTESIAN_POINT ( 'NONE',  ( 56.31377616017810084, 209.9865022471902876, -10.00000000000009592 ) ) ;
#32070 = CARTESIAN_POINT ( 'NONE',  ( 152.6757560589063303, 266.2048287524194166, 16.73757896668104195 ) ) ;
#32071 = CARTESIAN_POINT ( 'NONE',  ( 188.5410240070633563, 293.7196559869043426, 13.01390607220156248 ) ) ;
#32072 = CARTESIAN_POINT ( 'NONE',  ( 191.5235241413101903, 298.4719041358723075, 8.455706032256406601 ) ) ;
#32073 = CARTESIAN_POINT ( 'NONE',  ( 208.3699316049496133, 269.7396870210121733, -1.898463622294385811 ) ) ;
#32074 = CARTESIAN_POINT ( 'NONE',  ( 154.8679462054080318, 262.4078440388265676, 17.98338675682672871 ) ) ;
#32075 = VERTEX_POINT ( 'NONE', #24800 ) ;
#32076 = AXIS2_PLACEMENT_3D ( 'NONE', #70486, #1615, #55761 ) ;
#32077 = ORIENTED_EDGE ( 'NONE', *, *, #37270, .T. ) ;
#32078 = DIRECTION ( 'NONE',  ( -1.000000000000000000, 0.000000000000000000, 0.000000000000000000 ) ) ;
#32079 = CARTESIAN_POINT ( 'NONE',  ( 164.4506649252758734, 248.7574976766044585, 10.04808630291115357 ) ) ;
#32080 = ORIENTED_EDGE ( 'NONE', *, *, #60011, .F. ) ;
#32081 = DIRECTION ( 'NONE',  ( -0.8770933717188679202, -0.4803199113995043623, 0.000000000000000000 ) ) ;
#32082 = CARTESIAN_POINT ( 'NONE',  ( 155.3659625055495326, 262.0475265963984839, -17.02029351793501988 ) ) ;
#32083 = ORIENTED_EDGE ( 'NONE', *, *, #97182, .F. ) ;
#32084 = CARTESIAN_POINT ( 'NONE',  ( 162.8384627734353387, 250.8402808221231624, -13.07578932517241732 ) ) ;
#32085 = CARTESIAN_POINT ( 'NONE',  ( 79.08643767721619611, 59.41746268492353522, -16.53334974603829366 ) ) ;
#32086 = VECTOR ( 'NONE', #13622, 1000.000000000000000 ) ;
#32087 = CARTESIAN_POINT ( 'NONE',  ( 204.9004517216375518, 275.7490024547470853, 14.55104398969427670 ) ) ;
#32088 = CARTESIAN_POINT ( 'NONE',  ( 80.85195420596313909, 43.03173977397389649, 9.658905536921107426 ) ) ;
#32089 = ORIENTED_EDGE ( 'NONE', *, *, #42263, .T. ) ;
#32090 = CARTESIAN_POINT ( 'NONE',  ( 161.4396252346964218, 251.0253620690641299, 14.51972485405798885 ) ) ;
#32091 = CARTESIAN_POINT ( 'NONE',  ( 21.51366908625220731, 51.25433263228030967, 59.99999999999999289 ) ) ;
#32092 = CARTESIAN_POINT ( 'NONE',  ( 148.7588072053147243, 273.7711778218048835, -8.803803025135483296 ) ) ;
#32093 = B_SPLINE_SURFACE_WITH_KNOTS ( 'NONE', 3, 1, ( 
 ( #40443, #87136 ),
 ( #1967, #9579 ),
 ( #55140, #32852 ),
 ( #39433, #85096 ),
 ( #77971, #55634 ),
 ( #54637, #94199 ),
 ( #17668, #24753 ),
 ( #86619, #46539 ),
 ( #69357, #17153 ),
 ( #85616, #38945 ),
 ( #8566, #94693 ),
 ( #8070, #71378 ),
 ( #92695, #63761 ),
 ( #62236, #24262 ),
 ( #69851, #38443 ),
 ( #70352, #47550 ),
 ( #100276, #48051 ),
 ( #31353, #86125 ),
 ( #23246, #1476 ),
 ( #78993, #30862 ),
 ( #25255, #56138 ),
 ( #48566, #16159 ),
 ( #93188, #23743 ),
 ( #47057, #964 ),
 ( #31840, #32357 ),
 ( #63258, #62743 ),
 ( #93699, #16655 ),
 ( #78477, #9064 ),
 ( #57143, #27762 ),
 ( #79507, #18167 ),
 ( #95719, #19188 ),
 ( #66260, #11578 ),
 ( #18672, #2995 ),
 ( #57644, #42436 ) ),
 .UNSPECIFIED., .T., .F., .F.,
 ( 4, 2, 2, 2, 2, 2, 2, 2, 2, 2, 2, 2, 2, 2, 2, 2, 4 ),
 ( 2, 2 ),
 ( 0.000000000000000000, 0.06250000000000000000, 0.1250000000000000000, 0.1875000000000000000, 0.2500000000000000000, 0.3125000000000000000, 0.3750000000000000000, 0.4375000000000000000, 0.5000000000000000000, 0.5625000000000000000, 0.6250000000000000000, 0.6875000000000000000, 0.7500000000000000000, 0.8125000000000000000, 0.8750000000000000000, 0.9375000000000000000, 1.000000000000000000 ),
 ( 0.000000000000000000, 1.000000000000000000 ),
 .UNSPECIFIED. ) ;
#32094 = VERTEX_POINT ( 'NONE', #40494 ) ;
#32095 = ORIENTED_EDGE ( 'NONE', *, *, #77797, .T. ) ;
#32096 = EDGE_CURVE ( 'NONE', #3586, #55387, #78976, .T. ) ;
#32097 = ORIENTED_EDGE ( 'NONE', *, *, #53103, .T. ) ;
#32098 = CARTESIAN_POINT ( 'NONE',  ( 73.54926982385974554, 62.06432499625495325, 14.76512139019120973 ) ) ;
#32099 = ORIENTED_EDGE ( 'NONE', *, *, #55322, .T. ) ;
#32100 = ADVANCED_FACE ( 'NONE', ( #38993 ), #16208, .F. ) ;
#32101 = FACE_OUTER_BOUND ( 'NONE', #34222, .T. ) ;
#32102 = ORIENTED_EDGE ( 'NONE', *, *, #31342, .T. ) ;
#32103 = CARTESIAN_POINT ( 'NONE',  ( 164.4915767550571957, 245.7392269735623529, -6.407198159945809657 ) ) ;
#32104 = AXIS2_PLACEMENT_3D ( 'NONE', #43103, #97847, #97357 ) ;
#32105 = CARTESIAN_POINT ( 'NONE',  ( 81.87257924523440522, 45.31425140043580768, 10.75858732970988108 ) ) ;
#32106 = ADVANCED_FACE ( 'NONE', ( #85670 ), #47101, .T. ) ;
#32107 = DIRECTION ( 'NONE',  ( -1.000000000000000000, 0.000000000000000000, 0.000000000000000000 ) ) ;
#32108 = EDGE_CURVE ( 'NONE', #184, #44213, #66739, .T. ) ;
#32109 = CARTESIAN_POINT ( 'NONE',  ( 194.3541845315608612, 294.0156730581561533, -14.67567721756631016 ) ) ;
#32110 = CARTESIAN_POINT ( 'NONE',  ( 82.70749068191635445, 53.29046182800484388, -15.29114564428902234 ) ) ;
#32111 = DIRECTION ( 'NONE',  ( -0.8660254037844359321, -0.5000000000000051070, -0.000000000000000000 ) ) ;
#32112 = PLANE ( 'NONE',  #91717 ) ;
#32113 = CARTESIAN_POINT ( 'NONE',  ( 14.52983486323338802, 31.49540643055186706, 3.479690158560446702E-15 ) ) ;
#32114 = CIRCLE ( 'NONE', #19213, 5.000000000000023981 ) ;
#32115 = CARTESIAN_POINT ( 'NONE',  ( 198.6517795750437472, 276.7950782437291082, -15.35400847641894195 ) ) ;
#32116 = CARTESIAN_POINT ( 'NONE',  ( 164.3090168944849836, 246.0554299274959931, 2.641760039552302430 ) ) ;
#32118 = ORIENTED_EDGE ( 'NONE', *, *, #39399, .T. ) ;
#32117 = CARTESIAN_POINT ( 'NONE',  ( 197.8809552785519656, 287.9071269377202498, 17.61728046362068412 ) ) ;
#32119 = FACE_OUTER_BOUND ( 'NONE', #85077, .T. ) ;
#32120 = CARTESIAN_POINT ( 'NONE',  ( 168.2393331516044839, 256.9261763197810069, -14.65768061478250139 ) ) ;
#32121 = CARTESIAN_POINT ( 'NONE',  ( 159.9470087484377814, 253.6106496594791508, -16.54933891566789939 ) ) ;
#32122 = LINE ( 'NONE', #71665, #87897 ) ;
#32123 =( BOUNDED_CURVE ( )  B_SPLINE_CURVE ( 2, ( #11330, #66491, #96443, #97419, #88870, #58384, #4189, #11818, #12311 ),
 .UNSPECIFIED., .F., .T. ) 
 B_SPLINE_CURVE_WITH_KNOTS ( ( 3, 2, 2, 2, 3 ),
 ( 0.5766129032258064946, 0.5779569892473118697, 0.5806451612903226200, 0.5833333333333333703, 0.5846774193548387455 ),
 .UNSPECIFIED. ) 
 CURVE ( )  GEOMETRIC_REPRESENTATION_ITEM ( )  RATIONAL_B_SPLINE_CURVE ( ( 0.9330127018922194093, 0.9330127018922194093, 1.000000000000000000, 0.8660254037844387076, 1.000000000000000000, 0.8660254037844387076, 1.000000000000000000, 0.9330127018922194093, 0.9330127018922194093 ) ) 
 REPRESENTATION_ITEM ( '' )  );
#32124 = CARTESIAN_POINT ( 'NONE',  ( 85.51176157151247992, 45.57569484508597668, -8.758718004448168060 ) ) ;
#32125 = CARTESIAN_POINT ( 'NONE',  ( 200.6800100461949228, 283.0590218669948399, 18.32402613046234308 ) ) ;
#32126 = CARTESIAN_POINT ( 'NONE',  ( 115.2960263294082068, 225.8262482093458061, 3.021315404115420679E-15 ) ) ;
#32127 = ORIENTED_EDGE ( 'NONE', *, *, #53625, .F. ) ;
#32128 = CYLINDRICAL_SURFACE ( 'NONE', #68801, 17.82106496071139645 ) ;
#32129 =( BOUNDED_CURVE ( )  B_SPLINE_CURVE ( 2, ( #15221, #7638, #92288, #53721, #46631, #77557, #44625, #67950, #36537, #84681, #46116, #77032, #53 ),
 .UNSPECIFIED., .F., .T. ) 
 B_SPLINE_CURVE_WITH_KNOTS ( ( 3, 2, 2, 2, 2, 2, 3 ),
 ( 0.9125000000000000888, 0.9150000000000000355, 0.9200000000000000400, 0.9250000000000000444, 0.9300000000000000488, 0.9350000000000000533, 0.9375000000000000000 ),
 .UNSPECIFIED. ) 
 CURVE ( )  GEOMETRIC_REPRESENTATION_ITEM ( )  RATIONAL_B_SPLINE_CURVE ( ( 0.9755282581475767101, 0.9755282581475772652, 1.000000000000000000, 0.9510565162951535312, 1.000000000000000000, 0.9510565162951535312, 1.000000000000000000, 0.9510565162951535312, 1.000000000000000000, 0.9510565162951535312, 1.000000000000000000, 0.9755282581475768211, 0.9755282581475768211 ) ) 
 REPRESENTATION_ITEM ( '' )  );
#32130 = FACE_OUTER_BOUND ( 'NONE', #38453, .T. ) ;
#32131 = VECTOR ( 'NONE', #37629, 1000.000000000000000 ) ;
#32132 = CARTESIAN_POINT ( 'NONE',  ( 66.47763888060634940, 67.99612994687967671, 6.463816603905427449 ) ) ;
#32133 = CARTESIAN_POINT ( 'NONE',  ( 18.62362889609498851, 174.8927522451417929, -10.00000000000009059 ) ) ;
#32134 = CARTESIAN_POINT ( 'NONE',  ( 88.13101510164368335, 227.8149278399160949, -9.188101187500095079 ) ) ;
#32135 = CARTESIAN_POINT ( 'NONE',  ( 82.37597161381533795, 40.39206419195442521, -1.284498707061657585 ) ) ;
#32136 = VECTOR ( 'NONE', #13162, 1000.000000000000000 ) ;
#32137 = CARTESIAN_POINT ( 'NONE',  ( 174.5189524011659614, 282.4582611793903197, -14.74069674323029666 ) ) ;
#32138 = CARTESIAN_POINT ( 'NONE',  ( 166.9710150895549816, 278.2521958780282603, -13.38400322088418015 ) ) ;
#32139 = VECTOR ( 'NONE', #4873, 1000.000000000000000 ) ;
#32141 = CARTESIAN_POINT ( 'NONE',  ( 75.64798029740516938, 65.57340602677163588, 13.80036590763650750 ) ) ;
#32140 = CARTESIAN_POINT ( 'NONE',  ( 5.344833028331274605, 164.7048013555410080, 4.594050593750051981 ) ) ;
#32142 = CARTESIAN_POINT ( 'NONE',  ( 161.4726291907278721, 250.9681975403669867, 14.52346149734912117 ) ) ;
#32143 = ORIENTED_EDGE ( 'NONE', *, *, #60859, .T. ) ;
#32144 = VECTOR ( 'NONE', #48419, 1000.000000000000000 ) ;
#32146 = EDGE_LOOP ( 'NONE', ( #73389, #39348, #10914, #43412 ) ) ;
#32145 = UNCERTAINTY_MEASURE_WITH_UNIT (LENGTH_MEASURE( 1.000000000000000082E-05 ), #88338, 'distance_accuracy_value', 'NONE');
#32147 = FACE_OUTER_BOUND ( 'NONE', #55731, .T. ) ;
#32148 = CARTESIAN_POINT ( 'NONE',  ( 189.0883302520865641, 261.4014440129419086, -6.086672140557672250 ) ) ;
#32149 = CARTESIAN_POINT ( 'NONE',  ( 148.3005007218871754, 275.7829932922234093, 6.053100225771809839 ) ) ;
#32150 = CARTESIAN_POINT ( 'NONE',  ( 28.04762285228751395, 28.14441083166262203, 10.00000000000000533 ) ) ;
#32151 = CARTESIAN_POINT ( 'NONE',  ( 207.5462191418491500, 271.1663988579299485, -5.239401497773396699 ) ) ;
#32152 = VECTOR ( 'NONE', #22872, 1000.000000000000000 ) ;
#32153 = CARTESIAN_POINT ( 'NONE',  ( 185.0684497205900527, 286.3477220876792444, 16.15350733335134237 ) ) ;
#32154 = CARTESIAN_POINT ( 'NONE',  ( 74.21225604557145061, 68.54784490154126786, -11.57567064299385784 ) ) ;
#32155 = CARTESIAN_POINT ( 'NONE',  ( 35.79112540406920573, 179.2202760586659736, -5.415160957724236172E-17 ) ) ;
#32156 = CARTESIAN_POINT ( 'NONE',  ( 84.29722201641486379, 226.1427522451419065, 10.00000000000009237 ) ) ;
#32157 = CARTESIAN_POINT ( 'NONE',  ( 199.6370389866197570, 277.2768894341252235, 15.10745654191603826 ) ) ;
#32158 = ORIENTED_EDGE ( 'NONE', *, *, #95638, .T. ) ;
#32159 = DIRECTION ( 'NONE',  ( 0.8660254037844375974, 0.5000000000000017764, 3.252519625699413953E-16 ) ) ;
#32160 = CARTESIAN_POINT ( 'NONE',  ( 182.1677925300641618, 260.8189200811837622, -10.57058814963136939 ) ) ;
#32161 = EDGE_CURVE ( 'NONE', #28264, #42536, #26, .T. ) ;
#32162 = AXIS2_PLACEMENT_3D ( 'NONE', #9242, #41117, #16337 ) ;
#32163 = DIRECTION ( 'NONE',  ( 0.8503781557569302096, -0.05328141121993811014, 0.5234673661555743207 ) ) ;
#32164 = CARTESIAN_POINT ( 'NONE',  ( 80.58798105445690396, 57.19556934344895183, -16.22990577884235108 ) ) ;
#32165 = CARTESIAN_POINT ( 'NONE',  ( 68.87153398673127924, 63.79608234936608113, -12.28269806760821936 ) ) ;
#32166 = CARTESIAN_POINT ( 'NONE',  ( -13.55913805958770624, 162.9786897466781852, -9.594050593750095501 ) ) ;
#32167 = CARTESIAN_POINT ( 'NONE',  ( 176.2580550267919932, 278.7780497695933946, -16.99066290002705060 ) ) ;
#32168 = CARTESIAN_POINT ( 'NONE',  ( 148.3253847707240141, 273.7398928553401447, -9.074433450356286457 ) ) ;
#32169 = CARTESIAN_POINT ( 'NONE',  ( 190.0365785169351227, 262.5605203951380417, 8.321803530341849608 ) ) ;
#32170 = CARTESIAN_POINT ( 'NONE',  ( 204.1953342137782954, 276.9703018036655067, 13.84727111424505885 ) ) ;
#32171 = CARTESIAN_POINT ( 'NONE',  ( 26.50806851326374414, 176.1115022471901739, -5.000000000000041744 ) ) ;
#32172 = CARTESIAN_POINT ( 'NONE',  ( 146.6647111637776106, 276.6162639173599587, -0.6373001129109082674 ) ) ;
#32173 = CARTESIAN_POINT ( 'NONE',  ( 189.8147415777049218, 301.8782188922952514, -0.5019643756309712934 ) ) ;
#32174 = ORIENTED_EDGE ( 'NONE', *, *, #52940, .T. ) ;
#32175 = CARTESIAN_POINT ( 'NONE',  ( 152.3114242215494869, 267.6756387370063521, -15.40863746480569851 ) ) ;
#32176 = CARTESIAN_POINT ( 'NONE',  ( 163.8111161534324935, 246.9178193081252743, -7.110480325054721717 ) ) ;
#32177 = B_SPLINE_CURVE_WITH_KNOTS ( 'NONE', 3,
 ( #91897, #44243, #14845, #59939, #36645, #46223, #45731, #38123, #76653, #69040, #67551, #30555, #7750, #69547, #31041, #25444 ),
 .UNSPECIFIED., .F., .F.,
 ( 4, 1, 2, 2, 2, 1, 2, 2, 4 ),
 ( 0.000000000000000000, 0.1249999999999992506, 0.1875000000000008604, 0.2500000000000024980, 0.5000000000000014433, 0.6250000000000024425, 0.6875000000000014433, 0.7500000000000003331, 1.000000000000000000 ),
 .UNSPECIFIED. ) ;
#32178 = CARTESIAN_POINT ( 'NONE',  ( 162.1227137712282342, 251.8422180177273901, -14.11218862277787345 ) ) ;
#32179 = CARTESIAN_POINT ( 'NONE',  ( 108.9159718882352479, 227.5643266524159856, -9.188101187500093303 ) ) ;
#32180 = CARTESIAN_POINT ( 'NONE',  ( 12.13982549814181411, 27.98502408145591502, -5.678558825948271327 ) ) ;
#32181 = LINE ( 'NONE', #94029, #3924 ) ;
#32182 = CARTESIAN_POINT ( 'NONE',  ( 73.93788252295223629, 58.97677190194296770, -16.17750573964183403 ) ) ;
#32184 = CARTESIAN_POINT ( 'NONE',  ( 191.5665563241051359, 276.8936798736086757, 16.95695192525134587 ) ) ;
#32183 = DIRECTION ( 'NONE',  ( -0.8660254037844387076, -0.4999999999999998890, -0.000000000000000000 ) ) ;
#32185 = CARTESIAN_POINT ( 'NONE',  ( 191.3376789240739697, 299.2404140316400003, -7.572576518662374134 ) ) ;
#32186 = CARTESIAN_POINT ( 'NONE',  ( 192.0543497034057054, 263.3254378250766763, -4.345169357874051563 ) ) ;
#32187 = CARTESIAN_POINT ( 'NONE',  ( 149.1004267900891307, 272.3974806997987343, -12.86882154300063341 ) ) ;
#32188 = CARTESIAN_POINT ( 'NONE',  ( 49.38557292990258674, 205.9865022471902876, 10.00000000000009415 ) ) ;
#32189 = LINE ( 'NONE', #94037, #74205 ) ;
#32190 = CARTESIAN_POINT ( 'NONE',  ( 76.26946404230704957, 64.97317754398874001, 14.67006731301515998 ) ) ;
#32191 = ORIENTED_EDGE ( 'NONE', *, *, #20988, .T. ) ;
#32192 = CARTESIAN_POINT ( 'NONE',  ( 189.7324944835817178, 265.9585424814845851, 10.76132878117026159 ) ) ;
#32193 = CARTESIAN_POINT ( 'NONE',  ( 71.98264401366868981, 72.39816763649429276, -2.869464145551841039 ) ) ;
#32194 = CARTESIAN_POINT ( 'NONE',  ( 196.5613103808260860, 267.5413228629882383, 9.637417835835831781 ) ) ;
#32195 = EDGE_LOOP ( 'NONE', ( #41557, #22108, #73738, #28119 ) ) ;
#32196 = CARTESIAN_POINT ( 'NONE',  ( 72.09021951009610518, 72.27625441170016529, 1.322546034541348225 ) ) ;
#32197 = CARTESIAN_POINT ( 'NONE',  ( -22.42236680055709641, 157.8615022471902591, 0.000000000000000000 ) ) ;
#32199 = CARTESIAN_POINT ( 'NONE',  ( 83.90043522580160129, 51.91099903043517827, -14.50837359699251294 ) ) ;
#32198 = B_SPLINE_CURVE_WITH_KNOTS ( 'NONE', 3,
 ( #55292, #53791, #84753, #61896, #40093, #24909, #71036, #54288, #31499, #92357, #93861, #86273, #62391, #55784, #7712, #54806, #15292, #93348, #86776, #46191, #85783, #9742 ),
 .UNSPECIFIED., .F., .F.,
 ( 4, 1, 1, 2, 2, 1, 1, 2, 2, 1, 1, 2, 2, 4 ),
 ( 0.5972366333919344461, 0.6475820542179384631, 0.6727547646309413043, 0.6853411198374419477, 0.6979274750439424801, 0.7482728958699466082, 0.7734456062829488943, 0.7860319614894499818, 0.7986183166959511803, 0.8489637375219629689, 0.8741364479349700289, 0.8867228031414734479, 0.8993091583479768669, 1.000000000000000000 ),
 .UNSPECIFIED. ) ;
#32200 = CARTESIAN_POINT ( 'NONE',  ( 172.9438399295877957, 262.8668947608421718, -16.49499919880818766 ) ) ;
#32201 = CARTESIAN_POINT ( 'NONE',  ( 192.6224552386041182, 297.0151161785129261, 12.49354144254605181 ) ) ;
#32202 = CARTESIAN_POINT ( 'NONE',  ( 190.9225659192872229, 280.7668985173125975, 16.65464037187561175 ) ) ;
#32203 = AXIS2_PLACEMENT_3D ( 'NONE', #10989, #41351, #34754 ) ;
#32204 = CARTESIAN_POINT ( 'NONE',  ( 30.66616357392367220, 39.74646525600392977, 2.839279412974139660 ) ) ;
#32205 = CARTESIAN_POINT ( 'NONE',  ( 83.56516159190486803, 41.02999554113897318, 0.5818837730058337154 ) ) ;
#32206 = VERTEX_POINT ( 'NONE', #58680 ) ;
#32207 = CARTESIAN_POINT ( 'NONE',  ( 164.3996301846870267, 247.3020492865104529, 7.248807534621905191 ) ) ;
#32208 = DIRECTION ( 'NONE',  ( -0.9659258262890730862, 0.2588190451025027539, -3.627714260166394782E-16 ) ) ;
#32209 = CARTESIAN_POINT ( 'NONE',  ( -62.46655456400515050, 61.78343361634738073, 59.99999999999999289 ) ) ;
#32210 = ORIENTED_EDGE ( 'NONE', *, *, #86399, .F. ) ;
#32211 = CIRCLE ( 'NONE', #35398, 70.00000000000001421 ) ;
#32212 = CARTESIAN_POINT ( 'NONE',  ( 86.43064670831508067, 47.06455762112943120, -10.03233545160486706 ) ) ;
#32213 = CARTESIAN_POINT ( 'NONE',  ( -8.669243101527598583, 25.19333184544593252, 10.00000000000000000 ) ) ;
#32214 = CARTESIAN_POINT ( 'NONE',  ( 204.2133777088835700, 276.9390495533970693, 13.75768580338462144 ) ) ;
#32215 = B_SPLINE_CURVE_WITH_KNOTS ( 'NONE', 3,
 ( #94545, #25099, #65958, #21848, #29450, #98375, #67446, #89324, #5650, #52244, #36540, #28963, #35557, #60326, #82210, #98871, #83188, #37044, #91282, #13275, #27480, #58348, #51766, #81210, #35051, #89797, #43134, #11782, #74584, #12781, #20876, #75562, #42642, #6150, #97873, #43646, #44137, #13748, #96909, #75071, #73572, #4154, #19878, #90804, #82708, #36042, #50748, #81701, #12274, #59841, #21359, #74076 ),
 .UNSPECIFIED., .F., .F.,
 ( 4, 2, 2, 2, 2, 2, 2, 2, 2, 2, 2, 2, 2, 2, 2, 2, 2, 2, 2, 2, 2, 2, 2, 2, 2, 4 ),
 ( 0.0001369149182890826025, 0.001149345445623905365, 0.001402453077457536598, 0.001655560709291167831, 0.001782114525207983882, 0.001908668341124799498, 0.002035222157041615115, 0.002161775972958430731, 0.002414883604792085817, 0.002667991236625740469, 0.003174206500293014210, 0.004186637027627614603, 0.005199067554962213261, 0.005705282818629513891, 0.005958390450463124308, 0.006084944266379932985, 0.006211498082296740796, 0.006274774990255143833, 0.006338051898213546871, 0.006464605714130344273, 0.006717713345963950353, 0.007223928609631210217, 0.007477036241464778132, 0.007730143873298345181, 0.007983251505131912229, 0.008236359136965481012 ),
 .UNSPECIFIED. ) ;
#32216 = CARTESIAN_POINT ( 'NONE',  ( -167.0327448629461742, 42.61639673982678289, -30.52142883766498116 ) ) ;
#32217 = CARTESIAN_POINT ( 'NONE',  ( 32.24342178309110096, 47.97677246190462341, -10.00000000000000000 ) ) ;
#32218 = VECTOR ( 'NONE', #73289, 1000.000000000000000 ) ;
#32219 = LINE ( 'NONE', #1836, #48569 ) ;
#32220 = CARTESIAN_POINT ( 'NONE',  ( -13.11024591527723615, 15.00000000000000000, -32.50000000000017053 ) ) ;
#32221 = ORIENTED_EDGE ( 'NONE', *, *, #35498, .T. ) ;
#32222 = ORIENTED_EDGE ( 'NONE', *, *, #81676, .T. ) ;
#32223 = CARTESIAN_POINT ( 'NONE',  ( 175.0525616523904091, 258.5361325477437049, 12.82765623556165835 ) ) ;
#32224 = EDGE_LOOP ( 'NONE', ( #99626, #97027, #35624, #45310 ) ) ;
#32225 = CARTESIAN_POINT ( 'NONE',  ( 77.13583932239204444, 49.51254683941623824, -14.95790760833234678 ) ) ;
#32226 = VERTEX_POINT ( 'NONE', #11625 ) ;
#32227 = CARTESIAN_POINT ( 'NONE',  ( 173.2978849248910365, 270.6387814481042255, 17.71865970584200767 ) ) ;
#32229 = CARTESIAN_POINT ( 'NONE',  ( 79.44876042842709296, 54.60773761053498987, 15.97065083431682275 ) ) ;
#32228 = VECTOR ( 'NONE', #29775, 1000.000000000000000 ) ;
#32230 = ORIENTED_EDGE ( 'NONE', *, *, #55194, .F. ) ;
#32231 = CARTESIAN_POINT ( 'NONE',  ( 185.1874674929625542, 281.7807588590592331, -16.37341951865305489 ) ) ;
#32232 = CARTESIAN_POINT ( 'NONE',  ( 164.7349053118283564, 245.3177695503021027, -2.492200678360605437 ) ) ;
#32233 = CARTESIAN_POINT ( 'NONE',  ( 147.9420216129083769, 274.4038973224264168, -6.684832208247039276 ) ) ;
#32234 = CARTESIAN_POINT ( 'NONE',  ( 196.0610340319988154, 284.4280829583078685, -17.56065396538383894 ) ) ;
#32235 = CARTESIAN_POINT ( 'NONE',  ( 82.70122523897394728, 40.55072272859479909, 0.9023291622205993345 ) ) ;
#32236 = CARTESIAN_POINT ( 'NONE',  ( 186.4022004759940501, 277.8269278096638004, -17.81691120636144277 ) ) ;
#32237 = ADVANCED_FACE ( 'NONE', ( #12622 ), #41494, .T. ) ;
#32238 = LINE ( 'NONE', #62118, #79274 ) ;
#32239 = CARTESIAN_POINT ( 'NONE',  ( 157.9319255052028836, 280.9761857261652267, 2.111273384039783707 ) ) ;
#32240 = CARTESIAN_POINT ( 'NONE',  ( 130.8370663736463655, 246.3458772461660544, 9.188101187500095079 ) ) ;
#32241 = CARTESIAN_POINT ( 'NONE',  ( 186.9363924785116922, 262.3438794472209565, -10.23320327271459362 ) ) ;
#32242 = ORIENTED_EDGE ( 'NONE', *, *, #63926, .T. ) ;
#32243 = AXIS2_PLACEMENT_3D ( 'NONE', #84924, #55464, #86451 ) ;
#32244 = B_SPLINE_CURVE_WITH_KNOTS ( 'NONE', 3,
 ( #17213, #32918, #9649, #1031, #63822, #85687, #93771, #47117, #9130, #87204, #64324, #31909, #78038, #17736, #54199, #8629, #70941, #1544 ),
 .UNSPECIFIED., .F., .F.,
 ( 4, 2, 2, 2, 2, 2, 2, 2, 4 ),
 ( 1.040834085586084257E-17, 0.0002877161428173316722, 0.0005754322856346529361, 0.0008631484284519741999, 0.001150864571269295464, 0.001438580714086616728, 0.001726296856903937992, 0.002014012999721259255, 0.002301729142538580519 ),
 .UNSPECIFIED. ) ;
#32246 = ORIENTED_EDGE ( 'NONE', *, *, #93627, .F. ) ;
#32245 = CARTESIAN_POINT ( 'NONE',  ( 22.60804823384966156, 31.79103043416549923, 8.090169943749478065 ) ) ;
#32247 = CARTESIAN_POINT ( 'NONE',  ( 111.7912168577913974, 246.8967562850347122, -4.648177544792955347E-16 ) ) ;
#32248 = CARTESIAN_POINT ( 'NONE',  ( 180.7877033413244021, 256.2435947011284725, 1.191093872994401393 ) ) ;
#32249 = LINE ( 'NONE', #79897, #10765 ) ;
#32250 = CARTESIAN_POINT ( 'NONE',  ( 190.5440129798993212, 300.2296708901008628, 2.619235206888629541 ) ) ;
#32251 = CARTESIAN_POINT ( 'NONE',  ( 73.66446749447686670, 67.99659565248040849, 11.28331122821951560 ) ) ;
#32252 = CARTESIAN_POINT ( 'NONE',  ( -19.65312891409030271, 93.06504152958497400, 10.00000000000000000 ) ) ;
#32253 = CARTESIAN_POINT ( 'NONE',  ( 169.3277966998927866, 263.8928266120187800, -17.36417683515335142 ) ) ;
#32254 = CARTESIAN_POINT ( 'NONE',  ( 148.2098452982477568, 273.9400130919484582, 10.40469228891075026 ) ) ;
#32255 = CARTESIAN_POINT ( 'NONE',  ( 33.63407072503001416, 49.62913085183823370, -10.00000000000000000 ) ) ;
#32256 = ORIENTED_EDGE ( 'NONE', *, *, #97587, .T. ) ;
#32257 = CARTESIAN_POINT ( 'NONE',  ( 148.3629184514745987, 273.6748826132846375, -8.219814532462343948 ) ) ;
#32258 = CARTESIAN_POINT ( 'NONE',  ( -6.281727404287059890, 25.63055774385195917, 10.00000000000000000 ) ) ;
#32259 = EDGE_LOOP ( 'NONE', ( #52528, #94238, #44454, #86918 ) ) ;
#32260 = CYLINDRICAL_SURFACE ( 'NONE', #33826, 15.60714546451156970 ) ;
#32261 = CARTESIAN_POINT ( 'NONE',  ( 157.2721445379966951, 276.7763377113812453, 10.24542939855939849 ) ) ;
#32262 = CARTESIAN_POINT ( 'NONE',  ( 151.7267614974901733, 267.8485355488985533, -16.42520090999607874 ) ) ;
#32263 = CARTESIAN_POINT ( 'NONE',  ( 190.8072577185990610, 300.1591305089344814, 3.698484652594827171 ) ) ;
#32264 = CARTESIAN_POINT ( 'NONE',  ( 14.65434579541631521, 169.2677522451417929, -5.000000000000041744 ) ) ;
#32266 = CARTESIAN_POINT ( 'NONE',  ( 153.4834637178363153, 276.1882586661345726, -8.644278876002948309 ) ) ;
#32265 = CARTESIAN_POINT ( 'NONE',  ( 161.4920976794100795, 281.5001473778777381, -6.616262511153973236 ) ) ;
#32267 = CARTESIAN_POINT ( 'NONE',  ( 200.5039526449628795, 267.3497397166782434, 6.370409075474873006 ) ) ;
#32268 = EDGE_LOOP ( 'NONE', ( #80278, #96818, #46591, #33153 ) ) ;
#32269 = CARTESIAN_POINT ( 'NONE',  ( 147.0538900202505488, 275.9421863647172017, 5.192507380313251986 ) ) ;
#32270 = CARTESIAN_POINT ( 'NONE',  ( 73.78372473906969731, 65.88421683824888930, 13.39692504310327692 ) ) ;
#32271 = CARTESIAN_POINT ( 'NONE',  ( 157.2948870673828026, 280.9759411348209142, 6.053012778684776940 ) ) ;
#32272 = CARTESIAN_POINT ( 'NONE',  ( -22.42236680055709641, 157.8615022471902591, 0.000000000000000000 ) ) ;
#32273 = CARTESIAN_POINT ( 'NONE',  ( 187.5025819648600134, 297.9165075386694639, -4.258172756825077343 ) ) ;
#32274 = CARTESIAN_POINT ( 'NONE',  ( 204.2143397907769611, 276.5280330293650195, 13.36303585211030054 ) ) ;
#32275 = CARTESIAN_POINT ( 'NONE',  ( 74.20995892610953604, 68.60058487300136676, 11.52733404855581867 ) ) ;
#32276 = CARTESIAN_POINT ( 'NONE',  ( 73.90039612685991699, 68.57416616861503655, 10.88887154151077397 ) ) ;
#32277 = CARTESIAN_POINT ( 'NONE',  ( 70.70154975520648577, 71.34200407928535981, -2.184243020790304524 ) ) ;
#32278 = DIRECTION ( 'NONE',  ( -0.8660254037844384856, -0.5000000000000002220, -3.252519625699449945E-16 ) ) ;
#32279 = CARTESIAN_POINT ( 'NONE',  ( 86.66977078063996487, 220.8458772461660544, 9.188101187500095079 ) ) ;
#32280 = DIRECTION ( 'NONE',  ( 0.8660254037844382635, 0.5000000000000005551, 0.000000000000000000 ) ) ;
#32281 = CARTESIAN_POINT ( 'NONE',  ( 192.4212750754384160, 297.3635704425909125, -12.73704185013552248 ) ) ;
#32282 = CARTESIAN_POINT ( 'NONE',  ( -89.11465314115665137, 93.37593066204027537, 37.50000000000002132 ) ) ;
#32283 = B_SPLINE_CURVE_WITH_KNOTS ( 'NONE', 3,
 ( #99092, #37756, #92025, #76294 ),
 .UNSPECIFIED., .F., .F.,
 ( 4, 4 ),
 ( 0.01312060649816892619, 0.01948601111665982516 ),
 .UNSPECIFIED. ) ;
#32285 = CARTESIAN_POINT ( 'NONE',  ( 78.19980343102787401, 47.50132803318881258, 14.37731510607409646 ) ) ;
#32284 = CIRCLE ( 'NONE', #1567, 14.82106496071144619 ) ;
#32286 = EDGE_CURVE ( 'NONE', #65623, #71581, #13610, .T. ) ;
#32287 = AXIS2_PLACEMENT_3D ( 'NONE', #42016, #87700, #25318 ) ;
#32288 = CARTESIAN_POINT ( 'NONE',  ( 78.02231740044358332, 54.72928692317312027, 16.06689032128053896 ) ) ;
#32289 = SURFACE_SIDE_STYLE ('',( #1408 ) ) ;
#32290 = CARTESIAN_POINT ( 'NONE',  ( 77.77623215880998941, 62.01577911499505547, 15.64215120907620005 ) ) ;
#32292 = CARTESIAN_POINT ( 'NONE',  ( 76.24073292652140310, 51.11943835579473472, 16.06739483476730967 ) ) ;
#32291 = CARTESIAN_POINT ( 'NONE',  ( 189.3775153017087973, 300.6355170167246911, -1.634152055493470757 ) ) ;
#32293 = CARTESIAN_POINT ( 'NONE',  ( 161.9230673771116358, 250.1880157158810505, 12.87702452034784883 ) ) ;
#32294 = CARTESIAN_POINT ( 'NONE',  ( 169.2311904526189323, 252.2068874694283238, -9.079601461500399040 ) ) ;
#32295 = CARTESIAN_POINT ( 'NONE',  ( 161.4297399252889136, 251.4380930145043180, 13.08186051037274922 ) ) ;
#32296 = CARTESIAN_POINT ( 'NONE',  ( 157.1837449796689725, 258.3967629017010381, 16.97243084443542216 ) ) ;
#32297 = CARTESIAN_POINT ( 'NONE',  ( -5.676897265278508797, 155.9824982072973683, -6.972266317189433020E-16 ) ) ;
#32298 = EDGE_CURVE ( 'NONE', #66637, #25284, #96778, .T. ) ;
#32299 = CIRCLE ( 'NONE', #87348, 70.00000000000001421 ) ;
#32300 = CARTESIAN_POINT ( 'NONE',  ( 37.27951979288245354, 183.1423013555409796, -4.594050593750043987 ) ) ;
#32301 = EDGE_CURVE ( 'NONE', #16291, #5537, #53580, .T. ) ;
#32302 = CARTESIAN_POINT ( 'NONE',  ( 77.36034478572226192, 203.2202760586659736, -5.415160957724236172E-17 ) ) ;
#32303 = DIRECTION ( 'NONE',  ( -0.000000000000000000, -0.000000000000000000, -1.000000000000000000 ) ) ;
#32304 = FACE_OUTER_BOUND ( 'NONE', #57665, .T. ) ;
#32305 = CARTESIAN_POINT ( 'NONE',  ( 84.36110011788976237, 49.31626265921352115, -12.91867116132553761 ) ) ;
#32307 = CARTESIAN_POINT ( 'NONE',  ( 72.69493809724967548, 71.16443809380129437, -7.267007365939472052 ) ) ;
#32306 = CARTESIAN_POINT ( 'NONE',  ( 86.69305172099772960, 43.39454550306078318, -4.013483749032378256 ) ) ;
#32309 = VECTOR ( 'NONE', #19152, 1000.000000000000000 ) ;
#32308 = CARTESIAN_POINT ( 'NONE',  ( 196.2417448688663626, 269.4613107492011181, -10.73862409626361369 ) ) ;
#32310 = CARTESIAN_POINT ( 'NONE',  ( 31.93509797303403630, 20.29860640527293825, -2.839279412974138328 ) ) ;
#32311 = CARTESIAN_POINT ( 'NONE',  ( 72.44129552685039641, 70.67501955208014408, -7.848061272651224662 ) ) ;
#32312 = CARTESIAN_POINT ( 'NONE',  ( 81.98039554206116009, 47.27905221821983162, -12.37811565305940142 ) ) ;
#32313 = CARTESIAN_POINT ( 'NONE',  ( 9.022134044517839513, 26.18502408145589655, 5.678558825948277544 ) ) ;
#32314 = CARTESIAN_POINT ( 'NONE',  ( 67.34640541081718368, 215.8149278399160664, -9.188101187500095079 ) ) ;
#32315 = CARTESIAN_POINT ( 'NONE',  ( 99.59154365750384841, 216.7592609112380444, 2.679491924311254714 ) ) ;
#32316 = CARTESIAN_POINT ( 'NONE',  ( 155.4495868485232108, 261.4004128932040203, -18.48326470492642315 ) ) ;
#32317 = CARTESIAN_POINT ( 'NONE',  ( 159.2111180226792726, 254.8852497853115722, 16.01057445397460910 ) ) ;
#32318 = CARTESIAN_POINT ( 'NONE',  ( 187.6582181093866382, 259.5698042993466288, -5.491801991258111748 ) ) ;
#32319 = CARTESIAN_POINT ( 'NONE',  ( 202.0830002332459117, 280.6289715805018545, 17.37494336322426136 ) ) ;
#32320 = AXIS2_PLACEMENT_3D ( 'NONE', #78030, #79054, #31903 ) ;
#32321 = CARTESIAN_POINT ( 'NONE',  ( 80.19044581452921250, 55.04695057392905255, -15.97072302619556261 ) ) ;
#32322 = CARTESIAN_POINT ( 'NONE',  ( 87.52040938742109688, 45.06780532364838621, -6.102424753035670335 ) ) ;
#32323 = CARTESIAN_POINT ( 'NONE',  ( 117.4407359106297974, 228.6115022471901739, -5.000000000000041744 ) ) ;
#32324 = CARTESIAN_POINT ( 'NONE',  ( 161.4726291907278721, 250.9681975403669867, 14.52346149734912117 ) ) ;
#32325 = CARTESIAN_POINT ( 'NONE',  ( 164.3138894970802824, 246.0469903322357368, -2.642126690130961020 ) ) ;
#32326 = ORIENTED_EDGE ( 'NONE', *, *, #8589, .T. ) ;
#32327 = CARTESIAN_POINT ( 'NONE',  ( 77.07045653762983761, 49.53584601179438351, 14.97980822837095793 ) ) ;
#32328 = CARTESIAN_POINT ( 'NONE',  ( 185.4693431800836549, 271.4295055675165713, 16.77522542003663020 ) ) ;
#32329 = ORIENTED_EDGE ( 'NONE', *, *, #29393, .T. ) ;
#32330 = CARTESIAN_POINT ( 'NONE',  ( 206.2041691044954348, 273.4908977089264113, -9.455375957961031474 ) ) ;
#32331 = FACE_OUTER_BOUND ( 'NONE', #58158, .T. ) ;
#32332 = DIRECTION ( 'NONE',  ( -0.8660254037844387076, -0.4999999999999998890, -0.000000000000000000 ) ) ;
#32333 = VERTEX_POINT ( 'NONE', #98726 ) ;
#32334 = CARTESIAN_POINT ( 'NONE',  ( 177.1640644942122265, 252.7834580030144878, -0.2671950879854613770 ) ) ;
#32335 = VERTEX_POINT ( 'NONE', #13121 ) ;
#32336 = CARTESIAN_POINT ( 'NONE',  ( 156.6812872898450735, 261.2670451491295012, 0.000000000000000000 ) ) ;
#32337 = B_SPLINE_CURVE_WITH_KNOTS ( 'NONE', 3,
 ( #75869, #6448, #99652, #92095, #30238, #43044, #53526, #37327, #81613, #73988, #68228, #4572, #67745, #98670, #99151, #75186, #82813, #51358, #20486, #40877, #58936, #12388, #71823, #32797 ),
 .UNSPECIFIED., .F., .F.,
 ( 4, 2, 2, 2, 2, 2, 2, 2, 2, 2, 2, 4 ),
 ( 0.000000000000000000, 0.1249999999999957534, 0.2499999999999915068, 0.3749999999999872324, 0.4374999999999828471, 0.4999999999999784617, 0.5624999999999741318, 0.6249999999999698019, 0.6874999999999654721, 0.7499999999999611422, 0.8749999999999805711, 1.000000000000000000 ),
 .UNSPECIFIED. ) ;
#32338 = CARTESIAN_POINT ( 'NONE',  ( 48.93451802855033606, 192.3927522451418213, 10.00000000000009948 ) ) ;
#32339 = CARTESIAN_POINT ( 'NONE',  ( 206.9658671503163134, 271.7722489768942182, -5.682263345440972557 ) ) ;
#32340 = VERTEX_POINT ( 'NONE', #99209 ) ;
#32341 = CARTESIAN_POINT ( 'NONE',  ( 25.52954022263673295, 23.24335787977764056, -9.188101187500008038 ) ) ;
#32342 = CARTESIAN_POINT ( 'NONE',  ( 66.60594655232844730, 69.00361448147799592, -1.130437426683872149 ) ) ;
#32343 = CARTESIAN_POINT ( 'NONE',  ( 74.82458239918585718, 66.79921256097772186, -13.19236156228707024 ) ) ;
#32344 = CARTESIAN_POINT ( 'NONE',  ( 85.04986998970780121, 47.88075954187213767, -11.53627252243822099 ) ) ;
#32345 = ADVANCED_FACE ( 'NONE', ( #84534 ), #41689, .F. ) ;
#32346 = EDGE_CURVE ( 'NONE', #89501, #45207, #14603, .T. ) ;
#32347 = ORIENTED_EDGE ( 'NONE', *, *, #76478, .F. ) ;
#32348 = PLANE ( 'NONE',  #40027 ) ;
#32349 = CARTESIAN_POINT ( 'NONE',  ( 206.5237403681858552, 272.9373840435757188, -10.81420335655575116 ) ) ;
#32350 = ORIENTED_EDGE ( 'NONE', *, *, #49738, .F. ) ;
#32351 = CARTESIAN_POINT ( 'NONE',  ( 171.5552605186996686, 284.7348010384742452, 10.70351548841014555 ) ) ;
#32353 = CARTESIAN_POINT ( 'NONE',  ( 68.33289931102945047, 65.68983735164607651, -10.34968271987537669 ) ) ;
#32352 = CARTESIAN_POINT ( 'NONE',  ( 68.04192742210889833, 65.44532392020195743, 10.42765866839662081 ) ) ;
#32354 = CARTESIAN_POINT ( 'NONE',  ( -11.40312891409031693, 78.77562236714182120, 59.99999999999999289 ) ) ;
#32355 = CARTESIAN_POINT ( 'NONE',  ( 155.3017250444513024, 261.6565170503553190, 18.58368563027307374 ) ) ;
#32356 = CARTESIAN_POINT ( 'NONE',  ( 185.4281315057809252, 292.4669413526785888, -10.95545331475209672 ) ) ;
#32357 = CARTESIAN_POINT ( 'NONE',  ( 157.1965120183049578, 258.3746497421212780, -18.06591467563559306 ) ) ;
#32358 = CARTESIAN_POINT ( 'NONE',  ( 150.1064787036151245, 245.2202760586659167, -5.415160957724236172E-17 ) ) ;
#32359 = VECTOR ( 'NONE', #65889, 1000.000000000000000 ) ;
#32360 = ADVANCED_FACE ( 'NONE', ( #43979 ), #31859, .T. ) ;
#32361 = CARTESIAN_POINT ( 'NONE',  ( 206.4640599017556895, 270.6242529349663073, 2.487210561828315125 ) ) ;
#32362 = CARTESIAN_POINT ( 'NONE',  ( -19.65312891409030271, 93.06504152958497400, 20.00000000000000355 ) ) ;
#32363 = CARTESIAN_POINT ( 'NONE',  ( 93.00275509369619442, 218.3768266524159856, -9.188101187500091527 ) ) ;
#32364 = ORIENTED_EDGE ( 'NONE', *, *, #50394, .T. ) ;
#32365 = CARTESIAN_POINT ( 'NONE',  ( 191.4941427383744781, 298.9694107557253346, 8.584406880462095657 ) ) ;
#32366 = CARTESIAN_POINT ( 'NONE',  ( 78.17116731237634042, 61.83023861435394508, -16.09040300007290725 ) ) ;
#32367 = ORIENTED_EDGE ( 'NONE', *, *, #73883, .F. ) ;
#32368 = CARTESIAN_POINT ( 'NONE',  ( 75.98104421109889017, 51.53574906954564483, 16.18761828508177203 ) ) ;
#32369 = ORIENTED_EDGE ( 'NONE', *, *, #55279, .T. ) ;
#32370 = CARTESIAN_POINT ( 'NONE',  ( 80.08699412898864978, 44.58265640332982116, -11.70218130687201885 ) ) ;
#32371 = ADVANCED_FACE ( 'NONE', ( #45070 ), #69866, .T. ) ;
#32372 = DIRECTION ( 'NONE',  ( 0.000000000000000000, -0.3470917258701496921, 0.9378311862123591691 ) ) ;
#32373 = CARTESIAN_POINT ( 'NONE',  ( 146.5095091551180815, 276.8850816817948726, 0.1418322875769769398 ) ) ;
#32374 = CARTESIAN_POINT ( 'NONE',  ( 81.03183881876289263, 56.09329797361272085, 16.10623978537670098 ) ) ;
#32375 = CARTESIAN_POINT ( 'NONE',  ( 85.27864792750219181, 47.17654793273538161, -10.80350663618311557 ) ) ;
#32376 = CARTESIAN_POINT ( 'NONE',  ( 162.4198556707359842, 249.3275531507180460, 11.06129461055015106 ) ) ;
#32377 = CARTESIAN_POINT ( 'NONE',  ( 71.75763553740291911, 221.4244531367911293, -4.594050593750046652 ) ) ;
#32378 = VERTEX_POINT ( 'NONE', #10582 ) ;
#32379 = VECTOR ( 'NONE', #23548, 1000.000000000000000 ) ;
#32380 = ORIENTED_EDGE ( 'NONE', *, *, #18984, .F. ) ;
#32381 = B_SPLINE_CURVE_WITH_KNOTS ( 'NONE', 3,
 ( #19528, #50388, #81340, #11914 ),
 .UNSPECIFIED., .F., .F.,
 ( 4, 4 ),
 ( 0.02696644195202606634, 0.03618975469407011841 ),
 .UNSPECIFIED. ) ;
#32382 = CARTESIAN_POINT ( 'NONE',  ( 115.4741365526546417, 244.1427522451419350, 10.00000000000009415 ) ) ;
#32383 = B_SPLINE_SURFACE_WITH_KNOTS ( 'NONE', 3, 1, ( 
 ( #15567, #53088 ),
 ( #30292, #91624 ),
 ( #46470, #77906 ),
 ( #61180, #84042 ),
 ( #38373, #31279 ),
 ( #93623, #69286 ),
 ( #92147, #77400 ),
 ( #45479, #92626 ),
 ( #22194, #14600 ),
 ( #68781, #62167 ),
 ( #100211, #7478 ),
 ( #8493, #93116 ),
 ( #22700, #76413 ),
 ( #6986, #37871 ),
 ( #39363, #23668 ),
 ( #54560, #53577 ),
 ( #16085, #30797 ),
 ( #85544, #61676 ),
 ( #15076, #46991 ),
 ( #70277, #888 ),
 ( #31767, #45965 ),
 ( #76882, #62671 ),
 ( #24190, #55073 ),
 ( #86059, #16585 ),
 ( #47481, #78405 ),
 ( #8986, #39857 ),
 ( #70792, #1402 ),
 ( #73302, #72313 ),
 ( #56581, #25702 ),
 ( #32281, #94128 ),
 ( #9502, #87055 ),
 ( #41884, #10492 ),
 ( #40864, #48496 ),
 ( #2919, #63688 ) ),
 .UNSPECIFIED., .T., .F., .F.,
 ( 4, 2, 2, 2, 2, 2, 2, 2, 2, 2, 2, 2, 2, 2, 2, 2, 4 ),
 ( 2, 2 ),
 ( 0.000000000000000000, 0.06250000000000000000, 0.1250000000000000000, 0.1875000000000000000, 0.2500000000000000000, 0.3125000000000000000, 0.3750000000000000000, 0.4375000000000000000, 0.5000000000000000000, 0.5625000000000000000, 0.6250000000000000000, 0.6875000000000000000, 0.7500000000000000000, 0.8125000000000000000, 0.8750000000000000000, 0.9375000000000000000, 1.000000000000000000 ),
 ( 0.000000000000000000, 1.000000000000000000 ),
 .UNSPECIFIED. ) ;
#32384 = CARTESIAN_POINT ( 'NONE',  ( 163.0424334805279045, 248.2492167524936804, -9.671494865076915914 ) ) ;
#32385 = ORIENTED_EDGE ( 'NONE', *, *, #57742, .T. ) ;
#32386 = CARTESIAN_POINT ( 'NONE',  ( 76.23159145087653599, 64.83013986238610471, -14.34096891692713704 ) ) ;
#32387 = CARTESIAN_POINT ( 'NONE',  ( 183.8301289239822722, 272.2411597453489662, -17.34995410509954183 ) ) ;
#32388 = CARTESIAN_POINT ( 'NONE',  ( 187.4250779816339900, 264.0915145022557908, -12.27137290262548852 ) ) ;
#32390 = B_SPLINE_CURVE_WITH_KNOTS ( 'NONE', 3,
 ( #77661, #15829, #1149, #46734, #62933, #86299, #16833, #47720, #71058, #32543, #94377, #17333, #69033, #80181, #48754, #71558, #25955, #25434, #81182, #50227, #11749, #33545, #11262, #79686, #2155, #96372, #65431, #10247, #42612, #56827, #26450, #64944, #87813, #96879, #18351, #57325, #88297, #18853, #49734, #80687, #10747, #49244, #40621, #42125, #64441, #57823, #34054, #41623 ),
 .UNSPECIFIED., .F., .F.,
 ( 4, 2, 2, 2, 2, 2, 2, 2, 2, 2, 2, 2, 2, 2, 2, 2, 2, 2, 2, 2, 2, 2, 2, 4 ),
 ( 0.0008566085972837732439, 0.001056739686836194372, 0.001156805231612405152, 0.001256870776388615716, 0.001457001865941131603, 0.001657132955493647707, 0.002057395134598692492, 0.002457657313703737710, 0.003258181671913780008, 0.004058706030123822306, 0.004859230388333865905, 0.005259492567438886837, 0.005459623656991471896, 0.005559689201767801722, 0.005609721974155967503, 0.005659754746544131548, 0.005709787518932297329, 0.005759820291320463109, 0.005859885836096787731, 0.006060016925649376260, 0.006460279104754438825, 0.006860541283859499656, 0.007060672373412010122, 0.007260803462964518853 ),
 .UNSPECIFIED. ) ;
#32389 = PLANE ( 'NONE',  #67255 ) ;
#32391 = ORIENTED_EDGE ( 'NONE', *, *, #28791, .T. ) ;
#32392 = CARTESIAN_POINT ( 'NONE',  ( 85.39547059847991761, 43.80125623371271359, -5.793701783558419471 ) ) ;
#32393 = CARTESIAN_POINT ( 'NONE',  ( -105.0000000000000000, 4.999999999999999112, -54.99999999999999289 ) ) ;
#32394 = CARTESIAN_POINT ( 'NONE',  ( 206.1405152101578437, 273.6011494880188479, -9.618815605734603480 ) ) ;
#32395 = LINE ( 'NONE', #94234, #20608 ) ;
#32396 = LINE ( 'NONE', #86161, #62498 ) ;
#32397 = CARTESIAN_POINT ( 'NONE',  ( 109.5562962934610738, 227.3927522451417929, -10.00000000000009237 ) ) ;
#32398 = CYLINDRICAL_SURFACE ( 'NONE', #37283, 17.82106496071139645 ) ;
#32399 = VERTEX_POINT ( 'NONE', #3006 ) ;
#32400 = CARTESIAN_POINT ( 'NONE',  ( 202.8239709173147389, 277.7017072501616894, -15.26945558628286470 ) ) ;
#32401 = CARTESIAN_POINT ( 'NONE',  ( 161.5875797534026219, 250.7690973254556468, 12.95526170413129030 ) ) ;
#32402 = CARTESIAN_POINT ( 'NONE',  ( 82.91132241635402522, 41.41978976119851552, 2.605981997472240241 ) ) ;
#32403 = CARTESIAN_POINT ( 'NONE',  ( 185.0420741367827020, 264.2165883964872251, -12.05581981974006744 ) ) ;
#32404 = CARTESIAN_POINT ( 'NONE',  ( 83.54394669835052412, 52.38488257041225182, 14.79586828322707071 ) ) ;
#32405 = CARTESIAN_POINT ( 'NONE',  ( 110.8733765985977300, 241.4865022471902876, -10.00000000000009592 ) ) ;
#32406 = CARTESIAN_POINT ( 'NONE',  ( 155.3654218642418527, 271.4162630973418686, 14.04413973620215828 ) ) ;
#32407 = VERTEX_POINT ( 'NONE', #18181 ) ;
#32408 = CARTESIAN_POINT ( 'NONE',  ( 184.2948240331882914, 264.1576318679792053, 13.78297524835661925 ) ) ;
#32409 = CARTESIAN_POINT ( 'NONE',  ( 163.1008115941903895, 248.1481028935802442, 11.25332017433677834 ) ) ;
#32410 = B_SPLINE_CURVE_WITH_KNOTS ( 'NONE', 3,
 ( #46393, #60594, #16506, #24106 ),
 .UNSPECIFIED., .F., .F.,
 ( 4, 4 ),
 ( 0.001717231910942013280, 0.007031907792270792809 ),
 .UNSPECIFIED. ) ;
#32411 = ADVANCED_FACE ( 'NONE', ( #55645 ), #24766, .T. ) ;
#32412 = CARTESIAN_POINT ( 'NONE',  ( 164.3138894970802824, 246.0469903322357368, -2.642126690130961020 ) ) ;
#32414 = CARTESIAN_POINT ( 'NONE',  ( 73.67502235716121106, 55.34260408957710808, 16.11561656089581973 ) ) ;
#32413 = CARTESIAN_POINT ( 'NONE',  ( 180.4856426815808845, 267.2495753203921254, -15.61375793168770620 ) ) ;
#32415 = CARTESIAN_POINT ( 'NONE',  ( 199.1239910296074243, 281.8565664318417703, -16.59351424064629654 ) ) ;
#32416 = EDGE_CURVE ( 'NONE', #66772, #53637, #45929, .T. ) ;
#32417 = CARTESIAN_POINT ( 'NONE',  ( 33.41142024434631708, 24.45404122711135386, -8.090169943749478065 ) ) ;
#32418 = CARTESIAN_POINT ( 'NONE',  ( 172.1882770616424239, 274.9807513487110668, 16.44417690625383344 ) ) ;
#32419 = CARTESIAN_POINT ( 'NONE',  ( 166.5511016027801361, 286.2022811075372033, -3.211568022117319288 ) ) ;
#32420 = DIRECTION ( 'NONE',  ( -0.000000000000000000, -0.000000000000000000, -1.000000000000000000 ) ) ;
#32421 = CARTESIAN_POINT ( 'NONE',  ( 47.03029105687465261, 114.3563895605556269, -10.00000000000000000 ) ) ;
#32422 = CARTESIAN_POINT ( 'NONE',  ( 194.8728601672216598, 266.1307473366540535, -7.448611987400203915 ) ) ;
#32423 =( BOUNDED_CURVE ( )  B_SPLINE_CURVE ( 2, ( #76877, #385, #62161, #7473, #29788, #91617, #22188, #47964, #19965, #87049, #97003, #9996, #8980 ),
 .UNSPECIFIED., .F., .T. ) 
 B_SPLINE_CURVE_WITH_KNOTS ( ( 3, 2, 2, 2, 2, 2, 3 ),
 ( 0.3375000000000000222, 0.3400000000000000244, 0.3449999999999999734, 0.3499999999999999778, 0.3549999999999999822, 0.3599999999999999867, 0.3624999999999999889 ),
 .UNSPECIFIED. ) 
 CURVE ( )  GEOMETRIC_REPRESENTATION_ITEM ( )  RATIONAL_B_SPLINE_CURVE ( ( 0.9755282581475768211, 0.9755282581475768211, 1.000000000000000000, 0.9510565162951535312, 1.000000000000000000, 0.9510565162951535312, 1.000000000000000000, 0.9510565162951535312, 1.000000000000000000, 0.9510565162951535312, 1.000000000000000000, 0.9755282581475768211, 0.9755282581475768211 ) ) 
 REPRESENTATION_ITEM ( '' )  );
#32424 = CARTESIAN_POINT ( 'NONE',  ( -4.208943576872074210, 174.5024278399160949, 9.188101187500095079 ) ) ;
#32425 = CARTESIAN_POINT ( 'NONE',  ( 82.44703276532530367, 48.69185277918708721, 13.19452699896754133 ) ) ;
#32426 = ORIENTED_EDGE ( 'NONE', *, *, #72641, .T. ) ;
#32427 = EDGE_CURVE ( 'NONE', #42896, #15150, #88373, .T. ) ;
#32428 = FACE_OUTER_BOUND ( 'NONE', #65288, .T. ) ;
#32429 = DIRECTION ( 'NONE',  ( 0.000000000000000000, 0.000000000000000000, -1.000000000000000000 ) ) ;
#32430 = DIRECTION ( 'NONE',  ( -0.000000000000000000, -0.000000000000000000, 1.000000000000000000 ) ) ;
#32431 = CARTESIAN_POINT ( 'NONE',  ( 28.72751893051112049, 178.2048013555409796, 4.594050593750051981 ) ) ;
#32432 = CARTESIAN_POINT ( 'NONE',  ( 171.4603946439460458, 289.8468835499439251, 4.041829335023700231 ) ) ;
#32433 = CARTESIAN_POINT ( 'NONE',  ( 26.95805898326085170, 39.65659080271453263, -1.878358725466461243E-16 ) ) ;
#32434 = CARTESIAN_POINT ( 'NONE',  ( 84.45526090851787160, 42.21020478296429701, -2.202011278587945320 ) ) ;
#32435 = CARTESIAN_POINT ( 'NONE',  ( 147.2999496562918296, 275.5159985734018164, -0.1418322875769767455 ) ) ;
#32436 = CARTESIAN_POINT ( 'NONE',  ( 73.06766668685415311, 65.73470164174882768, 13.24181784610626522 ) ) ;
#32437 = DIRECTION ( 'NONE',  ( -0.000000000000000000, -1.000000000000000000, -0.000000000000000000 ) ) ;
#32438 = CARTESIAN_POINT ( 'NONE',  ( 186.8364736135580699, 295.8946893679862455, -7.705750633037059316 ) ) ;
#32439 = EDGE_CURVE ( 'NONE', #20045, #44171, #68904, .T. ) ;
#32440 = CARTESIAN_POINT ( 'NONE',  ( 190.7840340658656544, 261.9460261807228676, -1.050979231100866773 ) ) ;
#32441 = ADVANCED_FACE ( 'NONE', ( #86630 ), #52061, .T. ) ;
#32442 = VECTOR ( 'NONE', #22312, 1000.000000000000114 ) ;
#32443 = CARTESIAN_POINT ( 'NONE',  ( 71.90223342829808928, 198.9865022471901739, 1.119607411625061291E-15 ) ) ;
#32444 = CARTESIAN_POINT ( 'NONE',  ( 164.4528277499967714, 246.1922880518520458, 1.577904702918717650 ) ) ;
#32445 = DIRECTION ( 'NONE',  ( 0.000000000000000000, 0.000000000000000000, 1.000000000000000000 ) ) ;
#32446 = CARTESIAN_POINT ( 'NONE',  ( 172.8673893914040036, 290.0046394668156040, 5.992580976346847166 ) ) ;
#32447 = CARTESIAN_POINT ( 'NONE',  ( 23.55782238408397689, 196.6589784336661637, -6.496448406907675876E-16 ) ) ;
#32448 = CARTESIAN_POINT ( 'NONE',  ( 67.53003662305086152, 66.80518130314699476, -8.448892015563799873 ) ) ;
#32449 = CARTESIAN_POINT ( 'NONE',  ( -4.824821883096095831, 80.30437515058552833, 13.53724619112298022 ) ) ;
#32450 = CARTESIAN_POINT ( 'NONE',  ( 199.0756812798354645, 285.8378008023734083, -18.45377816087746936 ) ) ;
#32451 = DIRECTION ( 'NONE',  ( -0.000000000000000000, 0.000000000000000000, -1.000000000000000000 ) ) ;
#32452 = ORIENTED_EDGE ( 'NONE', *, *, #16685, .T. ) ;
#32453 = PLANE ( 'NONE',  #32974 ) ;
#32454 = CARTESIAN_POINT ( 'NONE',  ( 29.55951135474875358, 176.3262482093457777, 3.021315404115420679E-15 ) ) ;
#32455 = CARTESIAN_POINT ( 'NONE',  ( 202.6802583809553369, 277.9056299575880757, -15.43640205419024269 ) ) ;
#32456 = CARTESIAN_POINT ( 'NONE',  ( 207.0300480714610671, 270.6212163841511256, -1.302876346950213149 ) ) ;
#32457 = CARTESIAN_POINT ( 'NONE',  ( 29.59504171901726366, 22.80170272979927759, 7.433330006724137462 ) ) ;
#32458 = CARTESIAN_POINT ( 'NONE',  ( 162.8789161433191452, 248.5324370884573568, 9.731756914259689140 ) ) ;
#32459 = CARTESIAN_POINT ( 'NONE',  ( 196.8104339078508076, 289.7613243423628546, -16.40335862274955403 ) ) ;
#32460 = CARTESIAN_POINT ( 'NONE',  ( 185.5175662163113088, 267.6491969837045986, -14.61920004980039955 ) ) ;
#32461 = ORIENTED_EDGE ( 'NONE', *, *, #19961, .T. ) ;
#32462 = CARTESIAN_POINT ( 'NONE',  ( 34.89708068152319242, 43.08080186712595605, -3.090169943749475845 ) ) ;
#32463 = CARTESIAN_POINT ( 'NONE',  ( 11.06209807803029221, 12.10170272979924988, -7.433330006724141015 ) ) ;
#32464 = CARTESIAN_POINT ( 'NONE',  ( 80.07551378063752168, 57.23092041213119074, -16.24140625160306683 ) ) ;
#32465 = CARTESIAN_POINT ( 'NONE',  ( 71.51903464973995028, 72.36264346112822921, -1.271393898589449512 ) ) ;
#32466 = ADVANCED_FACE ( 'NONE', ( #4982 ), #6747, .T. ) ;
#32467 = VERTEX_POINT ( 'NONE', #76848 ) ;
#32468 = CARTESIAN_POINT ( 'NONE',  ( 25.04665064082957926, 175.2677522451417929, -5.000000000000041744 ) ) ;
#32469 = CARTESIAN_POINT ( 'NONE',  ( 178.7933174507511467, 282.3263610565340969, 15.41595973002548803 ) ) ;
#32470 = CARTESIAN_POINT ( 'NONE',  ( 151.3589047706063582, 268.4856820897672378, 14.56544807350869419 ) ) ;
#32471 = CARTESIAN_POINT ( 'NONE',  ( 180.5860009740894156, 257.6394960767527778, -7.420540326864959901 ) ) ;
#32472 = CARTESIAN_POINT ( 'NONE',  ( 149.4491471355718772, 271.7934793437897270, 11.43912701239353780 ) ) ;
#32473 = ORIENTED_EDGE ( 'NONE', *, *, #72364, .T. ) ;
#32474 = ORIENTED_EDGE ( 'NONE', *, *, #13923, .T. ) ;
#32475 = EDGE_CURVE ( 'NONE', #75378, #71488, #14568, .T. ) ;
#32477 = DIRECTION ( 'NONE',  ( 0.8660254037844382635, 0.5000000000000005551, 0.000000000000000000 ) ) ;
#32476 = CARTESIAN_POINT ( 'NONE',  ( 161.8882824960653579, 250.2482648971885340, -13.83574485983625557 ) ) ;
#32478 = ORIENTED_EDGE ( 'NONE', *, *, #73533, .F. ) ;
#32479 = CARTESIAN_POINT ( 'NONE',  ( 153.0790963368640689, 265.5062228982576471, -17.74594954892339160 ) ) ;
#32480 = CARTESIAN_POINT ( 'NONE',  ( 71.65684213956077997, 72.06054752937143348, -3.528960205221522095 ) ) ;
#32481 = DIRECTION ( 'NONE',  ( 0.8660254037844395958, 0.4999999999999985567, 0.000000000000000000 ) ) ;
#32482 = CARTESIAN_POINT ( 'NONE',  ( 76.77756057274272905, 63.67496528870245243, 15.32214893988671101 ) ) ;
#32483 = B_SPLINE_CURVE_WITH_KNOTS ( 'NONE', 3,
 ( #68269, #61662, #31263, #14081 ),
 .UNSPECIFIED., .F., .F.,
 ( 4, 4 ),
 ( 0.009073585509988487535, 0.01733964532496718933 ),
 .UNSPECIFIED. ) ;
#32484 = CARTESIAN_POINT ( 'NONE',  ( 157.1002372043759010, 258.5414026113353430, -17.73553732786789539 ) ) ;
#32485 = CARTESIAN_POINT ( 'NONE',  ( 98.68587325814904432, 227.7833772461660544, -9.188101187500095079 ) ) ;
#32486 = EDGE_CURVE ( 'NONE', #35100, #99896, #99080, .T. ) ;
#32487 = CARTESIAN_POINT ( 'NONE',  ( 180.5853021615070872, 287.4186537074930925, -13.97997887675522399 ) ) ;
#32488 = ADVANCED_FACE ( 'NONE', ( #7964 ), #7445, .F. ) ;
#32489 = VERTEX_POINT ( 'NONE', #93074 ) ;
#32490 = CARTESIAN_POINT ( 'NONE',  ( 208.3057440179679531, 269.8508631828800617, 2.969924427282375046 ) ) ;
#32491 = B_SPLINE_CURVE_WITH_KNOTS ( 'NONE', 3,
 ( #69140, #30657, #5862, #92483, #23030, #84886, #15426, #46323, #36747, #250, #62023, #54419, #85395, #93990, #41232, #55421, #25557, #17971, #47339, #17449, #47825, #70129, #85917, #39222, #78764, #63046, #39714, #48866, #71677, #8353, #16443, #32138, #24541, #93486, #742, #46846, #78263, #8844, #31626, #55919, #86408, #62525, #79798, #70642, #16939, #24042, #87438, #40228 ),
 .UNSPECIFIED., .F., .F.,
 ( 4, 2, 2, 2, 2, 2, 2, 2, 2, 2, 2, 2, 2, 2, 2, 2, 2, 2, 2, 2, 2, 2, 2, 4 ),
 ( 0.0005932163644935171086, 0.001587166566766770115, 0.001835654117335065207, 0.002084141667903359647, 0.002208385443187456994, 0.002332629218471554342, 0.002456872993755651255, 0.002581116769039748168, 0.002829604319607905566, 0.003078091870176063397, 0.003575066971312377325, 0.004569017173584972655, 0.005562967375857569285, 0.006059942476993858060, 0.006556917578130146834, 0.006681161353414236809, 0.006743283241056252306, 0.006805405128698267803, 0.006929648903982187774, 0.007053892679266107746, 0.007302380229833928607, 0.007550867780401747734, 0.008047842881537415477, 0.008544817982673081486 ),
 .UNSPECIFIED. ) ;
#32492 = VERTEX_POINT ( 'NONE', #23629 ) ;
#32493 = EDGE_CURVE ( 'NONE', #51511, #87203, #54522, .T. ) ;
#32494 = CARTESIAN_POINT ( 'NONE',  ( 30.11465696128792757, 23.10170272979928541, -7.433330006724141015 ) ) ;
#32495 = CARTESIAN_POINT ( 'NONE',  ( 159.4230536986738400, 254.5181664265525683, 16.83068086755798376 ) ) ;
#32496 = CARTESIAN_POINT ( 'NONE',  ( 66.90449132437942126, 69.67812219415840502, -1.620417471643094798 ) ) ;
#32497 = EDGE_CURVE ( 'NONE', #78822, #1997, #71773, .T. ) ;
#32498 = CARTESIAN_POINT ( 'NONE',  ( 54.51857766514267212, 202.2833772461660828, -9.188101187500095079 ) ) ;
#32499 = CARTESIAN_POINT ( 'NONE',  ( 74.10605571268695257, 68.62492193873490010, 10.95106078344675637 ) ) ;
#32500 = DIRECTION ( 'NONE',  ( -0.5000000000000001110, 0.8660254037844385966, 0.000000000000000000 ) ) ;
#32501 = CARTESIAN_POINT ( 'NONE',  ( -22.42236680055709641, 157.8615022471902591, 0.000000000000000000 ) ) ;
#32502 = CARTESIAN_POINT ( 'NONE',  ( 175.4753921014799403, 272.5933248971207945, 16.60100264507961043 ) ) ;
#32503 = EDGE_LOOP ( 'NONE', ( #67993, #74902, #31505, #45077 ) ) ;
#32504 = CARTESIAN_POINT ( 'NONE',  ( 187.8824611759788183, 271.4673514592827246, -16.49468309722856674 ) ) ;
#32505 = CARTESIAN_POINT ( 'NONE',  ( 86.15569456219643030, 43.34566298074329893, -3.128694683549113176 ) ) ;
#32506 = CARTESIAN_POINT ( 'NONE',  ( 146.8195026170398023, 276.3481572557323034, 4.765869558735466249 ) ) ;
#32507 = DIRECTION ( 'NONE',  ( 0.4458072818673421978, 0.8951289669282590511, 0.000000000000000000 ) ) ;
#32508 = EDGE_LOOP ( 'NONE', ( #13643, #24887, #30153, #74157 ) ) ;
#32509 = CARTESIAN_POINT ( 'NONE',  ( 172.9131096068250599, 260.2067844819827087, -13.87985791031445260 ) ) ;
#32510 = CARTESIAN_POINT ( 'NONE',  ( 170.7736899422801571, 275.3227619045933920, -16.19396132888206452 ) ) ;
#32511 = CARTESIAN_POINT ( 'NONE',  ( 43.53831125515428369, 65.97156238185917232, -10.00000000000000000 ) ) ;
#32512 = CARTESIAN_POINT ( 'NONE',  ( 193.2140586456748679, 295.9904290195353269, -12.67640480829088823 ) ) ;
#32513 = CARTESIAN_POINT ( 'NONE',  ( 190.4163244163388242, 300.8362468508201459, 4.691083071570470331 ) ) ;
#32514 = CARTESIAN_POINT ( 'NONE',  ( 31.36687970962302785, 200.4637435831424739, 2.679491924311251605 ) ) ;
#32515 = CARTESIAN_POINT ( 'NONE',  ( 205.8379285891498682, 274.1252448892948905, 10.44730901608240181 ) ) ;
#32516 = CARTESIAN_POINT ( 'NONE',  ( 67.48492722593299220, 67.03479993418675065, 8.993132823606122983 ) ) ;
#32517 = CARTESIAN_POINT ( 'NONE',  ( 74.81986938884084282, 64.47242206951092669, -14.05694895914753673 ) ) ;
#32518 = DIRECTION ( 'NONE',  ( 0.4999999999999998890, -0.8660254037844385966, 0.000000000000000000 ) ) ;
#32519 = CARTESIAN_POINT ( 'NONE',  ( 110.7287787077026451, 243.9244531367911293, -4.594050593750046652 ) ) ;
#32520 = ORIENTED_EDGE ( 'NONE', *, *, #90858, .T. ) ;
#32521 = CARTESIAN_POINT ( 'NONE',  ( 191.8210230231139803, 298.4032374945642232, -8.800268167321144475 ) ) ;
#32522 = CARTESIAN_POINT ( 'NONE',  ( 69.87353541051622585, 64.19244626969324941, 12.43200581978026342 ) ) ;
#32523 = CARTESIAN_POINT ( 'NONE',  ( 203.4357368910538355, 278.2859629599173559, -16.45855118664066197 ) ) ;
#32524 = CARTESIAN_POINT ( 'NONE',  ( 183.2596571801339280, 284.8004292275762168, -14.94647318252461687 ) ) ;
#32525 = CARTESIAN_POINT ( 'NONE',  ( 83.74768966023471251, 52.21580090503303495, -15.05827679895701898 ) ) ;
#32526 = AXIS2_PLACEMENT_3D ( 'NONE', #85916, #30656, #61539 ) ;
#32527 = CARTESIAN_POINT ( 'NONE',  ( 177.9929206047679031, 255.3858926944306234, 4.850379692699073431 ) ) ;
#32528 = ORIENTED_EDGE ( 'NONE', *, *, #79413, .F. ) ;
#32529 = CARTESIAN_POINT ( 'NONE',  ( 80.61477260300527803, 57.23824740812084144, -16.23096960288277302 ) ) ;
#32530 = CARTESIAN_POINT ( 'NONE',  ( 154.6560229494072871, 273.6100238714292914, -13.40105020477086839 ) ) ;
#32531 = CARTESIAN_POINT ( 'NONE',  ( 185.9207523352618523, 262.0077436853858330, 9.914687552586279651 ) ) ;
#32532 = CARTESIAN_POINT ( 'NONE',  ( 164.9402323277223275, 244.9621327266073081, -1.073314903116530106 ) ) ;
#32533 = CARTESIAN_POINT ( 'NONE',  ( 132.2983106946500982, 253.3149278399160949, -9.188101187500095079 ) ) ;
#32534 = CARTESIAN_POINT ( 'NONE',  ( 189.6995965464004712, 294.6853058160613159, -12.59856403867662955 ) ) ;
#32535 = CARTESIAN_POINT ( 'NONE',  ( 185.7715223625128260, 296.9187202208149756, 4.298953271262141662 ) ) ;
#32536 = B_SPLINE_CURVE_WITH_KNOTS ( 'NONE', 3,
 ( #67585, #68084, #59972, #12414, #59467, #35697, #67083, #43281, #74226, #82841, #21984, #99006, #66597, #97521, #14396, #52880, #83830, #89934, #45279, #20513, #12921, #43780, #5303, #28587, #90449, #44281, #22972, #55719, #71966, #95314, #46256, #14876, #9675, #25871, #91933, #18266, #41029, #9153, #49160, #24843, #84330, #15361, #71470, #40029 ),
 .UNSPECIFIED., .F., .F.,
 ( 4, 2, 2, 2, 2, 2, 2, 2, 2, 2, 2, 2, 2, 2, 2, 2, 2, 2, 2, 2, 2, 4 ),
 ( 0.0003194575834195127750, 0.001336248915430739625, 0.001844644581436353159, 0.002098842414439147999, 0.002225941330940528831, 0.002353040247441909663, 0.002607238080444787987, 0.002861435913447666311, 0.003369831579453307167, 0.004386622911464483493, 0.005403414243475661120, 0.005911809909481204398, 0.006166007742483933969, 0.006420205575486663541, 0.006483755033737345283, 0.006547304491988027025, 0.006610853950238708768, 0.006674403408489390510, 0.006928601241492172991, 0.007436996907497737952, 0.007945392573503302913, 0.008453788239508869609 ),
 .UNSPECIFIED. ) ;
#32537 = CARTESIAN_POINT ( 'NONE',  ( 188.4211857319924945, 281.8444091920245569, -16.71250961025338810 ) ) ;
#32538 = CARTESIAN_POINT ( 'NONE',  ( 43.63646518856938172, 66.22046553916848666, -10.00000000000000000 ) ) ;
#32539 = CARTESIAN_POINT ( 'NONE',  ( 40.68897417663616523, 203.4869531367911293, 4.594050593750046652 ) ) ;
#32540 = CARTESIAN_POINT ( 'NONE',  ( 85.62748912975605720, 48.34643938460052937, -11.70855452506934391 ) ) ;
#32541 = CARTESIAN_POINT ( 'NONE',  ( 87.95999259833929784, 44.52227941376569476, -3.981728561935235611 ) ) ;
#32542 = CARTESIAN_POINT ( 'NONE',  ( 171.0832173816872626, 259.7879900724919935, 15.08573027344413653 ) ) ;
#32543 = CARTESIAN_POINT ( 'NONE',  ( 151.5918080220145896, 278.2509154019998050, -1.647039589299454043 ) ) ;
#32544 = LINE ( 'NONE', #83918, #53170 ) ;
#32545 = CARTESIAN_POINT ( 'NONE',  ( -19.65312891409030271, 93.06504152958497400, -10.00000000000000888 ) ) ;
#32546 = CARTESIAN_POINT ( 'NONE',  ( 156.6119464822673990, 270.4807277697740346, -14.77393801743134105 ) ) ;
#32547 = CARTESIAN_POINT ( 'NONE',  ( 122.4745085665788906, 241.5177522451418497, -10.00000000000009592 ) ) ;
#32548 = CARTESIAN_POINT ( 'NONE',  ( 80.44948470589578449, 51.95659882761868431, -15.19047218006325650 ) ) ;
#32549 = VERTEX_POINT ( 'NONE', #32247 ) ;
#32550 = EDGE_CURVE ( 'NONE', #28252, #70323, #55526, .T. ) ;
#32551 = CARTESIAN_POINT ( 'NONE',  ( 163.3706531435203146, 247.6807236201477735, 10.06957846017757241 ) ) ;
#32552 = CYLINDRICAL_SURFACE ( 'NONE', #44735, 10.00000000000010658 ) ;
#32553 = CARTESIAN_POINT ( 'NONE',  ( 28.37560933628243731, 181.0643266524159856, -9.188101187500093303 ) ) ;
#32554 = CARTESIAN_POINT ( 'NONE',  ( 8.494131180097229006, 27.83705186507752671, 3.090169943749475401 ) ) ;
#32555 = CARTESIAN_POINT ( 'NONE',  ( 79.17566594283800896, 50.17566997415585206, -15.28976903731980741 ) ) ;
#32556 = CARTESIAN_POINT ( 'NONE',  ( 146.8516045228164160, 276.2925551239072774, 3.995954059407343273 ) ) ;
#32557 = CARTESIAN_POINT ( 'NONE',  ( 72.21281551018738298, 72.08933296411181857, 3.049783143056646662 ) ) ;
#32559 = CARTESIAN_POINT ( 'NONE',  ( 51.46042545625488174, 210.5177522451419065, 5.000000000000046185 ) ) ;
#32558 = DIRECTION ( 'NONE',  ( 0.000000000000000000, 0.000000000000000000, 1.000000000000000000 ) ) ;
#32560 = CARTESIAN_POINT ( 'NONE',  ( 172.1508111218572026, 287.0958522653913860, 7.470856674359275473 ) ) ;
#32561 = CARTESIAN_POINT ( 'NONE',  ( 184.6893784852484828, 257.7963074246405313, 1.363638931471332638 ) ) ;
#32562 = EDGE_CURVE ( 'NONE', #26502, #35860, #95539, .T. ) ;
#32563 = CARTESIAN_POINT ( 'NONE',  ( 205.2660270307054304, 275.1158074454486382, -13.97598661256119179 ) ) ;
#32564 = CARTESIAN_POINT ( 'NONE',  ( 162.2294822266495089, 251.8890613771950200, -13.02408023403573978 ) ) ;
#32565 = EDGE_LOOP ( 'NONE', ( #21147, #71839, #26406, #4943 ) ) ;
#32566 = EDGE_CURVE ( 'NONE', #64025, #14234, #54355, .T. ) ;
#32567 = CARTESIAN_POINT ( 'NONE',  ( 27.73493783529170997, 173.4865022471901739, 1.119607411625061291E-15 ) ) ;
#32568 = DIRECTION ( 'NONE',  ( -0.5104483989331149996, -0.8599083858334093389, 0.000000000000000000 ) ) ;
#32569 = B_SPLINE_CURVE_WITH_KNOTS ( 'NONE', 3,
 ( #9535, #40889, #94654, #2436, #25209, #56612, #40396, #69807, #70822, #77930, #86574, #55591, #48526, #46496, #77432, #70307, #417, #31306, #1431, #47507, #32312, #16117, #24708, #62194, #93145, #47015, #8521, #39390, #31796, #86087, #66702, #28202, #72344, #57600, #18122, #49024, #65213, #95675, #89090, #26222, #96155, #19639, #81948, #35808, #89563, #80463 ),
 .UNSPECIFIED., .F., .F.,
 ( 4, 1, 1, 1, 2, 2, 1, 1, 1, 2, 2, 1, 1, 2, 2, 1, 1, 2, 2, 1, 1, 2, 2, 1, 2, 2, 1, 2, 2, 4 ),
 ( 0.000000000000000000, 0.06249999999998910594, 0.09374999999998365197, 0.1093749999999809319, 0.1171874999999812095, 0.1249999999999814870, 0.1874999999999751310, 0.2187499999999721612, 0.2343749999999688860, 0.2421874999999692468, 0.2499999999999695799, 0.3124999999999819034, 0.3437499999999878986, 0.3593749999999907296, 0.3749999999999935052, 0.4374999999999977796, 0.4687499999999999445, 0.4843750000000010547, 0.5000000000000021094, 0.5625000000000041078, 0.5937500000000052180, 0.6093750000000056621, 0.6250000000000063283, 0.6875000000000054401, 0.7187500000000034417, 0.7500000000000013323, 0.8124999999999976685, 0.8437499999999973355, 0.8749999999999970024, 1.000000000000000000 ),
 .UNSPECIFIED. ) ;
#32570 = CARTESIAN_POINT ( 'NONE',  ( 162.8037981520209314, 248.6625452659484381, 9.809699077002424161 ) ) ;
#32571 = CARTESIAN_POINT ( 'NONE',  ( 146.7502831681854332, 255.5333772461660260, 9.188101187500095079 ) ) ;
#32572 = CARTESIAN_POINT ( 'NONE',  ( 42.70206918026080700, 25.44966523072497822, -2.296566073217252530E-15 ) ) ;
#32574 = CARTESIAN_POINT ( 'NONE',  ( 200.1233510698300222, 282.0231834965481994, 17.42297826929840809 ) ) ;
#32573 = CARTESIAN_POINT ( 'NONE',  ( 163.8921714668630045, 247.1588185633375758, 6.247182185919442077 ) ) ;
#32575 = CARTESIAN_POINT ( 'NONE',  ( -19.65312891409030271, 93.06504152958497400, -10.00000000000000888 ) ) ;
#32576 = CARTESIAN_POINT ( 'NONE',  ( 68.35453417343931903, 65.67399229982113695, 10.37910612949749911 ) ) ;
#32577 = CARTESIAN_POINT ( 'NONE',  ( 183.1886578041060716, 257.7166335271973594, -2.049690715180576106 ) ) ;
#32578 = CARTESIAN_POINT ( 'NONE',  ( 66.11564498168849013, 69.06652558778995399, 2.579580841645931599 ) ) ;
#32579 = ORIENTED_EDGE ( 'NONE', *, *, #56548, .F. ) ;
#32580 = CARTESIAN_POINT ( 'NONE',  ( 179.5196496019146650, 266.1175816663657656, 16.29367087753972498 ) ) ;
#32581 = CARTESIAN_POINT ( 'NONE',  ( 148.5274394637608282, 249.8927522451417929, -10.00000000000009237 ) ) ;
#32582 = CARTESIAN_POINT ( 'NONE',  ( 153.1991487056075130, 277.8144349384043608, -5.978376906038552541 ) ) ;
#32583 = CARTESIAN_POINT ( 'NONE',  ( 4.462289544239298245, 25.68290643055184930, 3.479690158560446702E-15 ) ) ;
#32584 = DIRECTION ( 'NONE',  ( -0.09248003802712849442, 0.9957145386939476595, 0.000000000000000000 ) ) ;
#32585 = CARTESIAN_POINT ( 'NONE',  ( 206.0946696452135427, 273.6805563358039421, -10.19627505985792837 ) ) ;
#32586 = CARTESIAN_POINT ( 'NONE',  ( 25.55253460671674759, 33.49103043416550918, -8.090169943749479842 ) ) ;
#32587 = CARTESIAN_POINT ( 'NONE',  ( -13.90914858307771063, 104.6155556099271280, 43.90259622397829986 ) ) ;
#32588 = CARTESIAN_POINT ( 'NONE',  ( 66.30954113569532637, 68.28728378170325186, 3.992301261007319191 ) ) ;
#32589 = CARTESIAN_POINT ( 'NONE',  ( 162.6425574510925003, 248.9418223522047526, -10.70838742014210077 ) ) ;
#32590 = AXIS2_PLACEMENT_3D ( 'NONE', #15132, #83596, #60233 ) ;
#32591 = CARTESIAN_POINT ( 'NONE',  ( -24.63924516542739696, 141.7012482093459198, 1.426039447152360146E-13 ) ) ;
#32592 = VERTEX_POINT ( 'NONE', #41336 ) ;
#32593 = EDGE_CURVE ( 'NONE', #53210, #80145, #95611, .T. ) ;
#32594 = DIRECTION ( 'NONE',  ( 0.5000000000000048850, -0.8660254037844358210, 0.000000000000000000 ) ) ;
#32595 = CARTESIAN_POINT ( 'NONE',  ( 86.32568876638555366, 47.65221178568590688, 10.70297444941600418 ) ) ;
#32596 = ORIENTED_EDGE ( 'NONE', *, *, #36819, .T. ) ;
#32597 = CARTESIAN_POINT ( 'NONE',  ( 165.3929592122126451, 286.2279243276498732, 4.432946431554212197 ) ) ;
#32598 = PLANE ( 'NONE',  #61293 ) ;
#32599 = EDGE_LOOP ( 'NONE', ( #79993, #37667, #2214, #61738 ) ) ;
#32600 = LINE ( 'NONE', #39170, #89612 ) ;
#32601 = CARTESIAN_POINT ( 'NONE',  ( 85.35443477132466228, 48.30880629543902671, -11.80360700664790663 ) ) ;
#32602 = EDGE_CURVE ( 'NONE', #44538, #53287, #46000, .T. ) ;
#32603 = CARTESIAN_POINT ( 'NONE',  ( 2.117331368781439682, 160.4824982072973683, 3.021315404115420679E-15 ) ) ;
#32604 = VERTEX_POINT ( 'NONE', #97098 ) ;
#32605 = CARTESIAN_POINT ( 'NONE',  ( 173.9797063438981013, 267.3139811165434594, 17.17281660156877621 ) ) ;
#32606 = CARTESIAN_POINT ( 'NONE',  ( -32.91998363024201524, 94.57991847588093037, 43.90692951987065129 ) ) ;
#32607 = CARTESIAN_POINT ( 'NONE',  ( 151.0036289208911171, 269.1010379121764799, 14.24595189915657478 ) ) ;
#32608 = LINE ( 'NONE', #70602, #76875 ) ;
#32609 = ORIENTED_EDGE ( 'NONE', *, *, #54968, .F. ) ;
#32610 = EDGE_CURVE ( 'NONE', #76706, #66378, #42336, .T. ) ;
#32611 = DIRECTION ( 'NONE',  ( -0.09573633691163400961, -0.9954067278227238802, 0.000000000000000000 ) ) ;
#32612 = CARTESIAN_POINT ( 'NONE',  ( 202.6551236945213361, 279.6380246773706517, 15.55476940527561425 ) ) ;
#32613 = VERTEX_POINT ( 'NONE', #42825 ) ;
#32614 = ORIENTED_EDGE ( 'NONE', *, *, #63678, .F. ) ;
#32615 = CARTESIAN_POINT ( 'NONE',  ( 73.11277796669548934, 60.16616684050868002, 15.29999328649868851 ) ) ;
#32616 = VERTEX_POINT ( 'NONE', #58051 ) ;
#32617 = CARTESIAN_POINT ( 'NONE',  ( 160.8275201602635036, 271.0864152119986556, 16.51521213740326743 ) ) ;
#32618 = ORIENTED_EDGE ( 'NONE', *, *, #90867, .F. ) ;
#32619 = CARTESIAN_POINT ( 'NONE',  ( 82.37905398250840960, 46.52165906567139331, 11.60550393209069320 ) ) ;
#32620 = CARTESIAN_POINT ( 'NONE',  ( 69.74653821704758627, 65.80766725781488447, 11.05544688728975622 ) ) ;
#32621 = LINE ( 'NONE', #16415, #69522 ) ;
#32622 = CARTESIAN_POINT ( 'NONE',  ( 82.49110201129202835, 53.29505896912813512, -15.32863176240265268 ) ) ;
#32623 = LINE ( 'NONE', #70616, #57984 ) ;
#32624 = ORIENTED_EDGE ( 'NONE', *, *, #68098, .F. ) ;
#32625 = CARTESIAN_POINT ( 'NONE',  ( 188.9516232634142909, 259.5449388965931234, 2.625812016075142807 ) ) ;
#32626 = CARTESIAN_POINT ( 'NONE',  ( 23.10466909204031083, 21.84335787977762777, 9.188101187500006262 ) ) ;
#32627 = CARTESIAN_POINT ( 'NONE',  ( 164.5348324038273518, 245.6643059921780718, 1.473102934610569958 ) ) ;
#32628 = CARTESIAN_POINT ( 'NONE',  ( 205.7668501412109663, 274.2483563724483133, 11.09689540819876896 ) ) ;
#32630 = ORIENTED_EDGE ( 'NONE', *, *, #99553, .T. ) ;
#32629 = CARTESIAN_POINT ( 'NONE',  ( 198.1679321590325458, 277.6257778925182720, -16.56331389466651061 ) ) ;
#32631 = CARTESIAN_POINT ( 'NONE',  ( 147.3775965199690461, 275.3815102604642675, -3.878554353302192226 ) ) ;
#32632 = CARTESIAN_POINT ( 'NONE',  ( 48.83428215874786815, 87.09189275153327969, -10.00000000000000000 ) ) ;
#32633 = CARTESIAN_POINT ( 'NONE',  ( 159.8188415394622268, 253.8326417772889840, -15.43862849427313222 ) ) ;
#32634 = FACE_OUTER_BOUND ( 'NONE', #55753, .T. ) ;
#32635 = EDGE_CURVE ( 'NONE', #93745, #14058, #99921, .T. ) ;
#32636 = CARTESIAN_POINT ( 'NONE',  ( 200.8551880497955437, 282.7556046643899776, 18.00894873733387058 ) ) ;
#32637 = CARTESIAN_POINT ( 'NONE',  ( -27.42236680055714260, 166.5217562850347406, 1.224646799147364892E-15 ) ) ;
#32638 = ORIENTED_EDGE ( 'NONE', *, *, #76713, .F. ) ;
#32639 = CARTESIAN_POINT ( 'NONE',  ( 155.0112353102835243, 262.1596600290110359, -17.54170487059483818 ) ) ;
#32640 = CARTESIAN_POINT ( 'NONE',  ( 138.9289912384832917, 241.0177522451417929, 5.000000000000051514 ) ) ;
#32642 = EDGE_CURVE ( 'NONE', #6303, #50548, #89509, .T. ) ;
#32641 = CARTESIAN_POINT ( 'NONE',  ( -3.297639133650708043, 162.2365022471902023, -10.00000000000009237 ) ) ;
#32643 = CARTESIAN_POINT ( 'NONE',  ( 22.44857442947627035, 173.7677522451417929, -5.000000000000041744 ) ) ;
#32644 = CARTESIAN_POINT ( 'NONE',  ( 80.71549903385694336, 229.6589784336661353, -6.496448406907676862E-16 ) ) ;
#32645 = CARTESIAN_POINT ( 'NONE',  ( 82.41933087065974917, 40.38430946149325962, -0.8419157720437354664 ) ) ;
#32646 = LINE ( 'NONE', #16442, #45452 ) ;
#32647 = CARTESIAN_POINT ( 'NONE',  ( 163.1177074157340030, 248.1188384722309195, 11.53923137679231026 ) ) ;
#32649 = CARTESIAN_POINT ( 'NONE',  ( 75.78086150065365700, 65.61082703666508564, 13.82051080074114502 ) ) ;
#32648 = CARTESIAN_POINT ( 'NONE',  ( 13.13906166239122619, 169.2048013555410080, 4.594050593750051981 ) ) ;
#32650 = CARTESIAN_POINT ( 'NONE',  ( 161.3227470381586102, 251.2278010437646856, 14.45097375514160731 ) ) ;
#32651 = ORIENTED_EDGE ( 'NONE', *, *, #56017, .F. ) ;
#32652 = VERTEX_POINT ( 'NONE', #3381 ) ;
#32653 = CARTESIAN_POINT ( 'NONE',  ( 165.9091197491159164, 246.2627970730538323, -2.747640711776688338 ) ) ;
#32654 = CARTESIAN_POINT ( 'NONE',  ( 200.9106067213441520, 267.7885642596323805, -3.100825223188956148 ) ) ;
#32655 = CARTESIAN_POINT ( 'NONE',  ( 88.02757723400505085, 43.99990312156534600, 0.5524629566968192185 ) ) ;
#32656 = CARTESIAN_POINT ( 'NONE',  ( 32.56068451518306262, 20.92755873383627829, 6.180339887498953466 ) ) ;
#32657 = CARTESIAN_POINT ( 'NONE',  ( 71.15274061880276690, 41.48415679381830046, 1.224646799147354045E-15 ) ) ;
#32658 = CARTESIAN_POINT ( 'NONE',  ( 112.1543725048143898, 228.8927522451417929, -10.00000000000009237 ) ) ;
#32659 = CARTESIAN_POINT ( 'NONE',  ( 74.38673974678103207, 68.41474614631960094, -11.27947015944677212 ) ) ;
#32660 = CARTESIAN_POINT ( 'NONE',  ( 35.81758128034870481, 200.6744531367911293, 4.594050593750047540 ) ) ;
#32661 = CARTESIAN_POINT ( 'NONE',  ( 79.60625107924917643, 216.7677522451418497, 10.00000000000009592 ) ) ;
#32662 = CARTESIAN_POINT ( 'NONE',  ( 195.9148236425762661, 275.2641294645287076, 15.61648565824300050 ) ) ;
#32663 = ORIENTED_EDGE ( 'NONE', *, *, #72268, .F. ) ;
#32664 = B_SPLINE_CURVE_WITH_KNOTS ( 'NONE', 3,
 ( #68807, #99735, #45993, #76911, #69318, #36411, #100240, #44001, #36963, #29378, #23253, #76959, #45062, #6580, #68362, #6069 ),
 .UNSPECIFIED., .F., .F.,
 ( 4, 1, 2, 2, 2, 1, 2, 2, 4 ),
 ( 0.000000000000000000, 0.1249999999999942268, 0.1874999999999933109, 0.2499999999999923950, 0.4999999999999982236, 0.6250000000000007772, 0.6875000000000017764, 0.7500000000000027756, 1.000000000000000000 ),
 .UNSPECIFIED. ) ;
#32665 = CARTESIAN_POINT ( 'NONE',  ( 82.90600853043393670, 44.75983668713269026, 9.542372462439493219 ) ) ;
#32666 = EDGE_CURVE ( 'NONE', #43772, #12458, #31403, .T. ) ;
#32667 = CARTESIAN_POINT ( 'NONE',  ( 46.60452734134891273, 70.48356709729733893, 177.5919119679930134 ) ) ;
#32668 = CARTESIAN_POINT ( 'NONE',  ( -12.00317221093202136, 170.0024278399160949, 9.188101187500095079 ) ) ;
#32669 = CARTESIAN_POINT ( 'NONE',  ( 194.3252252352508265, 294.0658320307167628, 14.07225870721148731 ) ) ;
#32670 = CARTESIAN_POINT ( 'NONE',  ( 151.1811967613751335, 268.7934813906678642, -15.79361349403328418 ) ) ;
#32671 = CARTESIAN_POINT ( 'NONE',  ( 74.14312167556930433, 66.30466486950707861, 1.224646799147354045E-15 ) ) ;
#32672 = CARTESIAN_POINT ( 'NONE',  ( 194.9636675848471441, 292.9600174435121289, -15.57898232594655319 ) ) ;
#32673 = CARTESIAN_POINT ( 'NONE',  ( 190.6479877716197393, 262.7614712451651826, 8.392489763586285179 ) ) ;
#32674 = CARTESIAN_POINT ( 'NONE',  ( 204.6780326111993986, 276.1342436545999703, 14.85609018352459287 ) ) ;
#32675 = ADVANCED_FACE ( 'NONE', ( #2252 ), #47321, .T. ) ;
#32676 = CARTESIAN_POINT ( 'NONE',  ( 191.8453338867844877, 298.3611298435110371, -9.039024722281077118 ) ) ;
#32677 = CARTESIAN_POINT ( 'NONE',  ( 148.3190727836317535, 273.7508255376806119, 8.080277324579027365 ) ) ;
#32678 = ORIENTED_EDGE ( 'NONE', *, *, #33382, .T. ) ;
#32679 = ADVANCED_FACE ( 'NONE', ( #63528 ), #63029, .T. ) ;
#32680 = CARTESIAN_POINT ( 'NONE',  ( 161.6725611998193983, 251.8560077465454299, -13.81138343693815251 ) ) ;
#32681 = CARTESIAN_POINT ( 'NONE',  ( 115.2218061334819623, 228.1423013555409796, -4.594050593750043987 ) ) ;
#32682 = CARTESIAN_POINT ( 'NONE',  ( 14.85095921958720666, 14.28920272979925699, -7.433330006724141015 ) ) ;
#32683 = CARTESIAN_POINT ( 'NONE',  ( 72.83042459652598666, 60.89494529775108589, -15.49726665856611163 ) ) ;
#32684 = FACE_OUTER_BOUND ( 'NONE', #54532, .T. ) ;
#32686 = CARTESIAN_POINT ( 'NONE',  ( 143.0969038086192597, 260.4263049900483225, -7.951529393128359935 ) ) ;
#32685 = CARTESIAN_POINT ( 'NONE',  ( 195.7291534503633272, 291.6341570319625021, 16.44925029361851543 ) ) ;
#32687 = CARTESIAN_POINT ( 'NONE',  ( 149.9821146867828929, 276.3814977895287370, -6.888571825090875400 ) ) ;
#32688 = CARTESIAN_POINT ( 'NONE',  ( 20.83817183295411013, 35.52903772873357724, -1.583844403245363575 ) ) ;
#32689 = CARTESIAN_POINT ( 'NONE',  ( 196.9976074755333286, 289.4371302133026802, -16.79549473444794216 ) ) ;
#32690 = CARTESIAN_POINT ( 'NONE',  ( 81.94814304414562400, 41.00889934599905473, -3.213059439476845913 ) ) ;
#32691 = CARTESIAN_POINT ( 'NONE',  ( 172.8847284319935795, 290.1773784869942006, -1.864525648362560295 ) ) ;
#32692 = CARTESIAN_POINT ( 'NONE',  ( 155.7716105177659927, 262.8426515368366267, -17.72795275872529430 ) ) ;
#32693 = EDGE_LOOP ( 'NONE', ( #78081, #53798, #95063, #95949 ) ) ;
#32694 = CARTESIAN_POINT ( 'NONE',  ( 189.4381674897702794, 265.0040801212285828, 12.03645615491573828 ) ) ;
#32695 = AXIS2_PLACEMENT_3D ( 'NONE', #12167, #73970, #80609 ) ;
#32696 = CARTESIAN_POINT ( 'NONE',  ( 175.6497225671480749, 278.5846401578337463, 15.45330369560194050 ) ) ;
#32697 = CARTESIAN_POINT ( 'NONE',  ( 198.8044191836357584, 269.5069306727704088, 9.250748962204042414 ) ) ;
#32698 = ORIENTED_EDGE ( 'NONE', *, *, #95424, .F. ) ;
#32699 = B_SPLINE_SURFACE_WITH_KNOTS ( 'NONE', 3, 1, ( 
 ( #78365, #31721 ),
 ( #1857, #32739 ),
 ( #24147, #61634 ),
 ( #23623, #63644 ),
 ( #347, #70236 ),
 ( #840, #93580 ),
 ( #63142, #94087 ),
 ( #92586, #25136 ),
 ( #76842, #23129 ),
 ( #54024, #55032 ),
 ( #84979, #62121 ),
 ( #93069, #54517 ),
 ( #85495, #19576 ),
 ( #80905, #27157 ),
 ( #49441, #79395 ),
 ( #72271, #80396 ),
 ( #33770, #64657 ),
 ( #88510, #25660 ),
 ( #95606, #2366 ),
 ( #58044, #89026 ),
 ( #19073, #57031 ),
 ( #48451, #96594 ),
 ( #26155, #33244 ),
 ( #9962, #57533 ),
 ( #64145, #88014 ),
 ( #42820, #18563 ),
 ( #34248, #10965 ),
 ( #48957, #73750 ),
 ( #71767, #41838 ),
 ( #72783, #95096 ),
 ( #11958, #56539 ) ),
 .UNSPECIFIED., .F., .F., .F.,
 ( 4, 3, 3, 3, 3, 3, 3, 3, 3, 3, 4 ),
 ( 2, 2 ),
 ( 0.000000000000000000, 0.1122669598086760978, 0.2243161639709538580, 0.3396355846219034635, 0.4553962076585165719, 0.5677860799922357371, 0.6749047109689572110, 0.7773884377078412733, 0.8775581155834328850, 0.9782364162377978900, 1.000000000000000000 ),
 ( 0.000000000000000000, 1.000000000000000000 ),
 .UNSPECIFIED. ) ;
#32700 = CARTESIAN_POINT ( 'NONE',  ( 79.47297740959983514, 51.20435970566347095, 15.10662661765129222 ) ) ;
#32701 = CARTESIAN_POINT ( 'NONE',  ( 83.61754957953866096, 52.24592005514148951, -14.70745080183156972 ) ) ;
#32702 = LINE ( 'NONE', #70703, #24217 ) ;
#32703 = CARTESIAN_POINT ( 'NONE',  ( 192.7507137768506880, 296.7929658737652971, 11.30364540927242345 ) ) ;
#32704 = ORIENTED_EDGE ( 'NONE', *, *, #19726, .F. ) ;
#32705 = ADVANCED_FACE ( 'NONE', ( #56427 ), #10347, .T. ) ;
#32706 = CARTESIAN_POINT ( 'NONE',  ( 159.9635946688021022, 268.7707599091479551, -17.14635356962945778 ) ) ;
#32707 = CARTESIAN_POINT ( 'NONE',  ( 35.38177548881301249, 32.37878583063844218, 9.188101187500006262 ) ) ;
#32708 = CARTESIAN_POINT ( 'NONE',  ( 190.0370014622527322, 286.8089957100377205, 16.96978714573610247 ) ) ;
#32709 = ORIENTED_EDGE ( 'NONE', *, *, #39279, .T. ) ;
#32710 = CARTESIAN_POINT ( 'NONE',  ( 164.7173348071851819, 279.5549278273611549, 11.88884794519514365 ) ) ;
#32711 = CARTESIAN_POINT ( 'NONE',  ( 194.4826705584825390, 293.7931287314651740, -16.11258321617245315 ) ) ;
#32712 = CARTESIAN_POINT ( 'NONE',  ( 10.46624461501205872, 188.3967562850346837, -4.648177544792955347E-16 ) ) ;
#32713 = ORIENTED_EDGE ( 'NONE', *, *, #84708, .F. ) ;
#32714 = CARTESIAN_POINT ( 'NONE',  ( 86.35458572345136474, 46.97350791603361131, -10.52386536561718700 ) ) ;
#32715 = CARTESIAN_POINT ( 'NONE',  ( 146.4729408656479563, 243.8262482093457493, 3.021315404115420679E-15 ) ) ;
#32716 = CARTESIAN_POINT ( 'NONE',  ( 69.71912771937687126, 204.3927522451418213, 10.00000000000009948 ) ) ;
#32717 = CARTESIAN_POINT ( 'NONE',  ( 6.626006335531184455, 41.42259438955097295, 59.99999999999999289 ) ) ;
#32718 = CARTESIAN_POINT ( 'NONE',  ( 73.98570270871887544, 68.92876820612472955, -11.10152750440661862 ) ) ;
#32719 = CARTESIAN_POINT ( 'NONE',  ( 155.1398527401465230, 261.9368881057492899, -17.02245700497956449 ) ) ;
#32720 = VERTEX_POINT ( 'NONE', #1752 ) ;
#32722 = ORIENTED_EDGE ( 'NONE', *, *, #83749, .F. ) ;
#32721 =( BOUNDED_CURVE ( )  B_SPLINE_CURVE ( 2, ( #76206, #60964, #6782, #68572, #91923, #70568, #78189, #55844, #40661 ),
 .UNSPECIFIED., .F., .T. ) 
 B_SPLINE_CURVE_WITH_KNOTS ( ( 3, 2, 2, 2, 3 ),
 ( 0.4475806451612903136, 0.4489247311827956888, 0.4516129032258064391, 0.4543010752688171894, 0.4556451612903225645 ),
 .UNSPECIFIED. ) 
 CURVE ( )  GEOMETRIC_REPRESENTATION_ITEM ( )  RATIONAL_B_SPLINE_CURVE ( ( 0.9330127018922194093, 0.9330127018922194093, 1.000000000000000000, 0.8660254037844387076, 1.000000000000000000, 0.8660254037844387076, 1.000000000000000000, 0.9330127018922194093, 0.9330127018922194093 ) ) 
 REPRESENTATION_ITEM ( '' )  );
#32723 = CARTESIAN_POINT ( 'NONE',  ( 178.4103510133881230, 261.0373811071510772, 12.15853430941466762 ) ) ;
#32724 = EDGE_LOOP ( 'NONE', ( #90819, #50080, #74090, #6187 ) ) ;
#32725 = CARTESIAN_POINT ( 'NONE',  ( 81.27629932712225980, 55.76935796986149541, 16.38776540150240990 ) ) ;
#32726 = ORIENTED_EDGE ( 'NONE', *, *, #96221, .F. ) ;
#32727 = CARTESIAN_POINT ( 'NONE',  ( 173.0071317692371053, 271.0804120453940413, 16.43005499174315887 ) ) ;
#32728 = CARTESIAN_POINT ( 'NONE',  ( 78.99356797199125424, 52.14063585753078911, 15.48230155875487135 ) ) ;
#32729 = ORIENTED_EDGE ( 'NONE', *, *, #2265, .F. ) ;
#32730 = CARTESIAN_POINT ( 'NONE',  ( 185.3138185638633217, 281.8611869091093354, -16.40392399104547039 ) ) ;
#32731 = CARTESIAN_POINT ( 'NONE',  ( 27.80420065655628648, 34.79103043416550634, 8.090169943749478065 ) ) ;
#32732 = CARTESIAN_POINT ( 'NONE',  ( 147.9288777062709528, 274.4266632365326473, -6.420914853544658740 ) ) ;
#32733 = CARTESIAN_POINT ( 'NONE',  ( 196.3804621193912112, 284.6068645810997850, -17.33595723632800656 ) ) ;
#32734 = CARTESIAN_POINT ( 'NONE',  ( 82.51641340783935163, 40.44452228410568040, 0.9102053940968845014 ) ) ;
#32735 = CARTESIAN_POINT ( 'NONE',  ( 201.1060504099706350, 282.3210983108598384, -18.18000168485860257 ) ) ;
#32736 = CARTESIAN_POINT ( 'NONE',  ( 76.67567146729663818, 63.34086528488000312, -15.41964329106467346 ) ) ;
#32737 = CARTESIAN_POINT ( 'NONE',  ( 157.9598681688460715, 280.9884947929961072, 2.154129884594043531 ) ) ;
#32738 = CARTESIAN_POINT ( 'NONE',  ( 125.9924764494033980, 252.7369531367911293, -4.594050593750048428 ) ) ;
#32739 = CARTESIAN_POINT ( 'NONE',  ( 70.76698439857202061, 60.51306593283057111, -14.69096287377648657 ) ) ;
#32740 = CARTESIAN_POINT ( 'NONE',  ( 36.38853680410606728, 41.98502408145596121, -5.678558825948271327 ) ) ;
#32741 = ADVANCED_FACE ( 'NONE', ( #32119 ), #61763, .F. ) ;
#32742 = ORIENTED_EDGE ( 'NONE', *, *, #10635, .T. ) ;
#32744 = ORIENTED_EDGE ( 'NONE', *, *, #96915, .F. ) ;
#32743 = FACE_OUTER_BOUND ( 'NONE', #72359, .T. ) ;
#32745 = CARTESIAN_POINT ( 'NONE',  ( 203.6424794855465450, 276.2395053873065649, 13.34248587893602433 ) ) ;
#32746 = CARTESIAN_POINT ( 'NONE',  ( 177.7978932797991263, 254.0055511546904654, 1.349567550766762825 ) ) ;
#32747 = CARTESIAN_POINT ( 'NONE',  ( 171.8805646714124862, 288.2467586487748576, -4.631873833586762856 ) ) ;
#32748 = CARTESIAN_POINT ( 'NONE',  ( 146.7209719250423632, 276.5188174203767062, 3.774014941632788389 ) ) ;
#32749 = CARTESIAN_POINT ( 'NONE',  ( 73.27264618352865000, 66.51157917954436982, 12.27253699350153404 ) ) ;
#32750 = CARTESIAN_POINT ( 'NONE',  ( 200.9521687275011175, 282.5876292032514243, -18.16013154125647944 ) ) ;
#32751 = CARTESIAN_POINT ( 'NONE',  ( 175.0853012839055509, 287.6725234473790351, -9.381267066206161687 ) ) ;
#32752 = CARTESIAN_POINT ( 'NONE',  ( 174.9264754436019302, 282.2672310181519606, 14.40274484580208814 ) ) ;
#32753 = CARTESIAN_POINT ( 'NONE',  ( 177.2275806558985778, 256.0915070734015444, -7.361266378673213318 ) ) ;
#32754 = ORIENTED_EDGE ( 'NONE', *, *, #11844, .F. ) ;
#32755 = CARTESIAN_POINT ( 'NONE',  ( 148.3874010092782498, 273.6324775792697892, -8.328854486678444857 ) ) ;
#32756 = CARTESIAN_POINT ( 'NONE',  ( 12.05626958406300098, 167.7677522451417929, -5.000000000000041744 ) ) ;
#32757 = EDGE_LOOP ( 'NONE', ( #98795, #69607 ) ) ;
#32758 = CARTESIAN_POINT ( 'NONE',  ( 71.86256228778262312, 72.60615528678950170, -0.5650332253009007211 ) ) ;
#32759 = CARTESIAN_POINT ( 'NONE',  ( 190.6688270659779221, 284.0946164064107506, -17.60360843008351495 ) ) ;
#32760 = CARTESIAN_POINT ( 'NONE',  ( 151.9683803660127808, 267.4300393925500998, -16.94882632825642332 ) ) ;
#32761 = CARTESIAN_POINT ( 'NONE',  ( 190.6023073677431512, 300.5141149296460981, 3.174888932019753973 ) ) ;
#32762 = CARTESIAN_POINT ( 'NONE',  ( 203.0337691736598629, 278.9821914694464340, 16.08167820133810011 ) ) ;
#32764 = CARTESIAN_POINT ( 'NONE',  ( 154.9134057170828100, 277.4270410806878999, -8.857178202958200686 ) ) ;
#32763 = CARTESIAN_POINT ( 'NONE',  ( 153.5124280503948171, 269.9541434048999804, 14.88175143766969377 ) ) ;
#32765 = VECTOR ( 'NONE', #46255, 1000.000000000000000 ) ;
#32766 = FACE_OUTER_BOUND ( 'NONE', #87514, .T. ) ;
#32767 = VERTEX_POINT ( 'NONE', #49340 ) ;
#32768 = CARTESIAN_POINT ( 'NONE',  ( 165.8366156597141696, 280.8532225693821260, -11.02208513961526926 ) ) ;
#32769 = CARTESIAN_POINT ( 'NONE',  ( 187.1558864241382594, 261.9731673870204531, -8.720117667986704291 ) ) ;
#32770 = CARTESIAN_POINT ( 'NONE',  ( -14.83262083840142154, 124.7156766241961208, -37.49999999999995737 ) ) ;
#32771 = CARTESIAN_POINT ( 'NONE',  ( 85.13974472830308571, 208.4155109091896350, 2.679491924311254714 ) ) ;
#32772 = CARTESIAN_POINT ( 'NONE',  ( 6.354935675815381657, 181.1427522451419350, 10.00000000000009415 ) ) ;
#32773 = CARTESIAN_POINT ( 'NONE',  ( 85.14411491811664234, 46.97365546850126350, 10.63533560768400044 ) ) ;
#32774 = CARTESIAN_POINT ( 'NONE',  ( 42.87860686303044844, 124.5258428655388911, -10.00000000000000000 ) ) ;
#32775 = CARTESIAN_POINT ( 'NONE',  ( 67.87252889196815886, 69.68634872786070389, 1.786884576500594068 ) ) ;
#32776 = CARTESIAN_POINT ( 'NONE',  ( 25.88271472100439041, 39.90032630942972247, 10.00000000000000000 ) ) ;
#32777 = CARTESIAN_POINT ( 'NONE',  ( 90.02596631606967037, 210.5327760586659451, 1.948934522072303157E-15 ) ) ;
#32778 = CARTESIAN_POINT ( 'NONE',  ( 203.5258219653775313, 278.1299310341851765, -16.21052911601769608 ) ) ;
#32779 = CARTESIAN_POINT ( 'NONE',  ( 88.05007481205849729, 44.74915561242152506, -4.497590196485170999 ) ) ;
#32780 = CARTESIAN_POINT ( 'NONE',  ( 147.9466025080311624, 275.4568191937016195, 4.863263704339665594 ) ) ;
#32781 = CARTESIAN_POINT ( 'NONE',  ( 202.7754741559590173, 279.4295715634463022, -15.65855077192107636 ) ) ;
#32782 = VECTOR ( 'NONE', #76736, 1000.000000000000000 ) ;
#32783 = B_SPLINE_CURVE_WITH_KNOTS ( 'NONE', 3,
 ( #66542, #81784, #50340, #12868, #97470, #12359, #57941, #28529, #96996, #5247, #19957, #17575, #50834, #20967 ),
 .UNSPECIFIED., .F., .F.,
 ( 4, 2, 2, 2, 2, 2, 4 ),
 ( 0.001073766153608202850, 0.001318213484469830509, 0.001562660815331458168, 0.002051555477054679659, 0.002296002807916289971, 0.002540450138777900716, 0.003029344800501188560 ),
 .UNSPECIFIED. ) ;
#32784 = CARTESIAN_POINT ( 'NONE',  ( 78.45861607683767147, 57.52921583862547550, 16.22413336569833220 ) ) ;
#32785 = CARTESIAN_POINT ( 'NONE',  ( 84.80383116528092557, 49.89350275441562843, -13.17492736023872091 ) ) ;
#32786 = CARTESIAN_POINT ( 'NONE',  ( 78.02488749478023067, 61.97397559377148468, 15.68332185870741036 ) ) ;
#32788 = CARTESIAN_POINT ( 'NONE',  ( 208.1912724900461740, 270.0491336852600170, -0.9856800448607289100 ) ) ;
#32787 = FACE_OUTER_BOUND ( 'NONE', #56307, .T. ) ;
#32789 = CARTESIAN_POINT ( 'NONE',  ( 207.9308153155450611, 270.5002587446924167, 5.985796430201889784 ) ) ;
#32790 = CARTESIAN_POINT ( 'NONE',  ( 169.2274513788552497, 252.2158712044186757, -9.272252751866769671 ) ) ;
#32791 = CARTESIAN_POINT ( 'NONE',  ( 205.4591571362178968, 274.7812962902297613, -13.63513100400704658 ) ) ;
#32792 = CARTESIAN_POINT ( 'NONE',  ( 168.2913993615551078, 273.7323137512423159, 16.83521432247344407 ) ) ;
#32793 = EDGE_CURVE ( 'NONE', #86134, #21873, #91934, .T. ) ;
#32794 = CARTESIAN_POINT ( 'NONE',  ( 78.65123893946785927, 54.86935689443330944, -16.05544503379834964 ) ) ;
#32795 = CARTESIAN_POINT ( 'NONE',  ( 40.82928596147627331, 60.38352576601455723, 10.00000000000000000 ) ) ;
#32796 = LINE ( 'NONE', #56078, #10910 ) ;
#32798 = EDGE_CURVE ( 'NONE', #95045, #79982, #15167, .T. ) ;
#32797 = CARTESIAN_POINT ( 'NONE',  ( 71.66369827319218189, 72.02185750324218816, -1.551229696566573502 ) ) ;
#32799 = CARTESIAN_POINT ( 'NONE',  ( 48.78150646083578579, 186.7202760586659736, -5.415160957724236172E-17 ) ) ;
#32801 = ADVANCED_FACE ( 'NONE', ( #37967 ), #14691, .T. ) ;
#32800 = CARTESIAN_POINT ( 'NONE',  ( 76.99381129068922291, 63.91386138922637628, -15.28064156999390732 ) ) ;
#32802 = ADVANCED_FACE ( 'NONE', ( #76021 ), #9239, .T. ) ;
#32803 = CARTESIAN_POINT ( 'NONE',  ( 61.79834339388186493, 215.6744531367911293, 4.594050593750047540 ) ) ;
#32804 = CARTESIAN_POINT ( 'NONE',  ( 88.19107160583139660, 43.69314304319705400, 0.1842422985582090333 ) ) ;
#32805 = CARTESIAN_POINT ( 'NONE',  ( 83.40455683621979688, 49.60330724181036999, -13.41979453150748114 ) ) ;
#32807 = DIRECTION ( 'NONE',  ( -0.000000000000000000, 0.000000000000000000, -1.000000000000000000 ) ) ;
#32806 = CARTESIAN_POINT ( 'NONE',  ( 175.5746833524315775, 278.5347786252573314, 16.94864957847115505 ) ) ;
#32808 = CARTESIAN_POINT ( 'NONE',  ( -54.21831688459418785, 33.63902229265146104, 10.00000000000000000 ) ) ;
#32809 = CARTESIAN_POINT ( 'NONE',  ( 25.99623195869282100, 35.98502408145594700, -5.678558825948271327 ) ) ;
#32810 = CARTESIAN_POINT ( 'NONE',  ( 164.2257943664163804, 246.1995755744450776, 2.121218676196017287E-15 ) ) ;
#32811 = CARTESIAN_POINT ( 'NONE',  ( 149.1486417047969155, 272.3139700178423368, -11.47583619705022606 ) ) ;
#32812 = VERTEX_POINT ( 'NONE', #47576 ) ;
#32813 = CARTESIAN_POINT ( 'NONE',  ( 24.83368966200164607, 16.19860640527292261, 2.839279412974134775 ) ) ;
#32814 = CARTESIAN_POINT ( 'NONE',  ( 64.07166007881600933, 216.9869531367911293, 4.594050593750046652 ) ) ;
#32815 = CARTESIAN_POINT ( 'NONE',  ( 76.64464310018406934, 63.53199411942404851, 15.34601863127964627 ) ) ;
#32816 = CARTESIAN_POINT ( 'NONE',  ( -22.42236680055709641, 157.8615022471902591, 0.000000000000000000 ) ) ;
#32817 = CARTESIAN_POINT ( 'NONE',  ( 172.8067276174556355, 290.3015201877066147, -0.3301680610896204904 ) ) ;
#32818 = FACE_OUTER_BOUND ( 'NONE', #81582, .T. ) ;
#32819 = CARTESIAN_POINT ( 'NONE',  ( 202.1076200406028818, 280.5863288232868058, 16.88052457987451760 ) ) ;
#32820 = CARTESIAN_POINT ( 'NONE',  ( 114.8426596992763962, 247.1115022471903160, -5.000000000000047962 ) ) ;
#32821 = CARTESIAN_POINT ( 'NONE',  ( 200.6449165581618956, 283.1198055712825976, 18.35107460171532523 ) ) ;
#32822 = CARTESIAN_POINT ( 'NONE',  ( 206.8986117509267899, 272.2880877623646825, 6.975890063856878598 ) ) ;
#32823 = VERTEX_POINT ( 'NONE', #2503 ) ;
#32824 = CARTESIAN_POINT ( 'NONE',  ( 149.1198674273730660, 273.3870518558833851, -9.828147701528390456 ) ) ;
#32825 = CARTESIAN_POINT ( 'NONE',  ( 185.3272745120582101, 271.3634168311705253, 16.73381828275187999 ) ) ;
#32826 = VERTEX_POINT ( 'NONE', #39961 ) ;
#32827 = CARTESIAN_POINT ( 'NONE',  ( 202.2576150004249200, 280.3265299319959354, 16.24828394350762295 ) ) ;
#32828 = CARTESIAN_POINT ( 'NONE',  ( 67.68514482100736984, 66.83340866827894899, -8.536435324610977204 ) ) ;
#32829 = CARTESIAN_POINT ( 'NONE',  ( 66.77376812102318127, 68.41195941748605946, -4.433129028897194068 ) ) ;
#32830 = DIRECTION ( 'NONE',  ( 0.000000000000000000, 0.000000000000000000, 1.000000000000000000 ) ) ;
#32831 = ORIENTED_EDGE ( 'NONE', *, *, #30962, .T. ) ;
#32832 = CARTESIAN_POINT ( 'NONE',  ( 72.48454840684568978, 71.59325672763723958, 6.192859277029556075 ) ) ;
#32833 = CARTESIAN_POINT ( 'NONE',  ( 170.4750202401941408, 250.3351638306627365, 3.406270645389806173 ) ) ;
#32834 = CARTESIAN_POINT ( 'NONE',  ( 148.6206126714731397, 275.0791264792570132, 7.693551923222978317 ) ) ;
#32835 = AXIS2_PLACEMENT_3D ( 'NONE', #88441, #19001, #49876 ) ;
#32836 = EDGE_LOOP ( 'NONE', ( #17257, #26664, #44037, #6183 ) ) ;
#32837 = PRODUCT_DEFINITION ( 'UNKNOWN', '', #52713, #25049 ) ;
#32838 = CARTESIAN_POINT ( 'NONE',  ( 21.83270445532239989, 34.64646525600390703, -2.839279412974133887 ) ) ;
#32839 = CARTESIAN_POINT ( 'NONE',  ( 75.12194974421997529, 66.37886708184480256, -13.15189938993499830 ) ) ;
#32840 = CARTESIAN_POINT ( 'NONE',  ( 84.55133599061954897, 48.00037868907449479, -11.86301670575332068 ) ) ;
#32841 = CIRCLE ( 'NONE', #89533, 1.449999999999993072 ) ;
#32842 = CARTESIAN_POINT ( 'NONE',  ( 167.9894996763587756, 276.8290543759245566, 15.53392256876827204 ) ) ;
#32843 = DIRECTION ( 'NONE',  ( -0.6911977992267216431, 0.7226656227773233798, 0.000000000000000000 ) ) ;
#32844 = VERTEX_POINT ( 'NONE', #48597 ) ;
#32845 = VERTEX_POINT ( 'NONE', #88147 ) ;
#32846 = CARTESIAN_POINT ( 'NONE',  ( 185.9403311553370770, 296.8630701276886157, 7.448205859860947520 ) ) ;
#32848 = CARTESIAN_POINT ( 'NONE',  ( 148.2670916631250861, 273.8408594794321971, -7.980554973576580835 ) ) ;
#32847 = CARTESIAN_POINT ( 'NONE',  ( 68.04555932152995013, 65.72381589692875536, 10.88124144663173354 ) ) ;
#32849 = CARTESIAN_POINT ( 'NONE',  ( 208.3194307158603067, 269.8271571267425770, -2.120200867047394855 ) ) ;
#32850 = CARTESIAN_POINT ( 'NONE',  ( 154.8989000222956349, 262.3542304552891551, 17.41779271305265908 ) ) ;
#32851 = CARTESIAN_POINT ( 'NONE',  ( 185.2939906634090619, 292.6913508051172812, -11.83370942357023026 ) ) ;
#32852 = CARTESIAN_POINT ( 'NONE',  ( 157.8429099974857195, 257.2550556002704525, -17.85752049034686095 ) ) ;
#32853 = CARTESIAN_POINT ( 'NONE',  ( 137.1425535231280151, 259.1744531367911009, 4.594050593750047540 ) ) ;
#32854 = CARTESIAN_POINT ( 'NONE',  ( 71.78107986572921106, 62.71246368623720002, -14.51539090988953440 ) ) ;
#32855 = EDGE_CURVE ( 'NONE', #14695, #68463, #15539, .T. ) ;
#32856 = VECTOR ( 'NONE', #45765, 1000.000000000000000 ) ;
#32857 = DIRECTION ( 'NONE',  ( -0.000000000000000000, -0.000000000000000000, -1.000000000000000000 ) ) ;
#32858 = CARTESIAN_POINT ( 'NONE',  ( 78.11742282250361313, 228.1589784336661353, -6.496448406907675876E-16 ) ) ;
#32859 = ORIENTED_EDGE ( 'NONE', *, *, #66106, .F. ) ;
#32860 = CARTESIAN_POINT ( 'NONE',  ( 150.6431064791187850, 269.7254810985950257, 15.11064854015152470 ) ) ;
#32861 = CARTESIAN_POINT ( 'NONE',  ( 78.14027010749673252, 61.52421145379764766, -16.15198519767693242 ) ) ;
#32862 = EDGE_CURVE ( 'NONE', #2950, #84918, #91925, .T. ) ;
#32863 = ORIENTED_EDGE ( 'NONE', *, *, #34860, .F. ) ;
#32864 = CARTESIAN_POINT ( 'NONE',  ( 195.3376996304517945, 292.3121749368662563, -16.73230682301962702 ) ) ;
#32865 = EDGE_LOOP ( 'NONE', ( #51881, #91068, #7845, #19686 ) ) ;
#32866 = CARTESIAN_POINT ( 'NONE',  ( 80.31236711830932506, 44.94079046180152659, -11.22303980454576333 ) ) ;
#32867 = CARTESIAN_POINT ( 'NONE',  ( 83.23273246114447943, 208.8615022471902023, 5.000000000000051514 ) ) ;
#32868 = DIRECTION ( 'NONE',  ( 0.8660254037844377084, 0.5000000000000015543, 0.000000000000000000 ) ) ;
#32869 = CARTESIAN_POINT ( 'NONE',  ( 162.8386403195304410, 249.0994062285972461, 10.29435687412694911 ) ) ;
#32870 = CARTESIAN_POINT ( 'NONE',  ( 81.15909907030567183, 48.17545335780159377, -13.29838471746604966 ) ) ;
#32871 = CARTESIAN_POINT ( 'NONE',  ( 207.6964130646365163, 270.9062553526738384, 2.975933372805272814 ) ) ;
#32872 = CARTESIAN_POINT ( 'NONE',  ( 89.32180003184730310, 228.5024278399160949, 9.188101187500095079 ) ) ;
#32873 = ORIENTED_EDGE ( 'NONE', *, *, #14466, .F. ) ;
#32874 = EDGE_LOOP ( 'NONE', ( #52622, #67880, #22903, #62083 ) ) ;
#32875 = CARTESIAN_POINT ( 'NONE',  ( -115.0954152546897973, 78.37593066204027537, -37.49999999999999289 ) ) ;
#32876 = CARTESIAN_POINT ( 'NONE',  ( 208.1912724900461740, 270.0491336852600170, -0.9856800448607289100 ) ) ;
#32877 = ORIENTED_EDGE ( 'NONE', *, *, #69523, .F. ) ;
#32878 = ADVANCED_FACE ( 'NONE', ( #64287 ), #48078, .T. ) ;
#32879 = CARTESIAN_POINT ( 'NONE',  ( 19.48182849416020090, 34.18080186712593616, 3.090169943749475401 ) ) ;
#32880 = CARTESIAN_POINT ( 'NONE',  ( 165.1988661533298739, 286.0649040768676628, 1.324426972201139918 ) ) ;
#32881 = CARTESIAN_POINT ( 'NONE',  ( 110.0998739067015606, 222.8262482093458061, 3.021315404115420679E-15 ) ) ;
#32882 = CARTESIAN_POINT ( 'NONE',  ( 87.74222765753326314, 44.73834681983743877, 5.012736470890956753 ) ) ;
#32883 = ORIENTED_EDGE ( 'NONE', *, *, #33652, .F. ) ;
#32884 = CARTESIAN_POINT ( 'NONE',  ( 188.7025032568610641, 295.1526436589835498, 11.77953644933642430 ) ) ;
#32885 = CARTESIAN_POINT ( 'NONE',  ( 158.1484577441942747, 274.4577636394142246, 13.02392648995051161 ) ) ;
#32886 = CARTESIAN_POINT ( 'NONE',  ( 159.2713554375903300, 254.7809155221686410, -15.70062444474382168 ) ) ;
#32887 = CARTESIAN_POINT ( 'NONE',  ( 155.8082389063325195, 262.2725718350632178, -17.02355505207763287 ) ) ;
#32888 = CARTESIAN_POINT ( 'NONE',  ( 177.5742234820266106, 284.9350511118382769, 13.03802085023674628 ) ) ;
#32889 = CYLINDRICAL_SURFACE ( 'NONE', #95346, 17.82106496071139645 ) ;
#32890 = CARTESIAN_POINT ( 'NONE',  ( 139.7950166422676261, 261.5177522451418781, 5.000000000000046185 ) ) ;
#32891 = VERTEX_POINT ( 'NONE', #79536 ) ;
#32892 = CARTESIAN_POINT ( 'NONE',  ( 203.6032271198143633, 277.1556831885280303, -14.25317073278892011 ) ) ;
#32893 = CARTESIAN_POINT ( 'NONE',  ( 200.7897860911934913, 282.8688841796032420, 18.17522996445731920 ) ) ;
#32894 = CARTESIAN_POINT ( 'NONE',  ( 83.08910943491284229, 41.56722408657803669, 2.852113461528766880 ) ) ;
#32895 = CARTESIAN_POINT ( 'NONE',  ( 187.8608301704034886, 266.3119843265345708, -12.10641229248959405 ) ) ;
#32896 = CARTESIAN_POINT ( 'NONE',  ( 83.44503355366286712, 51.91352208420825320, 15.00625484349790284 ) ) ;
#32897 = CARTESIAN_POINT ( 'NONE',  ( 199.4720805209845196, 266.1420231043892954, 4.760232788326643316 ) ) ;
#32898 = CARTESIAN_POINT ( 'NONE',  ( 153.1398868314278729, 270.6072410628295302, 13.89127424760058283 ) ) ;
#32899 = VERTEX_POINT ( 'NONE', #10094 ) ;
#32900 = CARTESIAN_POINT ( 'NONE',  ( 206.8968397926183229, 272.2911568841838061, 7.145103750817420440 ) ) ;
#32902 = CARTESIAN_POINT ( 'NONE',  ( 185.6113847613186465, 266.0283385180310347, 13.02359781958079488 ) ) ;
#32901 = CARTESIAN_POINT ( 'NONE',  ( 179.4063595725527875, 266.1022058418245706, -14.81063788915213308 ) ) ;
#32903 = CARTESIAN_POINT ( 'NONE',  ( 199.2216792767152640, 281.9425204638906166, -16.60457197858584522 ) ) ;
#32904 = ADVANCED_FACE ( 'NONE', ( #25804 ), #40957, .T. ) ;
#32905 = CARTESIAN_POINT ( 'NONE',  ( 33.22292548896825082, 27.38052372038642801, 10.00000000000000533 ) ) ;
#32906 = CARTESIAN_POINT ( 'NONE',  ( -11.40312891409031693, 78.77562236714182120, 52.49999999999999289 ) ) ;
#32907 = CARTESIAN_POINT ( 'NONE',  ( 168.7545650535763002, 272.9722043789810186, 15.95301077176753601 ) ) ;
#32908 = CARTESIAN_POINT ( 'NONE',  ( 181.5493510114948492, 273.6912172031477439, 16.52691019570659847 ) ) ;
#32909 = LINE ( 'NONE', #23808, #9715 ) ;
#32910 = CARTESIAN_POINT ( 'NONE',  ( 192.0613752418878448, 262.3092312885352158, 2.971550368156713251 ) ) ;
#32911 = CARTESIAN_POINT ( 'NONE',  ( 207.7836085030675690, 270.7552284231231852, -5.468305433308493058 ) ) ;
#32912 = CARTESIAN_POINT ( 'NONE',  ( -0.5554856785977280165, 179.6744531367911577, 4.594050593750047540 ) ) ;
#32913 = PLANE ( 'NONE',  #48501 ) ;
#32914 = ORIENTED_EDGE ( 'NONE', *, *, #54833, .T. ) ;
#32915 = EDGE_CURVE ( 'NONE', #63230, #983, #49542, .T. ) ;
#32916 = EDGE_CURVE ( 'NONE', #99556, #34648, #4888, .T. ) ;
#32918 = CARTESIAN_POINT ( 'NONE',  ( 161.3295519522830830, 253.0809256290032465, -15.05235766421041532 ) ) ;
#32917 = AXIS2_PLACEMENT_3D ( 'NONE', #97418, #13313, #52766 ) ;
#32919 = LINE ( 'NONE', #63823, #88873 ) ;
#32920 = CARTESIAN_POINT ( 'NONE',  ( 81.97536373108215457, 41.18676643964585793, 5.503149011488202902 ) ) ;
#32921 = CARTESIAN_POINT ( 'NONE',  ( 27.67213724359008964, 174.5327760586659736, 1.948934522072302763E-15 ) ) ;
#32922 = CYLINDRICAL_SURFACE ( 'NONE', #45840, 11.89249999999999652 ) ;
#32923 = CARTESIAN_POINT ( 'NONE',  ( 39.22461576370143632, 27.81029122506297568, 8.090169943749479842 ) ) ;
#32924 = CARTESIAN_POINT ( 'NONE',  ( 180.9647783388077755, 293.3161038431775296, 6.181325619054465648 ) ) ;
#32925 = CARTESIAN_POINT ( 'NONE',  ( 146.6363376198206652, 276.6654083370839885, -0.5879280619134327202 ) ) ;
#32926 = CARTESIAN_POINT ( 'NONE',  ( 196.2967275982209117, 290.6510897708104721, 17.16888829023426055 ) ) ;
#32927 = CARTESIAN_POINT ( 'NONE',  ( 6.950328144465094837, 181.4865022471903160, -10.00000000000009592 ) ) ;
#32928 = CARTESIAN_POINT ( 'NONE',  ( 0.005075371086064872639, 27.18819441265828019, -10.00000000000000000 ) ) ;
#32929 = PRODUCT ( 'Center Base Mounting Screw', 'Center Base Mounting Screw', '', ( #75570 ) ) ;
#32930 = CARTESIAN_POINT ( 'NONE',  ( 186.5128128464827455, 296.3652354721813822, -8.829210103799347564 ) ) ;
#32931 = CARTESIAN_POINT ( 'NONE',  ( -27.42236680055714260, 166.5217562850347406, 1.224646799147364892E-15 ) ) ;
#32932 = CARTESIAN_POINT ( 'NONE',  ( 90.08876690777130136, 209.4865022471901455, 1.119607411625061291E-15 ) ) ;
#32933 = CARTESIAN_POINT ( 'NONE',  ( 74.40040945360185276, 65.95912601619707516, -13.09620949053549666 ) ) ;
#32934 = CARTESIAN_POINT ( 'NONE',  ( -63.30067564770008914, 39.94154026010144065, 10.00000000000000000 ) ) ;
#32935 = CARTESIAN_POINT ( 'NONE',  ( 203.4000736791844872, 270.0313898409100375, 6.690177824349802904 ) ) ;
#32936 = CARTESIAN_POINT ( 'NONE',  ( 48.83545950068980090, 192.8768266524159856, -9.188101187500091527 ) ) ;
#32937 = CARTESIAN_POINT ( 'NONE',  ( 190.5217943342473745, 281.4870030958396683, 17.81127109971334121 ) ) ;
#32938 = CARTESIAN_POINT ( 'NONE',  ( 204.9345165894207526, 270.9732339236668963, -6.503218611638661883 ) ) ;
#32939 = CARTESIAN_POINT ( 'NONE',  ( 151.0801312611820890, 268.9685319718947198, -15.83903210480701240 ) ) ;
#32940 = CARTESIAN_POINT ( 'NONE',  ( 144.9863040978925142, 263.1751974929321705, -1.822351119449946140E-15 ) ) ;
#32941 = ORIENTED_EDGE ( 'NONE', *, *, #20929, .T. ) ;
#32942 = LINE ( 'NONE', #8650, #7082 ) ;
#32943 = CARTESIAN_POINT ( 'NONE',  ( 48.05801951159152452, 75.31115804243518141, -10.00000000000000000 ) ) ;
#32944 = DIRECTION ( 'NONE',  ( -0.03277852384266333879, 0.9994626398093607866, 0.000000000000000000 ) ) ;
#32945 = CYLINDRICAL_SURFACE ( 'NONE', #21314, 60.00000000000002132 ) ;
#32946 = CARTESIAN_POINT ( 'NONE',  ( 22.11595037535113661, 30.95586893147756413, 7.433330006724141015 ) ) ;
#32947 = CARTESIAN_POINT ( 'NONE',  ( 162.9148248802443106, 248.4702413316674381, 9.709394404200100581 ) ) ;
#32948 = CARTESIAN_POINT ( 'NONE',  ( 196.4783028304046013, 290.3365922432724346, -16.37291435488387492 ) ) ;
#32949 = CARTESIAN_POINT ( 'NONE',  ( 189.0300115529333311, 269.8965634406930576, -15.48922461594477795 ) ) ;
#32950 = VERTEX_POINT ( 'NONE', #97217 ) ;
#32951 = CARTESIAN_POINT ( 'NONE',  ( 7.668962567711002265, 16.37878583063838533, 9.188101187500006262 ) ) ;
#32952 = DIRECTION ( 'NONE',  ( 0.8660254037844382635, 0.5000000000000004441, 0.000000000000000000 ) ) ;
#32953 = CARTESIAN_POINT ( 'NONE',  ( 72.06083603792721703, 60.17315645985856065, -15.09511454206493042 ) ) ;
#32954 = PLANE ( 'NONE',  #87807 ) ;
#32955 = ORIENTED_EDGE ( 'NONE', *, *, #77533, .T. ) ;
#32956 = DIRECTION ( 'NONE',  ( -0.8660254037844387076, -0.4999999999999998890, -0.000000000000000000 ) ) ;
#32957 = FACE_OUTER_BOUND ( 'NONE', #74283, .T. ) ;
#32958 = DIRECTION ( 'NONE',  ( 1.000000000000000000, 0.000000000000000000, 0.000000000000000000 ) ) ;
#32959 = CARTESIAN_POINT ( 'NONE',  ( 149.6071296322179194, 271.5198456328920997, 12.75640156477042453 ) ) ;
#32960 = ORIENTED_EDGE ( 'NONE', *, *, #24673, .T. ) ;
#32961 = ORIENTED_EDGE ( 'NONE', *, *, #1513, .T. ) ;
#32963 = CARTESIAN_POINT ( 'NONE',  ( 151.0960476679098008, 269.3483702054729747, -13.92775656254562300 ) ) ;
#32962 = CARTESIAN_POINT ( 'NONE',  ( 189.6192806120793364, 274.1937585566731741, -15.66399881635599201 ) ) ;
#32964 = ORIENTED_EDGE ( 'NONE', *, *, #72781, .F. ) ;
#32965 = CARTESIAN_POINT ( 'NONE',  ( 152.7729059155601021, 266.0365602647466972, -17.50667083025758686 ) ) ;
#32966 = CARTESIAN_POINT ( 'NONE',  ( 72.06656620204616104, 72.31304997165260318, -3.465063205002326452 ) ) ;
#32967 = CARTESIAN_POINT ( 'NONE',  ( 68.88004550269626236, 70.89535253697187045, -0.8688780715835217050 ) ) ;
#32968 = CARTESIAN_POINT ( 'NONE',  ( 3.124773676633713748, 24.73705186507751463, -3.090169943749475845 ) ) ;
#32969 = CARTESIAN_POINT ( 'NONE',  ( 157.0877926458200307, 258.5629572190321710, -17.40668770468195703 ) ) ;
#32970 = B_SPLINE_CURVE_WITH_KNOTS ( 'NONE', 3,
 ( #26419, #18819, #42586, #64412, #34994, #3145, #34030, #17824, #96347, #73519, #88772, #49703, #95862, #18325, #56801, #48725, #42100, #79657, #80657, #26914, #11236, #73033, #95376, #57794, #3626, #34504, #65406, #25928, #50205, #80155, #94844, #81156, #87293, #11724, #65896, #27419, #25405, #10221, #41089, #72025, #2627, #33516, #87786, #47528 ),
 .UNSPECIFIED., .F., .F.,
 ( 4, 2, 2, 2, 2, 2, 2, 2, 2, 2, 2, 2, 2, 2, 2, 2, 2, 2, 2, 2, 2, 4 ),
 ( 0.0008953238127824564166, 0.0009931015673485474055, 0.001090879321914638286, 0.001188657076480728950, 0.001286434831046820047, 0.001481990340179001591, 0.001677545849311183569, 0.002068656867575712974, 0.002459767885840242162, 0.004024211958898229677, 0.004806433995427187439, 0.005197545013691587390, 0.005393100522823786498, 0.005490878277389886486, 0.005588656031955986474, 0.005637544909239055116, 0.005686433786522122891, 0.005784211541088147418, 0.005979767050220238973, 0.006370878068484379583, 0.006761989086748520193, 0.007153100105012659936 ),
 .UNSPECIFIED. ) ;
#32971 = CARTESIAN_POINT ( 'NONE',  ( 102.9345500736427113, 239.4244531367911293, -4.594050593750046652 ) ) ;
#32972 = CARTESIAN_POINT ( 'NONE',  ( 148.9322735291567597, 272.6887306911919495, -12.40988026045598858 ) ) ;
#32974 = AXIS2_PLACEMENT_3D ( 'NONE', #23837, #2062, #17241 ) ;
#32973 = CARTESIAN_POINT ( 'NONE',  ( 183.7864977633626324, 289.5743890241738541, -13.10971297814887215 ) ) ;
#32975 = ADVANCED_FACE ( 'NONE', ( #98701 ), #66775, .T. ) ;
#32976 = ORIENTED_EDGE ( 'NONE', *, *, #98535, .F. ) ;
#32977 = DIRECTION ( 'NONE',  ( -0.4554470513245730823, -0.8902628732232696906, 0.000000000000000000 ) ) ;
#32978 = ORIENTED_EDGE ( 'NONE', *, *, #19445, .T. ) ;
#32979 = CARTESIAN_POINT ( 'NONE',  ( 28.30082151474694641, 24.84335787977763843, 9.188101187500006262 ) ) ;
#32980 = CARTESIAN_POINT ( 'NONE',  ( 159.2554912534056939, 254.8083930951974878, 16.49944922174842432 ) ) ;
#32981 = CARTESIAN_POINT ( 'NONE',  ( 70.93672144898081910, 70.68531007502453178, -6.225600342418550426 ) ) ;
#32982 = EDGE_CURVE ( 'NONE', #52414, #28862, #27180, .T. ) ;
#32983 = CARTESIAN_POINT ( 'NONE',  ( 66.96803994030899787, 197.2202760586659736, -5.415160957724236172E-17 ) ) ;
#32984 = CARTESIAN_POINT ( 'NONE',  ( 73.93840856004327122, 68.59252082510937498, 11.39217114877861547 ) ) ;
#32985 = CARTESIAN_POINT ( 'NONE',  ( 191.5694344253287511, 298.8390017285333897, 8.250976118904059575 ) ) ;
#32986 = CARTESIAN_POINT ( 'NONE',  ( -115.0954152546900673, 78.37593066204081538, 30.52142883766498827 ) ) ;
#32987 = CARTESIAN_POINT ( 'NONE',  ( 176.5111396222833946, 273.2017208239215620, 16.97504237463097709 ) ) ;
#32988 = VERTEX_POINT ( 'NONE', #44459 ) ;
#32989 = VECTOR ( 'NONE', #22867, 1000.000000000000000 ) ;
#32990 = CARTESIAN_POINT ( 'NONE',  ( 73.47351968716873216, 58.90398476228797620, -15.65848594678527839 ) ) ;
#32991 = AXIS2_PLACEMENT_3D ( 'NONE', #5508, #13616, #28296 ) ;
#32992 = CARTESIAN_POINT ( 'NONE',  ( 177.8586651343115363, 288.9770943732676756, 11.13517240723511392 ) ) ;
#32993 = CARTESIAN_POINT ( 'NONE',  ( 170.9811431790156462, 280.9458665424763240, 14.82329785628973440 ) ) ;
#32994 = EDGE_LOOP ( 'NONE', ( #69897, #36022, #1988, #42822 ) ) ;
#32995 = CARTESIAN_POINT ( 'NONE',  ( 171.7034968969801980, 259.3927777497087277, -13.81093080074480461 ) ) ;
#32996 = CARTESIAN_POINT ( 'NONE',  ( 173.8399428679245773, 278.0649905663252639, -16.28034435741132668 ) ) ;
#32997 = ADVANCED_FACE ( 'NONE', ( #52070 ), #15546, .T. ) ;
#32998 = CYLINDRICAL_SURFACE ( 'NONE', #1426, 17.82106496071139645 ) ;
#32999 = CARTESIAN_POINT ( 'NONE',  ( 193.1569697810063531, 296.0893098336876506, -13.02398914535779539 ) ) ;
#33000 = CIRCLE ( 'NONE', #29751, 70.00000000000001421 ) ;
#33001 = CARTESIAN_POINT ( 'NONE',  ( 148.9275518150011806, 272.6969089400084272, 12.34519124974546500 ) ) ;
#33002 = CARTESIAN_POINT ( 'NONE',  ( 178.8499588115995209, 270.3591463898502525, 16.16603941770465624 ) ) ;
#33003 = CARTESIAN_POINT ( 'NONE',  ( 88.05246585649720714, 43.65063640626211594, -1.233213520688016374 ) ) ;
#33004 = CARTESIAN_POINT ( 'NONE',  ( 67.52528295890758159, 67.08866990654458107, 8.951888472663769747 ) ) ;
#33005 = CARTESIAN_POINT ( 'NONE',  ( 73.19903135511377457, 64.92610867417256770, -13.26410356664282553 ) ) ;
#33006 = CARTESIAN_POINT ( 'NONE',  ( 5.530962353892125094, 15.14441083166257584, 0.000000000000000000 ) ) ;
#33007 = CARTESIAN_POINT ( 'NONE',  ( 109.0781781035623226, 233.7833772461660544, -9.188101187500095079 ) ) ;
#33008 = ORIENTED_EDGE ( 'NONE', *, *, #8161, .T. ) ;
#33009 = CARTESIAN_POINT ( 'NONE',  ( 191.1192699377806719, 299.6187094927299199, -9.526914969203620132 ) ) ;
#33010 = CARTESIAN_POINT ( 'NONE',  ( 83.29340746618338187, 41.55334719867666848, 2.042985643346537206 ) ) ;
#33011 = CARTESIAN_POINT ( 'NONE',  ( 155.1398527401465230, 261.9368881057492899, -17.02245700497956449 ) ) ;
#33012 = EDGE_CURVE ( 'NONE', #58450, #35, #42358, .T. ) ;
#33013 = B_SPLINE_CURVE_WITH_KNOTS ( 'NONE', 3,
 ( #56945, #95003, #33157, #41748, #10872, #87931 ),
 .UNSPECIFIED., .F., .F.,
 ( 4, 2, 4 ),
 ( 0.02072061098569386028, 0.02529064359198138212, 0.02986067619826890049 ),
 .UNSPECIFIED. ) ;
#33014 = CARTESIAN_POINT ( 'NONE',  ( 182.8075329105516289, 285.5996758505444291, -15.91971760981349071 ) ) ;
#33015 = CARTESIAN_POINT ( 'NONE',  ( 83.90892505094211629, 51.89215068963646615, -14.49862402916220461 ) ) ;
#33016 = CARTESIAN_POINT ( 'NONE',  ( 174.8677899224096564, 252.9159942513826707, 5.064243870650649626 ) ) ;
#33017 = EDGE_LOOP ( 'NONE', ( #31661, #13881, #85607, #69698 ) ) ;
#33018 = FACE_OUTER_BOUND ( 'NONE', #13907, .T. ) ;
#33019 =( BOUNDED_CURVE ( )  B_SPLINE_CURVE ( 2, ( #80272, #41714, #11357, #34619, #55895, #57412, #42211, #65031, #88393 ),
 .UNSPECIFIED., .F., .T. ) 
 B_SPLINE_CURVE_WITH_KNOTS ( ( 3, 2, 2, 2, 3 ),
 ( 0.6733870967741935054, 0.6747311827956988806, 0.6774193548387096309, 0.6801075268817203812, 0.6814516129032257563 ),
 .UNSPECIFIED. ) 
 CURVE ( )  GEOMETRIC_REPRESENTATION_ITEM ( )  RATIONAL_B_SPLINE_CURVE ( ( 0.9330127018922194093, 0.9330127018922194093, 1.000000000000000000, 0.8660254037844387076, 1.000000000000000000, 0.8660254037844387076, 1.000000000000000000, 0.9330127018922194093, 0.9330127018922194093 ) ) 
 REPRESENTATION_ITEM ( '' )  );
#33020 = CARTESIAN_POINT ( 'NONE',  ( 154.5768095353619174, 273.4844840904814305, -13.32170113451727111 ) ) ;
#33021 = CARTESIAN_POINT ( 'NONE',  ( 182.7382853101230182, 260.8451441236999244, 9.502958598710858240 ) ) ;
#33022 = CARTESIAN_POINT ( 'NONE',  ( 164.6359882590319899, 245.4890989114802551, -0.8957991669032092652 ) ) ;
#33023 = CARTESIAN_POINT ( 'NONE',  ( 73.55652807945510574, 69.73106060664957795, -9.395567069825068174 ) ) ;
#33024 = CARTESIAN_POINT ( 'NONE',  ( 150.6386650955079176, 269.7331738006648720, -15.06054658539322766 ) ) ;
#33025 = CARTESIAN_POINT ( 'NONE',  ( 188.7422573179599397, 298.9020585943546280, 4.794932212363814727 ) ) ;
#33026 = CARTESIAN_POINT ( 'NONE',  ( -17.81126293257621995, 23.08927765589694303, 177.5919119679930134 ) ) ;
#33027 = CARTESIAN_POINT ( 'NONE',  ( 61.04057116557046925, 215.2369531367911009, -4.594050593750048428 ) ) ;
#33028 = CARTESIAN_POINT ( 'NONE',  ( 73.41965926039753754, 61.58357384648181920, -15.38293892878691160 ) ) ;
#33029 = CARTESIAN_POINT ( 'NONE',  ( 205.0716081116550527, 275.4525508911965517, -12.57761053684872188 ) ) ;
#33030 = CARTESIAN_POINT ( 'NONE',  ( 88.04743768874705268, 44.61440943640608481, -4.110277753786412802 ) ) ;
#33031 = EDGE_CURVE ( 'NONE', #61735, #30468, #60467, .T. ) ;
#33032 = CARTESIAN_POINT ( 'NONE',  ( 71.56516262931459949, 71.04936870583668451, -5.185425663852958778 ) ) ;
#33033 = CARTESIAN_POINT ( 'NONE',  ( 174.2107174956932454, 262.0554560900756087, 14.36206619626495140 ) ) ;
#33034 = CARTESIAN_POINT ( 'NONE',  ( -75.14068524134967220, 52.46521621197197760, -10.00000000000000000 ) ) ;
#33035 = CARTESIAN_POINT ( 'NONE',  ( 178.6412003039374383, 292.1250764344173945, -7.162751075077554930 ) ) ;
#33036 = CARTESIAN_POINT ( 'NONE',  ( 155.6328838216860220, 261.0829332228125850, -17.51014940606912518 ) ) ;
#33037 = CARTESIAN_POINT ( 'NONE',  ( 180.0228151894829978, 262.0024909477526194, 12.25612893952419924 ) ) ;
#33038 = EDGE_CURVE ( 'NONE', #84449, #86487, #29771, .T. ) ;
#33039 = CARTESIAN_POINT ( 'NONE',  ( 125.0725847779322351, 243.0177522451418497, -10.00000000000009592 ) ) ;
#33040 = CARTESIAN_POINT ( 'NONE',  ( 41.97569090598251762, 208.3207943907113133, -18.47570218321542868 ) ) ;
#33041 = ORIENTED_EDGE ( 'NONE', *, *, #86968, .T. ) ;
#33042 = ADVANCED_FACE ( 'NONE', ( #91601 ), #54477, .F. ) ;
#33043 = CARTESIAN_POINT ( 'NONE',  ( 189.8238368927809745, 301.8624653444729802, -0.3620111495846872751 ) ) ;
#33044 = DIRECTION ( 'NONE',  ( -0.000000000000000000, -0.000000000000000000, -1.000000000000000000 ) ) ;
#33045 = CARTESIAN_POINT ( 'NONE',  ( 30.62142885764206568, 197.6744531367911293, 4.594050593750047540 ) ) ;
#33046 = CARTESIAN_POINT ( 'NONE',  ( 15.34872451668155868, 24.56454794089041016, 10.00000000000000355 ) ) ;
#33047 = CARTESIAN_POINT ( 'NONE',  ( 67.97219646607847210, 65.51810466360356600, -10.31124141321363830 ) ) ;
#33048 = CARTESIAN_POINT ( 'NONE',  ( 76.28872632190459058, 51.00282802105012081, -16.03419075268624994 ) ) ;
#33049 = CARTESIAN_POINT ( 'NONE',  ( 190.9559560067148425, 299.9015775189195665, -4.895152914295826108 ) ) ;
#33050 = CARTESIAN_POINT ( 'NONE',  ( 66.60908278236352942, 68.04996951702554497, -6.508824207629166914 ) ) ;
#33051 = EDGE_CURVE ( 'NONE', #91537, #11685, #1277, .T. ) ;
#33053 = CARTESIAN_POINT ( 'NONE',  ( 66.61587002248265321, 199.2677522451418213, -5.000000000000041744 ) ) ;
#33052 = CARTESIAN_POINT ( 'NONE',  ( 5.551812139918021138, 18.90829794293878408, 10.00000000000000355 ) ) ;
#33054 = EDGE_CURVE ( 'NONE', #34850, #6051, #28161, .T. ) ;
#33055 = CARTESIAN_POINT ( 'NONE',  ( 121.2656814440110367, 247.4865022471902876, -10.00000000000009592 ) ) ;
#33056 = CARTESIAN_POINT ( 'NONE',  ( 181.5287480975334802, 256.6865332137753626, 1.316448668424534452 ) ) ;
#33057 = CARTESIAN_POINT ( 'NONE',  ( 204.7237927799493775, 276.0549847173622879, -12.81020997223575364 ) ) ;
#33058 = CARTESIAN_POINT ( 'NONE',  ( 13.18854085237251184, 31.24736827225017066, 177.5919119679930134 ) ) ;
#33059 = ORIENTED_EDGE ( 'NONE', *, *, #63291, .F. ) ;
#33060 = VECTOR ( 'NONE', #26819, 1000.000000000000227 ) ;
#33061 = CARTESIAN_POINT ( 'NONE',  ( 36.90037335867700818, 182.1115022471902023, -5.000000000000041744 ) ) ;
#33062 = B_SPLINE_CURVE_WITH_KNOTS ( 'NONE', 3,
 ( #44747, #50866, #6266, #27090, #50370, #30057, #38654, #68061, #69558, #93397, #68556, #99482, #164, #47252, #46234, #39133, #60949, #31051, #77159, #91907, #37162, #22463, #98984, #54850, #15849, #53358, #46757, #61938, #61451, #92402 ),
 .UNSPECIFIED., .F., .F.,
 ( 4, 2, 2, 2, 2, 2, 2, 2, 2, 2, 2, 2, 2, 2, 4 ),
 ( 0.0007900407600501114895, 0.001551840822610036589, 0.001932740853890018654, 0.002313640885170001153, 0.003075440947729968753, 0.003456340979009963395, 0.003837241010289958038, 0.004218141041569941838, 0.004599041072849926505, 0.004979941104129911172, 0.005360841135409894972, 0.005741741166689878773, 0.006122641197969864307, 0.006503541229249848107, 0.006884441260529831907 ),
 .UNSPECIFIED. ) ;
#33063 = DIRECTION ( 'NONE',  ( 0.8660254037844387076, 0.4999999999999998890, 0.000000000000000000 ) ) ;
#33064 = CARTESIAN_POINT ( 'NONE',  ( 162.7561251957091031, 248.7451172484279027, 11.07313294959361194 ) ) ;
#33065 = CARTESIAN_POINT ( 'NONE',  ( -12.32793173735119652, 169.8149278399160664, 9.188101187500093303 ) ) ;
#33066 = CARTESIAN_POINT ( 'NONE',  ( 34.28181963472369631, 41.83396525600392835, -2.839279412974133887 ) ) ;
#33068 = CARTESIAN_POINT ( 'NONE',  ( 169.7667591601442041, 263.3286932583389444, 15.85558928611421159 ) ) ;
#33067 = DIRECTION ( 'NONE',  ( 0.5000000000000012212, -0.8660254037844379305, 0.000000000000000000 ) ) ;
#33069 = CARTESIAN_POINT ( 'NONE',  ( 192.1640094933931096, 297.8091675017319062, 12.36911124822534447 ) ) ;
#33070 = CARTESIAN_POINT ( 'NONE',  ( 30.35763184873497877, 26.03085787977764198, 9.188101187500006262 ) ) ;
#33071 = CARTESIAN_POINT ( 'NONE',  ( -72.81784413424504976, 47.52919789448971244, 10.00000000000000000 ) ) ;
#33072 = CIRCLE ( 'NONE', #31465, 0.1418229129684228651 ) ;
#33073 = CARTESIAN_POINT ( 'NONE',  ( 186.7082609234106485, 259.3128397857586265, -2.368698930973139216 ) ) ;
#33074 = CARTESIAN_POINT ( 'NONE',  ( 65.88310562884009869, 69.02589174572793240, 1.996831191910242609 ) ) ;
#33075 = ORIENTED_EDGE ( 'NONE', *, *, #62355, .T. ) ;
#33076 = FACE_OUTER_BOUND ( 'NONE', #20448, .T. ) ;
#33077 = DIRECTION ( 'NONE',  ( -0.5000000000000001110, 0.8660254037844385966, 0.000000000000000000 ) ) ;
#33078 = CARTESIAN_POINT ( 'NONE',  ( 7.601631632957884577, 27.49540643055185285, 3.479690158560446702E-15 ) ) ;
#33079 = CARTESIAN_POINT ( 'NONE',  ( 166.0359548300953350, 285.6250091532941724, 0.4950489585154529970 ) ) ;
#33080 = CARTESIAN_POINT ( 'NONE',  ( 19.25205234332785764, 23.06628583063841020, -9.188101187500006262 ) ) ;
#33081 = CARTESIAN_POINT ( 'NONE',  ( 206.9483995484939101, 272.2018527673814106, 9.530154192725417417 ) ) ;
#33082 = CARTESIAN_POINT ( 'NONE',  ( 17.41845772768865075, 33.55466486950699334, -1.111400068045478839E-16 ) ) ;
#33083 = CARTESIAN_POINT ( 'NONE',  ( 88.22249780726667723, 44.22164796532466369, -1.816046898853142855 ) ) ;
#33084 = VERTEX_POINT ( 'NONE', #36251 ) ;
#33085 = CARTESIAN_POINT ( 'NONE',  ( -16.76269525828470464, 104.2312461070085021, 43.89948692389422291 ) ) ;
#33086 = CARTESIAN_POINT ( 'NONE',  ( 207.6508796976096107, 270.9851214578045528, 6.713685698622268383 ) ) ;
#33088 = CARTESIAN_POINT ( 'NONE',  ( -12.68721568607400485, 24.67147432707382748, -10.00000000000000000 ) ) ;
#33087 = B_SPLINE_CURVE_WITH_KNOTS ( 'NONE', 3,
 ( #45072, #83117, #84615, #53658, #99297, #54149, #98807, #45562, #44560, #84133, #77492, #36973, #76011, #15156, #6589 ),
 .UNSPECIFIED., .F., .F.,
 ( 4, 2, 2, 2, 1, 2, 2, 4 ),
 ( 0.007447265025110824666, 0.1315163568969734964, 0.2555854487688362653, 0.5037236325125593606, 0.6277927243844221294, 0.6898272703203521816, 0.7518618162562823448, 1.000000000000000000 ),
 .UNSPECIFIED. ) ;
#33089 = CARTESIAN_POINT ( 'NONE',  ( 116.9873692804980010, 249.8967562850347122, -4.648177544792955347E-16 ) ) ;
#33090 = CARTESIAN_POINT ( 'NONE',  ( 193.8365934467825298, 294.9121671145370556, 14.14845633038902584 ) ) ;
#33091 = ORIENTED_EDGE ( 'NONE', *, *, #14525, .T. ) ;
#33092 = ORIENTED_EDGE ( 'NONE', *, *, #76401, .F. ) ;
#33093 = CARTESIAN_POINT ( 'NONE',  ( 156.2856527893789007, 276.9858201599269591, -10.11406258096672950 ) ) ;
#33094 = CARTESIAN_POINT ( 'NONE',  ( 86.30241807085522510, 47.23217017718856425, 10.82197119102028893 ) ) ;
#33095 = VERTEX_POINT ( 'NONE', #35763 ) ;
#33096 = CARTESIAN_POINT ( 'NONE',  ( 77.80689875040398817, 57.80620150817188829, 16.17428301622781461 ) ) ;
#33097 = CARTESIAN_POINT ( 'NONE',  ( 155.4968470730201204, 262.5308716345893458, -17.34543517382400424 ) ) ;
#33098 = ORIENTED_EDGE ( 'NONE', *, *, #73337, .T. ) ;
#33099 = CARTESIAN_POINT ( 'NONE',  ( 78.39455052809223901, 61.40085115147536499, -15.85312059573208998 ) ) ;
#33100 = CARTESIAN_POINT ( 'NONE',  ( 79.05300200689268308, 59.41537015362479224, -16.53193985632130847 ) ) ;
#33101 = B_SPLINE_CURVE_WITH_KNOTS ( 'NONE', 3,
 ( #4834, #51921, #89475, #52403, #35715, #81369, #97544, #11937, #43301, #73727 ),
 .UNSPECIFIED., .F., .F.,
 ( 4, 2, 2, 2, 4 ),
 ( 0.000000000000000000, 0.2500000000000000000, 0.5000000000000000000, 0.7500000000000000000, 1.000000000000000000 ),
 .UNSPECIFIED. ) ;
#33102 = CARTESIAN_POINT ( 'NONE',  ( -66.21217304253431735, 40.79406095866392690, 10.00000000000000000 ) ) ;
#33103 = VERTEX_POINT ( 'NONE', #4365 ) ;
#33104 = CARTESIAN_POINT ( 'NONE',  ( 161.8811854682448939, 250.2605573099562264, 13.51112293479948789 ) ) ;
#33105 = CARTESIAN_POINT ( 'NONE',  ( 166.1269882802908171, 273.9879501969531930, -15.27021006158703287 ) ) ;
#33106 = FACE_OUTER_BOUND ( 'NONE', #14725, .T. ) ;
#33107 = DIRECTION ( 'NONE',  ( 0.000000000000000000, 0.000000000000000000, 1.000000000000000000 ) ) ;
#33108 = ORIENTED_EDGE ( 'NONE', *, *, #47274, .T. ) ;
#33109 = CARTESIAN_POINT ( 'NONE',  ( 171.1037398668862579, 254.7221107261599684, -11.48652484307285881 ) ) ;
#33110 = CARTESIAN_POINT ( 'NONE',  ( 202.9972156839127990, 279.0455039708822937, 16.77197898838388213 ) ) ;
#33111 = ORIENTED_EDGE ( 'NONE', *, *, #56810, .F. ) ;
#33112 = ORIENTED_EDGE ( 'NONE', *, *, #43878, .F. ) ;
#33113 = CARTESIAN_POINT ( 'NONE',  ( 156.7891510251116927, 266.6197213971674955, -16.22205799199115361 ) ) ;
#33114 = ORIENTED_EDGE ( 'NONE', *, *, #70740, .F. ) ;
#33115 = CARTESIAN_POINT ( 'NONE',  ( -17.81126293257622706, 23.08927765589692527, -10.00000000000000000 ) ) ;
#33116 = VERTEX_POINT ( 'NONE', #80929 ) ;
#33117 = CARTESIAN_POINT ( 'NONE',  ( 77.56105267981614304, 49.72783448595330924, -15.46007777815280981 ) ) ;
#33118 = CARTESIAN_POINT ( 'NONE',  ( 17.60357497223980516, 35.28838536716092023, 10.00000000000000000 ) ) ;
#33119 = CARTESIAN_POINT ( 'NONE',  ( 70.82976944384030560, 68.20446162899281717, 9.207867830786081953 ) ) ;
#33120 = CARTESIAN_POINT ( 'NONE',  ( 25.96864935082050252, 154.0458036431183189, -30.52142883766499892 ) ) ;
#33121 = EDGE_CURVE ( 'NONE', #11929, #63370, #5368, .T. ) ;
#33122 = CARTESIAN_POINT ( 'NONE',  ( 174.5758580735184182, 290.0543502012598651, 6.328980342067771936 ) ) ;
#33123 = CARTESIAN_POINT ( 'NONE',  ( -19.78867382312482803, 93.10677061150157385, 59.99999999999999289 ) ) ;
#33124 = ORIENTED_EDGE ( 'NONE', *, *, #3471, .F. ) ;
#33125 = CARTESIAN_POINT ( 'NONE',  ( -61.60412911085353471, 37.02832515102500111, 10.00000000000000000 ) ) ;
#33126 = CARTESIAN_POINT ( 'NONE',  ( 15.27916758686040488, 29.79752408145592568, -5.678558825948271327 ) ) ;
#33127 = CARTESIAN_POINT ( 'NONE',  ( 206.0691053506789387, 273.7248349927971844, 11.70564474658248422 ) ) ;
#33128 = CARTESIAN_POINT ( 'NONE',  ( 190.9810003742392439, 298.2187262335144737, -9.520436992407670829 ) ) ;
#33130 = VERTEX_POINT ( 'NONE', #97114 ) ;
#33129 = CARTESIAN_POINT ( 'NONE',  ( 207.0261077644705097, 271.6721741260535623, 5.334318399223184848 ) ) ;
#33131 = ORIENTED_EDGE ( 'NONE', *, *, #27020, .F. ) ;
#33132 = CARTESIAN_POINT ( 'NONE',  ( 169.0033239945426260, 257.7505650133988411, -14.14853767920301131 ) ) ;
#33133 = CARTESIAN_POINT ( 'NONE',  ( 45.00959873851216031, 26.39040679176986970, 1.333680081654574804E-15 ) ) ;
#33134 = EDGE_CURVE ( 'NONE', #27844, #74106, #58551, .T. ) ;
#33135 = DIRECTION ( 'NONE',  ( -0.8916269620120450545, 0.4527707594502665689, 0.000000000000000000 ) ) ;
#33136 = ADVANCED_FACE ( 'NONE', ( #34270 ), #50459, .F. ) ;
#33137 = AXIS2_PLACEMENT_3D ( 'NONE', #66521, #89863, #97448 ) ;
#33138 = CARTESIAN_POINT ( 'NONE',  ( 200.1385401540174769, 283.9968752310148830, 17.30012534137638625 ) ) ;
#33139 = CARTESIAN_POINT ( 'NONE',  ( 109.6465072765698210, 234.1115022471902307, 10.00000000000009592 ) ) ;
#33140 = EDGE_LOOP ( 'NONE', ( #23224, #13788, #13221, #33906 ) ) ;
#33141 = CARTESIAN_POINT ( 'NONE',  ( 152.5864982446449005, 269.4261691430817791, 15.31489403458886400 ) ) ;
#33142 = CARTESIAN_POINT ( 'NONE',  ( 5.867642952189432215, 25.16126292948893450, -6.180339887498951690 ) ) ;
#33143 = CARTESIAN_POINT ( 'NONE',  ( -15.09704997274537597, 40.23729735856676371, 59.99999999999999289 ) ) ;
#33144 = CARTESIAN_POINT ( 'NONE',  ( 164.3706594650489023, 245.9486618633701482, -1.665857659249071698 ) ) ;
#33145 = CARTESIAN_POINT ( 'NONE',  ( 13.35530768973961457, 178.5177522451418497, -10.00000000000009592 ) ) ;
#33146 = CARTESIAN_POINT ( 'NONE',  ( 90.05242219234915524, 231.9869531367911293, 4.594050593750046652 ) ) ;
#33147 = AXIS2_PLACEMENT_3D ( 'NONE', #94291, #32944, #3570 ) ;
#33148 = CARTESIAN_POINT ( 'NONE',  ( 82.39049329420826950, 40.94913840096306501, -1.238713965289769181 ) ) ;
#33149 = CARTESIAN_POINT ( 'NONE',  ( 22.75701074986381656, 14.10801979619928659, 3.090169943749476733 ) ) ;
#33150 = CARTESIAN_POINT ( 'NONE',  ( 162.9529104326093716, 248.4042752199367214, 11.77079043123004176 ) ) ;
#33151 = CARTESIAN_POINT ( 'NONE',  ( 2.773212693257451900, 184.6589784336661637, -6.496448406907675876E-16 ) ) ;
#33152 = CARTESIAN_POINT ( 'NONE',  ( 184.1438436585225134, 256.9788754071735184, 3.690260418413948251 ) ) ;
#33153 = ORIENTED_EDGE ( 'NONE', *, *, #54078, .T. ) ;
#33155 = ORIENTED_EDGE ( 'NONE', *, *, #27698, .F. ) ;
#33154 = UNCERTAINTY_MEASURE_WITH_UNIT (LENGTH_MEASURE( 1.000000000000000082E-05 ), #20316, 'distance_accuracy_value', 'NONE');
#33156 = CARTESIAN_POINT ( 'NONE',  ( 199.0331857822236543, 266.6627783094973552, -2.856755361176172681 ) ) ;
#33157 = CARTESIAN_POINT ( 'NONE',  ( 184.6303280917163363, 262.2872244324082089, 12.09539929678677517 ) ) ;
#33158 = CARTESIAN_POINT ( 'NONE',  ( 164.4568492923521887, 247.7993767033852919, 8.703614106482779889 ) ) ;
#33159 = CARTESIAN_POINT ( 'NONE',  ( 161.6755750489535046, 250.6166850027345276, -13.01404233079112061 ) ) ;
#33160 = DIRECTION ( 'NONE',  ( -0.000000000000000000, -0.000000000000000000, 1.000000000000000000 ) ) ;
#33161 = CARTESIAN_POINT ( 'NONE',  ( 74.21927401529055146, 68.62113723208385352, -11.51360559050239374 ) ) ;
#33162 = EDGE_CURVE ( 'NONE', #14526, #48417, #81409, .T. ) ;
#33163 = CARTESIAN_POINT ( 'NONE',  ( 33.89617418964321871, 196.5024278399160949, -9.188101187500093303 ) ) ;
#33164 = CARTESIAN_POINT ( 'NONE',  ( 75.63696797857046761, 221.1427522451418781, -10.00000000000009415 ) ) ;
#33165 = CARTESIAN_POINT ( 'NONE',  ( 196.3340813134408052, 275.6274763521643649, 15.39790310608117174 ) ) ;
#33166 = ORIENTED_EDGE ( 'NONE', *, *, #41313, .T. ) ;
#33167 = CARTESIAN_POINT ( 'NONE',  ( 82.63346302021976442, 44.24771747269379318, 9.093021782927767305 ) ) ;
#33168 = ADVANCED_FACE ( 'NONE', ( #89522 ), #35261, .F. ) ;
#33169 = ADVANCED_FACE ( 'NONE', ( #20083 ), #89049, .T. ) ;
#33170 = CARTESIAN_POINT ( 'NONE',  ( 175.2303977473730470, 281.2452381793661402, -14.37900534504002081 ) ) ;
#33171 = AXIS2_PLACEMENT_3D ( 'NONE', #24229, #84080, #46505 ) ;
#33172 = DIRECTION ( 'NONE',  ( 0.5242119900219359696, 0.000000000000000000, -0.8515878049368965641 ) ) ;
#33173 = EDGE_CURVE ( 'NONE', #97169, #73589, #14365, .T. ) ;
#33174 = CARTESIAN_POINT ( 'NONE',  ( 69.11330294371380489, 64.33813860942547080, -11.97090107321349883 ) ) ;
#33175 = CARTESIAN_POINT ( 'NONE',  ( 207.1432938686257046, 271.8642859028066141, -6.405155839440290322 ) ) ;
#33176 = LINE ( 'NONE', #55449, #40226 ) ;
#33177 = CARTESIAN_POINT ( 'NONE',  ( 194.3011251241114508, 294.1075746476782342, -14.76047579547631905 ) ) ;
#33178 = EDGE_CURVE ( 'NONE', #63052, #28914, #98075, .T. ) ;
#33179 = ADVANCED_FACE ( 'NONE', ( #57555 ), #91714, .F. ) ;
#33180 = CARTESIAN_POINT ( 'NONE',  ( -48.47243291925848752, 30.64988553008148031, 10.00000000000000000 ) ) ;
#33181 = CARTESIAN_POINT ( 'NONE',  ( 204.8189571845487080, 275.8901551335242175, 13.43702398685204358 ) ) ;
#33182 = CARTESIAN_POINT ( 'NONE',  ( 146.8637854207107409, 276.2714571898724216, 0.7988785540157756770 ) ) ;
#33183 = CARTESIAN_POINT ( 'NONE',  ( 207.4826643481121664, 271.2764789897469768, 7.783310782367018454 ) ) ;
#33184 = VERTEX_POINT ( 'NONE', #92004 ) ;
#33185 = CARTESIAN_POINT ( 'NONE',  ( 181.1381746692000831, 268.2224384537198034, 15.93641414596886463 ) ) ;
#33186 = CARTESIAN_POINT ( 'NONE',  ( 108.5637151982415389, 242.6744531367911293, 4.594050593750047540 ) ) ;
#33187 = CARTESIAN_POINT ( 'NONE',  ( 19.96532700332172183, 20.03085787977762422, 9.188101187500006262 ) ) ;
#33188 = CARTESIAN_POINT ( 'NONE',  ( 75.15246256102729205, 67.05878861674010238, 13.14576163508979612 ) ) ;
#33189 = CARTESIAN_POINT ( 'NONE',  ( 83.53204454370724363, 52.39401912150450613, -15.17729711222452416 ) ) ;
#33191 = DIRECTION ( 'NONE',  ( 1.804112415015878984E-15, -1.000000000000000000, 0.000000000000000000 ) ) ;
#33190 = CARTESIAN_POINT ( 'NONE',  ( 195.7578697689113199, 291.5844189092309193, 17.18796537138345215 ) ) ;
#33192 = CARTESIAN_POINT ( 'NONE',  ( 204.4580234391050624, 272.8508129992514455, -9.749047436841882686 ) ) ;
#33193 = CARTESIAN_POINT ( 'NONE',  ( 190.1696732520942135, 261.0657627445133357, -4.620374468803995605 ) ) ;
#33194 = CARTESIAN_POINT ( 'NONE',  ( 148.9285945872975390, 272.6951028054104427, -12.01265727652413240 ) ) ;
#33195 = CARTESIAN_POINT ( 'NONE',  ( 190.2514126175606464, 263.1309047876983414, 9.365642484728958550 ) ) ;
#33196 = CARTESIAN_POINT ( 'NONE',  ( 175.7360147442049083, 291.5370265259801386, -1.082392496102676738 ) ) ;
#33197 = CARTESIAN_POINT ( 'NONE',  ( 194.6820509838467785, 270.8910309865917156, -14.27696746312268239 ) ) ;
#33198 = EDGE_LOOP ( 'NONE', ( #25733, #77587, #22775, #79739, #56495, #36582, #55111, #36069, #7694, #31337, #45527, #82540, #98652, #67839, #27397, #30273, #79920, #95360, #59899, #8301 ) ) ;
#33199 = CARTESIAN_POINT ( 'NONE',  ( 189.2480760824234096, 265.7019095893114127, 10.75718835852465283 ) ) ;
#33200 = CARTESIAN_POINT ( 'NONE',  ( 176.0605106315991293, 278.7961450278489224, 15.46843456374776338 ) ) ;
#33201 = CARTESIAN_POINT ( 'NONE',  ( 165.5220966049394349, 269.3702310919443335, -16.46924383601979258 ) ) ;
#33202 = CARTESIAN_POINT ( 'NONE',  ( 71.90400658755808649, 72.53437165389429708, 1.750395423964768993 ) ) ;
#33203 = CARTESIAN_POINT ( 'NONE',  ( 200.1971017585360926, 272.2107728627942720, 12.83095891089018536 ) ) ;
#33204 = CIRCLE ( 'NONE', #99535, 70.00000000000001421 ) ;
#33205 = DIRECTION ( 'NONE',  ( -0.5000000000000002220, 0.8660254037844385966, 0.000000000000000000 ) ) ;
#33206 = CARTESIAN_POINT ( 'NONE',  ( -15.31269525828471068, 104.2312461070085021, 36.50000000000000000 ) ) ;
#33207 = CARTESIAN_POINT ( 'NONE',  ( 148.1271767189874424, 275.1914202840015378, 5.919243137104419183 ) ) ;
#33208 = ORIENTED_EDGE ( 'NONE', *, *, #44744, .F. ) ;
#33209 = CARTESIAN_POINT ( 'NONE',  ( 190.8416422453866232, 280.8388896373550097, 16.64352526479659744 ) ) ;
#33210 = B_SPLINE_SURFACE_WITH_KNOTS ( 'NONE', 3, 1, ( 
 ( #84070, #100236 ),
 ( #52110, #45004 ),
 ( #30820, #21718 ),
 ( #23202, #60691 ),
 ( #45502, #38401 ),
 ( #83559, #90675 ),
 ( #76435, #21231 ),
 ( #37402, #91649 ),
 ( #92172, #74940 ),
 ( #61700, #22216 ),
 ( #14123, #61205 ),
 ( #54093, #75950 ),
 ( #6526, #68308 ),
 ( #99231, #53113 ),
 ( #5524, #7010 ),
 ( #37895, #99731 ),
 ( #22722, #53601 ),
 ( #78947, #79463 ),
 ( #71838, #1925 ),
 ( #54591, #15596 ),
 ( #78434, #32811 ),
 ( #25732, #10027 ),
 ( #56093, #8030 ),
 ( #16611, #39887 ),
 ( #87086, #64213 ),
 ( #63716, #17107 ),
 ( #95164, #17622 ),
 ( #9015, #38903 ),
 ( #920, #23696 ),
 ( #63213, #24220 ),
 ( #48003, #85573 ),
 ( #71333, #93655 ),
 ( #62698, #94155 ),
 ( #55100, #33314 ) ),
 .UNSPECIFIED., .T., .F., .F.,
 ( 4, 2, 2, 2, 2, 2, 2, 2, 2, 2, 2, 2, 2, 2, 2, 2, 4 ),
 ( 2, 2 ),
 ( 0.000000000000000000, 0.06250000000000000000, 0.1250000000000000000, 0.1875000000000000000, 0.2500000000000000000, 0.3125000000000000000, 0.3750000000000000000, 0.4375000000000000000, 0.5000000000000000000, 0.5625000000000000000, 0.6250000000000000000, 0.6875000000000000000, 0.7500000000000000000, 0.8125000000000000000, 0.8750000000000000000, 0.9375000000000000000, 1.000000000000000000 ),
 ( 0.000000000000000000, 1.000000000000000000 ),
 .UNSPECIFIED. ) ;
#33211 = CARTESIAN_POINT ( 'NONE',  ( 43.73469409959700016, 27.11110640527295956, -2.839279412974138328 ) ) ;
#33212 = CARTESIAN_POINT ( 'NONE',  ( 195.3690366949981296, 290.3742493059416461, -16.73554728058864427 ) ) ;
#33213 = ORIENTED_EDGE ( 'NONE', *, *, #97554, .T. ) ;
#33214 = CARTESIAN_POINT ( 'NONE',  ( 164.8655127169167827, 279.6105928571379309, 11.86288285680936383 ) ) ;
#33215 = EDGE_CURVE ( 'NONE', #24657, #13582, #23529, .T. ) ;
#33216 = CARTESIAN_POINT ( 'NONE',  ( 147.8163551302855296, 274.6215580551378821, -9.286329195885331345 ) ) ;
#33217 = CARTESIAN_POINT ( 'NONE',  ( 108.1850894041355957, 243.2677522451419065, -5.000000000000047962 ) ) ;
#33218 = ORIENTED_EDGE ( 'NONE', *, *, #54019, .T. ) ;
#33219 = CARTESIAN_POINT ( 'NONE',  ( 79.29399852950436411, 59.91530550262321242, 16.14991020500348284 ) ) ;
#33220 = DIRECTION ( 'NONE',  ( -0.2837547813814349507, -0.9281390619545439868, -0.2409172175609568534 ) ) ;
#33221 = DIRECTION ( 'NONE',  ( 0.000000000000000000, 0.000000000000000000, 1.000000000000000000 ) ) ;
#33222 = CARTESIAN_POINT ( 'NONE',  ( 75.20389695419315501, 52.88180760346911313, -15.99093876381489920 ) ) ;
#33223 = CARTESIAN_POINT ( 'NONE',  ( 154.8833801513861772, 262.3811116602312268, -17.49275566389638215 ) ) ;
#33224 = ORIENTED_EDGE ( 'NONE', *, *, #30034, .F. ) ;
#33225 = VERTEX_POINT ( 'NONE', #45825 ) ;
#33226 = LINE ( 'NONE', #65127, #12505 ) ;
#33227 = ORIENTED_EDGE ( 'NONE', *, *, #79064, .F. ) ;
#33228 = CARTESIAN_POINT ( 'NONE',  ( 77.34702598425042197, 49.11609959051940422, -15.28751209942174860 ) ) ;
#33229 = VERTEX_POINT ( 'NONE', #53923 ) ;
#33230 = LINE ( 'NONE', #79880, #60530 ) ;
#33231 = CARTESIAN_POINT ( 'NONE',  ( 78.67033018268951139, 50.72589383312638489, 15.10119772252972403 ) ) ;
#33232 = ORIENTED_EDGE ( 'NONE', *, *, #30852, .T. ) ;
#33233 = CARTESIAN_POINT ( 'NONE',  ( 164.8012313184158018, 245.2028895370295913, -2.462952685407667097 ) ) ;
#33234 = CARTESIAN_POINT ( 'NONE',  ( 147.6842102149426239, 274.8504397624737408, -5.874512262071210245 ) ) ;
#33235 = LINE ( 'NONE', #92581, #73897 ) ;
#33236 = CARTESIAN_POINT ( 'NONE',  ( 192.4663556654298588, 297.2854885702906245, -12.98646995774174684 ) ) ;
#33237 = CARTESIAN_POINT ( 'NONE',  ( 152.8328714238065515, 265.9326969577624027, -16.29536156676786263 ) ) ;
#33238 = CARTESIAN_POINT ( 'NONE',  ( -25.62627769214124740, 24.57763045674671432, -10.00000000000000000 ) ) ;
#33240 = EDGE_CURVE ( 'NONE', #14896, #38420, #32491, .T. ) ;
#33239 = B_SPLINE_CURVE_WITH_KNOTS ( 'NONE', 3,
 ( #83361, #68613, #30624, #36714, #53895, #98550, #44313, #7821, #17808, #48709, #75500, #12711, #28895, #66879, #44064, #52669, #36475, #74516, #6084, #6593, #60753, #22279, #37959, #52173, #45076, #13691, #89738, #83626, #36977, #45567, #68867 ),
 .UNSPECIFIED., .F., .F.,
 ( 4, 3, 3, 3, 3, 3, 3, 3, 3, 3, 4 ),
 ( 0.000000000000000000, 0.1333490885032321271, 0.3007194338854310423, 0.4699862290245110930, 0.5844252810809297261, 0.6686540514502729016, 0.7354980260655470392, 0.8028463152565559202, 0.8633854507757028340, 0.9437142632666930542, 1.000000000000000000 ),
 .UNSPECIFIED. ) ;
#33241 = CARTESIAN_POINT ( 'NONE',  ( 154.0522741418830606, 280.1392850030782711, 2.230978122590827617 ) ) ;
#33242 = CARTESIAN_POINT ( 'NONE',  ( 128.2389901622930495, 244.8458772461660544, 9.188101187500095079 ) ) ;
#33243 = ORIENTED_EDGE ( 'NONE', *, *, #57359, .T. ) ;
#33244 = CARTESIAN_POINT ( 'NONE',  ( 70.79441317036970815, 61.10405584021994940, -14.44842289594245166 ) ) ;
#33245 = CARTESIAN_POINT ( 'NONE',  ( 5.396842180905148112, 18.51421378149916563, -9.188101187500004485 ) ) ;
#33246 = ORIENTED_EDGE ( 'NONE', *, *, #88434, .T. ) ;
#33247 = VECTOR ( 'NONE', #45336, 1000.000000000000000 ) ;
#33249 = ORIENTED_EDGE ( 'NONE', *, *, #74474, .F. ) ;
#33248 = CARTESIAN_POINT ( 'NONE',  ( 85.67146519243034675, 48.43225591334719837, -12.22341872913517591 ) ) ;
#33250 = CARTESIAN_POINT ( 'NONE',  ( 203.5065352982886111, 276.4905705151080042, 13.85652113363879323 ) ) ;
#33251 = CARTESIAN_POINT ( 'NONE',  ( 177.6229113889583573, 253.4088548334622146, 1.384122540242602950 ) ) ;
#33252 = CARTESIAN_POINT ( 'NONE',  ( 172.9134852821738093, 290.3302075368507076, -5.008290383854661521 ) ) ;
#33253 = CARTESIAN_POINT ( 'NONE',  ( 146.8702612584350220, 276.2602407099124662, 4.074116067346697179 ) ) ;
#33254 = CARTESIAN_POINT ( 'NONE',  ( 156.0507216674837707, 279.5060275253360373, 7.618106348741741307 ) ) ;
#33255 = ADVANCED_FACE ( 'NONE', ( #71171 ), #54940, .F. ) ;
#33256 = CARTESIAN_POINT ( 'NONE',  ( 164.0241303531365702, 249.6968001490059237, 11.40766388789279517 ) ) ;
#33257 = CARTESIAN_POINT ( 'NONE',  ( 79.58936028502597537, 59.22294857574252802, 16.56770033466462166 ) ) ;
#33258 = CARTESIAN_POINT ( 'NONE',  ( 171.8643346617544125, 280.1325139634143966, 13.88504993119007125 ) ) ;
#33259 = ADVANCED_FACE ( 'NONE', ( #2268 ), #70699, .F. ) ;
#33260 = CARTESIAN_POINT ( 'NONE',  ( 177.1425110050965088, 256.0051583568908313, -7.288962701963175306 ) ) ;
#33261 = VERTEX_POINT ( 'NONE', #28531 ) ;
#33262 = CARTESIAN_POINT ( 'NONE',  ( 194.3177355571849318, 294.0788045336591381, -15.93712594727561616 ) ) ;
#33263 = CARTESIAN_POINT ( 'NONE',  ( 152.6922851986468572, 273.5033374046732888, 11.91467210813521582 ) ) ;
#33264 = VERTEX_POINT ( 'NONE', #58433 ) ;
#33265 = CARTESIAN_POINT ( 'NONE',  ( 163.9394958709336549, 277.9080926337546771, 13.13436882728932886 ) ) ;
#33266 = CARTESIAN_POINT ( 'NONE',  ( 205.1070472173078940, 268.9988147858434786, -3.031129214391079518 ) ) ;
#33267 = CARTESIAN_POINT ( 'NONE',  ( 192.1051365471491579, 297.9111384358179180, -10.71776918011019220 ) ) ;
#33268 = CARTESIAN_POINT ( 'NONE',  ( -59.87889494062799400, 37.30571521936384016, -10.00000000000000000 ) ) ;
#33269 = CARTESIAN_POINT ( 'NONE',  ( 162.8789161433191452, 248.5324370884573568, 9.731756914259689140 ) ) ;
#33271 = CARTESIAN_POINT ( 'NONE',  ( 151.6355143709362494, 275.0870865548936877, -8.630920780667789671 ) ) ;
#33270 = CARTESIAN_POINT ( 'NONE',  ( 153.5196858120735044, 269.9415063994401294, 14.50335029241602491 ) ) ;
#33272 = CARTESIAN_POINT ( 'NONE',  ( 201.0356089830534643, 282.4431064412383989, -18.18835788025466371 ) ) ;
#33273 = ORIENTED_EDGE ( 'NONE', *, *, #31734, .F. ) ;
#33274 = VECTOR ( 'NONE', #57743, 1000.000000000000114 ) ;
#33275 = CARTESIAN_POINT ( 'NONE',  ( 12.39361081041026580, 166.4155109091896065, 2.679491924311254714 ) ) ;
#33276 = CARTESIAN_POINT ( 'NONE',  ( 78.41477381122238910, 47.32040575024743134, -14.22103711499937617 ) ) ;
#33277 = CARTESIAN_POINT ( 'NONE',  ( 73.38945809345867133, 65.55744267816019999, -12.97487857549163870 ) ) ;
#33278 = VECTOR ( 'NONE', #88669, 1000.000000000000114 ) ;
#33279 = CARTESIAN_POINT ( 'NONE',  ( 192.0963028965829551, 297.9264387674147656, 11.34530024772836754 ) ) ;
#33280 = DIRECTION ( 'NONE',  ( -0.000000000000000000, -0.000000000000000000, -1.000000000000000000 ) ) ;
#33281 = CARTESIAN_POINT ( 'NONE',  ( 155.6126298223767890, 261.1180141786725244, 18.15400560664037855 ) ) ;
#33282 = EDGE_CURVE ( 'NONE', #68650, #83827, #50594, .T. ) ;
#33283 = CARTESIAN_POINT ( 'NONE',  ( -10.94779052401099051, 173.6744531367911293, 4.594050593750047540 ) ) ;
#33284 = CARTESIAN_POINT ( 'NONE',  ( 94.73480590126506229, 219.3768266524160140, 9.188101187500098632 ) ) ;
#33285 = CARTESIAN_POINT ( 'NONE',  ( 155.2922060645262263, 261.6730044072216401, -16.98884022075611355 ) ) ;
#33286 = CARTESIAN_POINT ( 'NONE',  ( 88.19523698511710563, 44.46804064255652378, -4.670053027270656187 ) ) ;
#33287 = CARTESIAN_POINT ( 'NONE',  ( 47.78135487164288264, 106.4364430393875267, -10.00000000000000000 ) ) ;
#33288 = DIRECTION ( 'NONE',  ( 0.4996954135095463823, -0.8654978445076774163, -0.03489949670249753444 ) ) ;
#33289 = CARTESIAN_POINT ( 'NONE',  ( 77.63260553344707660, 52.78140009998875115, 15.78914038458534641 ) ) ;
#33290 = CARTESIAN_POINT ( 'NONE',  ( 162.1709154337574716, 282.3874689244844376, 5.612144347381637033 ) ) ;
#33292 = CARTESIAN_POINT ( 'NONE',  ( 76.48237539624216197, 51.57453071699011105, 15.64553330800477404 ) ) ;
#33291 = CARTESIAN_POINT ( 'NONE',  ( 67.49618919058045208, 67.03867160555277849, 8.996887788448240997 ) ) ;
#33293 = CARTESIAN_POINT ( 'NONE',  ( 161.9199371792244619, 250.1934373776594214, 14.05412690039883827 ) ) ;
#33294 = ADVANCED_FACE ( 'NONE', ( #41740 ), #3763, .T. ) ;
#33295 = DIRECTION ( 'NONE',  ( -0.9682419296822714072, -0.2500151307524235422, 0.000000000000000000 ) ) ;
#33296 = CARTESIAN_POINT ( 'NONE',  ( 167.0271109968743417, 287.8086958075197686, 0.5416428030073258126 ) ) ;
#33297 = CARTESIAN_POINT ( 'NONE',  ( 187.3225869936034371, 268.9281182169409590, 15.57271238421296289 ) ) ;
#33298 = CARTESIAN_POINT ( 'NONE',  ( -19.65312891409030271, 93.06504152958497400, 10.00000000000000888 ) ) ;
#33299 = CARTESIAN_POINT ( 'NONE',  ( 207.8431546909062320, 270.6520914003897360, -6.441273666418043220 ) ) ;
#33300 = CARTESIAN_POINT ( 'NONE',  ( 66.37865437376702005, 68.04852424368543495, -4.838310726055023991 ) ) ;
#33301 = CARTESIAN_POINT ( 'NONE',  ( 50.26990084964904071, 190.6423013555410080, -4.594050593750043987 ) ) ;
#33302 = CARTESIAN_POINT ( 'NONE',  ( 76.91165928263828278, 63.32913628365751180, -15.47028109333149715 ) ) ;
#33303 = CARTESIAN_POINT ( 'NONE',  ( 66.20992061623260838, 209.0333772461660544, 9.188101187500095079 ) ) ;
#33304 = CARTESIAN_POINT ( 'NONE',  ( 161.2133744761260061, 251.4172398781588811, -14.30368667312104058 ) ) ;
#33305 = CARTESIAN_POINT ( 'NONE',  ( 83.88838745027602783, 50.86303177257806141, -14.42977140412262216 ) ) ;
#33306 = CARTESIAN_POINT ( 'NONE',  ( 106.6154183633243377, 222.3615022471902023, 5.000000000000051514 ) ) ;
#33308 = CARTESIAN_POINT ( 'NONE',  ( 200.2812248566589801, 283.7497380765769890, 17.06302258474581990 ) ) ;
#33307 = CARTESIAN_POINT ( 'NONE',  ( 83.33117328246518696, 42.97812013064149284, -7.544556126886196701 ) ) ;
#33309 = EDGE_CURVE ( 'NONE', #29501, #90465, #27567, .T. ) ;
#33310 = LINE ( 'NONE', #95161, #10516 ) ;
#33311 = VECTOR ( 'NONE', #3979, 1000.000000000000114 ) ;
#33312 = CARTESIAN_POINT ( 'NONE',  ( 31.76189289227714951, 20.19860640527293683, 2.839279412974134775 ) ) ;
#33313 = CARTESIAN_POINT ( 'NONE',  ( 110.0000000000000000, 15.00000000000000000, 9.212605237762131694 ) ) ;
#33314 = CARTESIAN_POINT ( 'NONE',  ( 149.2923684163597784, 272.0650280510108701, -12.99082738998495756 ) ) ;
#33315 = VERTEX_POINT ( 'NONE', #12361 ) ;
#33316 = CARTESIAN_POINT ( 'NONE',  ( 19.25205234332785764, 23.06628583063841020, -9.188101187500006262 ) ) ;
#33317 = CARTESIAN_POINT ( 'NONE',  ( 81.74442484449845381, 211.8768266524160140, 9.188101187500096856 ) ) ;
#33318 = CARTESIAN_POINT ( 'NONE',  ( 76.60814547930165475, 63.80470055869116663, 14.86801040537077867 ) ) ;
#33319 = CARTESIAN_POINT ( 'NONE',  ( 170.0999411130123633, 288.2716680735795194, -1.080197458295449442 ) ) ;
#33320 = DIRECTION ( 'NONE',  ( 0.000000000000000000, 0.000000000000000000, 1.000000000000000000 ) ) ;
#33321 = CARTESIAN_POINT ( 'NONE',  ( 153.6322440704845178, 264.5481429195353371, 18.09763679434087180 ) ) ;
#33322 = ORIENTED_EDGE ( 'NONE', *, *, #30542, .T. ) ;
#33323 =( BOUNDED_CURVE ( )  B_SPLINE_CURVE ( 2, ( #42452, #88638, #51053, #19695, #81511, #12081, #80520, #65759, #27281, #20186, #27775, #4985, #73386 ),
 .UNSPECIFIED., .F., .T. ) 
 B_SPLINE_CURVE_WITH_KNOTS ( ( 3, 2, 2, 2, 2, 2, 3 ),
 ( 0.1625000000000000056, 0.1650000000000000078, 0.1700000000000000122, 0.1749999999999999889, 0.1799999999999999933, 0.1849999999999999978, 0.1875000000000000000 ),
 .UNSPECIFIED. ) 
 CURVE ( )  GEOMETRIC_REPRESENTATION_ITEM ( )  RATIONAL_B_SPLINE_CURVE ( ( 0.9755282581475768211, 0.9755282581475768211, 1.000000000000000000, 0.9510565162951535312, 1.000000000000000000, 0.9510565162951535312, 1.000000000000000000, 0.9510565162951535312, 1.000000000000000000, 0.9510565162951535312, 1.000000000000000000, 0.9755282581475768211, 0.9755282581475768211 ) ) 
 REPRESENTATION_ITEM ( '' )  );
#33324 = AXIS2_PLACEMENT_3D ( 'NONE', #86167, #1522, #79036 ) ;
#33325 = CARTESIAN_POINT ( 'NONE',  ( 86.67919437798869353, 47.13106718819364716, 10.49222478779208068 ) ) ;
#33326 = CARTESIAN_POINT ( 'NONE',  ( 190.1285921677634008, 286.6309046793794550, 16.34626960247791772 ) ) ;
#33327 = CARTESIAN_POINT ( 'NONE',  ( 121.4100190113083784, 254.2365022471903728, 2.944929066748280225E-16 ) ) ;
#33328 = CARTESIAN_POINT ( 'NONE',  ( 12.05626958406292104, 187.7677522451419065, -5.000000000000047962 ) ) ;
#33329 = B_SPLINE_CURVE_WITH_KNOTS ( 'NONE', 3,
 ( #52736, #6661, #29951, #4673, #37539, #5169, #35564, #59848, #36048, #66951, #66464, #97880, #28453, #91289 ),
 .UNSPECIFIED., .F., .F.,
 ( 4, 2, 2, 2, 2, 2, 4 ),
 ( 0.0008442750654606336752, 0.001116754662652982583, 0.001389234259845331275, 0.001661713857037679966, 0.001934193454230028874, 0.002479152648614570999, 0.003024111842999113123 ),
 .UNSPECIFIED. ) ;
#33330 = CARTESIAN_POINT ( 'NONE',  ( 75.35067983306640826, 53.14245299146813295, 16.48596124111078609 ) ) ;
#33331 = EDGE_LOOP ( 'NONE', ( #20526, #97120, #63604, #34699 ) ) ;
#33332 = CARTESIAN_POINT ( 'NONE',  ( 187.4913029195216438, 273.0290542173935933, 15.64619952351353760 ) ) ;
#33333 = VERTEX_POINT ( 'NONE', #43227 ) ;
#33334 = CARTESIAN_POINT ( 'NONE',  ( 163.4216610345155800, 247.5923753613567442, 10.58669027323842826 ) ) ;
#33335 = DIRECTION ( 'NONE',  ( -0.9997524133706772176, 0.02225111142182466945, 0.000000000000000000 ) ) ;
#33336 = CARTESIAN_POINT ( 'NONE',  ( 201.4066285247549786, 281.8004817444100354, -17.79749223817309201 ) ) ;
#33337 = VERTEX_POINT ( 'NONE', #74169 ) ;
#33338 = FACE_OUTER_BOUND ( 'NONE', #66485, .T. ) ;
#33339 = ORIENTED_EDGE ( 'NONE', *, *, #36803, .F. ) ;
#33340 = LINE ( 'NONE', #15621, #78142 ) ;
#33341 = CARTESIAN_POINT ( 'NONE',  ( 171.1596004093629517, 249.5938752278392485, 2.804888548739752352 ) ) ;
#33342 = CARTESIAN_POINT ( 'NONE',  ( 17.38248943320504836, 35.13769309531819829, -10.00000000000000000 ) ) ;
#33343 = VERTEX_POINT ( 'NONE', #66544 ) ;
#33344 = CARTESIAN_POINT ( 'NONE',  ( 36.80649086932150027, 23.11110640527294535, -2.839279412974138328 ) ) ;
#33345 = VECTOR ( 'NONE', #67034, 1000.000000000000114 ) ;
#33346 = CARTESIAN_POINT ( 'NONE',  ( 84.76146393123151768, 50.45989236026047564, -13.93701821937661833 ) ) ;
#33347 = CARTESIAN_POINT ( 'NONE',  ( 79.61387698796545465, 49.22643846628885456, -14.28797054368582486 ) ) ;
#33348 = CARTESIAN_POINT ( 'NONE',  ( 168.1217531603526538, 276.7950771177830234, 15.34514958204382573 ) ) ;
#33349 = CARTESIAN_POINT ( 'NONE',  ( 83.10776606998568639, 40.75710275334526500, -2.573362665496658816E-06 ) ) ;
#33350 = AXIS2_PLACEMENT_3D ( 'NONE', #32545, #93886, #71060 ) ;
#33351 = VERTEX_POINT ( 'NONE', #58913 ) ;
#33352 = VERTEX_POINT ( 'NONE', #60912 ) ;
#33353 = CARTESIAN_POINT ( 'NONE',  ( 183.0914503401605202, 295.7967818983725010, 0.7459396247526526302 ) ) ;
#33355 = CARTESIAN_POINT ( 'NONE',  ( 194.9819925439454664, 292.9282776833073285, -15.33279721168237586 ) ) ;
#33354 = CARTESIAN_POINT ( 'NONE',  ( 67.66477494606748166, 65.93994996600352465, 10.43000743018374621 ) ) ;
#33356 = CARTESIAN_POINT ( 'NONE',  ( -19.65312891409030271, 93.06504152958497400, 177.5919119679930134 ) ) ;
#33357 = CARTESIAN_POINT ( 'NONE',  ( 194.5047661587782386, 293.7548580291293092, 14.86680123054176583 ) ) ;
#33358 = CARTESIAN_POINT ( 'NONE',  ( 159.6209877835443081, 264.4662034727394371, 17.77637312803328129 ) ) ;
#33359 = CARTESIAN_POINT ( 'NONE',  ( 70.94055981774539532, 61.07284667920529131, 15.02700796178418408 ) ) ;
#33360 = CARTESIAN_POINT ( 'NONE',  ( 207.4651458030734830, 271.3068219998286850, -3.821411492560412793 ) ) ;
#33361 = CARTESIAN_POINT ( 'NONE',  ( 204.0632701483897620, 269.1718737286272471, 2.454364474035033883 ) ) ;
#33362 = DIRECTION ( 'NONE',  ( 1.000000000000000000, 0.000000000000000000, 0.000000000000000000 ) ) ;
#33363 = CARTESIAN_POINT ( 'NONE',  ( 84.07169456928664886, 219.3458772461660544, 9.188101187500095079 ) ) ;
#33364 = EDGE_LOOP ( 'NONE', ( #18666, #84868, #14468, #54363 ) ) ;
#33365 = CARTESIAN_POINT ( 'NONE',  ( 150.0459203272414470, 271.3762512067029320, 12.15191700100081640 ) ) ;
#33366 = CARTESIAN_POINT ( 'NONE',  ( 77.96869982513443631, 61.39881034122267778, -16.15742658069109439 ) ) ;
#33367 = VERTEX_POINT ( 'NONE', #29055 ) ;
#33368 = CYLINDRICAL_SURFACE ( 'NONE', #81841, 17.82106496071139645 ) ;
#33369 = ORIENTED_EDGE ( 'NONE', *, *, #74862, .T. ) ;
#33370 = CARTESIAN_POINT ( 'NONE',  ( 79.90914067555259237, 44.54479442172742409, -11.07812196971692842 ) ) ;
#33371 = CARTESIAN_POINT ( 'NONE',  ( 66.69061599261269180, 67.49838889342164805, 6.509093489976348401 ) ) ;
#33372 = CARTESIAN_POINT ( 'NONE',  ( 191.0724301404414689, 299.6998384015373063, -9.342134220577969828 ) ) ;
#33373 = CARTESIAN_POINT ( 'NONE',  ( 83.71040786192132543, 41.77199054155873625, -1.945830175533111106 ) ) ;
#33374 = CARTESIAN_POINT ( 'NONE',  ( 85.97400624412107106, 47.01443177752299363, -10.25505571482220013 ) ) ;
#33375 = EDGE_CURVE ( 'NONE', #17718, #62885, #90394, .T. ) ;
#33376 = CARTESIAN_POINT ( 'NONE',  ( 207.6821401748263156, 270.9309767229963768, 1.759036204183980878 ) ) ;
#33377 = CARTESIAN_POINT ( 'NONE',  ( 95.05956542768421969, 219.5643266524160140, 9.188101187500095079 ) ) ;
#33378 = EDGE_LOOP ( 'NONE', ( #58879, #48936, #32102, #39905 ) ) ;
#33379 = EDGE_CURVE ( 'NONE', #33103, #14328, #62799, .T. ) ;
#33380 = ORIENTED_EDGE ( 'NONE', *, *, #24798, .T. ) ;
#33382 = EDGE_CURVE ( 'NONE', #59249, #59130, #68722, .T. ) ;
#33381 = CARTESIAN_POINT ( 'NONE',  ( 200.4117560436087047, 283.5236514288079093, -18.06783071421079612 ) ) ;
#33383 = VERTEX_POINT ( 'NONE', #53807 ) ;
#33384 = ADVANCED_FACE ( 'NONE', ( #77123 ), #36623, .T. ) ;
#33385 = AXIS2_PLACEMENT_3D ( 'NONE', #89000, #43803, #65612 ) ;
#33386 = CARTESIAN_POINT ( 'NONE',  ( 70.27108337839371188, 69.38421209371701082, -7.013144159806405931 ) ) ;
#33387 = CARTESIAN_POINT ( 'NONE',  ( 87.65075002439434115, 44.95127668719692338, -6.583683359477274344 ) ) ;
#33388 = CARTESIAN_POINT ( 'NONE',  ( -3.532187684056935062, 168.7677522451418781, 10.00000000000009592 ) ) ;
#33389 = CARTESIAN_POINT ( 'NONE',  ( 88.04001560340805099, 44.77405568574921091, 4.599260828767079978 ) ) ;
#33390 = ORIENTED_EDGE ( 'NONE', *, *, #5142, .F. ) ;
#33392 = CARTESIAN_POINT ( 'NONE',  ( 87.96802319852463370, 44.26031603380329926, -2.803967949215167454 ) ) ;
#33391 = AXIS2_PLACEMENT_3D ( 'NONE', #91101, #68250, #15532 ) ;
#33393 = CARTESIAN_POINT ( 'NONE',  ( 160.5038987594522837, 275.6177743208444326, 12.83085644997012409 ) ) ;
#33394 = FACE_OUTER_BOUND ( 'NONE', #64131, .T. ) ;
#33395 = CARTESIAN_POINT ( 'NONE',  ( 190.0534303668326288, 269.9073674132432643, 15.26070177760127322 ) ) ;
#33396 = CARTESIAN_POINT ( 'NONE',  ( 153.2283961777204695, 265.2476279883323400, -17.66880461074566000 ) ) ;
#33397 = AXIS2_PLACEMENT_3D ( 'NONE', #28982, #36058, #67463 ) ;
#33398 = CARTESIAN_POINT ( 'NONE',  ( 104.2158063034569579, 237.6427522451419065, -10.00000000000009592 ) ) ;
#33399 = CARTESIAN_POINT ( 'NONE',  ( -25.62627769214124740, 24.57763045674671432, 10.00000000000000000 ) ) ;
#33400 = EDGE_LOOP ( 'NONE', ( #92809, #78985, #16815, #33208 ) ) ;
#33401 = CARTESIAN_POINT ( 'NONE',  ( 6.228640307978117185, 167.7365022471902307, 10.00000000000009948 ) ) ;
#33402 = CARTESIAN_POINT ( 'NONE',  ( 161.4726291907278721, 250.9681975403669867, 14.52346149734912117 ) ) ;
#33403 = CARTESIAN_POINT ( 'NONE',  ( 85.33118850621276863, 44.02131733009327519, 6.393353383217204033 ) ) ;
#33404 = CARTESIAN_POINT ( 'NONE',  ( 14.87430715154758687, 30.36126292948894445, 6.180339887498949913 ) ) ;
#33405 = CARTESIAN_POINT ( 'NONE',  ( 77.82408648432202369, 62.02431454202515226, 15.64647534684074692 ) ) ;
#33406 = CARTESIAN_POINT ( 'NONE',  ( 116.2138665886018458, 231.2365022471901739, -10.00000000000009237 ) ) ;
#33407 = CARTESIAN_POINT ( 'NONE',  ( 163.1811051052586663, 248.0090304528921195, -11.35285691990875456 ) ) ;
#33408 = VERTEX_POINT ( 'NONE', #8238 ) ;
#33409 = AXIS2_PLACEMENT_3D ( 'NONE', #12624, #5506, #68292 ) ;
#33410 = VECTOR ( 'NONE', #68253, 1000.000000000000000 ) ;
#33411 = CARTESIAN_POINT ( 'NONE',  ( 164.4440639631384045, 245.8215215431751233, -2.910115319305802029 ) ) ;
#33413 = CARTESIAN_POINT ( 'NONE',  ( 184.4647054688699370, 266.0064431806318908, 13.20040557144585414 ) ) ;
#33412 = CARTESIAN_POINT ( 'NONE',  ( 178.2835513063369888, 265.3754860723226443, -14.94893715224946540 ) ) ;
#33414 = CARTESIAN_POINT ( 'NONE',  ( 199.1948953252038734, 281.7345316833016113, -16.58223543088974949 ) ) ;
#33415 = CARTESIAN_POINT ( 'NONE',  ( 31.41726478770819853, 19.10801979619930435, 3.090169943749476733 ) ) ;
#33416 = CARTESIAN_POINT ( 'NONE',  ( 2.487887237287232711, 134.7156766241960497, 21.50000000000008527 ) ) ;
#33417 = CARTESIAN_POINT ( 'NONE',  ( 171.9427383041699215, 274.8029616261534329, 16.32014694790107256 ) ) ;
#33418 = CARTESIAN_POINT ( 'NONE',  ( 180.7206978303440508, 273.1106064130323148, 17.40382843373642530 ) ) ;
#33419 = CARTESIAN_POINT ( 'NONE',  ( 161.0071479579559082, 273.4094594936241833, -15.40207120388050832 ) ) ;
#33420 = AXIS2_PLACEMENT_3D ( 'NONE', #56594, #72329, #88564 ) ;
#33421 = CARTESIAN_POINT ( 'NONE',  ( 191.7224207879665983, 261.3713821052344883, 3.085656737073688483 ) ) ;
#33422 = CARTESIAN_POINT ( 'NONE',  ( 72.69493809724967548, 71.16443809380129437, -7.267007365939472052 ) ) ;
#33423 = CARTESIAN_POINT ( 'NONE',  ( 4.992923434102598534, 167.5643266524160140, -9.188101187500093303 ) ) ;
#33424 = CARTESIAN_POINT ( 'NONE',  ( 81.55349978670373901, 45.99021204074624336, 11.55842612056192387 ) ) ;
#33425 = ORIENTED_EDGE ( 'NONE', *, *, #86609, .T. ) ;
#33426 = ADVANCED_FACE ( 'NONE', ( #70523 ), #1653, .F. ) ;
#33427 = CARTESIAN_POINT ( 'NONE',  ( 175.2159268917944530, 255.4244057975548685, 8.238669877113455442 ) ) ;
#33428 = CARTESIAN_POINT ( 'NONE',  ( 26.03432425566073150, 38.52903772873360566, -1.583844403245329602 ) ) ;
#33429 = CARTESIAN_POINT ( 'NONE',  ( 72.13898424358956163, 72.32266849676254594, -1.187258607322207560 ) ) ;
#33430 = CARTESIAN_POINT ( 'NONE',  ( 33.92367135321775606, 181.2048013555409796, 4.594050593750051981 ) ) ;
#33431 = EDGE_CURVE ( 'NONE', #51277, #23145, #77152, .T. ) ;
#33432 = CARTESIAN_POINT ( 'NONE',  ( 164.4678285797544106, 245.7803600197737524, -6.875991496205872799 ) ) ;
#33433 = CARTESIAN_POINT ( 'NONE',  ( 31.96529204653334588, 20.58380873178789017, 6.180339887498953466 ) ) ;
#33434 = CARTESIAN_POINT ( 'NONE',  ( 34.40128339993918871, 35.56454794089043503, 10.00000000000000355 ) ) ;
#33435 = CARTESIAN_POINT ( 'NONE',  ( 179.0573227211665426, 291.9330542595874363, 6.082073241091874749 ) ) ;
#33436 = CARTESIAN_POINT ( 'NONE',  ( 98.68481039724036918, 239.3297689869269220, -2.679491924311252493 ) ) ;
#33437 = CARTESIAN_POINT ( 'NONE',  ( 72.57818625921403566, 63.87955903443374694, 14.16064695466623213 ) ) ;
#33438 = CARTESIAN_POINT ( 'NONE',  ( 81.79443437784206594, 42.09912225842974465, 7.556739885930086054 ) ) ;
#33439 = CARTESIAN_POINT ( 'NONE',  ( 87.11381950699171739, 46.35653380776409449, -8.652283511631230439 ) ) ;
#33440 = CARTESIAN_POINT ( 'NONE',  ( 83.58343668721781228, 51.99607003748921841, 15.00733587213922426 ) ) ;
#33441 = CARTESIAN_POINT ( 'NONE',  ( 93.62503730655774348, 214.8615022471902023, 5.000000000000051514 ) ) ;
#33442 = DIRECTION ( 'NONE',  ( -0.9532659690011954234, 0.2314883312386637471, 0.1941575258509202206 ) ) ;
#33443 = B_SPLINE_CURVE_WITH_KNOTS ( 'NONE', 3,
 ( #60961, #84320, #99494, #37658 ),
 .UNSPECIFIED., .F., .F.,
 ( 4, 4 ),
 ( 0.02269224187031961687, 0.02872765270316010588 ),
 .UNSPECIFIED. ) ;
#33444 = CARTESIAN_POINT ( 'NONE',  ( 161.8799941797769293, 267.8308235043324430, -16.86646120607376531 ) ) ;
#33445 = CARTESIAN_POINT ( 'NONE',  ( 47.42782112377506820, 204.3149278399160664, 9.188101187500093303 ) ) ;
#33446 = CARTESIAN_POINT ( 'NONE',  ( 159.2511875226268216, 254.8158473755685520, 15.75855490706745599 ) ) ;
#33447 = EDGE_CURVE ( 'NONE', #54743, #56966, #47711, .T. ) ;
#33448 = EDGE_LOOP ( 'NONE', ( #27638, #27902 ) ) ;
#33449 = CARTESIAN_POINT ( 'NONE',  ( -8.055044619196017663, 84.65328059711238495, 13.81882856671667525 ) ) ;
#33450 = CARTESIAN_POINT ( 'NONE',  ( -8.406493707509316238, 25.24382671950691304, -10.00000000000000000 ) ) ;
#33451 = DIRECTION ( 'NONE',  ( 0.5000000000000013323, -0.8660254037844378194, 0.000000000000000000 ) ) ;
#33452 = ORIENTED_EDGE ( 'NONE', *, *, #64630, .T. ) ;
#33453 = PLANE ( 'NONE',  #16774 ) ;
#33454 = DIRECTION ( 'NONE',  ( 0.8660254037844395958, 0.4999999999999985567, 0.000000000000000000 ) ) ;
#33455 = PLANE ( 'NONE',  #33147 ) ;
#33456 = CARTESIAN_POINT ( 'NONE',  ( 95.76410038128526026, 214.5494855054052152, -2.679491924311248496 ) ) ;
#33457 = CARTESIAN_POINT ( 'NONE',  ( 20.82173017108080515, 32.99752408145591431, 5.678558825948277544 ) ) ;
#33458 = CARTESIAN_POINT ( 'NONE',  ( 202.4900219881211854, 279.9239892212719383, 15.63116161057562259 ) ) ;
#33459 = CARTESIAN_POINT ( 'NONE',  ( 149.3253462891332219, 272.0079086998416074, -12.99539319630191336 ) ) ;
#33460 = AXIS2_PLACEMENT_3D ( 'NONE', #35284, #19621, #49993 ) ;
#33461 = LINE ( 'NONE', #96292, #37071 ) ;
#33462 = ORIENTED_EDGE ( 'NONE', *, *, #87671, .T. ) ;
#33463 = VECTOR ( 'NONE', #95330, 1000.000000000000114 ) ;
#33464 = CARTESIAN_POINT ( 'NONE',  ( 16.02188117849498639, 11.11110640527290983, -2.839279412974138328 ) ) ;
#33465 = CARTESIAN_POINT ( 'NONE',  ( -13.11024591527723615, 27.99999999999999645, -48.00000000000017053 ) ) ;
#33466 = LINE ( 'NONE', #95817, #80894 ) ;
#33467 = CARTESIAN_POINT ( 'NONE',  ( -13.11024591527734628, 15.00000000000000000, 32.50000000000000000 ) ) ;
#33468 = EDGE_LOOP ( 'NONE', ( #12490, #82135, #57494 ) ) ;
#33469 = CARTESIAN_POINT ( 'NONE',  ( 178.7520316380132499, 282.5168896195049228, 15.81395202663239274 ) ) ;
#33470 = VECTOR ( 'NONE', #80783, 1000.000000000000114 ) ;
#33471 = CARTESIAN_POINT ( 'NONE',  ( 151.0036289208911171, 269.1010379121764799, 14.24595189915657478 ) ) ;
#33472 = CARTESIAN_POINT ( 'NONE',  ( 177.3441421416205799, 256.1034110073948113, -7.247860626662943062 ) ) ;
#33473 = CARTESIAN_POINT ( 'NONE',  ( 84.14312167556933275, 48.98415679381830756, 0.000000000000000000 ) ) ;
#33474 = ORIENTED_EDGE ( 'NONE', *, *, #31526, .F. ) ;
#33475 = EDGE_LOOP ( 'NONE', ( #3755, #84725, #20898, #35867 ) ) ;
#33477 = CARTESIAN_POINT ( 'NONE',  ( 174.6568604941508340, 274.7935765301870674, 17.62145267448687846 ) ) ;
#33476 = LINE ( 'NONE', #55247, #47112 ) ;
#33478 = ORIENTED_EDGE ( 'NONE', *, *, #57691, .T. ) ;
#33479 = CARTESIAN_POINT ( 'NONE',  ( 200.6985908945154335, 283.0268388936558495, -17.74173253065502820 ) ) ;
#33480 = DIRECTION ( 'NONE',  ( -0.000000000000000000, -0.000000000000000000, -1.000000000000000000 ) ) ;
#33481 = CARTESIAN_POINT ( 'NONE',  ( 72.79456978488967422, 56.87432143794737982, -15.93777291093744708 ) ) ;
#33482 = FACE_OUTER_BOUND ( 'NONE', #70421, .T. ) ;
#33483 = CARTESIAN_POINT ( 'NONE',  ( 157.3198323354746435, 258.1610526871778006, -16.77630483474704093 ) ) ;
#33484 = CARTESIAN_POINT ( 'NONE',  ( 112.9752924205922824, 236.0333772461660544, 9.188101187500095079 ) ) ;
#33485 = B_SPLINE_CURVE_WITH_KNOTS ( 'NONE', 3,
 ( #95508, #25547, #56929, #73649 ),
 .UNSPECIFIED., .F., .F.,
 ( 4, 4 ),
 ( 0.04392709020753635812, 0.04887066958154935581 ),
 .UNSPECIFIED. ) ;
#33486 = B_SPLINE_CURVE_WITH_KNOTS ( 'NONE', 3,
 ( #46361, #70170, #31171, #60071 ),
 .UNSPECIFIED., .F., .F.,
 ( 4, 4 ),
 ( 0.02479711570197204798, 0.03404299025597421618 ),
 .UNSPECIFIED. ) ;
#33487 = CARTESIAN_POINT ( 'NONE',  ( 182.7250377612010936, 287.9595840865778769, -13.19241888926224071 ) ) ;
#33488 = ORIENTED_EDGE ( 'NONE', *, *, #92930, .F. ) ;
#33489 = AXIS2_PLACEMENT_3D ( 'NONE', #13844, #44228, #44721 ) ;
#33490 = VECTOR ( 'NONE', #7, 1000.000000000000000 ) ;
#33491 = CARTESIAN_POINT ( 'NONE',  ( 207.5290616128274337, 271.1961165699281651, 2.604679844609484984 ) ) ;
#33492 = ORIENTED_EDGE ( 'NONE', *, *, #11761, .T. ) ;
#33493 = CARTESIAN_POINT ( 'NONE',  ( 33.10965510200716722, 34.51421378149920827, -9.188101187500004485 ) ) ;
#33494 = CARTESIAN_POINT ( 'NONE',  ( -22.42236680055709641, 157.8615022471902591, 0.000000000000000000 ) ) ;
#33495 = CARTESIAN_POINT ( 'NONE',  ( 78.59318410106391184, 47.91850279518009614, -14.47096384754294363 ) ) ;
#33496 = CARTESIAN_POINT ( 'NONE',  ( 68.45643432912224569, 201.1423013555409796, -4.594050593750043987 ) ) ;
#33497 = CARTESIAN_POINT ( 'NONE',  ( 73.96424987833113107, 68.60250435897062005, 11.39670188853133048 ) ) ;
#33498 = CARTESIAN_POINT ( 'NONE',  ( 150.7530568467738590, 269.5350414755053521, 15.60317050893315916 ) ) ;
#33499 = CARTESIAN_POINT ( 'NONE',  ( 150.7108765041139691, 269.6080999720726936, 13.72660302980452407 ) ) ;
#33501 = AXIS2_PLACEMENT_3D ( 'NONE', #19048, #73236, #33740 ) ;
#33500 = DIRECTION ( 'NONE',  ( 0.000000000000000000, 0.000000000000000000, -1.000000000000000000 ) ) ;
#33502 = ORIENTED_EDGE ( 'NONE', *, *, #69842, .F. ) ;
#33503 = CARTESIAN_POINT ( 'NONE',  ( 73.21300331465644717, 58.97917566933716671, -15.60506319839823064 ) ) ;
#33504 = CARTESIAN_POINT ( 'NONE',  ( 85.72508672120996209, 43.23034436632222111, -3.633758481124208295 ) ) ;
#33505 = FACE_OUTER_BOUND ( 'NONE', #39720, .T. ) ;
#33506 = DIRECTION ( 'NONE',  ( -0.8951289669282590511, 0.4458072818673421978, 0.000000000000000000 ) ) ;
#33507 = ORIENTED_EDGE ( 'NONE', *, *, #97007, .F. ) ;
#33508 = CARTESIAN_POINT ( 'NONE',  ( -19.65312891409030271, 93.06504152958497400, 10.00000000000000888 ) ) ;
#33509 = CARTESIAN_POINT ( 'NONE',  ( 173.8979489505312586, 277.9637680410879170, -15.96371148716977117 ) ) ;
#33510 = CARTESIAN_POINT ( 'NONE',  ( 162.2240457438445560, 259.4344955095195360, -16.32888341801637111 ) ) ;
#33511 = EDGE_CURVE ( 'NONE', #77610, #18050, #87312, .T. ) ;
#33512 = CARTESIAN_POINT ( 'NONE',  ( 81.65975360897576252, 52.35792944948207861, -15.54859200978484601 ) ) ;
#33513 = CARTESIAN_POINT ( 'NONE',  ( 148.9230895364621574, 272.7046378331555161, 12.20434325797056019 ) ) ;
#33514 = CARTESIAN_POINT ( 'NONE',  ( 180.8902496232956310, 271.3945185957094282, 16.78426242912689403 ) ) ;
#33515 = CARTESIAN_POINT ( 'NONE',  ( 164.3939401533646958, 245.9083385283718712, 2.844462461176849200 ) ) ;
#33516 = CARTESIAN_POINT ( 'NONE',  ( 168.1332551043281285, 255.5560320396268423, 13.96088319188761950 ) ) ;
#33517 = CARTESIAN_POINT ( 'NONE',  ( 30.80155721116056711, 46.36891074996812279, -10.00000000000000000 ) ) ;
#33518 = B_SPLINE_CURVE_WITH_KNOTS ( 'NONE', 3,
 ( #39683, #47307, #81976, #50527, #73354, #27747, #98658, #13061, #4955, #19664, #13549, #82496, #59611, #67735, #58133, #42905, #90077, #29242, #81480, #12053, #73846, #58616, #65725, #4435, #66243, #27250, #5442, #35333, #11562, #89115, #28231 ),
 .UNSPECIFIED., .F., .F.,
 ( 4, 3, 3, 3, 3, 3, 3, 3, 3, 3, 4 ),
 ( 0.000000000000000000, 0.1333490885032416196, 0.3007194338854398130, 0.4699862290245220287, 0.5844252810809438259, 0.6686540514502733457, 0.7354980260655562541, 0.8028463152565635808, 0.8633854507757173780, 0.9437142632667323561, 1.000000000000000000 ),
 .UNSPECIFIED. ) ;
#33519 = CARTESIAN_POINT ( 'NONE',  ( 118.1714448432989144, 239.0333772461660544, 9.188101187500095079 ) ) ;
#33520 = ORIENTED_EDGE ( 'NONE', *, *, #19629, .F. ) ;
#33521 = LINE ( 'NONE', #19825, #91848 ) ;
#33522 = FACE_OUTER_BOUND ( 'NONE', #27508, .T. ) ;
#33523 = DIRECTION ( 'NONE',  ( -1.000000000000000000, 0.000000000000000000, 0.000000000000000000 ) ) ;
#33524 = CARTESIAN_POINT ( 'NONE',  ( 204.7235752877335244, 276.0553614249301972, 14.82397698933823271 ) ) ;
#33525 = CARTESIAN_POINT ( 'NONE',  ( 83.83095627921952087, 51.88776739408810812, -14.90233955705620694 ) ) ;
#33526 = CARTESIAN_POINT ( 'NONE',  ( 76.22397158102836556, 50.99593462407597855, -15.55193810795204179 ) ) ;
#33527 = ORIENTED_EDGE ( 'NONE', *, *, #54999, .F. ) ;
#33528 = CARTESIAN_POINT ( 'NONE',  ( 80.34499676519902778, 57.43793486056498665, -16.58883017036144381 ) ) ;
#33529 = CARTESIAN_POINT ( 'NONE',  ( 157.9584063519955635, 274.6739674095948658, -12.56162459328316316 ) ) ;
#33531 = CARTESIAN_POINT ( 'NONE',  ( 182.0644918927315814, 260.4883331680307492, 9.524347663358822658 ) ) ;
#33530 = CARTESIAN_POINT ( 'NONE',  ( 147.7269416596823248, 275.9539214970327521, 2.717771182133930541 ) ) ;
#33532 = CARTESIAN_POINT ( 'NONE',  ( 74.59892996465779902, 66.99479792721430726, 12.53190758343627031 ) ) ;
#33533 = CARTESIAN_POINT ( 'NONE',  ( 137.3322569020296555, 250.0958772461660544, -9.188101187500095079 ) ) ;
#33534 = CARTESIAN_POINT ( 'NONE',  ( 57.23161641937174693, 215.3967562850347122, -4.648177544792955347E-16 ) ) ;
#33535 = LINE ( 'NONE', #34527, #74115 ) ;
#33536 = CARTESIAN_POINT ( 'NONE',  ( 59.38997056143013964, 205.0958772461660828, -9.188101187500095079 ) ) ;
#33537 = VECTOR ( 'NONE', #46485, 1000.000000000000000 ) ;
#33539 = CARTESIAN_POINT ( 'NONE',  ( 207.6628070930962906, 270.9644626028195376, 7.378217122120054761 ) ) ;
#33538 = AXIS2_PLACEMENT_3D ( 'NONE', #26258, #25770, #10059 ) ;
#33540 = CARTESIAN_POINT ( 'NONE',  ( 157.8820657059571033, 257.1872359237914338, -17.60412210594719440 ) ) ;
#33541 = CARTESIAN_POINT ( 'NONE',  ( 174.4320096083763190, 251.4713395514856416, 3.621238935830661365 ) ) ;
#33542 = B_SPLINE_SURFACE_WITH_KNOTS ( 'NONE', 3, 1, ( 
 ( #98, #39558 ),
 ( #91828, #30981 ),
 ( #6695, #70482 ),
 ( #588, #54259 ),
 ( #31973, #31473 ),
 ( #76122, #68479 ),
 ( #62364, #85230 ),
 ( #38065, #77083 ),
 ( #99409, #68979 ),
 ( #38577, #61868 ),
 ( #93321, #99901 ),
 ( #30488, #61378 ),
 ( #92333, #3127 ),
 ( #65383, #10201 ),
 ( #80135, #26398 ),
 ( #10698, #96326 ),
 ( #79635, #95843 ),
 ( #73013, #41065 ),
 ( #48187, #48701 ),
 ( #94327, #78605 ),
 ( #71510, #79133 ),
 ( #56781, #34012 ),
 ( #72002, #55263 ),
 ( #64897, #55757 ),
 ( #86749, #87271 ),
 ( #57275, #41577 ),
 ( #40570, #11214 ),
 ( #1610, #2607 ),
 ( #33495, #71008 ),
 ( #80637, #17283 ),
 ( #9191, #86245 ) ),
 .UNSPECIFIED., .F., .F., .F.,
 ( 4, 3, 3, 3, 3, 3, 3, 3, 3, 3, 4 ),
 ( 2, 2 ),
 ( 0.000000000000000000, 0.1122669598086731141, 0.2243161639709448096, 0.3396355846218966912, 0.4553962076584983087, 0.5677860799922205270, 0.6749047109689384483, 0.7773884377078154051, 0.8775581155834121239, 0.9782364162377549244, 1.000000000000000000 ),
 ( 0.000000000000000000, 1.000000000000000000 ),
 .UNSPECIFIED. ) ;
#33543 = CARTESIAN_POINT ( 'NONE',  ( 165.6871908161093643, 250.8440145507587715, 11.60328334000779726 ) ) ;
#33544 = CARTESIAN_POINT ( 'NONE',  ( 171.3957680990430390, 259.8009312154816257, 15.34336344307106792 ) ) ;
#33545 = CARTESIAN_POINT ( 'NONE',  ( 154.8275264459192613, 279.3822692668657623, -1.584013062148165396 ) ) ;
#33546 = CARTESIAN_POINT ( 'NONE',  ( 154.4470374439381146, 277.6591429590598068, -9.115886381272481742 ) ) ;
#33547 = CARTESIAN_POINT ( 'NONE',  ( 155.1398527401465230, 261.9368881057492899, -17.02245700497956449 ) ) ;
#33548 = CARTESIAN_POINT ( 'NONE',  ( 48.77433535142598231, 99.76555324011610537, -10.00000000000000000 ) ) ;
#33549 = VECTOR ( 'NONE', #2380, 1000.000000000000000 ) ;
#33550 = CARTESIAN_POINT ( 'NONE',  ( 127.7428297729342717, 237.8927522451417929, -10.00000000000009059 ) ) ;
#33551 = CARTESIAN_POINT ( 'NONE',  ( 79.26853152882971187, 52.33679484845949759, -15.48194681045292320 ) ) ;
#33552 = ORIENTED_EDGE ( 'NONE', *, *, #67444, .F. ) ;
#33553 = DIRECTION ( 'NONE',  ( -0.6835488936653838499, -0.7299047266382303611, 0.000000000000000000 ) ) ;
#33554 = CARTESIAN_POINT ( 'NONE',  ( 18.44000607287492954, 15.81029122506293838, 8.090169943749479842 ) ) ;
#33555 = EDGE_CURVE ( 'NONE', #79692, #37942, #24433, .T. ) ;
#33556 = CARTESIAN_POINT ( 'NONE',  ( 48.78150646083578579, 186.7202760586659736, -5.415160957724236172E-17 ) ) ;
#33557 = CARTESIAN_POINT ( 'NONE',  ( 17.92595094200897776, 22.30066082961421259, -10.00000000000000533 ) ) ;
#33558 = CARTESIAN_POINT ( 'NONE',  ( 68.02798755508815987, 65.19179537507288558, -10.68069436451683352 ) ) ;
#33559 = CARTESIAN_POINT ( 'NONE',  ( 65.76829148152603466, 69.09872882758028823, 0.1165290730599739394 ) ) ;
#33560 = DIRECTION ( 'NONE',  ( -0.8660254037844387076, -0.4999999999999998890, -0.000000000000000000 ) ) ;
#33561 = CARTESIAN_POINT ( 'NONE',  ( 190.8683709797118411, 300.0532792356709706, -4.461919767133968762 ) ) ;
#33562 = CARTESIAN_POINT ( 'NONE',  ( 66.90909321525144549, 68.17756947874360662, -6.600776075497404527 ) ) ;
#33563 = B_SPLINE_CURVE_WITH_KNOTS ( 'NONE', 3,
 ( #64007, #25513, #40188, #71128 ),
 .UNSPECIFIED., .F., .F.,
 ( 4, 4 ),
 ( 0.007140653581439226905, 0.01527480993219123249 ),
 .UNSPECIFIED. ) ;
#33565 = CARTESIAN_POINT ( 'NONE',  ( 52.39861964368801495, 214.3927522451419634, 2.944929066748280225E-16 ) ) ;
#33564 = DIRECTION ( 'NONE',  ( -0.7235470741700504860, -0.1663964660674512042, 0.6699192843471690750 ) ) ;
#33566 = CARTESIAN_POINT ( 'NONE',  ( 173.9238158565421770, 289.3171369187040227, 8.002423422717384938 ) ) ;
#33567 = CARTESIAN_POINT ( 'NONE',  ( 184.7990890438850329, 257.6713462901447542, 1.377030906181146097 ) ) ;
#33568 = CARTESIAN_POINT ( 'NONE',  ( 157.6036818288543486, 257.6694109429415107, -16.73826488331764395 ) ) ;
#33569 = CARTESIAN_POINT ( 'NONE',  ( 6.396987757676594555, 15.64441083166260427, 0.000000000000000000 ) ) ;
#33570 = EDGE_CURVE ( 'NONE', #97892, #38977, #92861, .T. ) ;
#33571 = CARTESIAN_POINT ( 'NONE',  ( 45.99364009841357159, 197.3615022471902591, -10.00000000000009592 ) ) ;
#33572 = CARTESIAN_POINT ( 'NONE',  ( 185.0682636646367314, 294.3875985914592661, 9.867065237507818054 ) ) ;
#33573 = VECTOR ( 'NONE', #1022, 1000.000000000000000 ) ;
#33574 = DIRECTION ( 'NONE',  ( 0.000000000000000000, 0.000000000000000000, -1.000000000000000000 ) ) ;
#33575 = CARTESIAN_POINT ( 'NONE',  ( 8.375921941576814689, 166.4548013555410080, -4.594050593750042211 ) ) ;
#33576 = CARTESIAN_POINT ( 'NONE',  ( 32.54976882715482134, 40.83396525600392835, -2.839279412974133887 ) ) ;
#33579 = EDGE_CURVE ( 'NONE', #2846, #68611, #35335, .T. ) ;
#33578 = DIRECTION ( 'NONE',  ( 0.000000000000000000, 0.000000000000000000, 1.000000000000000000 ) ) ;
#33577 = CARTESIAN_POINT ( 'NONE',  ( 164.3996301846870267, 247.3020492865104529, 7.248807534621905191 ) ) ;
#33580 = DIRECTION ( 'NONE',  ( -0.9292718480896766664, -0.3693965786901617920, 0.000000000000000000 ) ) ;
#33581 = CARTESIAN_POINT ( 'NONE',  ( 32.54976882715482134, 40.83396525600392835, -2.839279412974133887 ) ) ;
#33582 = DIRECTION ( 'NONE',  ( -0.9514785060800255989, 0.3077152132536228324, 0.000000000000000000 ) ) ;
#33583 = CARTESIAN_POINT ( 'NONE',  ( 186.9451997612131038, 258.7018344183949807, -2.460581910096537150 ) ) ;
#33584 = CARTESIAN_POINT ( 'NONE',  ( 149.2923684163597784, 272.0650280510108701, -12.99082738998495756 ) ) ;
#33585 = PLANE ( 'NONE',  #43862 ) ;
#33586 = CARTESIAN_POINT ( 'NONE',  ( 11.99908958663318970, 18.87878583063839955, -9.188101187500006262 ) ) ;
#33587 = CARTESIAN_POINT ( 'NONE',  ( 153.9505496568006322, 278.0639657297674034, -5.205343530163337284 ) ) ;
#33588 = CARTESIAN_POINT ( 'NONE',  ( 15.22926075146606273, 30.83396525600389637, -2.839279412974133887 ) ) ;
#33589 = CARTESIAN_POINT ( 'NONE',  ( 160.3910089434251347, 252.8416187631903824, 14.67024385955689780 ) ) ;
#33590 = CARTESIAN_POINT ( 'NONE',  ( 153.2359015056687781, 277.7311577273633247, -5.083231879104856965 ) ) ;
#33591 = CARTESIAN_POINT ( 'NONE',  ( 84.83002093244189723, 50.29676582423640241, -13.82165720535206788 ) ) ;
#33592 = CARTESIAN_POINT ( 'NONE',  ( 206.3018347371251195, 273.3217358710584790, -9.309724106897926177 ) ) ;
#33593 = CARTESIAN_POINT ( 'NONE',  ( 54.51751480423398988, 213.8297689869269220, -2.679491924311252493 ) ) ;
#33594 = VERTEX_POINT ( 'NONE', #32016 ) ;
#33595 = CARTESIAN_POINT ( 'NONE',  ( 192.8323852661406761, 296.6515067047851062, 11.86505947732313615 ) ) ;
#33596 = CARTESIAN_POINT ( 'NONE',  ( 164.9335952247126045, 244.9736285262353306, -1.661461410667423255 ) ) ;
#33597 = CARTESIAN_POINT ( 'NONE',  ( 66.25889107252001509, 68.18093703880344947, 4.235875044229025832 ) ) ;
#33598 = CARTESIAN_POINT ( 'NONE',  ( 87.62362232749241286, 45.09856358269391308, 6.901305344596342373 ) ) ;
#33599 = CARTESIAN_POINT ( 'NONE',  ( 154.9226727788713731, 262.3130548330639726, 18.22497199616848818 ) ) ;
#33600 = VERTEX_POINT ( 'NONE', #48230 ) ;
#33601 = VERTEX_POINT ( 'NONE', #23415 ) ;
#33602 = CARTESIAN_POINT ( 'NONE',  ( 158.5416719719927130, 277.8521597524036792, -9.836060501838524317 ) ) ;
#33603 = CARTESIAN_POINT ( 'NONE',  ( 86.65390046659096868, 47.16758140886460637, 10.54653844973484489 ) ) ;
#33604 = ORIENTED_EDGE ( 'NONE', *, *, #11780, .T. ) ;
#33605 = AXIS2_PLACEMENT_3D ( 'NONE', #43883, #43384, #4914 ) ;
#33606 = CARTESIAN_POINT ( 'NONE',  ( 78.08056911966330915, 59.58490249653190318, 16.06997153095679209 ) ) ;
#33607 = DIRECTION ( 'NONE',  ( -0.8660254037844385966, -0.5000000000000001110, -6.091690621058838765E-17 ) ) ;
#33608 = EDGE_LOOP ( 'NONE', ( #89467, #93813, #80670, #42183 ) ) ;
#33609 = LINE ( 'NONE', #57389, #19998 ) ;
#33610 = CARTESIAN_POINT ( 'NONE',  ( 84.46782944188609576, 48.58092674594113447, -12.38698248680477221 ) ) ;
#33611 = AXIS2_PLACEMENT_3D ( 'NONE', #71049, #9230, #79677 ) ;
#33612 = CARTESIAN_POINT ( 'NONE',  ( 80.48572449743757318, 43.55285070694157668, 9.722916489287488417 ) ) ;
#33613 = VERTEX_POINT ( 'NONE', #61913 ) ;
#33614 = CARTESIAN_POINT ( 'NONE',  ( 175.1183745746886871, 267.9007702990796247, 17.47926410801357022 ) ) ;
#33615 = CARTESIAN_POINT ( 'NONE',  ( 206.4768661561222984, 273.0185725604343361, 11.39716120335626925 ) ) ;
#33616 = VECTOR ( 'NONE', #91285, 1000.000000000000114 ) ;
#33617 = CARTESIAN_POINT ( 'NONE',  ( 151.4268868568842379, 274.9972536827360159, -8.604776644755594006 ) ) ;
#33618 = ORIENTED_EDGE ( 'NONE', *, *, #99360, .T. ) ;
#33619 = EDGE_CURVE ( 'NONE', #28770, #4321, #54305, .T. ) ;
#33620 = CARTESIAN_POINT ( 'NONE',  ( 172.0721957670934898, 256.4003672175040833, -11.61734053971215452 ) ) ;
#33621 = ORIENTED_EDGE ( 'NONE', *, *, #73853, .T. ) ;
#33622 = ORIENTED_EDGE ( 'NONE', *, *, #26204, .F. ) ;
#33623 = CARTESIAN_POINT ( 'NONE',  ( 158.5402111638430824, 267.6492219652220683, -16.22994191499176608 ) ) ;
#33624 = VERTEX_POINT ( 'NONE', #85273 ) ;
#33625 = CARTESIAN_POINT ( 'NONE',  ( -19.65312891409030271, 93.06504152958497400, 10.00000000000000000 ) ) ;
#33626 = EDGE_LOOP ( 'NONE', ( #58757, #91419, #9916, #16321 ) ) ;
#33627 = ADVANCED_FACE ( 'NONE', ( #23921 ), #71051, .T. ) ;
#33628 = AXIS2_PLACEMENT_3D ( 'NONE', #84287, #15315, #77133 ) ;
#33629 =( BOUNDED_CURVE ( )  B_SPLINE_CURVE ( 2, ( #43998, #6017, #15098, #29817, #75433, #29326, #30318, #98240, #52602 ),
 .UNSPECIFIED., .F., .T. ) 
 B_SPLINE_CURVE_WITH_KNOTS ( ( 3, 2, 2, 2, 3 ),
 ( 0.004032258064516129788, 0.005376344086021505805, 0.008064516129032257841, 0.01075268817204301161, 0.01209677419354838676 ),
 .UNSPECIFIED. ) 
 CURVE ( )  GEOMETRIC_REPRESENTATION_ITEM ( )  RATIONAL_B_SPLINE_CURVE ( ( 0.9330127018922194093, 0.9330127018922194093, 1.000000000000000000, 0.8660254037844387076, 1.000000000000000000, 0.8660254037844387076, 1.000000000000000000, 0.9330127018922192983, 0.9330127018922194093 ) ) 
 REPRESENTATION_ITEM ( '' )  );
#33630 = CARTESIAN_POINT ( 'NONE',  ( 159.0888396382809447, 259.5703526363064384, 16.71962710754473491 ) ) ;
#33631 = CARTESIAN_POINT ( 'NONE',  ( 193.4506777133003368, 295.5805927723682203, 14.77919976000363000 ) ) ;
#33632 = CARTESIAN_POINT ( 'NONE',  ( 188.1412547211656943, 273.5593357346770063, 17.08033167198486879 ) ) ;
#33633 = CARTESIAN_POINT ( 'NONE',  ( 72.01212875430924498, 70.46278977997356208, 6.938461426218038852 ) ) ;
#33634 = CARTESIAN_POINT ( 'NONE',  ( 192.0331311261993790, 298.0358554833232461, 11.82583305898340953 ) ) ;
#33635 = CARTESIAN_POINT ( 'NONE',  ( -17.42236680055705023, 149.2012482093457777, 0.000000000000000000 ) ) ;
#33636 = EDGE_CURVE ( 'NONE', #71153, #4561, #70018, .T. ) ;
#33637 = CARTESIAN_POINT ( 'NONE',  ( 196.9412859255907620, 289.5346819993642953, -17.37273023188612342 ) ) ;
#33638 = VECTOR ( 'NONE', #22246, 1000.000000000000227 ) ;
#33639 = VERTEX_POINT ( 'NONE', #63432 ) ;
#33640 = LINE ( 'NONE', #94967, #17260 ) ;
#33641 = CARTESIAN_POINT ( 'NONE',  ( 26.41418602390824333, 17.11110640527292759, -2.839279412974138328 ) ) ;
#33642 = CARTESIAN_POINT ( 'NONE',  ( 205.7639495959071212, 274.2533802642843170, 10.79039487422292432 ) ) ;
#33644 = CARTESIAN_POINT ( 'NONE',  ( 164.6241018286200699, 245.5096868128744632, 3.031483545445131433 ) ) ;
#33643 = CARTESIAN_POINT ( 'NONE',  ( 149.3629284598386278, 271.9428144707212027, -12.99253781774931049 ) ) ;
#33646 = ORIENTED_EDGE ( 'NONE', *, *, #88200, .F. ) ;
#33645 = CARTESIAN_POINT ( 'NONE',  ( 206.8251824619401873, 271.5843563996517673, 6.058312812321095642 ) ) ;
#33647 = VECTOR ( 'NONE', #37461, 1000.000000000000114 ) ;
#33648 = VERTEX_POINT ( 'NONE', #79678 ) ;
#33649 = EDGE_CURVE ( 'NONE', #96111, #55260, #64409, .T. ) ;
#33650 = CARTESIAN_POINT ( 'NONE',  ( 146.8463403758815389, 276.3016728938570736, -2.700094491758966875 ) ) ;
#33651 = CARTESIAN_POINT ( 'NONE',  ( 171.5219099648802796, 259.6759708972976455, -14.96685982020008332 ) ) ;
#33652 = EDGE_CURVE ( 'NONE', #8187, #70225, #92006, .T. ) ;
#33653 = CARTESIAN_POINT ( 'NONE',  ( 163.7831042501927072, 247.9065475540300554, 8.386170005195905830 ) ) ;
#33654 = CARTESIAN_POINT ( 'NONE',  ( 79.14312167556931854, 57.64441083166269664, 0.000000000000000000 ) ) ;
#33655 = CARTESIAN_POINT ( 'NONE',  ( 200.7897860911934913, 282.8688841796032420, 18.17522996445731920 ) ) ;
#33656 = CARTESIAN_POINT ( 'NONE',  ( 191.0099562606770860, 262.1165538832237303, -0.7421737651540062375 ) ) ;
#33657 = ORIENTED_EDGE ( 'NONE', *, *, #62596, .F. ) ;
#33658 = CARTESIAN_POINT ( 'NONE',  ( -37.20311282697427657, 64.84237164687553445, -10.00000000000000000 ) ) ;
#33659 = CIRCLE ( 'NONE', #36885, 14.82106496071144619 ) ;
#33660 = LINE ( 'NONE', #10358, #92070 ) ;
#33661 = CARTESIAN_POINT ( 'NONE',  ( 19.34531673258195639, 188.6427522451419350, 10.00000000000009237 ) ) ;
#33662 = CARTESIAN_POINT ( 'NONE',  ( 99.38934535084139554, 234.3149278399160949, 9.188101187500093303 ) ) ;
#33663 = CARTESIAN_POINT ( 'NONE',  ( 82.10040256005657966, 40.74948492577103565, -0.8666556322613548913 ) ) ;
#33664 = CARTESIAN_POINT ( 'NONE',  ( 84.65919635822490363, 50.58401048434825498, 13.62798742565141907 ) ) ;
#33665 = CARTESIAN_POINT ( 'NONE',  ( 207.5772549350081988, 271.1126432873252838, 2.658056670308439617 ) ) ;
#33666 = CARTESIAN_POINT ( 'NONE',  ( 18.36166996137734841, 193.6589784336661637, -6.496448406907675876E-16 ) ) ;
#33667 = DIRECTION ( 'NONE',  ( 0.000000000000000000, 0.000000000000000000, 1.000000000000000000 ) ) ;
#33668 = EDGE_LOOP ( 'NONE', ( #79383, #42915, #69754, #36566 ) ) ;
#33669 = B_SPLINE_CURVE_WITH_KNOTS ( 'NONE', 3,
 ( #80822, #79808, #74179, #75658 ),
 .UNSPECIFIED., .F., .F.,
 ( 4, 4 ),
 ( 0.0009145195436546301338, 0.001503970514818383109 ),
 .UNSPECIFIED. ) ;
#33670 = ORIENTED_EDGE ( 'NONE', *, *, #2265, .T. ) ;
#33671 = CARTESIAN_POINT ( 'NONE',  ( 185.8137939302156099, 260.3527139192792106, -5.808480177743201800 ) ) ;
#33672 = CARTESIAN_POINT ( 'NONE',  ( 88.16428468221791093, 44.07872432484457903, 0.5427949595267680394 ) ) ;
#33673 = LINE ( 'NONE', #3771, #12749 ) ;
#33674 = CARTESIAN_POINT ( 'NONE',  ( 195.1546726974473245, 264.9111313380191177, -4.390412657300894139 ) ) ;
#33675 = CARTESIAN_POINT ( 'NONE',  ( 86.32721218574307898, 47.55264674982593931, -11.12316258729871699 ) ) ;
#33676 = CARTESIAN_POINT ( 'NONE',  ( 74.11446612904798315, 67.86722427140298919, -11.63493275082046452 ) ) ;
#33677 = CARTESIAN_POINT ( 'NONE',  ( 33.57176175898906934, 184.0643266524159856, -9.188101187500093303 ) ) ;
#33678 = CARTESIAN_POINT ( 'NONE',  ( 79.60625107924913380, 226.7677522451419350, -5.000000000000047962 ) ) ;
#33679 = AXIS2_PLACEMENT_3D ( 'NONE', #46633, #77558, #39020 ) ;
#33680 = ORIENTED_EDGE ( 'NONE', *, *, #30542, .F. ) ;
#33681 = B_SPLINE_CURVE_WITH_KNOTS ( 'NONE', 3,
 ( #23324, #15725, #54211, #85179 ),
 .UNSPECIFIED., .F., .F.,
 ( 4, 4 ),
 ( 0.01724406098665899612, 0.02362940485487354664 ),
 .UNSPECIFIED. ) ;
#33682 = CARTESIAN_POINT ( 'NONE',  ( 82.17579637593928510, 43.45516270846064089, 8.362656290713127660 ) ) ;
#33683 = B_SPLINE_CURVE_WITH_KNOTS ( 'NONE', 3,
 ( #78113, #8703, #98928, #29506, #60383, #31987, #1109, #40582, #10213, #2620, #63897, #9205, #40078, #9728, #70494, #1623, #47683, #39571, #94835, #71023, #24402, #64908, #64404, #10711, #32509, #95367, #49694, #2113, #25398, #80146, #3138, #55277, #25920, #41588, #63401, #32995, #62893, #78618, #55769, #56286, #87284, #87778, #71523, #93848, #17815, #86257, #48716, #18810, #79647, #18314 ),
 .UNSPECIFIED., .F., .F.,
 ( 4, 2, 2, 2, 2, 2, 2, 2, 2, 2, 2, 2, 2, 2, 2, 2, 2, 2, 2, 2, 2, 2, 2, 2, 4 ),
 ( 0.001348966706550652024, 0.001814384599846849324, 0.002279802493143046407, 0.002512511439791146033, 0.002628865913115252008, 0.002745220386439358416, 0.002861574859763464391, 0.002977929333087570365, 0.003210638279735712926, 0.003676056173031953811, 0.004141474066328193829, 0.005072309852920743253, 0.006003145639513294413, 0.006468563532809569125, 0.006933981426105842970, 0.007050335899429947643, 0.007108513136091999113, 0.007166690372754051450, 0.007283044846078170001, 0.007399399319402288552, 0.007632108266050384275, 0.007864817212698478263, 0.008097526159346574853, 0.008330235105994669709, 0.008795652999290947890 ),
 .UNSPECIFIED. ) ;
#33684 = CARTESIAN_POINT ( 'NONE',  ( 178.7559403991110969, 259.1783237468100083, -10.26446977356301815 ) ) ;
#33685 = AXIS2_PLACEMENT_3D ( 'NONE', #10324, #48317, #10821 ) ;
#33686 = EDGE_CURVE ( 'NONE', #30496, #50515, #85799, .T. ) ;
#33687 = CARTESIAN_POINT ( 'NONE',  ( -2.124636079309504488, 160.3923013555410080, 4.594050593750050204 ) ) ;
#33688 = VECTOR ( 'NONE', #31368, 1000.000000000000114 ) ;
#33689 = CARTESIAN_POINT ( 'NONE',  ( 68.70265395645864714, 63.99518547148130665, -12.05469093682469328 ) ) ;
#33690 = CARTESIAN_POINT ( 'NONE',  ( 199.1216527653377000, 285.7581758537840528, -18.37739894744384728 ) ) ;
#33691 = CARTESIAN_POINT ( 'NONE',  ( 186.8532369007405691, 282.7788865962135105, 16.19183947954036285 ) ) ;
#33692 = CARTESIAN_POINT ( 'NONE',  ( 147.4563929227680603, 275.2450308873625886, -3.847749617713808412 ) ) ;
#33693 = EDGE_CURVE ( 'NONE', #29349, #26521, #16329, .T. ) ;
#33694 = CARTESIAN_POINT ( 'NONE',  ( 72.21141513960786540, 68.08919752073838083, -10.92203768660748153 ) ) ;
#33695 = CARTESIAN_POINT ( 'NONE',  ( 204.5133713884061706, 276.4194452585140311, 14.87364779308245843 ) ) ;
#33696 = CARTESIAN_POINT ( 'NONE',  ( 146.5095091551180815, 276.8850816817948726, 0.1418322875769769398 ) ) ;
#33697 = CARTESIAN_POINT ( 'NONE',  ( 164.4781197247689306, 245.7625352337404649, -1.511762618280499515 ) ) ;
#33698 = VERTEX_POINT ( 'NONE', #17324 ) ;
#33699 = CIRCLE ( 'NONE', #59551, 17.82106496071138224 ) ;
#33700 = CARTESIAN_POINT ( 'NONE',  ( -9.864998445682774175, 175.1115022471903160, -5.000000000000047962 ) ) ;
#33701 = CARTESIAN_POINT ( 'NONE',  ( 161.3862585056135686, 251.5213894571381559, -13.16453305755435288 ) ) ;
#33702 = CARTESIAN_POINT ( 'NONE',  ( 123.0160347675418677, 232.6423013555409796, -4.594050593750043987 ) ) ;
#33703 = CARTESIAN_POINT ( 'NONE',  ( 17.52000153575897912, 22.06628583063841020, -9.188101187500006262 ) ) ;
#33705 = EDGE_CURVE ( 'NONE', #66239, #7719, #45001, .T. ) ;
#33704 = LINE ( 'NONE', #64597, #88161 ) ;
#33706 = LINE ( 'NONE', #81333, #45177 ) ;
#33707 = VECTOR ( 'NONE', #55893, 1000.000000000000000 ) ;
#33708 = CARTESIAN_POINT ( 'NONE',  ( 196.1241105319816143, 290.9500712997905794, 15.97146679939154268 ) ) ;
#33709 = CARTESIAN_POINT ( 'NONE',  ( 190.6266536543345467, 300.4719459242942321, -7.634394059267482824 ) ) ;
#33710 = ORIENTED_EDGE ( 'NONE', *, *, #14539, .T. ) ;
#33711 = CARTESIAN_POINT ( 'NONE',  ( 189.6469694556133163, 261.3224043400873029, -4.488274779931007430 ) ) ;
#33712 = CARTESIAN_POINT ( 'NONE',  ( -19.65312891409030271, 93.06504152958497400, -10.00000000000000888 ) ) ;
#33713 = DIRECTION ( 'NONE',  ( 0.000000000000000000, 0.000000000000000000, 1.000000000000000000 ) ) ;
#33714 = CARTESIAN_POINT ( 'NONE',  ( 176.2137180456981582, 292.6001369887544001, -1.126497586118241578 ) ) ;
#33715 = CARTESIAN_POINT ( 'NONE',  ( 81.62115332376640708, 55.85468755722441614, -16.37141313285761512 ) ) ;
#33716 = ORIENTED_EDGE ( 'NONE', *, *, #9515, .F. ) ;
#33717 = CARTESIAN_POINT ( 'NONE',  ( 189.2133311240501428, 265.6839626369376788, 10.75809594643768818 ) ) ;
#33719 = CARTESIAN_POINT ( 'NONE',  ( 175.7664583004113581, 278.6328268015002436, 15.45987238875895642 ) ) ;
#33718 = B_SPLINE_CURVE_WITH_KNOTS ( 'NONE', 3,
 ( #66329, #97261, #66818, #51111 ),
 .UNSPECIFIED., .F., .F.,
 ( 4, 4 ),
 ( 0.02587343813425229538, 0.03511505140344501480 ),
 .UNSPECIFIED. ) ;
#33720 = CARTESIAN_POINT ( 'NONE',  ( 168.0773408278945737, 271.5331236227465297, -17.46290692964277369 ) ) ;
#33721 = ADVANCED_FACE ( 'NONE', ( #40615 ), #71549, .F. ) ;
#33722 = EDGE_CURVE ( 'NONE', #85517, #41680, #72560, .T. ) ;
#33723 = CARTESIAN_POINT ( 'NONE',  ( 80.24736013087236586, 55.07173234547738616, 15.97097506978094650 ) ) ;
#33724 = CARTESIAN_POINT ( 'NONE',  ( 83.51092623577891061, 51.50185674319120466, -14.43088262691036583 ) ) ;
#33725 = CARTESIAN_POINT ( 'NONE',  ( 72.11718761729461846, 71.53392678631075796, -5.852761162471809442 ) ) ;
#33726 = CARTESIAN_POINT ( 'NONE',  ( 150.5916768389222682, 278.2969151622902473, -4.257825285333056330E-05 ) ) ;
#33727 = AXIS2_PLACEMENT_3D ( 'NONE', #27576, #57446, #19969 ) ;
#33728 = ORIENTED_EDGE ( 'NONE', *, *, #2526, .T. ) ;
#33729 = CARTESIAN_POINT ( 'NONE',  ( 191.0828858044439187, 280.5038866170701226, 16.76379900847850735 ) ) ;
#33730 = CARTESIAN_POINT ( 'NONE',  ( 14.68538779211344902, 8.288480858562296660, 1.475505719884397138E-15 ) ) ;
#33731 = DIRECTION ( 'NONE',  ( -0.8660254037844379305, -0.5000000000000011102, -0.000000000000000000 ) ) ;
#33732 = VERTEX_POINT ( 'NONE', #12748 ) ;
#33733 = CARTESIAN_POINT ( 'NONE',  ( 77.77576245277342082, 61.68761876588025217, 16.07113493600747844 ) ) ;
#33734 = CARTESIAN_POINT ( 'NONE',  ( 194.6356465353167948, 293.5281665672507643, -16.13180903283129197 ) ) ;
#33735 = CARTESIAN_POINT ( 'NONE',  ( 87.13707957584176711, 44.08023128113844535, -5.302241763375429073 ) ) ;
#33736 = VERTEX_POINT ( 'NONE', #64938 ) ;
#33737 = CARTESIAN_POINT ( 'NONE',  ( 79.04010335995445757, 59.81086823702358402, 16.49488376190979722 ) ) ;
#33738 = CARTESIAN_POINT ( 'NONE',  ( 187.0283284352577482, 292.0378153221775506, 12.26537691906332661 ) ) ;
#33739 = CARTESIAN_POINT ( 'NONE',  ( 150.6931560952953646, 269.6387926204777727, 14.65021044537114037 ) ) ;
#33740 = DIRECTION ( 'NONE',  ( 0.000000000000000000, 0.000000000000000000, 1.000000000000000000 ) ) ;
#33741 = AXIS2_PLACEMENT_3D ( 'NONE', #28673, #36766, #97134 ) ;
#33742 = DIRECTION ( 'NONE',  ( 0.7694697644498921241, -0.6386832404231594928, 0.000000000000000000 ) ) ;
#33743 = CARTESIAN_POINT ( 'NONE',  ( 189.4317935910015933, 300.3290466316845482, 3.295136749739974835 ) ) ;
#33744 = CARTESIAN_POINT ( 'NONE',  ( 35.77629671259011701, 179.9155109091896065, 2.679491924311254714 ) ) ;
#33745 = APPLICATION_CONTEXT ( 'automotive_design' ) ;
#33746 = ORIENTED_EDGE ( 'NONE', *, *, #7196, .T. ) ;
#33747 = EDGE_CURVE ( 'NONE', #45184, #74753, #10740, .T. ) ;
#33748 = ORIENTED_EDGE ( 'NONE', *, *, #35572, .F. ) ;
#33749 = CARTESIAN_POINT ( 'NONE',  ( 178.4554328054981056, 260.9870558088289272, 12.11472630447901544 ) ) ;
#33750 = ORIENTED_EDGE ( 'NONE', *, *, #81599, .T. ) ;
#33751 = CYLINDRICAL_SURFACE ( 'NONE', #67584, 16.60714546451156792 ) ;
#33752 = VERTEX_POINT ( 'NONE', #82173 ) ;
#33753 = CARTESIAN_POINT ( 'NONE',  ( 173.0740556585676870, 271.0053932585017265, 16.44676307064808185 ) ) ;
#33754 = CARTESIAN_POINT ( 'NONE',  ( 155.6328838216860220, 261.0829332228125850, -17.51014940606912518 ) ) ;
#33755 = ORIENTED_EDGE ( 'NONE', *, *, #51100, .F. ) ;
#33756 = EDGE_CURVE ( 'NONE', #566, #95472, #95394, .T. ) ;
#33757 = CARTESIAN_POINT ( 'NONE',  ( 82.27971551521895321, 41.21092863865097655, 3.244910409712729926 ) ) ;
#33758 = CARTESIAN_POINT ( 'NONE',  ( 80.89042375233061932, 43.66431198654377965, -9.574497798402536120 ) ) ;
#33759 = CARTESIAN_POINT ( 'NONE',  ( 161.9362388422072740, 277.2664551573698759, -12.85986196030900075 ) ) ;
#33760 = CARTESIAN_POINT ( 'NONE',  ( 193.1977289678065404, 296.0187128512746995, -12.37159405312863925 ) ) ;
#33761 = VECTOR ( 'NONE', #46216, 1000.000000000000000 ) ;
#33762 = CARTESIAN_POINT ( 'NONE',  ( 201.4617167010348737, 281.7050662241970826, -17.43131506460443703 ) ) ;
#33763 = CARTESIAN_POINT ( 'NONE',  ( 42.33744422746375591, 122.7866300363639169, -10.00000000000000000 ) ) ;
#33764 = ADVANCED_FACE ( 'NONE', ( #74551 ), #42606, .T. ) ;
#33766 = CARTESIAN_POINT ( 'NONE',  ( 154.4124318019600821, 279.5684750503268106, 2.145998202272423327 ) ) ;
#33765 = VECTOR ( 'NONE', #17129, 1000.000000000000227 ) ;
#33767 = EDGE_CURVE ( 'NONE', #60917, #46791, #33535, .T. ) ;
#33768 = CARTESIAN_POINT ( 'NONE',  ( 136.0332187963529975, 249.3458772461660544, 9.188101187500095079 ) ) ;
#33769 = ORIENTED_EDGE ( 'NONE', *, *, #6687, .F. ) ;
#33770 = CARTESIAN_POINT ( 'NONE',  ( 70.45109164464976459, 61.27252908298403611, -14.82318262686264987 ) ) ;
#33771 = CIRCLE ( 'NONE', #46673, 70.00000000000001421 ) ;
#33772 = VERTEX_POINT ( 'NONE', #34049 ) ;
#33773 = CIRCLE ( 'NONE', #54768, 0.1418229129680828593 ) ;
#33774 = EDGE_CURVE ( 'NONE', #49648, #77284, #65150, .T. ) ;
#33776 = ORIENTED_EDGE ( 'NONE', *, *, #41947, .T. ) ;
#33775 = CARTESIAN_POINT ( 'NONE',  ( 82.59110617328815351, 43.40291750172000462, -8.843653439107631797 ) ) ;
#33777 = B_SPLINE_CURVE_WITH_KNOTS ( 'NONE', 3,
 ( #3224, #2211, #87381, #55861, #78205, #85863, #16390, #25492, #71111, #8792, #1712, #79245, #95458, #49301, #48300, #39661, #33093, #47281, #70585, #40678, #86352, #71616, #63989, #33602, #94931, #56385, #17910, #41174, #2715, #11322, #59355, #18915, #28474, #73116, #34586, #50283, #4697, #35082, #81726, #20401, #88862, #65986, #11810, #36071, #42181, #75100, #95943, #12812, #44164, #82236, #3707, #97409, #65486, #27978 ),
 .UNSPECIFIED., .F., .F.,
 ( 4, 2, 2, 2, 2, 2, 2, 2, 2, 2, 2, 2, 2, 2, 2, 2, 2, 2, 2, 2, 2, 2, 2, 2, 2, 2, 4 ),
 ( 0.0006796803024578544411, 0.0008900614930580021296, 0.001100442683658149710, 0.001205633278958223500, 0.001310823874258297290, 0.001416014469558371080, 0.001521205064858445087, 0.001731586255458504413, 0.001941967446058563956, 0.002362729827258603678, 0.003204254589658812793, 0.004045779352059021908, 0.004887304114459229722, 0.005308066495659372226, 0.005518447686259440009, 0.005623638281559479105, 0.005676233579209463524, 0.005728828876859447077, 0.005781424174509430629, 0.005834019472159414181, 0.005939210067459516594, 0.006149591258059718818, 0.006570353639260159695, 0.006780734829860449522, 0.006991116020460741085, 0.007201497211061031779, 0.007411878401661323341 ),
 .UNSPECIFIED. ) ;
#33778 = CARTESIAN_POINT ( 'NONE',  ( 174.4636408308574005, 253.7873770250515406, -9.029445656122202735 ) ) ;
#33779 = CARTESIAN_POINT ( 'NONE',  ( 23.46864935082055581, 158.3759306620404743, -30.52142883766493853 ) ) ;
#33780 = CARTESIAN_POINT ( 'NONE',  ( 75.87525401958798454, 64.72722897157592570, -14.29033900848947169 ) ) ;
#33781 = CARTESIAN_POINT ( 'NONE',  ( -24.40473831032599961, 23.22649767201583515, 10.00000000000000000 ) ) ;
#33782 = CARTESIAN_POINT ( 'NONE',  ( 153.7897413227238701, 277.0882903415827627, 7.164246204486259373 ) ) ;
#33783 = CARTESIAN_POINT ( 'NONE',  ( 200.7694952279801157, 282.9040289856181403, -17.94628235092568502 ) ) ;
#33784 = DIRECTION ( 'NONE',  ( 0.000000000000000000, 0.000000000000000000, 1.000000000000000000 ) ) ;
#33785 = CARTESIAN_POINT ( 'NONE',  ( 171.4518979572709441, 280.1349275936351546, 13.78886128221634522 ) ) ;
#33786 = CARTESIAN_POINT ( 'NONE',  ( 76.46584302315547177, 51.61417680368897010, -15.65621440425051603 ) ) ;
#33787 = CARTESIAN_POINT ( 'NONE',  ( 177.6627089506813775, 255.3829110640776321, -8.402693274504045462 ) ) ;
#33788 = VECTOR ( 'NONE', #95561, 1000.000000000000000 ) ;
#33789 = ORIENTED_EDGE ( 'NONE', *, *, #87685, .F. ) ;
#33790 = CARTESIAN_POINT ( 'NONE',  ( 183.8332630652478201, 272.5615133970043757, -16.17603297288676600 ) ) ;
#33791 = CARTESIAN_POINT ( 'NONE',  ( 66.31491329446379268, 68.86277721778741068, 0.1110262474478811850 ) ) ;
#33792 = ORIENTED_EDGE ( 'NONE', *, *, #44896, .F. ) ;
#33793 = CARTESIAN_POINT ( 'NONE',  ( 163.2061145480615210, 278.0382269583403172, 13.71808048336174224 ) ) ;
#33794 = CARTESIAN_POINT ( 'NONE',  ( 47.39496755818312579, 108.2889530649357681, 10.00000000000000000 ) ) ;
#33795 = CARTESIAN_POINT ( 'NONE',  ( 191.9061344778403679, 298.2558201306721912, -9.413471345614182084 ) ) ;
#33796 = CARTESIAN_POINT ( 'NONE',  ( 148.9275518150011806, 272.6969089400084272, 12.34519124974546500 ) ) ;
#33797 = CARTESIAN_POINT ( 'NONE',  ( 162.8042930031641049, 248.6616881586264469, 11.14389129512055554 ) ) ;
#33799 = CARTESIAN_POINT ( 'NONE',  ( 151.8965004642948600, 275.2307284912582759, -8.622094983838675120 ) ) ;
#33798 = CARTESIAN_POINT ( 'NONE',  ( -50.41871976035449165, 31.58591985673633928, -10.00000000000000000 ) ) ;
#33800 = AXIS2_PLACEMENT_3D ( 'NONE', #48639, #79573, #95284 ) ;
#33801 = ORIENTED_EDGE ( 'NONE', *, *, #85707, .F. ) ;
#33802 = B_SPLINE_SURFACE_WITH_KNOTS ( 'NONE', 3, 1, ( 
 ( #47647, #16261 ),
 ( #68956, #54745 ),
 ( #85732, #47153 ),
 ( #78584, #61848 ),
 ( #1072, #29966 ),
 ( #91805, #38552 ),
 ( #568, #53263 ),
 ( #92796, #61356 ),
 ( #23350, #54236 ),
 ( #14765, #30464 ),
 ( #8171, #85206 ),
 ( #92311, #22861 ),
 ( #53745, #46141 ),
 ( #39041, #31451 ),
 ( #84704, #8664 ),
 ( #39536, #31951 ),
 ( #62853, #71484 ),
 ( #11681, #79105 ),
 ( #26373, #19294 ),
 ( #9688, #63861 ),
 ( #49655, #42054 ),
 ( #95820, #95327 ),
 ( #57250, #10176 ),
 ( #48164, #72990 ),
 ( #64874, #57748 ),
 ( #11188, #56251 ),
 ( #41551, #79612 ),
 ( #50161, #2584 ),
 ( #3582, #94799 ),
 ( #70984, #48679 ),
 ( #34462, #10674 ) ),
 .UNSPECIFIED., .F., .F., .F.,
 ( 4, 3, 3, 3, 3, 3, 3, 3, 3, 3, 4 ),
 ( 2, 2 ),
 ( 0.000000000000000000, 0.1333490885032317108, 0.3007194338854392579, 0.4699862290245125918, 0.5844252810809411613, 0.6686540514502808952, 0.7354980260655639146, 0.8028463152565747940, 0.8633854507757208196, 0.9437142632667219200, 1.000000000000000000 ),
 ( 0.000000000000000000, 1.000000000000000000 ),
 .UNSPECIFIED. ) ;
#33803 = CARTESIAN_POINT ( 'NONE',  ( 70.51282955450930956, 62.70216424510687148, -13.59275263340693130 ) ) ;
#33804 = CARTESIAN_POINT ( 'NONE',  ( 193.4149181402707995, 276.1162583725824788, -16.31078380200698064 ) ) ;
#33805 = CARTESIAN_POINT ( 'NONE',  ( 75.20365466289253220, 64.98199045542118313, -13.95732831142939467 ) ) ;
#33806 = CARTESIAN_POINT ( 'NONE',  ( 192.6224552386041182, 297.0151161785129261, 12.49354144254605181 ) ) ;
#33807 = CARTESIAN_POINT ( 'NONE',  ( 80.77766742949400225, 43.16040824514890772, -9.863399489045445279 ) ) ;
#33808 = CARTESIAN_POINT ( 'NONE',  ( 66.99589590513352277, 68.94589010804261875, 3.022793341730511063 ) ) ;
#33809 = CARTESIAN_POINT ( 'NONE',  ( -6.887775800123916881, 157.6423013555410080, -4.594050593750043987 ) ) ;
#33810 = CARTESIAN_POINT ( 'NONE',  ( 155.1865148098964937, 261.8560670301561686, -16.99758927948949605 ) ) ;
#33811 = CARTESIAN_POINT ( 'NONE',  ( 88.07382696622103424, 44.71549268748395889, -4.363432358687163060 ) ) ;
#33812 = DIRECTION ( 'NONE',  ( -0.000000000000000000, -0.000000000000000000, -1.000000000000000000 ) ) ;
#33813 = CARTESIAN_POINT ( 'NONE',  ( 178.6034478761426101, 280.7652058965896344, -16.81717848226262291 ) ) ;
#33814 = CARTESIAN_POINT ( 'NONE',  ( 75.13760321359936256, 55.20964237971745803, -16.13749542340338294 ) ) ;
#33815 = CARTESIAN_POINT ( 'NONE',  ( 162.4375581431960427, 282.5611924947268108, 5.618517507943365352 ) ) ;
#33817 = CARTESIAN_POINT ( 'NONE',  ( 162.6396274730868186, 248.9468972229755082, -10.26162218571527518 ) ) ;
#33816 = CARTESIAN_POINT ( 'NONE',  ( 190.4202270817170017, 300.3952711937946560, -0.8604814952887831492 ) ) ;
#33818 = CARTESIAN_POINT ( 'NONE',  ( 207.3608985824721174, 271.4873834824583128, 4.969352111496849744 ) ) ;
#33819 = CARTESIAN_POINT ( 'NONE',  ( 164.7307586990986863, 245.3249516942294122, -5.338649886695495894 ) ) ;
#33820 = CARTESIAN_POINT ( 'NONE',  ( 75.53863029606473845, 55.96446735458120969, -16.15547972021748180 ) ) ;
#33821 = CARTESIAN_POINT ( 'NONE',  ( 74.15479259499207387, 55.62765001666249276, -16.59030973340311022 ) ) ;
#33822 = CARTESIAN_POINT ( 'NONE',  ( 180.9235756063633858, 293.2599282431580718, -8.659743166530571301 ) ) ;
#33823 = CARTESIAN_POINT ( 'NONE',  ( 73.53729735990698657, 69.85633680769765874, 9.839233502311348190 ) ) ;
#33824 = CARTESIAN_POINT ( 'NONE',  ( 54.35637144981559743, 196.0643266524159856, -9.188101187500093303 ) ) ;
#33825 = CARTESIAN_POINT ( 'NONE',  ( 76.69634485559663517, 63.33187278031594758, -15.42689205524521157 ) ) ;
#33826 = AXIS2_PLACEMENT_3D ( 'NONE', #38350, #63161, #24166 ) ;
#33827 = CARTESIAN_POINT ( 'NONE',  ( 71.13526655237410523, 218.0024278399160664, 9.188101187500095079 ) ) ;
#33828 = CARTESIAN_POINT ( 'NONE',  ( 161.1750406344237661, 251.4836360396366501, -14.21198410781773802 ) ) ;
#33829 = EDGE_CURVE ( 'NONE', #1860, #26784, #49868, .T. ) ;
#33830 = AXIS2_PLACEMENT_3D ( 'NONE', #76887, #38380, #69293 ) ;
#33831 = DIRECTION ( 'NONE',  ( 0.4999999999999998890, -0.8660254037844385966, 0.000000000000000000 ) ) ;
#33833 = CARTESIAN_POINT ( 'NONE',  ( 37.34220537994157496, 54.61056725541210710, -10.00000000000000000 ) ) ;
#33832 = CARTESIAN_POINT ( 'NONE',  ( 197.4842693130445923, 286.5942071846287149, -17.75505217046438489 ) ) ;
#33834 = CIRCLE ( 'NONE', #51603, 0.5000000000000004441 ) ;
#33835 = CARTESIAN_POINT ( 'NONE',  ( 176.6803982052660160, 270.1099931746196035, -17.20834088444772902 ) ) ;
#33836 = CARTESIAN_POINT ( 'NONE',  ( 37.28583507901048222, 30.03085787977765975, 9.188101187500006262 ) ) ;
#33837 = CARTESIAN_POINT ( 'NONE',  ( 128.4003070610459929, 256.4860189848785694, -2.679491924311252493 ) ) ;
#33838 = DIRECTION ( 'NONE',  ( -0.000000000000000000, -0.000000000000000000, -1.000000000000000000 ) ) ;
#33839 = ORIENTED_EDGE ( 'NONE', *, *, #77682, .F. ) ;
#33840 = CARTESIAN_POINT ( 'NONE',  ( 18.38602693954342371, 22.56628583063840310, 9.188101187500006262 ) ) ;
#33841 = CARTESIAN_POINT ( 'NONE',  ( 77.73871025623044773, 221.8149278399160664, -9.188101187500095079 ) ) ;
#33842 = DIRECTION ( 'NONE',  ( 0.2938926261462335709, -0.5090369604551240323, 0.8090169943749504489 ) ) ;
#33843 = VECTOR ( 'NONE', #57429, 1000.000000000000114 ) ;
#33844 = CARTESIAN_POINT ( 'NONE',  ( 169.6038083371201992, 288.1641641989402842, -1.090344386142415578 ) ) ;
#33845 = CARTESIAN_POINT ( 'NONE',  ( 192.5284579606305613, 297.1779242397361713, -13.15228012403107272 ) ) ;
#33846 = DIRECTION ( 'NONE',  ( 0.8660254037844385966, 0.4999999999999999445, -5.782411586589351229E-17 ) ) ;
#33848 = EDGE_LOOP ( 'NONE', ( #64503, #62916, #50179, #50626, #90066 ) ) ;
#33847 = EDGE_CURVE ( 'NONE', #93728, #55151, #40897, .T. ) ;
#33849 = EDGE_CURVE ( 'NONE', #25515, #29839, #13123, .T. ) ;
#33850 = CARTESIAN_POINT ( 'NONE',  ( 48.58805178314242568, 84.67719436603331928, -10.00000000000000000 ) ) ;
#33851 = CARTESIAN_POINT ( 'NONE',  ( 193.8458974004921060, 288.0417099115973656, 16.67148095953266917 ) ) ;
#33852 = CARTESIAN_POINT ( 'NONE',  ( 72.51472823790616928, 71.58500209747694498, 5.264689056060205097 ) ) ;
#33854 = CARTESIAN_POINT ( 'NONE',  ( 87.27117856089937220, 44.98890866680353895, -6.231534082530008511 ) ) ;
#33853 = AXIS2_PLACEMENT_3D ( 'NONE', #86143, #31369, #25271 ) ;
#33855 = CARTESIAN_POINT ( 'NONE',  ( 117.8737486125219505, 248.8615022471903160, 5.000000000000046185 ) ) ;
#33856 = CARTESIAN_POINT ( 'NONE',  ( 12.94829542258092658, 189.8297689869269504, -2.679491924311252493 ) ) ;
#33857 = CARTESIAN_POINT ( 'NONE',  ( 74.99170170892071496, 53.13635499159778419, 16.50622363577149443 ) ) ;
#33858 = ORIENTED_EDGE ( 'NONE', *, *, #33173, .T. ) ;
#33859 = CARTESIAN_POINT ( 'NONE',  ( 165.5488484770429523, 246.8969043953118785, -1.737601649715255991 ) ) ;
#33860 = EDGE_LOOP ( 'NONE', ( #937, #46517, #51814, #14412 ) ) ;
#33861 = CARTESIAN_POINT ( 'NONE',  ( 202.4017613376760494, 280.0768611521521620, 15.73960524502980540 ) ) ;
#33862 = CYLINDRICAL_SURFACE ( 'NONE', #22311, 10.00000000000010658 ) ;
#33863 = CARTESIAN_POINT ( 'NONE',  ( 48.21858077004885246, 104.0489273421469818, 10.00000000000000000 ) ) ;
#33864 = ORIENTED_EDGE ( 'NONE', *, *, #17444, .F. ) ;
#33865 = CARTESIAN_POINT ( 'NONE',  ( 31.25085430583858681, 200.3967562850347122, -4.648177544792955347E-16 ) ) ;
#33866 = ORIENTED_EDGE ( 'NONE', *, *, #89149, .F. ) ;
#33867 = CARTESIAN_POINT ( 'NONE',  ( -54.45295541630240166, 33.76759809053437067, -10.00000000000000000 ) ) ;
#33868 = CARTESIAN_POINT ( 'NONE',  ( 41.06812061084161769, 204.5177522451419350, 5.000000000000046185 ) ) ;
#33869 = CARTESIAN_POINT ( 'NONE',  ( 153.4613150239306094, 264.8442007126561748, -16.86932470306368259 ) ) ;
#33870 = AXIS2_PLACEMENT_3D ( 'NONE', #95553, #95034, #79833 ) ;
#33871 = EDGE_LOOP ( 'NONE', ( #13711, #87253, #94076, #28090 ) ) ;
#33872 = CARTESIAN_POINT ( 'NONE',  ( 26.65419051621551461, 38.49540643055189548, 3.479690158560446702E-15 ) ) ;
#33873 = CARTESIAN_POINT ( 'NONE',  ( 83.24863284446355749, 48.31717972554097429, -12.63386792366998534 ) ) ;
#33874 = CARTESIAN_POINT ( 'NONE',  ( 74.14312167556930433, 66.30466486950707861, 1.224646799147354045E-15 ) ) ;
#33875 = CARTESIAN_POINT ( 'NONE',  ( 52.48883062679690426, 191.1115022471902023, -5.000000000000041744 ) ) ;
#33876 = ORIENTED_EDGE ( 'NONE', *, *, #68895, .T. ) ;
#33877 = ORIENTED_EDGE ( 'NONE', *, *, #6422, .T. ) ;
#33878 = LINE ( 'NONE', #11073, #62185 ) ;
#33879 = EDGE_CURVE ( 'NONE', #94756, #21068, #71270, .T. ) ;
#33881 = CARTESIAN_POINT ( 'NONE',  ( 194.3708539535661259, 293.9868007723104029, -16.01585187499628304 ) ) ;
#33880 = CARTESIAN_POINT ( 'NONE',  ( 68.13224077221879327, 65.78494403969656901, 10.87017445448774033 ) ) ;
#33882 = CARTESIAN_POINT ( 'NONE',  ( 85.29362735876655677, 48.41412782346650800, 12.38048700662147716 ) ) ;
#33883 = CARTESIAN_POINT ( 'NONE',  ( 155.5770330754656072, 261.1796695529068302, 18.26969263326161297 ) ) ;
#33884 = LINE ( 'NONE', #92102, #47977 ) ;
#33885 = CARTESIAN_POINT ( 'NONE',  ( 187.2429337685844359, 291.3981873160698228, -14.13502898539333508 ) ) ;
#33886 = CARTESIAN_POINT ( 'NONE',  ( 208.0844008978733086, 270.2342407127895285, -4.836932903224296254 ) ) ;
#33887 = CARTESIAN_POINT ( 'NONE',  ( 166.1759841011777610, 265.4597452293433548, 16.55821447247043920 ) ) ;
#33888 = CARTESIAN_POINT ( 'NONE',  ( 79.19335676987149952, 59.81345803429233143, 16.50342877771832661 ) ) ;
#33889 = EDGE_CURVE ( 'NONE', #100289, #82522, #45736, .T. ) ;
#33890 = CARTESIAN_POINT ( 'NONE',  ( 87.02133327910362937, 230.2369531367911009, -4.594050593750048428 ) ) ;
#33891 = ORIENTED_EDGE ( 'NONE', *, *, #67961, .T. ) ;
#33893 = B_SPLINE_CURVE_WITH_KNOTS ( 'NONE', 3,
 ( #83394, #75778, #6365, #99074, #91487, #22050, #52950, #14462, #45344, #92005, #84389, #45826, #7342, #38225, #69141, #1131, #88787, #17838, #64426, #41609, #2137, #42112, #73046, #49717 ),
 .UNSPECIFIED., .F., .F.,
 ( 4, 2, 2, 2, 2, 2, 2, 2, 2, 2, 2, 4 ),
 ( 0.000000000000000000, 0.1249999999999997780, 0.2499999999999995559, 0.3749999999999987788, 0.4374999999999988898, 0.4999999999999990008, 0.5624999999999991118, 0.6249999999999992228, 0.6874999999999993339, 0.7499999999999994449, 0.8749999999999996669, 1.000000000000000000 ),
 .UNSPECIFIED. ) ;
#33892 = CARTESIAN_POINT ( 'NONE',  ( 150.6790040019602088, 269.6633047651677089, 15.38315204620803378 ) ) ;
#33894 = CARTESIAN_POINT ( 'NONE',  ( 166.3356402791620781, 279.2072638237854676, -13.54689619094178177 ) ) ;
#33895 = EDGE_LOOP ( 'NONE', ( #84934, #67380, #98125, #48550 ) ) ;
#33896 = ORIENTED_EDGE ( 'NONE', *, *, #93357, .F. ) ;
#33897 = CARTESIAN_POINT ( 'NONE',  ( -89.11465314115667979, 93.37593066204033221, -30.52142883766496695 ) ) ;
#33898 = EDGE_CURVE ( 'NONE', #749, #42575, #55189, .T. ) ;
#33899 = CARTESIAN_POINT ( 'NONE',  ( -59.65739779450132829, 37.15562860896454112, -10.00000000000000000 ) ) ;
#33900 = DIRECTION ( 'NONE',  ( -1.000000000000000000, 0.000000000000000000, 0.000000000000000000 ) ) ;
#33901 = CARTESIAN_POINT ( 'NONE',  ( 159.2536436069973718, 254.8115933126508992, -15.76697951715411250 ) ) ;
#33902 = DIRECTION ( 'NONE',  ( 1.110223024625156343E-15, -1.000000000000000000, 0.000000000000000000 ) ) ;
#33903 = CARTESIAN_POINT ( 'NONE',  ( 85.18102929606172324, 229.1744531367911293, 4.594050593750047540 ) ) ;
#33904 = ORIENTED_EDGE ( 'NONE', *, *, #26037, .F. ) ;
#33905 = CARTESIAN_POINT ( 'NONE',  ( 207.6555576926778883, 270.9770189326688410, -1.235081510489080436 ) ) ;
#33906 = ORIENTED_EDGE ( 'NONE', *, *, #68021, .F. ) ;
#33907 = CARTESIAN_POINT ( 'NONE',  ( 24.41587626779758580, 32.83478043621389020, -8.090169943749479842 ) ) ;
#33908 = CARTESIAN_POINT ( 'NONE',  ( 72.72501144050022504, 69.27512644744767556, -9.364870738290214547 ) ) ;
#33909 = LINE ( 'NONE', #47208, #1064 ) ;
#33910 = CARTESIAN_POINT ( 'NONE',  ( -17.74943806285152448, 173.8927522451419634, 2.944929066748280225E-16 ) ) ;
#33911 = CARTESIAN_POINT ( 'NONE',  ( 87.98321614449201888, 44.37542847539244661, 4.756797044073171499 ) ) ;
#33912 = VECTOR ( 'NONE', #56205, 1000.000000000000000 ) ;
#33913 = ORIENTED_EDGE ( 'NONE', *, *, #64126, .T. ) ;
#33914 = CARTESIAN_POINT ( 'NONE',  ( 87.73337331461395650, 44.19923036242353476, -3.116042966821523041 ) ) ;
#33915 = CARTESIAN_POINT ( 'NONE',  ( 160.6448124520779288, 275.6763703598426787, 14.01705192569017022 ) ) ;
#33916 = CARTESIAN_POINT ( 'NONE',  ( 82.32665380160997870, 40.35341351610614424, -1.168632817617336839 ) ) ;
#33917 = CARTESIAN_POINT ( 'NONE',  ( -34.16292631813981728, 25.86630820016799248, 10.00000000000000000 ) ) ;
#33918 = CARTESIAN_POINT ( 'NONE',  ( 48.21858077004885246, 104.0489273421469818, -10.00000000000000000 ) ) ;
#33919 = DIRECTION ( 'NONE',  ( 0.4999999999999998890, -0.8660254037844385966, 0.000000000000000000 ) ) ;
#33920 = ADVANCED_FACE ( 'NONE', ( #1528 ), #46382, .F. ) ;
#33921 = CYLINDRICAL_SURFACE ( 'NONE', #58255, 17.82106496071139645 ) ;
#33922 = CARTESIAN_POINT ( 'NONE',  ( 202.7282074973916792, 277.5114398175890642, -15.40750263959311184 ) ) ;
#33923 = VECTOR ( 'NONE', #20172, 1000.000000000000000 ) ;
#33924 =( BOUNDED_CURVE ( )  B_SPLINE_CURVE ( 2, ( #17183, #62269, #61782, #10, #23786, #62781, #38480, #93225, #78511, #76508, #92729, #54671, #39464 ),
 .UNSPECIFIED., .F., .T. ) 
 B_SPLINE_CURVE_WITH_KNOTS ( ( 3, 2, 2, 2, 2, 2, 3 ),
 ( 0.8625000000000000444, 0.8649999999999999911, 0.8699999999999999956, 0.8750000000000000000, 0.8800000000000000044, 0.8850000000000000089, 0.8875000000000000666 ),
 .UNSPECIFIED. ) 
 CURVE ( )  GEOMETRIC_REPRESENTATION_ITEM ( )  RATIONAL_B_SPLINE_CURVE ( ( 0.9755282581475767101, 0.9755282581475772652, 1.000000000000000000, 0.9510565162951535312, 1.000000000000000000, 0.9510565162951535312, 1.000000000000000000, 0.9510565162951535312, 1.000000000000000000, 0.9510565162951535312, 1.000000000000000000, 0.9755282581475761550, 0.9755282581475767101 ) ) 
 REPRESENTATION_ITEM ( '' )  );
#33925 = CARTESIAN_POINT ( 'NONE',  ( 161.7910648966377209, 250.4166507187868831, 13.19274492748169436 ) ) ;
#33926 = CARTESIAN_POINT ( 'NONE',  ( 83.57754660192708229, 42.00176330557154358, 3.549989893534491792 ) ) ;
#33927 = CARTESIAN_POINT ( 'NONE',  ( 13.95435611255089725, 31.55466486950698268, -1.111400068045478839E-16 ) ) ;
#33928 = CARTESIAN_POINT ( 'NONE',  ( 78.17938457032805388, 61.84587351074209494, 15.72953426550225942 ) ) ;
#33929 = CARTESIAN_POINT ( 'NONE',  ( 109.1931406464380530, 245.3967562850346837, -4.648177544792955347E-16 ) ) ;
#33930 = ADVANCED_FACE ( 'NONE', ( #64008 ), #17407, .F. ) ;
#33931 = CARTESIAN_POINT ( 'NONE',  ( 202.3349865675690182, 280.1925184466412020, -15.80981137687728655 ) ) ;
#33932 = CARTESIAN_POINT ( 'NONE',  ( 76.73689447628605365, 63.01357867417375758, -15.17253155338367954 ) ) ;
#33933 = CARTESIAN_POINT ( 'NONE',  ( 182.1361237887369668, 264.3643447715849106, 13.55130394885500067 ) ) ;
#33934 = CARTESIAN_POINT ( 'NONE',  ( 199.2404585781709443, 281.6525708895557614, -16.58724268975067062 ) ) ;
#33935 = CARTESIAN_POINT ( 'NONE',  ( 38.51867309874058520, 23.20801979619931643, -3.090169943749474069 ) ) ;
#33936 = CARTESIAN_POINT ( 'NONE',  ( 78.33040301246538206, 47.74919695098484596, 13.91169181636929864 ) ) ;
#33938 = CARTESIAN_POINT ( 'NONE',  ( 155.5066938333533528, 261.3015006940112244, -18.40036130547566273 ) ) ;
#33937 =( BOUNDED_CURVE ( )  B_SPLINE_CURVE ( 2, ( #66991, #90350, #60373, #45186, #60870, #98422, #68484, #20930, #97430 ),
 .UNSPECIFIED., .F., .T. ) 
 B_SPLINE_CURVE_WITH_KNOTS ( ( 3, 2, 2, 2, 3 ),
 ( 0.6330645161290322509, 0.6344086021505376261, 0.6370967741935483764, 0.6397849462365591267, 0.6411290322580645018 ),
 .UNSPECIFIED. ) 
 CURVE ( )  GEOMETRIC_REPRESENTATION_ITEM ( )  RATIONAL_B_SPLINE_CURVE ( ( 0.9330127018922194093, 0.9330127018922194093, 1.000000000000000000, 0.8660254037844387076, 1.000000000000000000, 0.8660254037844387076, 1.000000000000000000, 0.9330127018922194093, 0.9330127018922194093 ) ) 
 REPRESENTATION_ITEM ( '' )  );
#33939 = FACE_OUTER_BOUND ( 'NONE', #41124, .T. ) ;
#33940 = CARTESIAN_POINT ( 'NONE',  ( 158.7260864440790726, 271.6582352343255025, -14.71012893904847729 ) ) ;
#33941 = CARTESIAN_POINT ( 'NONE',  ( 206.0345876666409026, 273.1343529140784767, -9.309084676637942479 ) ) ;
#33942 = CARTESIAN_POINT ( 'NONE',  ( 207.1572261440131797, 271.8401544939704877, -5.633070628900782140 ) ) ;
#33943 = CARTESIAN_POINT ( 'NONE',  ( 17.11727908708474288, 174.5643266524160424, 9.188101187500095079 ) ) ;
#33944 = CARTESIAN_POINT ( 'NONE',  ( 83.07383449898573247, 51.69909393465605518, 14.61845402798252636 ) ) ;
#33945 = ORIENTED_EDGE ( 'NONE', *, *, #10578, .T. ) ;
#33946 = CARTESIAN_POINT ( 'NONE',  ( 86.82730862513506054, 46.47781937394018570, 9.057350913429045747 ) ) ;
#33947 = DIRECTION ( 'NONE',  ( 0.3956464567955564338, -0.9184028970038813355, 0.000000000000000000 ) ) ;
#33948 = CARTESIAN_POINT ( 'NONE',  ( 82.00582843356828278, 41.75518532697849139, 5.420714220595918675 ) ) ;
#33949 = CARTESIAN_POINT ( 'NONE',  ( 43.26059451170998926, 183.5327760586659451, 1.948934522072302763E-15 ) ) ;
#33950 = CARTESIAN_POINT ( 'NONE',  ( 87.19358828159984398, 46.06351791880832991, 8.846884648199045742 ) ) ;
#33951 = CARTESIAN_POINT ( 'NONE',  ( 146.9376205018946848, 276.1435710778808925, 5.066564108429441937 ) ) ;
#33952 = CARTESIAN_POINT ( 'NONE',  ( 40.97195624589149077, 25.78380873178790011, -6.180339887498949025 ) ) ;
#33953 = CARTESIAN_POINT ( 'NONE',  ( 178.4805636753592353, 291.7095812787227374, 5.876746774786301586 ) ) ;
#33954 = CARTESIAN_POINT ( 'NONE',  ( 178.4024347723586459, 293.9091254782996430, 2.739406101672524851 ) ) ;
#33955 = CARTESIAN_POINT ( 'NONE',  ( 149.5479608754428114, 271.6223289258474551, 11.58749366327964303 ) ) ;
#33956 = CARTESIAN_POINT ( 'NONE',  ( 182.5885846253425768, 280.2995767727080079, -16.09058154987042855 ) ) ;
#33957 = CARTESIAN_POINT ( 'NONE',  ( 81.37766082491019404, 41.99711756777615079, 7.787696445709868520 ) ) ;
#33958 = CARTESIAN_POINT ( 'NONE',  ( 86.76444126019433156, 45.86660341771495553, -8.261827951889216592 ) ) ;
#33959 = DIRECTION ( 'NONE',  ( 0.000000000000000000, 0.000000000000000000, -1.000000000000000000 ) ) ;
#33960 = EDGE_CURVE ( 'NONE', #41197, #39035, #19171, .T. ) ;
#33961 = EDGE_CURVE ( 'NONE', #3380, #20756, #56383, .T. ) ;
#33962 = CARTESIAN_POINT ( 'NONE',  ( 182.5686778644665083, 296.6873302901632314, 1.787712280751329708 ) ) ;
#33963 = CARTESIAN_POINT ( 'NONE',  ( 88.86189758574333553, 212.1115022471902023, -5.000000000000041744 ) ) ;
#33964 = CARTESIAN_POINT ( 'NONE',  ( 75.66892512706360208, 65.56297878460881634, -13.78772485324686237 ) ) ;
#33965 = LINE ( 'NONE', #50625, #46586 ) ;
#33966 = EDGE_CURVE ( 'NONE', #67335, #30385, #100150, .T. ) ;
#33967 = CARTESIAN_POINT ( 'NONE',  ( 46.23738328933649200, 191.3768266524159856, -9.188101187500091527 ) ) ;
#33968 = CARTESIAN_POINT ( 'NONE',  ( 159.3528137482544196, 254.6398255893999476, 16.73628156321660398 ) ) ;
#33969 = ORIENTED_EDGE ( 'NONE', *, *, #53279, .T. ) ;
#33970 = CARTESIAN_POINT ( 'NONE',  ( 162.8271773159503937, 263.3686283302618563, 17.75290566180205687 ) ) ;
#33971 = CARTESIAN_POINT ( 'NONE',  ( 147.5693121967435957, 275.0494489676833041, 4.210973343677100189 ) ) ;
#33973 = CARTESIAN_POINT ( 'NONE',  ( 67.57495667756568025, 66.81435014269607109, -8.472947009434754762 ) ) ;
#33972 = CIRCLE ( 'NONE', #24264, 15.60714546451156970 ) ;
#33974 = ORIENTED_EDGE ( 'NONE', *, *, #78367, .F. ) ;
#33975 = CARTESIAN_POINT ( 'NONE',  ( 167.5658046615882597, 285.5733867727782354, 7.972160045818313279 ) ) ;
#33976 = CARTESIAN_POINT ( 'NONE',  ( 164.3706594650489023, 245.9486618633701482, -1.665857659249071698 ) ) ;
#33977 = CARTESIAN_POINT ( 'NONE',  ( 147.1495358447521369, 275.7765229371483997, 6.477374713577704668 ) ) ;
#33978 = CARTESIAN_POINT ( 'NONE',  ( 190.7608863809561797, 298.9511920904263320, -7.863160954977485240 ) ) ;
#33979 = CARTESIAN_POINT ( 'NONE',  ( 23.19008890107777177, 36.49540643055188838, 3.479690158560446702E-15 ) ) ;
#33980 = CARTESIAN_POINT ( 'NONE',  ( 202.2773826701151165, 280.2922913237452462, 16.62862787739668846 ) ) ;
#33981 = CARTESIAN_POINT ( 'NONE',  ( 196.2878005184348353, 290.6665519265632724, -16.69183432842427806 ) ) ;
#33982 = CARTESIAN_POINT ( 'NONE',  ( 204.4735667670548764, 276.4883888850707763, 14.55282211540290227 ) ) ;
#33983 = ORIENTED_EDGE ( 'NONE', *, *, #2, .T. ) ;
#33984 = CARTESIAN_POINT ( 'NONE',  ( 17.47068606603513530, 15.80170272979925628, 7.433330006724137462 ) ) ;
#33985 = CARTESIAN_POINT ( 'NONE',  ( 58.43017357788681210, 217.8207943907112849, -17.47570218321535052 ) ) ;
#33986 = DIRECTION ( 'NONE',  ( -0.8916269620120498285, 0.4527707594502571875, 0.000000000000000000 ) ) ;
#33987 = ORIENTED_EDGE ( 'NONE', *, *, #30144, .F. ) ;
#33988 = CARTESIAN_POINT ( 'NONE',  ( 179.4777768328064269, 283.0882700270193482, 16.09770196021716515 ) ) ;
#33989 = CARTESIAN_POINT ( 'NONE',  ( 191.1489696025915919, 299.5672681643093256, 8.892130899335590755 ) ) ;
#33990 = CARTESIAN_POINT ( 'NONE',  ( 177.7013443376605437, 255.3287069125248365, -6.832982159536398648 ) ) ;
#33991 = DIRECTION ( 'NONE',  ( -0.6911977992267138715, 0.7226656227773308183, 0.000000000000000000 ) ) ;
#33992 = EDGE_LOOP ( 'NONE', ( #90228, #68969, #69146, #46149 ) ) ;
#33993 = VECTOR ( 'NONE', #33553, 1000.000000000000000 ) ;
#33994 = ORIENTED_EDGE ( 'NONE', *, *, #95050, .F. ) ;
#33995 = ADVANCED_FACE ( 'NONE', ( #72128 ), #97915, .T. ) ;
#33996 = CARTESIAN_POINT ( 'NONE',  ( 207.1770866921659717, 271.8057550155037347, -5.569195235244989384 ) ) ;
#33997 = CARTESIAN_POINT ( 'NONE',  ( 196.8435556370661459, 289.7039558245273838, -16.43899056939217118 ) ) ;
#33998 = ORIENTED_EDGE ( 'NONE', *, *, #63681, .T. ) ;
#33999 = CARTESIAN_POINT ( 'NONE',  ( 153.0308080659177392, 265.5898606369461277, -17.74682723936668438 ) ) ;
#34000 = CARTESIAN_POINT ( 'NONE',  ( 159.6978881494930249, 254.0421391940632532, 15.34888828951022610 ) ) ;
#34001 = CARTESIAN_POINT ( 'NONE',  ( 72.61487623500035227, 57.17883103660691546, -16.35891038744556525 ) ) ;
#34002 = CARTESIAN_POINT ( 'NONE',  ( 78.40116303218597693, 61.34120641638568827, -15.86691968629957650 ) ) ;
#34003 = CARTESIAN_POINT ( 'NONE',  ( 157.3661765229227285, 258.0807821998820373, -18.27254492731150748 ) ) ;
#34004 = CARTESIAN_POINT ( 'NONE',  ( 105.5326262849960131, 240.9244531367911293, -4.594050593750046652 ) ) ;
#34005 = CARTESIAN_POINT ( 'NONE',  ( 149.1429535397850827, 272.3238222086447990, -12.91457852089092384 ) ) ;
#34006 = CARTESIAN_POINT ( 'NONE',  ( 184.1161166760942649, 288.9931618037095973, -13.06163573803795686 ) ) ;
#34007 = ORIENTED_EDGE ( 'NONE', *, *, #38335, .T. ) ;
#34008 = CARTESIAN_POINT ( 'NONE',  ( 207.8060684685902686, 270.7163266217015689, 2.015725026008670540 ) ) ;
#34009 = EDGE_LOOP ( 'NONE', ( #44802, #23494, #13649, #62769 ) ) ;
#34010 = CARTESIAN_POINT ( 'NONE',  ( 36.08541434599421649, 23.76004757982091320, 5.678558825948272215 ) ) ;
#34011 = CARTESIAN_POINT ( 'NONE',  ( 157.6466783816650832, 259.5949387289228412, 17.71616314254395519 ) ) ;
#34012 = CARTESIAN_POINT ( 'NONE',  ( 78.33244564584110492, 47.97788310747041152, -14.02544125455132651 ) ) ;
#34013 = CARTESIAN_POINT ( 'NONE',  ( 63.34103791831415009, 213.5024278399160949, 9.188101187500095079 ) ) ;
#34014 = CARTESIAN_POINT ( 'NONE',  ( 74.13497556468038852, 68.62018799133311120, 11.47049235834078296 ) ) ;
#34015 = CARTESIAN_POINT ( 'NONE',  ( 191.5766842709549280, 298.8264446275616137, 8.039910086100929831 ) ) ;
#34016 = CARTESIAN_POINT ( 'NONE',  ( 150.9195128607351251, 269.2467312020988857, 13.93698123781031484 ) ) ;
#34017 = CARTESIAN_POINT ( 'NONE',  ( 176.5965672854825925, 273.2588103071500427, 17.23532591839911277 ) ) ;
#34018 = ORIENTED_EDGE ( 'NONE', *, *, #34195, .T. ) ;
#34019 = CARTESIAN_POINT ( 'NONE',  ( 43.35468487962021555, 120.5828561944265687, 10.00000000000000000 ) ) ;
#34020 = CARTESIAN_POINT ( 'NONE',  ( 77.89397139995216435, 52.97378536012750061, 16.25196429188360625 ) ) ;
#34021 = VERTEX_POINT ( 'NONE', #12829 ) ;
#34022 = CARTESIAN_POINT ( 'NONE',  ( 70.16674147172682297, 69.76683255227192149, -6.105712478908892571 ) ) ;
#34023 = CARTESIAN_POINT ( 'NONE',  ( 207.7296438747196134, 270.8486979012336633, -6.692930657757584001 ) ) ;
#34024 = CARTESIAN_POINT ( 'NONE',  ( 79.77196807731678518, 53.06786404022832215, -16.06017792100006503 ) ) ;
#34025 = CARTESIAN_POINT ( 'NONE',  ( 190.6094661480870798, 300.5017155583701083, 4.598210453186021951 ) ) ;
#34026 = EDGE_CURVE ( 'NONE', #21258, #78457, #36060, .T. ) ;
#34027 = CARTESIAN_POINT ( 'NONE',  ( 180.3226476666923190, 271.1461042115498685, 16.43934610314749634 ) ) ;
#34028 = CARTESIAN_POINT ( 'NONE',  ( 164.8616299252405213, 245.0982760813026857, 1.544363874765093625 ) ) ;
#34029 = FACE_OUTER_BOUND ( 'NONE', #43685, .T. ) ;
#34030 = CARTESIAN_POINT ( 'NONE',  ( 164.1196843314846774, 253.9561035179159205, 14.46087810102053517 ) ) ;
#34031 = CARTESIAN_POINT ( 'NONE',  ( 208.0287371622045782, 270.3306531311065442, 3.558879245883286746 ) ) ;
#34032 = CARTESIAN_POINT ( 'NONE',  ( 120.4987145680870952, 246.5024278399160949, 9.188101187500095079 ) ) ;
#34033 = VERTEX_POINT ( 'NONE', #98912 ) ;
#34034 = CARTESIAN_POINT ( 'NONE',  ( 146.5913834600193582, 276.7432712258716947, -0.4909717733184599253 ) ) ;
#34035 = CARTESIAN_POINT ( 'NONE',  ( -35.25453232515824453, 42.38837410636706693, 59.99999999999999289 ) ) ;
#34036 = CARTESIAN_POINT ( 'NONE',  ( 203.0026270830780675, 279.0361311525880978, -16.61345826058821373 ) ) ;
#34037 = CARTESIAN_POINT ( 'NONE',  ( 79.50492434327871649, 59.51147149025595695, -16.19819612084857496 ) ) ;
#34038 = CARTESIAN_POINT ( 'NONE',  ( 74.27219104505947200, 58.60180873485686703, 15.82987398880578134 ) ) ;
#34039 = DIRECTION ( 'NONE',  ( -0.000000000000000000, -0.000000000000000000, -1.000000000000000000 ) ) ;
#34040 = ORIENTED_EDGE ( 'NONE', *, *, #53901, .F. ) ;
#34041 = CARTESIAN_POINT ( 'NONE',  ( 80.48345259418954356, 57.73457509892514139, -16.59664598758602949 ) ) ;
#34042 = CARTESIAN_POINT ( 'NONE',  ( 158.1111710560796837, 275.7850098430334924, -12.43649661082534053 ) ) ;
#34044 = CARTESIAN_POINT ( 'NONE',  ( 182.0304806200197163, 260.4090999588434556, 10.44904933884112452 ) ) ;
#34043 = CARTESIAN_POINT ( 'NONE',  ( 147.7887599827787994, 276.1980330845831304, 2.700269039940759619 ) ) ;
#34045 = CARTESIAN_POINT ( 'NONE',  ( 156.1927096727130788, 279.9932537871562204, -6.834036338872565786 ) ) ;
#34046 = CARTESIAN_POINT ( 'NONE',  ( 136.3847812948166336, 258.7369531367911009, -4.594050593750048428 ) ) ;
#34047 = AXIS2_PLACEMENT_3D ( 'NONE', #78774, #17456, #3770 ) ;
#34048 = CARTESIAN_POINT ( 'NONE',  ( 19.14685258109593136, 191.8615022471903160, 5.000000000000046185 ) ) ;
#34049 = CARTESIAN_POINT ( 'NONE',  ( 66.46320885748656337, 68.94986384069261476, 0.01364106734875079018 ) ) ;
#34050 = CARTESIAN_POINT ( 'NONE',  ( 68.48323730116675279, 210.3458772461660544, 9.188101187500095079 ) ) ;
#34051 = CARTESIAN_POINT ( 'NONE',  ( 170.9866585576324383, 249.8975409664863037, 4.362717337680877883 ) ) ;
#34052 = CARTESIAN_POINT ( 'NONE',  ( 15.92326719930538204, 21.14441083166260071, 10.00000000000000533 ) ) ;
#34053 = CARTESIAN_POINT ( 'NONE',  ( 170.3178023250738420, 289.0326318653803241, -4.561300590322002080 ) ) ;
#34054 = CARTESIAN_POINT ( 'NONE',  ( 154.8605589353703351, 280.6980785630116770, -0.9605439388476536555 ) ) ;
#34055 = CARTESIAN_POINT ( 'NONE',  ( 172.4250300583619264, 287.9095745046552679, -8.433196622960897670 ) ) ;
#34056 = CARTESIAN_POINT ( 'NONE',  ( 202.8151641853381477, 279.3608264160075692, -16.28741359973609448 ) ) ;
#34057 = VECTOR ( 'NONE', #49353, 999.9999999999998863 ) ;
#34058 = CARTESIAN_POINT ( 'NONE',  ( 195.5324022567268685, 289.7225984500359459, 16.26972560970180481 ) ) ;
#34059 = CARTESIAN_POINT ( 'NONE',  ( 121.6084831627943998, 251.0177522451418781, 5.000000000000046185 ) ) ;
#34060 = CARTESIAN_POINT ( 'NONE',  ( 77.75060393840874440, 52.81207349147976515, -15.76950510618580203 ) ) ;
#34061 = ORIENTED_EDGE ( 'NONE', *, *, #99531, .F. ) ;
#34062 = B_SPLINE_CURVE_WITH_KNOTS ( 'NONE', 3,
 ( #55169, #61777, #8594, #32387 ),
 .UNSPECIFIED., .F., .F.,
 ( 4, 4 ),
 ( 0.008234140320758805837, 0.01447576861028371242 ),
 .UNSPECIFIED. ) ;
#34063 = CARTESIAN_POINT ( 'NONE',  ( 66.49206384107228018, 67.79058194764397172, -6.885858948892061626 ) ) ;
#34064 = CARTESIAN_POINT ( 'NONE',  ( 147.6618183892331331, 274.8892235422768522, 8.990680574201936892 ) ) ;
#34065 = CARTESIAN_POINT ( 'NONE',  ( -3.504777292649705167, 156.5327760586659451, 1.948934522072302763E-15 ) ) ;
#34066 = B_SPLINE_CURVE_WITH_KNOTS ( 'NONE', 3,
 ( #25167, #89882, #13356, #74670, #1886, #48482, #42721, #65542, #58431, #28036, #71294, #88924, #79424, #58912, #82790, #51849, #35137, #9990, #40851, #20456, #51330, #82297, #32768, #63673, #2394, #56050, #74167, #27565, #67029, #97956, #73659, #94612, #81292, #87043, #90392, #43727, #34643, #36127, #71796, #89406, #4759, #96489, #27059, #11865, #4237, #66048 ),
 .UNSPECIFIED., .F., .F.,
 ( 4, 2, 2, 2, 2, 2, 2, 2, 2, 2, 2, 2, 2, 2, 2, 2, 2, 2, 2, 2, 2, 2, 4 ),
 ( 0.0001777723017766823428, 0.0006668324149998756251, 0.001155892528223068962, 0.001400422584834609034, 0.001644952641446149541, 0.001767217669751986906, 0.001889482698057824706, 0.002011747726363662288, 0.002134012754669499870, 0.002623072867893023671, 0.003112132981116547473, 0.004090253207563457165, 0.005068373434010366857, 0.005557433547233746676, 0.005801963603845436586, 0.006046493660457125628, 0.006107626174610013628, 0.006168758688762901628, 0.006291023717068675893, 0.006535553773680317230, 0.007024613886903500158, 0.007513674000126683086, 0.008002734113349866882 ),
 .UNSPECIFIED. ) ;
#34067 = CARTESIAN_POINT ( 'NONE',  ( 175.7270353543445935, 256.4821516345319310, -11.00345789725119872 ) ) ;
#34068 = CARTESIAN_POINT ( 'NONE',  ( 15.24912932961584744, 31.73705186507753950, -3.090169943749475845 ) ) ;
#34069 = CARTESIAN_POINT ( 'NONE',  ( 33.27389197678166965, 200.0177522451419350, 5.000000000000046185 ) ) ;
#34070 = CARTESIAN_POINT ( 'NONE',  ( 47.92671612011951510, 80.40884667711614497, -10.00000000000000000 ) ) ;
#34071 = CARTESIAN_POINT ( 'NONE',  ( 72.30187851786844533, 71.99614501073629924, -3.638213215807910572 ) ) ;
#34072 = CARTESIAN_POINT ( 'NONE',  ( 147.5634954182374372, 275.0595239235922236, 4.682022975662822439 ) ) ;
#34073 = CARTESIAN_POINT ( 'NONE',  ( 73.74125571288574577, 55.30219098885146423, -16.59355670855032372 ) ) ;
#34075 = CARTESIAN_POINT ( 'NONE',  ( 61.92489908531693033, 199.8927522451418213, 10.00000000000009592 ) ) ;
#34074 = CARTESIAN_POINT ( 'NONE',  ( 167.5661991301409444, 256.5966495963957072, 13.73677599192672716 ) ) ;
#34076 = CARTESIAN_POINT ( 'NONE',  ( 163.0264227101321808, 256.4156498409448659, -15.66890022965337970 ) ) ;
#34077 = CARTESIAN_POINT ( 'NONE',  ( 157.8719920515997046, 257.2046840049564480, -17.69857783492101433 ) ) ;
#34078 = DIRECTION ( 'NONE',  ( 1.000000000000000000, 0.000000000000000000, 0.000000000000000000 ) ) ;
#34079 = EDGE_CURVE ( 'NONE', #34648, #29382, #7176, .T. ) ;
#34080 = EDGE_CURVE ( 'NONE', #21251, #23755, #66408, .T. ) ;
#34081 = CARTESIAN_POINT ( 'NONE',  ( 42.09652578138355494, 205.1115022471903160, -5.000000000000047962 ) ) ;
#34082 = CARTESIAN_POINT ( 'NONE',  ( 185.0916526433780689, 294.1912918594279063, 9.743016488043720003 ) ) ;
#34083 = CARTESIAN_POINT ( 'NONE',  ( 149.7444450951932993, 271.6994330048118513, -11.56253598978762831 ) ) ;
#34084 = CARTESIAN_POINT ( 'NONE',  ( 10.02652254571713719, 176.5958772461660544, -9.188101187500095079 ) ) ;
#34085 = CARTESIAN_POINT ( 'NONE',  ( 29.80674373534435162, 38.18502408145592852, 5.678558825948277544 ) ) ;
#34086 = CARTESIAN_POINT ( 'NONE',  ( 164.3127595687991231, 252.5384005146300694, 13.43484586212805354 ) ) ;
#34087 = ADVANCED_FACE ( 'NONE', ( #60369 ), #84727, .F. ) ;
#34088 = CARTESIAN_POINT ( 'NONE',  ( 22.88158713136840561, 194.0177522451419350, 5.000000000000046185 ) ) ;
#34089 = CARTESIAN_POINT ( 'NONE',  ( 38.14222467998226307, 24.94754757982092386, 5.678558825948272215 ) ) ;
#34090 = CARTESIAN_POINT ( 'NONE',  ( 165.0297293518065658, 244.8071193337670195, 2.517333243890161665 ) ) ;
#34091 = FACE_OUTER_BOUND ( 'NONE', #74172, .T. ) ;
#34092 = CARTESIAN_POINT ( 'NONE',  ( 65.91222438545561602, 218.8615022471903160, 5.000000000000046185 ) ) ;
#34093 = CARTESIAN_POINT ( 'NONE',  ( 178.9979651084586578, 262.3326641942140327, -12.86811127174943614 ) ) ;
#34094 = CARTESIAN_POINT ( 'NONE',  ( 4.137530017820134631, 25.49540643055185285, 3.479690158560446702E-15 ) ) ;
#34095 = CARTESIAN_POINT ( 'NONE',  ( 153.0281328741066886, 278.1111380155435882, -6.210770828869143223 ) ) ;
#34096 = CARTESIAN_POINT ( 'NONE',  ( 19.52749640002317122, 16.98920272979925628, 7.433330006724137462 ) ) ;
#34097 = CARTESIAN_POINT ( 'NONE',  ( 67.62392126478502519, 221.3967562850346837, -4.648177544792955347E-16 ) ) ;
#34098 = FACE_OUTER_BOUND ( 'NONE', #26029, .T. ) ;
#34099 = CARTESIAN_POINT ( 'NONE',  ( 156.8945693171665425, 276.4456326148838912, 10.43105563263390856 ) ) ;
#34100 = CARTESIAN_POINT ( 'NONE',  ( 206.3454060440500086, 273.2462681537123785, -9.268083217908118954 ) ) ;
#34101 = ORIENTED_EDGE ( 'NONE', *, *, #4156, .F. ) ;
#34102 = CARTESIAN_POINT ( 'NONE',  ( 153.3127735718713609, 265.1014820546527631, 17.57722645152040641 ) ) ;
#34103 = CARTESIAN_POINT ( 'NONE',  ( 164.3274319858398087, 246.0235340536434592, -1.770631424362269168 ) ) ;
#34104 = B_SPLINE_CURVE_WITH_KNOTS ( 'NONE', 3,
 ( #38169, #31079, #23474, #76695 ),
 .UNSPECIFIED., .F., .F.,
 ( 4, 4 ),
 ( 0.001830914869364597564, 0.009761397888737791476 ),
 .UNSPECIFIED. ) ;
#34105 = CARTESIAN_POINT ( 'NONE',  ( 66.31578965481824639, 68.16347547130251883, 4.387282884348506329 ) ) ;
#34106 = CARTESIAN_POINT ( 'NONE',  ( 87.60007719130888404, 45.49888764405456953, 6.854024160836727830 ) ) ;
#34107 = ORIENTED_EDGE ( 'NONE', *, *, #29040, .T. ) ;
#34108 = ORIENTED_EDGE ( 'NONE', *, *, #74921, .F. ) ;
#34109 = DIRECTION ( 'NONE',  ( 0.4999999999999995004, 0.8660254037844389297, 0.000000000000000000 ) ) ;
#34110 = CARTESIAN_POINT ( 'NONE',  ( 86.50957498950597824, 47.24826369376732771, 10.71680696257866394 ) ) ;
#34111 = ORIENTED_EDGE ( 'NONE', *, *, #86371, .T. ) ;
#34112 = CARTESIAN_POINT ( 'NONE',  ( 196.1749740761792111, 288.8619730569873809, -17.33086882175758703 ) ) ;
#34113 = CARTESIAN_POINT ( 'NONE',  ( 177.8721144827672731, 263.9665094508621905, 14.68891706277765330 ) ) ;
#34114 = ORIENTED_EDGE ( 'NONE', *, *, #66263, .T. ) ;
#34115 = CARTESIAN_POINT ( 'NONE',  ( 36.35590661721340666, 26.15404122711136026, 8.090169943749479842 ) ) ;
#34116 = CARTESIAN_POINT ( 'NONE',  ( 83.18584357961942999, 48.96896753446518602, -13.12400861552115572 ) ) ;
#34117 = CARTESIAN_POINT ( 'NONE',  ( 80.77639761371902694, 43.06272340307192792, 9.748640195465013036 ) ) ;
#34118 = ORIENTED_EDGE ( 'NONE', *, *, #36828, .F. ) ;
#34119 = CARTESIAN_POINT ( 'NONE',  ( 161.5504728662519369, 250.8333683393111926, 12.94300825113363373 ) ) ;
#34120 = CARTESIAN_POINT ( 'NONE',  ( 169.5095520540864982, 276.3819341640797802, -15.71460239395836744 ) ) ;
#34121 = FACE_OUTER_BOUND ( 'NONE', #31725, .T. ) ;
#34122 = EDGE_LOOP ( 'NONE', ( #58368, #89599 ) ) ;
#34123 = CARTESIAN_POINT ( 'NONE',  ( 148.3010860587701814, 276.5068540982774721, -3.904121881399305050 ) ) ;
#34124 = ORIENTED_EDGE ( 'NONE', *, *, #16678, .T. ) ;
#34125 = CARTESIAN_POINT ( 'NONE',  ( 160.3638665304753488, 268.9007647980437241, -16.83629063676312398 ) ) ;
#34126 = EDGE_LOOP ( 'NONE', ( #9402, #93672, #14842, #26288, #60744 ) ) ;
#34127 = CARTESIAN_POINT ( 'NONE',  ( 177.9669066697758524, 253.3125553430435275, -3.218270011446984213 ) ) ;
#34128 = VECTOR ( 'NONE', #59867, 1000.000000000000227 ) ;
#34129 = ORIENTED_EDGE ( 'NONE', *, *, #55204, .T. ) ;
#34130 = CARTESIAN_POINT ( 'NONE',  ( 147.7331950265948137, 274.7655955798928744, 7.332100195727512038 ) ) ;
#34131 = CARTESIAN_POINT ( 'NONE',  ( 178.3794556815479098, 289.5192613054423987, -9.351548050966405512 ) ) ;
#34132 = CARTESIAN_POINT ( 'NONE',  ( 71.04820796358482937, 68.65144407467539622, 8.809617914912280412 ) ) ;
#34133 = CARTESIAN_POINT ( 'NONE',  ( 193.7596376655525887, 294.6616349329243576, 13.47874803057572279 ) ) ;
#34134 = CARTESIAN_POINT ( 'NONE',  ( 86.35121876318000034, 43.08468197994678661, 0.3078304325362931637 ) ) ;
#34135 = CARTESIAN_POINT ( 'NONE',  ( 158.6468336853046139, 255.8626189275596801, -16.06042259295567476 ) ) ;
#34136 = ORIENTED_EDGE ( 'NONE', *, *, #8315, .F. ) ;
#34137 = DIRECTION ( 'NONE',  ( -0.6855440362341480576, 0.7280311630581436377, 0.000000000000000000 ) ) ;
#34138 = CARTESIAN_POINT ( 'NONE',  ( 20.27385872851041526, 33.74646525600390135, 2.839279412974139660 ) ) ;
#34139 = EDGE_CURVE ( 'NONE', #31364, #15864, #8689, .T. ) ;
#34140 = CARTESIAN_POINT ( 'NONE',  ( 190.8261335000477743, 298.8222043136631783, -8.159106789104095370 ) ) ;
#34142 = ORIENTED_EDGE ( 'NONE', *, *, #30157, .T. ) ;
#34141 = CARTESIAN_POINT ( 'NONE',  ( -8.669243101527598583, 25.19333184544593252, -10.00000000000000000 ) ) ;
#34143 = EDGE_LOOP ( 'NONE', ( #98910, #30220 ) ) ;
#34144 = CARTESIAN_POINT ( 'NONE',  ( 187.1933455069532215, 276.8274618490077046, 17.59017769528927744 ) ) ;
#34145 = CARTESIAN_POINT ( 'NONE',  ( 69.86972952878745957, 62.75331692225537239, 13.91736506036380661 ) ) ;
#34146 = DIRECTION ( 'NONE',  ( 0.4999999999999973910, -0.8660254037844401509, -1.249000902703321145E-14 ) ) ;
#34147 = CARTESIAN_POINT ( 'NONE',  ( 19.07322413485131563, 11.41603393254324139, -1.583844403245362020 ) ) ;
#34148 = ADVANCED_FACE ( 'NONE', ( #22880 ), #23875, .F. ) ;
#34149 = CARTESIAN_POINT ( 'NONE',  ( 47.29267820409027934, 188.1115022471902023, -5.000000000000041744 ) ) ;
#34150 = CARTESIAN_POINT ( 'NONE',  ( 190.5793395442805149, 300.5538963668226415, -0.3437584566168827571 ) ) ;
#34151 = ORIENTED_EDGE ( 'NONE', *, *, #6573, .F. ) ;
#34152 = CARTESIAN_POINT ( 'NONE',  ( 70.02414138031360835, 62.78214778883172187, 13.38063900663788885 ) ) ;
#34153 = PLANE ( 'NONE',  #59244 ) ;
#34155 = EDGE_CURVE ( 'NONE', #59347, #30332, #92819, .T. ) ;
#34154 = CARTESIAN_POINT ( 'NONE',  ( -19.67426652243475615, 92.92480266137719980, 59.99999999999999289 ) ) ;
#34156 = CARTESIAN_POINT ( 'NONE',  ( 21.22170510744821570, 196.3927522451419634, 2.944929066748280225E-16 ) ) ;
#34157 = CARTESIAN_POINT ( 'NONE',  ( 108.5912123618160905, 227.3768266524159856, -9.188101187500093303 ) ) ;
#34158 = CARTESIAN_POINT ( 'NONE',  ( 184.0238465689049292, 296.8912303140136828, -2.771834375495716873 ) ) ;
#34159 = DIRECTION ( 'NONE',  ( -1.000000000000000000, 0.000000000000000000, 0.000000000000000000 ) ) ;
#34160 = CARTESIAN_POINT ( 'NONE',  ( 163.0311878320900121, 248.2686947869521532, 10.33250033289960435 ) ) ;
#34161 = CARTESIAN_POINT ( 'NONE',  ( 29.16053163240333745, 178.4548013555409796, -4.594050593750042211 ) ) ;
#34162 = CARTESIAN_POINT ( 'NONE',  ( 180.3268137483904354, 258.1330830615356149, 10.30874540274224849 ) ) ;
#34163 = ORIENTED_EDGE ( 'NONE', *, *, #65299, .T. ) ;
#34164 = VERTEX_POINT ( 'NONE', #14787 ) ;
#34165 = CARTESIAN_POINT ( 'NONE',  ( 185.2070000183807394, 260.0088792301957028, -5.784610090025596563 ) ) ;
#34166 = CARTESIAN_POINT ( 'NONE',  ( 88.07432094012324342, 44.02706539047903789, 0.5635391379978663684 ) ) ;
#34167 = CARTESIAN_POINT ( 'NONE',  ( 84.35036076898174429, 44.10653668295481822, 7.536754518051668406 ) ) ;
#34168 = CARTESIAN_POINT ( 'NONE',  ( 192.9721262430356887, 263.8139873464725724, -4.229629090758195709 ) ) ;
#34169 = CARTESIAN_POINT ( 'NONE',  ( 14.42807667092211865, 8.734156793818204534, -7.779800476318352071E-15 ) ) ;
#34170 = CARTESIAN_POINT ( 'NONE',  ( 182.3765091510860827, 284.2746805155291554, 14.91661155942450634 ) ) ;
#34171 = CARTESIAN_POINT ( 'NONE',  ( 168.0994545464640737, 251.8035359048624855, 10.51302091382670056 ) ) ;
#34172 = CARTESIAN_POINT ( 'NONE',  ( 44.28847903505648986, 202.5024278399160949, -9.188101187500093303 ) ) ;
#34173 = CARTESIAN_POINT ( 'NONE',  ( 89.56554322277027325, 212.5177522451417929, 5.000000000000051514 ) ) ;
#34174 = EDGE_LOOP ( 'NONE', ( #64734, #71750, #11945, #21446 ) ) ;
#34175 = CARTESIAN_POINT ( 'NONE',  ( 84.34447119165866980, 48.35867903125333100, 12.23554050903201151 ) ) ;
#34176 = CARTESIAN_POINT ( 'NONE',  ( -42.23460334637722013, 26.80738527414552053, 177.5919119679930134 ) ) ;
#34177 = CARTESIAN_POINT ( 'NONE',  ( 7.590999645455913658, 169.0643266524160140, -9.188101187500093303 ) ) ;
#34178 = CARTESIAN_POINT ( 'NONE',  ( 69.00853799725599913, 64.33131446021079114, -11.92797522396560872 ) ) ;
#34179 = CARTESIAN_POINT ( 'NONE',  ( 199.2299651681423143, 285.5705732690366858, -17.65328173313980642 ) ) ;
#34180 = CARTESIAN_POINT ( 'NONE',  ( 79.96162642484517846, 48.81434648651384833, 14.52309195649116269 ) ) ;
#34181 = CARTESIAN_POINT ( 'NONE',  ( 193.1977289678065404, 296.0187128512746995, -12.37159405312863925 ) ) ;
#34182 = EDGE_CURVE ( 'NONE', #57311, #57629, #28823, .T. ) ;
#34183 = DIRECTION ( 'NONE',  ( -0.000000000000000000, -0.000000000000000000, 1.000000000000000000 ) ) ;
#34184 = CARTESIAN_POINT ( 'NONE',  ( 164.2851776226980860, 246.0967207574460929, 5.847738044744511754 ) ) ;
#34185 = DIRECTION ( 'NONE',  ( -0.4999999999999987788, 0.8660254037844392627, 0.000000000000000000 ) ) ;
#34186 = CARTESIAN_POINT ( 'NONE',  ( 164.3274319858398087, 246.0235340536434592, -1.770631424362269168 ) ) ;
#34187 = ORIENTED_EDGE ( 'NONE', *, *, #90035, .T. ) ;
#34188 = VECTOR ( 'NONE', #9175, 999.9999999999998863 ) ;
#34189 = CARTESIAN_POINT ( 'NONE',  ( 6.950328144465177438, 161.4865022471901455, 1.119607411625061291E-15 ) ) ;
#34190 = CARTESIAN_POINT ( 'NONE',  ( 38.21438390411638153, 96.04939573986766277, 59.99999999999999289 ) ) ;
#34191 = CARTESIAN_POINT ( 'NONE',  ( 128.2121871902485566, 235.6423013555409796, -4.594050593750043987 ) ) ;
#34192 = EDGE_CURVE ( 'NONE', #23972, #45307, #23373, .T. ) ;
#34193 = CARTESIAN_POINT ( 'NONE',  ( 19.25205234332785764, 23.06628583063841020, -9.188101187500006262 ) ) ;
#34194 = CARTESIAN_POINT ( 'NONE',  ( 74.92662977279880465, 67.20364597524810790, 12.51845076170456572 ) ) ;
#34195 = EDGE_CURVE ( 'NONE', #12322, #61284, #15776, .T. ) ;
#34196 = CARTESIAN_POINT ( 'NONE',  ( 151.0217401543597475, 269.4701321406242869, 13.82207127286603843 ) ) ;
#34198 = CARTESIAN_POINT ( 'NONE',  ( 25.95381284194209215, 117.4816347750370369, 59.99999999999999289 ) ) ;
#34197 = CARTESIAN_POINT ( 'NONE',  ( 196.3341081413628899, 290.5863447708742342, 16.12390540996472410 ) ) ;
#34199 = CARTESIAN_POINT ( 'NONE',  ( 150.4061938829137830, 270.1358257521749238, -15.15106128367595062 ) ) ;
#34200 = VERTEX_POINT ( 'NONE', #39062 ) ;
#34201 = CARTESIAN_POINT ( 'NONE',  ( 191.0170959869219303, 299.7956799668270946, 7.353346939903929069 ) ) ;
#34202 = CARTESIAN_POINT ( 'NONE',  ( 148.9831146496684084, 272.6006712873522133, -12.63706091291043343 ) ) ;
#34203 = DIRECTION ( 'NONE',  ( 0.000000000000000000, 1.000000000000000000, 0.000000000000000000 ) ) ;
#34204 = CARTESIAN_POINT ( 'NONE',  ( -75.14068524134968641, 52.46521621197197760, -10.00000000000000000 ) ) ;
#34205 = CARTESIAN_POINT ( 'NONE',  ( 81.62646408706272894, 55.64454924624774890, -16.33875670839028871 ) ) ;
#34206 = ORIENTED_EDGE ( 'NONE', *, *, #16957, .F. ) ;
#34207 = CARTESIAN_POINT ( 'NONE',  ( 189.0039683861011497, 265.7567017869877759, 11.47791173151251165 ) ) ;
#34208 = CARTESIAN_POINT ( 'NONE',  ( 175.3277058627924987, 278.9854953265928543, 15.46303258205545461 ) ) ;
#34209 = CARTESIAN_POINT ( 'NONE',  ( 168.8411136774919044, 271.8979524934410961, -17.10145977970367426 ) ) ;
#34210 = CARTESIAN_POINT ( 'NONE',  ( 196.3306825188763014, 270.8885471599495531, 12.02977562913896037 ) ) ;
#34211 = CARTESIAN_POINT ( 'NONE',  ( 83.91531380489591641, 51.74629119495582330, -14.43556620278794611 ) ) ;
#34212 = CARTESIAN_POINT ( 'NONE',  ( 21.15788363470973366, 37.74176219324819215, -10.00000000000000000 ) ) ;
#34213 = CARTESIAN_POINT ( 'NONE',  ( 192.3401793061076717, 297.5040324353506094, 12.56432540404525611 ) ) ;
#34214 =( BOUNDED_SURFACE ( )  B_SPLINE_SURFACE ( 1, 2, ( 
 ( #29560, #36151, #90913, #52848, #74693, #14847, #21462, #38126, #82810, #68053, #7244, #59436, #84299, #5757, #43749, #97978, #6759, #61442, #22941, #28554, #83295, #12893, #90418, #13859, #13378, #75672, #44247, #6257, #67553, #37637, #98486, #29077, #37154, #60434, #91390, #83798, #14362, #45248, #45733, #53349, #76656, #68548, #99473, #60939, #91899, #69043, #99973, #30558, #61930, #8751, #23940, #93896, #8259, #9258, #24450, #86308, #62427, #23436, #54840, #46749, #55331, #85821, #16350, #15331, #32034, #39124, #32554, #24941, #40130, #84790, #46226, #31538, #92882, #47244, #77148, #93388, #31043, #71070, #155, #54325, #53830, #78164, #85296, #7752, #651, #15840, #55819, #86812, #17344, #39622, #38645, #62946, #69550, #78667, #1671, #77675, #70038, #70544, #1160, #16843, #47733, #63452, #94388, #48252, #79199, #9772, #40634, #71569, #2165, #33046, #63945, #94884, #3667, #80193, #4140, #96893, #81195, #34545, #50730, #81685, #33557, #2666, #48764, #11764, #64959, #73556, #73069, #64452, #65443, #35542, #96388, #26952, #35035, #95412, #57338, #12258, #65939, #87823, #27463, #11277, #56838, #10761, #42627, #79697, #34068, #26462, #25968, #25446, #43116, #58333, #56336, #95904, #87335, #88312, #57835, #18362, #41128, #19382, #88816, #18866, #50241, #49748, #41635, #89309, #19863, #17867, #74060, #49257, #4649, #72579, #10259, #72066, #80701, #3185, #82195, #37031, #13734, #20357, #75057, #67939, #89781, #29930, #5634, #53231, #97859, #83172, #22332, #74570, #99352, #20861, #58819, #51227, #21834, #76544, #38007, #12766, #67428, #28430, #43631, #91269, #75549, #28948, #98860, #21343, #51752, #29437, #60807, #7123, #52719, #90291, #45126, #36029, #97371, #37519, #59826, #98359, #5148, #60311, #44614, #66929, #36527, #83679, #59312, #91767, #90791, #84183, #82694, #6134, #14732, #13260, #45615, #44120, #52227, #14240, #76064, #27937, #6644, #68424, #39013, #99846, #30429, #46619, #77022, #69919, #92281, #8138, #46108, #24334, #15213, #38519, #68920, #533, #69429, #61320, #15718, #7628, #70946, #40007, #1550, #31419, #22828, #47122, #53713, #93776, #16729, #45, #30929, #23819, #62308, #8634, #23318, #55211, #39501, #1037, #77549, #61813, #93264, #92763, #70428, #54711, #85693, #84671, #78045, #54206, #47620, #32433, #86193, #31916, #94269, #24824, #85174, #16232, #62820, #78547, #9135, #63328, #55699, #86687, #17219, #79070, #48126, #9655, #19262, #10140, #72461, #96772, #50129, #2549, #11647, #26340, #71947, #25850, #26834, #94763, #49138, #41517, #41005, #81565, #27338, #42507, #71448, #80072, #50611, #3066, #11158, #10643, #40513, #79579, #64839, #33434, #87209, #2037, #32923, #58219, #42025, #18245, #89198, #33952, #88692, #73443, #81081, #18740, #95786, #57216, #19746, #88191, #72959, #64331, #63827, #48644, #49624, #56212, #25326, #17744, #80578, #95290, #56726, #87709, #3551, #34429, #4027, #65329, #34913, #96268, #57712, #65811, #44505, #13631, #75434, #66328, #36409, #74454, #66817, #60193, #91650, #14124, #6527, #97745, #52603, #4522, #98241, #13142, #67313, #43999, #83560, #60692, #29818, #59191, #27827, #97260, #59710, #42998, #98747, #53114, #28827, #83058, #36912, #45005, #5034, #67825, #51110 ),
 ( #58703, #75951, #37403, #68309, #74941, #35423, #90676, #12136, #29327, #91153, #12645, #20238, #21232, #82579, #52111, #28313, #21719, #6018, #99232, #20740, #82075, #5525, #35916, #22217, #73936, #89677, #43515, #90167, #51627, #62699, #55101, #39391, #93146, #9016, #39888, #92173, #61206, #7011, #70308, #23203, #54094, #84071, #22723, #8031, #53602, #30319, #94156, #24709, #1432, #85574, #61701, #70823, #77433, #31797, #86088, #93656, #62195, #38904, #92653, #63214, #85050, #54592, #7505, #37896, #84560, #69808, #99732, #32313, #14624, #418, #15099, #45990, #76436, #68804, #76907, #24221, #38402, #16612, #15597, #69315, #100237, #16118, #47016, #77931, #30821, #31307, #46497, #23697, #47508, #45503, #78435, #8522, #921, #96157, #48005, #41402, #56614, #79959, #87598, #26720, #3918, #73331, #2438, #71335, #9537, #2951, #86575, #41913, #96657, #72346, #26224, #80465, #57602, #48528, #11036, #94656, #34317, #25211, #34801, #57100, #50018, #65703, #88582, #79465, #10527, #78949, #56095, #40891, #63718, #17108, #33840, #64215, #10029, #88082, #87088, #40398, #72848, #3440, #17624, #19144, #33316, #64728, #95677, #95166, #55592, #25734, #49511, #65215, #80972, #11537, #42397, #18124, #71840, #1927, #32813, #35810, #35307, #28204, #60086, #4931, #50501, #98637, #59080, #13036, #66219, #67204, #67710, #81950, #28710, #5908, #97158, #90051, #83444, #36798, #89565, #29219, #43898, #58592, #12527, #13526, #81455, #66704, #20623, #27724, #68194, #14011, #91049, #58110, #97639, #37297, #51507, #98126, #20127, #42883, #21133, #5418, #82474, #59588, #74838, #43399, #90564, #21616, #27227, #52010, #50999, #75329, #74342, #89092, #52496, #36300, #82953, #12027, #44394, #44889, #73819, #75830, #6416, #19641, #4411, #7392, #56359, #99622, #84935, #25469, #76324, #2187, #22603, #60582, #91538, #24961, #79717, #41150, #83949, #69193, #29705, #22102, #76799, #6899, #100122, #52998, #38282, #37788, #55839, #45394, #68689, #99123, #30707, #30200, #14511, #45875, #61086, #33070, #71592, #63964, #61587, #92057, #77306, #53491, #86834, #48274, #84443, #14988, #53977, #92538, #38788, #23085, #17367, #69694, #31186, #15481, #46376, #7913, #299, #62077, #94408, #79220, #9794, #40654, #94907, #87358, #17887, #48786, #10280, #97385, #27953, #80214, #49277, #95436, #27482, #11298, #19881, #19401, #10782, #88837, #82213, #50260, #41657, #89800, #73575, #66460, #20374, #74078, #64978, #65465, #25988, #72600, #57357, #3204, #2689, #81213, #80724, #26482, #4158, #34089, #56857, #89328, #58350, #95921, #4668, #18888, #11787, #57857, #49768, #51245, #42157, #42644, #35053, #65961, #96911, #50751, #73092, #88333, #81703, #58834, #3685, #34564, #96406, #35559, #26975, #87843, #43137, #12276, #12783, #72088, #33581, #64475, #18382, #13750, #43648, #82710, #67954, #13277, #90308, #53727, #84686, #61334, #45143, #21361, #30444, #37046, #91783, #45628, #53245, #21850, #98874, #52246, #22844, #44631, #14255, #67449, #66946, #51768, #29452, #59328, #92293, #74587, #60328, #44139, #20879, #36044, #97875, #75073, #84201, #98377, #14747, #83190, #5653, #36542, #76082, #6657, #37534, #28449, #91284, #28965, #59844, #22349, #5165, #76557, #38023, #90806, #7136 ) ),
 .UNSPECIFIED., .F., .F., .T. ) 
 B_SPLINE_SURFACE_WITH_KNOTS ( ( 2, 2 ),
 ( 3, 2, 2, 2, 2, 2, 2, 2, 2, 2, 2, 2, 2, 2, 2, 2, 2, 2, 2, 2, 2, 2, 2, 2, 2, 2, 2, 2, 2, 2, 2, 2, 2, 2, 2, 2, 2, 2, 2, 2, 2, 2, 2, 2, 2, 2, 2, 2, 2, 2, 2, 2, 2, 2, 2, 2, 2, 2, 2, 2, 2, 2, 2, 2, 2, 2, 2, 2, 2, 2, 2, 2, 2, 2, 2, 2, 2, 2, 2, 2, 2, 2, 2, 2, 2, 2, 2, 2, 2, 2, 2, 2, 2, 2, 2, 2, 2, 2, 2, 2, 2, 2, 2, 2, 2, 2, 2, 2, 2, 2, 2, 2, 2, 2, 2, 2, 2, 2, 2, 2, 2, 2, 2, 2, 2, 2, 2, 2, 2, 2, 2, 2, 2, 2, 2, 2, 2, 2, 2, 2, 2, 2, 2, 2, 2, 2, 2, 2, 2, 2, 2, 2, 2, 2, 2, 2, 2, 2, 2, 2, 2, 2, 2, 2, 2, 2, 2, 2, 2, 2, 2, 2, 2, 2, 2, 2, 2, 2, 2, 2, 2, 2, 2, 2, 2, 2, 2, 2, 2, 2, 2, 2, 2, 2, 2, 2, 2, 2, 2, 2, 3 ),
 ( 0.000000000000000000, 1.000000000000000000 ),
 ( 0.000000000000000000, 0.005000000000000000104, 0.01000000000000000021, 0.01499999999999999944, 0.02000000000000000042, 0.02500000000000000139, 0.02999999999999999889, 0.03500000000000000333, 0.04000000000000000083, 0.04499999999999999833, 0.05000000000000000278, 0.05500000000000000028, 0.05999999999999999778, 0.06500000000000000222, 0.07000000000000000666, 0.07499999999999999722, 0.08000000000000000167, 0.08500000000000000611, 0.08999999999999999667, 0.09500000000000000111, 0.1000000000000000056, 0.1049999999999999961, 0.1100000000000000006, 0.1150000000000000050, 0.1199999999999999956, 0.1250000000000000000, 0.1300000000000000044, 0.1350000000000000089, 0.1400000000000000133, 0.1449999999999999900, 0.1499999999999999944, 0.1549999999999999989, 0.1600000000000000033, 0.1650000000000000078, 0.1700000000000000122, 0.1749999999999999889, 0.1799999999999999933, 0.1849999999999999978, 0.1900000000000000022, 0.1950000000000000067, 0.2000000000000000111, 0.2049999999999999878, 0.2099999999999999922, 0.2149999999999999967, 0.2200000000000000011, 0.2250000000000000056, 0.2300000000000000100, 0.2349999999999999867, 0.2399999999999999911, 0.2449999999999999956, 0.2500000000000000000, 0.2550000000000000044, 0.2600000000000000089, 0.2650000000000000133, 0.2700000000000000178, 0.2750000000000000222, 0.2800000000000000266, 0.2849999999999999756, 0.2899999999999999800, 0.2949999999999999845, 0.2999999999999999889, 0.3049999999999999933, 0.3099999999999999978, 0.3150000000000000022, 0.3200000000000000067, 0.3250000000000000111, 0.3300000000000000155, 0.3350000000000000200, 0.3400000000000000244, 0.3449999999999999734, 0.3499999999999999778, 0.3549999999999999822, 0.3599999999999999867, 0.3649999999999999911, 0.3699999999999999956, 0.3750000000000000000, 0.3800000000000000044, 0.3850000000000000089, 0.3900000000000000133, 0.3950000000000000178, 0.4000000000000000222, 0.4050000000000000266, 0.4099999999999999756, 0.4149999999999999800, 0.4199999999999999845, 0.4249999999999999889, 0.4299999999999999933, 0.4349999999999999978, 0.4400000000000000022, 0.4450000000000000067, 0.4500000000000000111, 0.4550000000000000155, 0.4600000000000000200, 0.4650000000000000244, 0.4699999999999999734, 0.4749999999999999778, 0.4799999999999999822, 0.4849999999999999867, 0.4899999999999999911, 0.4949999999999999956, 0.5000000000000000000, 0.5050000000000000044, 0.5100000000000000089, 0.5150000000000000133, 0.5200000000000000178, 0.5250000000000000222, 0.5300000000000000266, 0.5350000000000000311, 0.5400000000000000355, 0.5450000000000000400, 0.5500000000000000444, 0.5550000000000000488, 0.5600000000000000533, 0.5649999999999999467, 0.5699999999999999512, 0.5749999999999999556, 0.5799999999999999600, 0.5849999999999999645, 0.5899999999999999689, 0.5949999999999999734, 0.5999999999999999778, 0.6049999999999999822, 0.6099999999999999867, 0.6149999999999999911, 0.6199999999999999956, 0.6250000000000000000, 0.6300000000000000044, 0.6350000000000000089, 0.6400000000000000133, 0.6450000000000000178, 0.6500000000000000222, 0.6550000000000000266, 0.6600000000000000311, 0.6650000000000000355, 0.6700000000000000400, 0.6750000000000000444, 0.6800000000000000488, 0.6850000000000000533, 0.6899999999999999467, 0.6949999999999999512, 0.6999999999999999556, 0.7049999999999999600, 0.7099999999999999645, 0.7149999999999999689, 0.7199999999999999734, 0.7249999999999999778, 0.7299999999999999822, 0.7349999999999999867, 0.7399999999999999911, 0.7449999999999999956, 0.7500000000000000000, 0.7550000000000000044, 0.7600000000000000089, 0.7650000000000000133, 0.7700000000000000178, 0.7750000000000000222, 0.7800000000000000266, 0.7850000000000000311, 0.7900000000000000355, 0.7950000000000000400, 0.8000000000000000444, 0.8050000000000000488, 0.8100000000000000533, 0.8149999999999999467, 0.8199999999999999512, 0.8249999999999999556, 0.8299999999999999600, 0.8349999999999999645, 0.8399999999999999689, 0.8449999999999999734, 0.8499999999999999778, 0.8549999999999999822, 0.8599999999999999867, 0.8649999999999999911, 0.8699999999999999956, 0.8750000000000000000, 0.8800000000000000044, 0.8850000000000000089, 0.8900000000000000133, 0.8950000000000000178, 0.9000000000000000222, 0.9050000000000000266, 0.9100000000000000311, 0.9150000000000000355, 0.9200000000000000400, 0.9250000000000000444, 0.9300000000000000488, 0.9350000000000000533, 0.9399999999999999467, 0.9449999999999999512, 0.9499999999999999556, 0.9549999999999999600, 0.9599999999999999645, 0.9649999999999999689, 0.9699999999999999734, 0.9749999999999999778, 0.9799999999999999822, 0.9849999999999999867, 0.9899999999999999911, 0.9949999999999999956, 1.000000000000000000 ),
 .UNSPECIFIED. ) 
 GEOMETRIC_REPRESENTATION_ITEM ( )  RATIONAL_B_SPLINE_SURFACE ( (
 ( 1.000000000000000000, 0.9510565162951535312, 1.000000000000000000, 0.9510565162951535312, 1.000000000000000000, 0.9510565162951535312, 1.000000000000000000, 0.9510565162951535312, 1.000000000000000000, 0.9510565162951535312, 1.000000000000000000, 0.9510565162951535312, 1.000000000000000000, 0.9510565162951535312, 1.000000000000000000, 0.9510565162951535312, 1.000000000000000000, 0.9510565162951535312, 1.000000000000000000, 0.9510565162951535312, 1.000000000000000000, 0.9510565162951535312, 1.000000000000000000, 0.9510565162951535312, 1.000000000000000000, 0.9510565162951535312, 1.000000000000000000, 0.9510565162951535312, 1.000000000000000000, 0.9510565162951535312, 1.000000000000000000, 0.9510565162951535312, 1.000000000000000000, 0.9510565162951535312, 1.000000000000000000, 0.9510565162951535312, 1.000000000000000000, 0.9510565162951535312, 1.000000000000000000, 0.9510565162951535312, 1.000000000000000000, 0.9510565162951535312, 1.000000000000000000, 0.9510565162951535312, 1.000000000000000000, 0.9510565162951535312, 1.000000000000000000, 0.9510565162951535312, 1.000000000000000000, 0.9510565162951535312, 1.000000000000000000, 0.9510565162951535312, 1.000000000000000000, 0.9510565162951535312, 1.000000000000000000, 0.9510565162951535312, 1.000000000000000000, 0.9510565162951535312, 1.000000000000000000, 0.9510565162951535312, 1.000000000000000000, 0.9510565162951535312, 1.000000000000000000, 0.9510565162951535312, 1.000000000000000000, 0.9510565162951535312, 1.000000000000000000, 0.9510565162951535312, 1.000000000000000000, 0.9510565162951535312, 1.000000000000000000, 0.9510565162951535312, 1.000000000000000000, 0.9510565162951535312, 1.000000000000000000, 0.9510565162951535312, 1.000000000000000000, 0.9510565162951535312, 1.000000000000000000, 0.9510565162951535312, 1.000000000000000000, 0.9510565162951535312, 1.000000000000000000, 0.9510565162951535312, 1.000000000000000000, 0.9510565162951535312, 1.000000000000000000, 0.9510565162951535312, 1.000000000000000000, 0.9510565162951535312, 1.000000000000000000, 0.9510565162951535312, 1.000000000000000000, 0.9510565162951535312, 1.000000000000000000, 0.9510565162951535312, 1.000000000000000000, 0.9510565162951535312, 1.000000000000000000, 0.9510565162951535312, 1.000000000000000000, 0.9510565162951535312, 1.000000000000000000, 0.9510565162951535312, 1.000000000000000000, 0.9510565162951535312, 1.000000000000000000, 0.9510565162951535312, 1.000000000000000000, 0.9510565162951535312, 1.000000000000000000, 0.9510565162951535312, 1.000000000000000000, 0.9510565162951535312, 1.000000000000000000, 0.9510565162951535312, 1.000000000000000000, 0.9510565162951535312, 1.000000000000000000, 0.9510565162951535312, 1.000000000000000000, 0.9510565162951535312, 1.000000000000000000, 0.9510565162951535312, 1.000000000000000000, 0.9510565162951535312, 1.000000000000000000, 0.9510565162951535312, 1.000000000000000000, 0.9510565162951535312, 1.000000000000000000, 0.9510565162951535312, 1.000000000000000000, 0.9510565162951535312, 1.000000000000000000, 0.9510565162951535312, 1.000000000000000000, 0.9510565162951535312, 1.000000000000000000, 0.9510565162951535312, 1.000000000000000000, 0.9510565162951535312, 1.000000000000000000, 0.9510565162951535312, 1.000000000000000000, 0.9510565162951535312, 1.000000000000000000, 0.9510565162951535312, 1.000000000000000000, 0.9510565162951535312, 1.000000000000000000, 0.9510565162951535312, 1.000000000000000000, 0.9510565162951535312, 1.000000000000000000, 0.9510565162951535312, 1.000000000000000000, 0.9510565162951535312, 1.000000000000000000, 0.9510565162951535312, 1.000000000000000000, 0.9510565162951535312, 1.000000000000000000, 0.9510565162951535312, 1.000000000000000000, 0.9510565162951535312, 1.000000000000000000, 0.9510565162951535312, 1.000000000000000000, 0.9510565162951535312, 1.000000000000000000, 0.9510565162951535312, 1.000000000000000000, 0.9510565162951535312, 1.000000000000000000, 0.9510565162951535312, 1.000000000000000000, 0.9510565162951535312, 1.000000000000000000, 0.9510565162951535312, 1.000000000000000000, 0.9510565162951535312, 1.000000000000000000, 0.9510565162951535312, 1.000000000000000000, 0.9510565162951535312, 1.000000000000000000, 0.9510565162951535312, 1.000000000000000000, 0.9510565162951535312, 1.000000000000000000, 0.9510565162951535312, 1.000000000000000000, 0.9510565162951535312, 1.000000000000000000, 0.9510565162951535312, 1.000000000000000000, 0.9510565162951535312, 1.000000000000000000, 0.9510565162951535312, 1.000000000000000000, 0.9510565162951535312, 1.000000000000000000, 0.9510565162951535312, 1.000000000000000000, 0.9510565162951535312, 1.000000000000000000, 0.9510565162951535312, 1.000000000000000000, 0.9510565162951535312, 1.000000000000000000, 0.9510565162951535312, 1.000000000000000000, 0.9510565162951535312, 1.000000000000000000, 0.9510565162951535312, 1.000000000000000000, 0.9510565162951535312, 1.000000000000000000, 0.9510565162951535312, 1.000000000000000000, 0.9510565162951535312, 1.000000000000000000, 0.9510565162951535312, 1.000000000000000000, 0.9510565162951535312, 1.000000000000000000, 0.9510565162951535312, 1.000000000000000000, 0.9510565162951535312, 1.000000000000000000, 0.9510565162951535312, 1.000000000000000000, 0.9510565162951535312, 1.000000000000000000, 0.9510565162951535312, 1.000000000000000000, 0.9510565162951535312, 1.000000000000000000, 0.9510565162951535312, 1.000000000000000000, 0.9510565162951535312, 1.000000000000000000, 0.9510565162951535312, 1.000000000000000000, 0.9510565162951535312, 1.000000000000000000, 0.9510565162951535312, 1.000000000000000000, 0.9510565162951535312, 1.000000000000000000, 0.9510565162951535312, 1.000000000000000000, 0.9510565162951535312, 1.000000000000000000, 0.9510565162951535312, 1.000000000000000000, 0.9510565162951535312, 1.000000000000000000, 0.9510565162951535312, 1.000000000000000000, 0.9510565162951535312, 1.000000000000000000, 0.9510565162951535312, 1.000000000000000000, 0.9510565162951535312, 1.000000000000000000, 0.9510565162951535312, 1.000000000000000000, 0.9510565162951535312, 1.000000000000000000, 0.9510565162951535312, 1.000000000000000000, 0.9510565162951535312, 1.000000000000000000, 0.9510565162951535312, 1.000000000000000000, 0.9510565162951535312, 1.000000000000000000, 0.9510565162951535312, 1.000000000000000000, 0.9510565162951535312, 1.000000000000000000, 0.9510565162951535312, 1.000000000000000000, 0.9510565162951535312, 1.000000000000000000, 0.9510565162951535312, 1.000000000000000000, 0.9510565162951535312, 1.000000000000000000, 0.9510565162951535312, 1.000000000000000000, 0.9510565162951535312, 1.000000000000000000, 0.9510565162951535312, 1.000000000000000000, 0.9510565162951535312, 1.000000000000000000, 0.9510565162951535312, 1.000000000000000000, 0.9510565162951535312, 1.000000000000000000, 0.9510565162951535312, 1.000000000000000000, 0.9510565162951535312, 1.000000000000000000, 0.9510565162951535312, 1.000000000000000000, 0.9510565162951535312, 1.000000000000000000, 0.9510565162951535312, 1.000000000000000000, 0.9510565162951535312, 1.000000000000000000, 0.9510565162951535312, 1.000000000000000000, 0.9510565162951535312, 1.000000000000000000, 0.9510565162951535312, 1.000000000000000000, 0.9510565162951535312, 1.000000000000000000, 0.9510565162951535312, 1.000000000000000000, 0.9510565162951535312, 1.000000000000000000, 0.9510565162951535312, 1.000000000000000000, 0.9510565162951535312, 1.000000000000000000, 0.9510565162951535312, 1.000000000000000000, 0.9510565162951535312, 1.000000000000000000, 0.9510565162951535312, 1.000000000000000000, 0.9510565162951535312, 1.000000000000000000, 0.9510565162951535312, 1.000000000000000000, 0.9510565162951535312, 1.000000000000000000, 0.9510565162951535312, 1.000000000000000000, 0.9510565162951535312, 1.000000000000000000, 0.9510565162951535312, 1.000000000000000000, 0.9510565162951535312, 1.000000000000000000, 0.9510565162951535312, 1.000000000000000000, 0.9510565162951535312, 1.000000000000000000, 0.9510565162951535312, 1.000000000000000000, 0.9510565162951535312, 1.000000000000000000, 0.9510565162951535312, 1.000000000000000000, 0.9510565162951535312, 1.000000000000000000, 0.9510565162951535312, 1.000000000000000000, 0.9510565162951535312, 1.000000000000000000, 0.9510565162951535312, 1.000000000000000000, 0.9510565162951535312, 1.000000000000000000, 0.9510565162951535312, 1.000000000000000000, 0.9510565162951535312, 1.000000000000000000, 0.9510565162951535312, 1.000000000000000000, 0.9510565162951535312, 1.000000000000000000, 0.9510565162951535312, 1.000000000000000000, 0.9510565162951535312, 1.000000000000000000, 0.9510565162951535312, 1.000000000000000000, 0.9510565162951535312, 1.000000000000000000, 0.9510565162951535312, 1.000000000000000000, 0.9510565162951535312, 1.000000000000000000, 0.9510565162951535312, 1.000000000000000000, 0.9510565162951535312, 1.000000000000000000, 0.9510565162951535312, 1.000000000000000000, 0.9510565162951535312, 1.000000000000000000, 0.9510565162951535312, 1.000000000000000000),
 ( 1.000000000000000000, 0.9510565162951535312, 1.000000000000000000, 0.9510565162951535312, 1.000000000000000000, 0.9510565162951535312, 1.000000000000000000, 0.9510565162951535312, 1.000000000000000000, 0.9510565162951535312, 1.000000000000000000, 0.9510565162951535312, 1.000000000000000000, 0.9510565162951535312, 1.000000000000000000, 0.9510565162951535312, 1.000000000000000000, 0.9510565162951535312, 1.000000000000000000, 0.9510565162951535312, 1.000000000000000000, 0.9510565162951535312, 1.000000000000000000, 0.9510565162951535312, 1.000000000000000000, 0.9510565162951535312, 1.000000000000000000, 0.9510565162951535312, 1.000000000000000000, 0.9510565162951535312, 1.000000000000000000, 0.9510565162951535312, 1.000000000000000000, 0.9510565162951535312, 1.000000000000000000, 0.9510565162951535312, 1.000000000000000000, 0.9510565162951535312, 1.000000000000000000, 0.9510565162951535312, 1.000000000000000000, 0.9510565162951535312, 1.000000000000000000, 0.9510565162951535312, 1.000000000000000000, 0.9510565162951535312, 1.000000000000000000, 0.9510565162951535312, 1.000000000000000000, 0.9510565162951535312, 1.000000000000000000, 0.9510565162951535312, 1.000000000000000000, 0.9510565162951535312, 1.000000000000000000, 0.9510565162951535312, 1.000000000000000000, 0.9510565162951535312, 1.000000000000000000, 0.9510565162951535312, 1.000000000000000000, 0.9510565162951535312, 1.000000000000000000, 0.9510565162951535312, 1.000000000000000000, 0.9510565162951535312, 1.000000000000000000, 0.9510565162951535312, 1.000000000000000000, 0.9510565162951535312, 1.000000000000000000, 0.9510565162951535312, 1.000000000000000000, 0.9510565162951535312, 1.000000000000000000, 0.9510565162951535312, 1.000000000000000000, 0.9510565162951535312, 1.000000000000000000, 0.9510565162951535312, 1.000000000000000000, 0.9510565162951535312, 1.000000000000000000, 0.9510565162951535312, 1.000000000000000000, 0.9510565162951535312, 1.000000000000000000, 0.9510565162951535312, 1.000000000000000000, 0.9510565162951535312, 1.000000000000000000, 0.9510565162951535312, 1.000000000000000000, 0.9510565162951535312, 1.000000000000000000, 0.9510565162951535312, 1.000000000000000000, 0.9510565162951535312, 1.000000000000000000, 0.9510565162951535312, 1.000000000000000000, 0.9510565162951535312, 1.000000000000000000, 0.9510565162951535312, 1.000000000000000000, 0.9510565162951535312, 1.000000000000000000, 0.9510565162951535312, 1.000000000000000000, 0.9510565162951535312, 1.000000000000000000, 0.9510565162951535312, 1.000000000000000000, 0.9510565162951535312, 1.000000000000000000, 0.9510565162951535312, 1.000000000000000000, 0.9510565162951535312, 1.000000000000000000, 0.9510565162951535312, 1.000000000000000000, 0.9510565162951535312, 1.000000000000000000, 0.9510565162951535312, 1.000000000000000000, 0.9510565162951535312, 1.000000000000000000, 0.9510565162951535312, 1.000000000000000000, 0.9510565162951535312, 1.000000000000000000, 0.9510565162951535312, 1.000000000000000000, 0.9510565162951535312, 1.000000000000000000, 0.9510565162951535312, 1.000000000000000000, 0.9510565162951535312, 1.000000000000000000, 0.9510565162951535312, 1.000000000000000000, 0.9510565162951535312, 1.000000000000000000, 0.9510565162951535312, 1.000000000000000000, 0.9510565162951535312, 1.000000000000000000, 0.9510565162951535312, 1.000000000000000000, 0.9510565162951535312, 1.000000000000000000, 0.9510565162951535312, 1.000000000000000000, 0.9510565162951535312, 1.000000000000000000, 0.9510565162951535312, 1.000000000000000000, 0.9510565162951535312, 1.000000000000000000, 0.9510565162951535312, 1.000000000000000000, 0.9510565162951535312, 1.000000000000000000, 0.9510565162951535312, 1.000000000000000000, 0.9510565162951535312, 1.000000000000000000, 0.9510565162951535312, 1.000000000000000000, 0.9510565162951535312, 1.000000000000000000, 0.9510565162951535312, 1.000000000000000000, 0.9510565162951535312, 1.000000000000000000, 0.9510565162951535312, 1.000000000000000000, 0.9510565162951535312, 1.000000000000000000, 0.9510565162951535312, 1.000000000000000000, 0.9510565162951535312, 1.000000000000000000, 0.9510565162951535312, 1.000000000000000000, 0.9510565162951535312, 1.000000000000000000, 0.9510565162951535312, 1.000000000000000000, 0.9510565162951535312, 1.000000000000000000, 0.9510565162951535312, 1.000000000000000000, 0.9510565162951535312, 1.000000000000000000, 0.9510565162951535312, 1.000000000000000000, 0.9510565162951535312, 1.000000000000000000, 0.9510565162951535312, 1.000000000000000000, 0.9510565162951535312, 1.000000000000000000, 0.9510565162951535312, 1.000000000000000000, 0.9510565162951535312, 1.000000000000000000, 0.9510565162951535312, 1.000000000000000000, 0.9510565162951535312, 1.000000000000000000, 0.9510565162951535312, 1.000000000000000000, 0.9510565162951535312, 1.000000000000000000, 0.9510565162951535312, 1.000000000000000000, 0.9510565162951535312, 1.000000000000000000, 0.9510565162951535312, 1.000000000000000000, 0.9510565162951535312, 1.000000000000000000, 0.9510565162951535312, 1.000000000000000000, 0.9510565162951535312, 1.000000000000000000, 0.9510565162951535312, 1.000000000000000000, 0.9510565162951535312, 1.000000000000000000, 0.9510565162951535312, 1.000000000000000000, 0.9510565162951535312, 1.000000000000000000, 0.9510565162951535312, 1.000000000000000000, 0.9510565162951535312, 1.000000000000000000, 0.9510565162951535312, 1.000000000000000000, 0.9510565162951535312, 1.000000000000000000, 0.9510565162951535312, 1.000000000000000000, 0.9510565162951535312, 1.000000000000000000, 0.9510565162951535312, 1.000000000000000000, 0.9510565162951535312, 1.000000000000000000, 0.9510565162951535312, 1.000000000000000000, 0.9510565162951535312, 1.000000000000000000, 0.9510565162951535312, 1.000000000000000000, 0.9510565162951535312, 1.000000000000000000, 0.9510565162951535312, 1.000000000000000000, 0.9510565162951535312, 1.000000000000000000, 0.9510565162951535312, 1.000000000000000000, 0.9510565162951535312, 1.000000000000000000, 0.9510565162951535312, 1.000000000000000000, 0.9510565162951535312, 1.000000000000000000, 0.9510565162951535312, 1.000000000000000000, 0.9510565162951535312, 1.000000000000000000, 0.9510565162951535312, 1.000000000000000000, 0.9510565162951535312, 1.000000000000000000, 0.9510565162951535312, 1.000000000000000000, 0.9510565162951535312, 1.000000000000000000, 0.9510565162951535312, 1.000000000000000000, 0.9510565162951535312, 1.000000000000000000, 0.9510565162951535312, 1.000000000000000000, 0.9510565162951535312, 1.000000000000000000, 0.9510565162951535312, 1.000000000000000000, 0.9510565162951535312, 1.000000000000000000, 0.9510565162951535312, 1.000000000000000000, 0.9510565162951535312, 1.000000000000000000, 0.9510565162951535312, 1.000000000000000000, 0.9510565162951535312, 1.000000000000000000, 0.9510565162951535312, 1.000000000000000000, 0.9510565162951535312, 1.000000000000000000, 0.9510565162951535312, 1.000000000000000000, 0.9510565162951535312, 1.000000000000000000, 0.9510565162951535312, 1.000000000000000000, 0.9510565162951535312, 1.000000000000000000, 0.9510565162951535312, 1.000000000000000000, 0.9510565162951535312, 1.000000000000000000, 0.9510565162951535312, 1.000000000000000000, 0.9510565162951535312, 1.000000000000000000, 0.9510565162951535312, 1.000000000000000000, 0.9510565162951535312, 1.000000000000000000, 0.9510565162951535312, 1.000000000000000000, 0.9510565162951535312, 1.000000000000000000, 0.9510565162951535312, 1.000000000000000000, 0.9510565162951535312, 1.000000000000000000, 0.9510565162951535312, 1.000000000000000000, 0.9510565162951535312, 1.000000000000000000, 0.9510565162951535312, 1.000000000000000000, 0.9510565162951535312, 1.000000000000000000, 0.9510565162951535312, 1.000000000000000000, 0.9510565162951535312, 1.000000000000000000, 0.9510565162951535312, 1.000000000000000000, 0.9510565162951535312, 1.000000000000000000, 0.9510565162951535312, 1.000000000000000000, 0.9510565162951535312, 1.000000000000000000, 0.9510565162951535312, 1.000000000000000000, 0.9510565162951535312, 1.000000000000000000, 0.9510565162951535312, 1.000000000000000000, 0.9510565162951535312, 1.000000000000000000, 0.9510565162951535312, 1.000000000000000000, 0.9510565162951535312, 1.000000000000000000, 0.9510565162951535312, 1.000000000000000000, 0.9510565162951535312, 1.000000000000000000, 0.9510565162951535312, 1.000000000000000000, 0.9510565162951535312, 1.000000000000000000, 0.9510565162951535312, 1.000000000000000000, 0.9510565162951535312, 1.000000000000000000, 0.9510565162951535312, 1.000000000000000000, 0.9510565162951535312, 1.000000000000000000, 0.9510565162951535312, 1.000000000000000000, 0.9510565162951535312, 1.000000000000000000, 0.9510565162951535312, 1.000000000000000000, 0.9510565162951535312, 1.000000000000000000, 0.9510565162951535312, 1.000000000000000000, 0.9510565162951535312, 1.000000000000000000, 0.9510565162951535312, 1.000000000000000000, 0.9510565162951535312, 1.000000000000000000, 0.9510565162951535312, 1.000000000000000000) ) ) 
 REPRESENTATION_ITEM ( '' )  SURFACE ( )  );
#34215 = DIRECTION ( 'NONE',  ( -0.8660254037844359321, -0.5000000000000051070, -0.000000000000000000 ) ) ;
#34216 = CARTESIAN_POINT ( 'NONE',  ( 9.861089372814316079, 17.64441083166259006, -10.00000000000000533 ) ) ;
#34217 = CARTESIAN_POINT ( 'NONE',  ( 195.3624787578944222, 290.3824063481519602, -16.76522224015156226 ) ) ;
#34218 = ORIENTED_EDGE ( 'NONE', *, *, #77158, .F. ) ;
#34219 = CARTESIAN_POINT ( 'NONE',  ( 167.3220989969731818, 280.7870397072532569, 11.65856738288337269 ) ) ;
#34220 = CARTESIAN_POINT ( 'NONE',  ( 147.6512387128590262, 274.9075480792844246, -8.209968531507987777 ) ) ;
#34221 = CARTESIAN_POINT ( 'NONE',  ( 158.0832193973161566, 263.1600005068700057, -16.98150214051203477 ) ) ;
#34222 = EDGE_LOOP ( 'NONE', ( #81515, #41493, #4243, #2592 ) ) ;
#34223 = CARTESIAN_POINT ( 'NONE',  ( 78.93453705340030524, 60.10095773708777500, 16.11389061908799647 ) ) ;
#34224 = DIRECTION ( 'NONE',  ( 0.5000000000000003331, -0.8660254037844384856, -2.218671295934096141E-31 ) ) ;
#34225 = FACE_OUTER_BOUND ( 'NONE', #10345, .T. ) ;
#34226 = VERTEX_POINT ( 'NONE', #47177 ) ;
#34227 = CARTESIAN_POINT ( 'NONE',  ( 83.29773739198154203, 50.25459149593829267, -13.85366754400191525 ) ) ;
#34228 = CARTESIAN_POINT ( 'NONE',  ( 73.37704433742356969, 70.12506801342537699, -9.398789138188929471 ) ) ;
#34229 = CARTESIAN_POINT ( 'NONE',  ( 81.27906948385655994, 42.22991039144485370, -7.243114465301290217 ) ) ;
#34230 = ORIENTED_EDGE ( 'NONE', *, *, #38751, .T. ) ;
#34231 = EDGE_LOOP ( 'NONE', ( #65721, #34606, #55479, #91176 ) ) ;
#34232 = CARTESIAN_POINT ( 'NONE',  ( 94.74134171723733289, 237.0530062829862743, -4.648177544792955347E-16 ) ) ;
#34233 = ORIENTED_EDGE ( 'NONE', *, *, #56574, .T. ) ;
#34234 = FACE_OUTER_BOUND ( 'NONE', #75254, .T. ) ;
#34235 = ORIENTED_EDGE ( 'NONE', *, *, #26893, .F. ) ;
#34236 = DIRECTION ( 'NONE',  ( 0.000000000000000000, 0.000000000000000000, 1.000000000000000000 ) ) ;
#34237 = DIRECTION ( 'NONE',  ( -1.000000000000000000, 9.785293164094327883E-14, 0.000000000000000000 ) ) ;
#34238 = ORIENTED_EDGE ( 'NONE', *, *, #53447, .T. ) ;
#34239 = CARTESIAN_POINT ( 'NONE',  ( 185.8652519749559247, 282.2268457654508325, -16.59405335779809221 ) ) ;
#34240 = CARTESIAN_POINT ( 'NONE',  ( 82.17778236580524265, 40.63545381150629510, 3.437353603792591805 ) ) ;
#34241 = PLANE ( 'NONE',  #78043 ) ;
#34242 = CARTESIAN_POINT ( 'NONE',  ( 158.7111944379298336, 274.7584504872774005, -13.07079675756365233 ) ) ;
#34243 = CARTESIAN_POINT ( 'NONE',  ( 193.1649355862271591, 296.0755126543221536, -12.21556774862162698 ) ) ;
#34244 = CARTESIAN_POINT ( 'NONE',  ( 152.6873874250818517, 266.1846826352417565, -16.66598363829485763 ) ) ;
#34245 = CARTESIAN_POINT ( 'NONE',  ( 87.17876410986579572, 43.10751584725982610, -0.2475519180087527027 ) ) ;
#34246 = CARTESIAN_POINT ( 'NONE',  ( 2.620201125542898080, 178.9865022471903160, 10.00000000000009415 ) ) ;
#34247 = CARTESIAN_POINT ( 'NONE',  ( 137.8731756836298814, 262.6589784336661069, -6.496448406907675876E-16 ) ) ;
#34248 = CARTESIAN_POINT ( 'NONE',  ( 70.75845742388486315, 61.42534300271167069, -14.83394790560162413 ) ) ;
#34249 = ORIENTED_EDGE ( 'NONE', *, *, #65679, .T. ) ;
#34250 = ADVANCED_FACE ( 'NONE', ( #45669 ), #78099, .T. ) ;
#34252 = EDGE_LOOP ( 'NONE', ( #16180, #1329, #52009, #71621 ) ) ;
#34251 = CARTESIAN_POINT ( 'NONE',  ( 85.58533047404948491, 48.36141062822003533, -12.20656690058574689 ) ) ;
#34253 = CARTESIAN_POINT ( 'NONE',  ( 1.230952036757517520, 161.5177522451418213, 5.000000000000051514 ) ) ;
#34254 = ADVANCED_FACE ( 'NONE', ( #69974 ), #33542, .T. ) ;
#34255 = CARTESIAN_POINT ( 'NONE',  ( 76.26495795533084276, 64.90087152775714685, -14.31572824905659935 ) ) ;
#34256 = CARTESIAN_POINT ( 'NONE',  ( 190.2409037545352817, 300.2489383464547927, 3.136352422388450911 ) ) ;
#34257 = CARTESIAN_POINT ( 'NONE',  ( 157.7405083909982295, 280.7048132376855847, -7.110344775676333384 ) ) ;
#34258 = CARTESIAN_POINT ( 'NONE',  ( 21.61448739737248559, 51.35407934543722774, 59.99999999999999289 ) ) ;
#34259 = CARTESIAN_POINT ( 'NONE',  ( 171.7908256294744831, 280.0902348243839128, 13.88385109847706644 ) ) ;
#34260 = CIRCLE ( 'NONE', #60117, 10.00000000000001066 ) ;
#34261 = DIRECTION ( 'NONE',  ( -0.000000000000000000, -0.000000000000000000, -1.000000000000000000 ) ) ;
#34262 = CARTESIAN_POINT ( 'NONE',  ( 88.19053702688614749, 44.32527345396093921, -2.493626234014362009 ) ) ;
#34263 = ORIENTED_EDGE ( 'NONE', *, *, #29795, .T. ) ;
#34264 = CARTESIAN_POINT ( 'NONE',  ( 185.0512884836414855, 273.0606714723194841, -16.92976292810380556 ) ) ;
#34265 = CARTESIAN_POINT ( 'NONE',  ( 65.97951220193175459, 68.67161866859687791, -0.1777484692489773310 ) ) ;
#34266 = ORIENTED_EDGE ( 'NONE', *, *, #90029, .F. ) ;
#34268 = EDGE_CURVE ( 'NONE', #48220, #41092, #83298, .T. ) ;
#34267 = CARTESIAN_POINT ( 'NONE',  ( 164.0851047064185479, 278.1576806158360569, 13.30924083603244945 ) ) ;
#34269 = CARTESIAN_POINT ( 'NONE',  ( 156.3862274318223626, 277.3475818783230693, 10.00078872878025571 ) ) ;
#34270 = FACE_OUTER_BOUND ( 'NONE', #27571, .T. ) ;
#34271 = CARTESIAN_POINT ( 'NONE',  ( 81.33896983113768897, 44.83237125196090034, -10.57384344836858325 ) ) ;
#34272 = CARTESIAN_POINT ( 'NONE',  ( 202.3139361598622372, 280.2289788223093865, 15.93832709035092421 ) ) ;
#34274 = CARTESIAN_POINT ( 'NONE',  ( 88.28217478145764119, 43.95791727297697804, 2.470383038495642669 ) ) ;
#34273 = DIRECTION ( 'NONE',  ( -0.9182972510888841589, 0.3958915996110536906, 0.000000000000000000 ) ) ;
#34275 = CARTESIAN_POINT ( 'NONE',  ( 201.5343969995564635, 268.9872460397318719, 6.024498516268275594 ) ) ;
#34276 = EDGE_LOOP ( 'NONE', ( #65229, #10330, #41820, #28111 ) ) ;
#34277 = CARTESIAN_POINT ( 'NONE',  ( 12.50963621419470329, 166.4824982072973967, 3.021315404115420679E-15 ) ) ;
#34278 = CARTESIAN_POINT ( 'NONE',  ( 80.12217583349386985, 58.13818462438354828, 16.26693196410659326 ) ) ;
#34279 = EDGE_CURVE ( 'NONE', #53306, #66866, #19243, .T. ) ;
#34280 = LINE ( 'NONE', #11992, #62943 ) ;
#34281 = EDGE_CURVE ( 'NONE', #47682, #10473, #27880, .T. ) ;
#34282 = CARTESIAN_POINT ( 'NONE',  ( 192.6773196027083372, 296.9200883123592689, 11.15745042875121484 ) ) ;
#34283 = CARTESIAN_POINT ( 'NONE',  ( 80.85183824906197003, 42.96989659668948747, -9.583637002236184088 ) ) ;
#34284 = DIRECTION ( 'NONE',  ( -1.000000000000000000, 0.000000000000000000, 0.000000000000000000 ) ) ;
#34285 = CARTESIAN_POINT ( 'NONE',  ( 163.0309151244508712, 248.2691671304387739, 11.27270415168660200 ) ) ;
#34286 = CARTESIAN_POINT ( 'NONE',  ( 6.183361268541194278, 180.5024278399160664, 9.188101187500095079 ) ) ;
#34287 = CARTESIAN_POINT ( 'NONE',  ( 105.6144235841895664, 219.5327760586659451, 1.948934522072303157E-15 ) ) ;
#34288 = CARTESIAN_POINT ( 'NONE',  ( 203.5629025532486196, 278.0657055720176913, -15.85226727704602823 ) ) ;
#34289 = DIRECTION ( 'NONE',  ( -0.04218457335174585071, -0.9991098346884246251, 0.000000000000000000 ) ) ;
#34290 = CARTESIAN_POINT ( 'NONE',  ( 180.0469694969276588, 255.4107081643116715, -2.376983049801016712 ) ) ;
#34291 = LINE ( 'NONE', #65188, #96634 ) ;
#34292 = AXIS2_PLACEMENT_3D ( 'NONE', #87241, #72494, #41040 ) ;
#34293 = CARTESIAN_POINT ( 'NONE',  ( 77.55539304566268299, 52.43243923690647534, 15.72493065762432174 ) ) ;
#34294 = CARTESIAN_POINT ( 'NONE',  ( 161.0074043740847856, 281.6987162223563814, 5.593313803799454753 ) ) ;
#34295 = PLANE ( 'NONE',  #75926 ) ;
#34296 = CARTESIAN_POINT ( 'NONE',  ( 181.0995730718790071, 291.1750261779234279, 9.327186099670552011 ) ) ;
#34297 = EDGE_CURVE ( 'NONE', #33351, #49306, #79044, .T. ) ;
#34298 = DIRECTION ( 'NONE',  ( 1.000000000000000000, 0.000000000000000000, 0.000000000000000000 ) ) ;
#34299 = CARTESIAN_POINT ( 'NONE',  ( 164.6595190653735870, 245.4483423593538305, -5.562352988119640962 ) ) ;
#34300 = CARTESIAN_POINT ( 'NONE',  ( 80.95010002000924487, 53.96101425250913763, -15.71262299032070331 ) ) ;
#34301 = CARTESIAN_POINT ( 'NONE',  ( 166.2257170601846497, 253.6475096207515492, -13.42941508109017690 ) ) ;
#34302 = EDGE_CURVE ( 'NONE', #20754, #74292, #43575, .T. ) ;
#34303 = CARTESIAN_POINT ( 'NONE',  ( 75.37662461738884190, 53.50075842301595230, 16.04033158989234309 ) ) ;
#34304 = CARTESIAN_POINT ( 'NONE',  ( 79.98487687335507701, 226.1744531367911293, 4.594050593750047540 ) ) ;
#34305 = CARTESIAN_POINT ( 'NONE',  ( 207.7320178805681508, 270.8445860024863237, -5.379955943374661764 ) ) ;
#34306 = CARTESIAN_POINT ( 'NONE',  ( 72.47345658542111835, 57.49201715091417952, 15.81387984723518159 ) ) ;
#34307 = EDGE_CURVE ( 'NONE', #1103, #4020, #82248, .T. ) ;
#34308 = DIRECTION ( 'NONE',  ( -3.817860598523670672E-18, -1.090355031989287297E-16, -1.000000000000000000 ) ) ;
#34310 = DIRECTION ( 'NONE',  ( 0.4999999999999998890, -0.8660254037844385966, 0.000000000000000000 ) ) ;
#34309 = CARTESIAN_POINT ( 'NONE',  ( -68.29659580619643577, 42.72804590294295224, -10.00000000000000000 ) ) ;
#34311 = CARTESIAN_POINT ( 'NONE',  ( 176.2999854890552172, 269.8567107842857240, -17.42186202513282112 ) ) ;
#34312 = EDGE_CURVE ( 'NONE', #4372, #91593, #20293, .T. ) ;
#34313 = CARTESIAN_POINT ( 'NONE',  ( 35.77386594998528579, 21.44966523072496756, -2.296566073217252530E-15 ) ) ;
#34314 = CARTESIAN_POINT ( 'NONE',  ( 79.77267820561851863, 49.16024335904899090, -14.73473614307763846 ) ) ;
#34315 = CARTESIAN_POINT ( 'NONE',  ( 74.32283972735670829, 55.33658384534070507, 16.60204640374922036 ) ) ;
#34316 = VERTEX_POINT ( 'NONE', #19321 ) ;
#34317 = CARTESIAN_POINT ( 'NONE',  ( 21.54279312762077936, 14.29860640527291871, -2.839279412974138328 ) ) ;
#34318 = CARTESIAN_POINT ( 'NONE',  ( 72.38035161819672680, 212.5958772461660544, -9.188101187500095079 ) ) ;
#34319 = CARTESIAN_POINT ( 'NONE',  ( 170.8968330173543109, 288.5550931528428009, -1.069972840386552049 ) ) ;
#34320 = CARTESIAN_POINT ( 'NONE',  ( -32.70769541684651216, 94.08906143139476796, 10.41629251971181702 ) ) ;
#34321 = CARTESIAN_POINT ( 'NONE',  ( 188.9765056315804088, 286.3781189046455893, -15.97876018633670725 ) ) ;
#34322 = EDGE_CURVE ( 'NONE', #78871, #80478, #11871, .T. ) ;
#34323 = VERTEX_POINT ( 'NONE', #36469 ) ;
#34324 = CARTESIAN_POINT ( 'NONE',  ( 86.30241807085522510, 47.23217017718856425, 10.82197119102028893 ) ) ;
#34325 = CARTESIAN_POINT ( 'NONE',  ( 190.0153548218945048, 286.5829638478824677, 16.39362643471642755 ) ) ;
#34326 = CARTESIAN_POINT ( 'NONE',  ( 191.2622316156482043, 288.8574828335728171, -16.55244734589887656 ) ) ;
#34327 = CARTESIAN_POINT ( 'NONE',  ( 121.2656814440110367, 247.4865022471903444, -10.00000000000009415 ) ) ;
#34328 = CARTESIAN_POINT ( 'NONE',  ( 205.2391015854675516, 275.1624436846170738, -14.01434138479280911 ) ) ;
#34329 = B_SPLINE_CURVE_WITH_KNOTS ( 'NONE', 3,
 ( #10011, #40875, #3425, #89076, #88065, #80956, #71820, #34300, #18614, #64197, #78930, #65200, #26208, #3904, #27207, #58093, #96142, #49493, #32794, #56593, #18107, #26702, #49008, #1911, #79942, #10503, #57585, #41385, #72328, #2931, #25192, #63701, #11522, #50001, #33820, #88563, #19626, #95659, #64708, #57085, #19127, #42380, #73312, #9519, #40379, #94637 ),
 .UNSPECIFIED., .F., .F.,
 ( 4, 1, 2, 2, 1, 2, 2, 1, 1, 2, 2, 1, 1, 2, 2, 1, 1, 2, 2, 1, 1, 1, 2, 2, 1, 1, 1, 2, 2, 4 ),
 ( 0.000000000000000000, 0.06250000000000385803, 0.09375000000000578704, 0.1250000000000077161, 0.1875000000000154876, 0.2187500000000190681, 0.2500000000000226485, 0.3125000000000335287, 0.3437500000000370259, 0.3593750000000391354, 0.3750000000000411893, 0.4375000000000595080, 0.4687500000000667244, 0.4843750000000707767, 0.5000000000000747180, 0.5625000000000771605, 0.5937500000000761613, 0.6093750000000776046, 0.6250000000000790479, 0.6875000000000812683, 0.7187500000000821565, 0.7343750000000806022, 0.7421875000000799361, 0.7500000000000791589, 0.8125000000000575096, 0.8437500000000466294, 0.8593750000000411893, 0.8671875000000386358, 0.8750000000000360822, 1.000000000000000000 ),
 .UNSPECIFIED. ) ;
#34330 = CARTESIAN_POINT ( 'NONE',  ( 74.74299343307386323, 53.49955268462365865, 16.07385381711848638 ) ) ;
#34331 = ORIENTED_EDGE ( 'NONE', *, *, #18872, .T. ) ;
#34332 = CARTESIAN_POINT ( 'NONE',  ( 169.5338548541099897, 248.2712795993637371, -1.960221964079814860 ) ) ;
#34333 = ORIENTED_EDGE ( 'NONE', *, *, #83301, .F. ) ;
#34334 = CARTESIAN_POINT ( 'NONE',  ( 162.9148248802443106, 248.4702413316674381, 9.709394404200100581 ) ) ;
#34335 = CARTESIAN_POINT ( 'NONE',  ( 207.3718082758823869, 270.6308103407627073, -0.3710573916699856922 ) ) ;
#34336 = CARTESIAN_POINT ( 'NONE',  ( 153.3859906278383676, 264.9746663937372091, -17.41799046551451013 ) ) ;
#34337 = VERTEX_POINT ( 'NONE', #67883 ) ;
#34338 = CARTESIAN_POINT ( 'NONE',  ( -19.65312891409030271, 93.06504152958497400, 177.5919119679930134 ) ) ;
#34339 = ORIENTED_EDGE ( 'NONE', *, *, #24685, .T. ) ;
#34340 = CARTESIAN_POINT ( 'NONE',  ( 189.3827389365466445, 289.9845130480852049, 14.42905932677018122 ) ) ;
#34341 = CARTESIAN_POINT ( 'NONE',  ( 168.5042146316756373, 248.9333234090209430, 3.460101701789785711 ) ) ;
#34342 = CARTESIAN_POINT ( 'NONE',  ( 193.8652130780152731, 280.5836658925297229, -17.72338988841175933 ) ) ;
#34343 = CARTESIAN_POINT ( 'NONE',  ( 193.6888222081633444, 273.0013374295587028, 15.75238434690954747 ) ) ;
#34344 = EDGE_LOOP ( 'NONE', ( #56347, #41757, #66703, #62752 ) ) ;
#34345 = CARTESIAN_POINT ( 'NONE',  ( 103.9451733683222301, 237.4865022471903160, 10.00000000000009415 ) ) ;
#34346 = CARTESIAN_POINT ( 'NONE',  ( 24.92213970864663963, 37.49540643055189548, 3.479690158560446702E-15 ) ) ;
#34347 = CARTESIAN_POINT ( 'NONE',  ( 83.02699437693422624, 48.37159093816767808, -12.75497678487218600 ) ) ;
#34348 = DIRECTION ( 'NONE',  ( 0.8116583814955277143, 0.01378320505840788246, -0.5839697723396121143 ) ) ;
#34349 = CARTESIAN_POINT ( 'NONE',  ( 44.24123536260515976, 207.8967562850346837, -4.648177544792955347E-16 ) ) ;
#34350 = ORIENTED_EDGE ( 'NONE', *, *, #55204, .F. ) ;
#34351 = ORIENTED_EDGE ( 'NONE', *, *, #80926, .T. ) ;
#34352 = CARTESIAN_POINT ( 'NONE',  ( 186.3255980153079747, 298.7107439718217279, 1.073797455116038746 ) ) ;
#34354 = CARTESIAN_POINT ( 'NONE',  ( 194.6943296385021824, 293.4265244509877562, -16.10917128197217352 ) ) ;
#34353 = CARTESIAN_POINT ( 'NONE',  ( 163.9942050550062049, 246.6007000282974673, 5.791111691696777974 ) ) ;
#34355 = CARTESIAN_POINT ( 'NONE',  ( 85.56715572150820037, 48.66046822832736041, 12.44852408270450184 ) ) ;
#34356 = DIRECTION ( 'NONE',  ( -0.000000000000000000, -0.000000000000000000, -1.000000000000000000 ) ) ;
#34357 = CARTESIAN_POINT ( 'NONE',  ( 132.0211419364472363, 235.4824982072973683, 3.021315404115420679E-15 ) ) ;
#34358 = CARTESIAN_POINT ( 'NONE',  ( 187.6043408702985005, 291.4350663380896549, -13.94014698167784161 ) ) ;
#34359 = CARTESIAN_POINT ( 'NONE',  ( 164.0673170565375187, 246.4740663270022765, 4.489294478468116800 ) ) ;
#34360 = CARTESIAN_POINT ( 'NONE',  ( 165.9079365288987162, 265.8636615913461014, 16.81383221254800375 ) ) ;
#34361 = CARTESIAN_POINT ( 'NONE',  ( -70.00000000000000000, 20.00000000000000000, 59.99999999999999289 ) ) ;
#34362 = CARTESIAN_POINT ( 'NONE',  ( 106.1553423657898492, 232.0958772461660260, -9.188101187500095079 ) ) ;
#34364 = ORIENTED_EDGE ( 'NONE', *, *, #39691, .T. ) ;
#34363 = B_SPLINE_CURVE_WITH_KNOTS ( 'NONE', 3,
 ( #89388, #3746, #35622, #19939 ),
 .UNSPECIFIED., .F., .F.,
 ( 4, 4 ),
 ( 0.01639396528500873529, 0.02525301955254147593 ),
 .UNSPECIFIED. ) ;
#34365 = CARTESIAN_POINT ( 'NONE',  ( 73.91024718746507460, 55.00110737226054880, -16.60404657609226575 ) ) ;
#34366 = CARTESIAN_POINT ( 'NONE',  ( 163.0250628725154058, 276.5629096397734088, -14.03379528916789809 ) ) ;
#34367 = ORIENTED_EDGE ( 'NONE', *, *, #45399, .T. ) ;
#34368 = AXIS2_PLACEMENT_3D ( 'NONE', #98516, #59971, #58961 ) ;
#34369 = VERTEX_POINT ( 'NONE', #20799 ) ;
#34370 = CARTESIAN_POINT ( 'NONE',  ( 87.18059948837544937, 46.13477641244298155, -8.300795534149866484 ) ) ;
#34372 = B_SPLINE_SURFACE_WITH_KNOTS ( 'NONE', 3, 1, ( 
 ( #27930, #82190 ),
 ( #57333, #43626 ),
 ( #28425, #11270 ),
 ( #90287, #20856 ),
 ( #78787, #40253 ),
 ( #34063, #64954 ),
 ( #88307, #45122 ),
 ( #68420, #99347 ),
 ( #91760, #52222 ),
 ( #29431, #84663 ),
 ( #14727, #30923 ),
 ( #83167, #44116 ),
 ( #51748, #7118 ),
 ( #60307, #92758 ),
 ( #45608, #21828 ),
 ( #67423, #84178 ),
 ( #76540, #82690 ),
 ( #98355, #13256 ),
 ( #28943, #44608 ),
 ( #98855, #38003 ),
 ( #60801, #61808 ),
 ( #38512, #91264 ),
 ( #75053, #83672 ),
 ( #52714, #77017 ),
 ( #5629, #68916 ),
 ( #59820, #6638 ),
 ( #69424, #37 ),
 ( #22325, #36523 ),
 ( #75543, #99841 ),
 ( #67934, #90786 ),
 ( #53226, #30425 ) ),
 .UNSPECIFIED., .F., .F., .F.,
 ( 4, 3, 3, 3, 3, 3, 3, 3, 3, 3, 4 ),
 ( 2, 2 ),
 ( 0.000000000000000000, 0.1122669598086788734, 0.2243161639709606303, 0.3396355846219134000, 0.4553962076585122976, 0.5677860799922305191, 0.6749047109689531032, 0.7773884377078198460, 0.8775581155834139002, 0.9782364162377853445, 1.000000000000000000 ),
 ( 0.000000000000000000, 1.000000000000000000 ),
 .UNSPECIFIED. ) ;
#34371 = CARTESIAN_POINT ( 'NONE',  ( 197.4842693130445923, 286.5942071846287149, -17.75505217046438489 ) ) ;
#34373 = CARTESIAN_POINT ( 'NONE',  ( 30.93718178480143521, 33.56454794089042082, 10.00000000000000355 ) ) ;
#34374 = CARTESIAN_POINT ( 'NONE',  ( 42.33744422746375591, 122.7866300363639169, 10.00000000000000000 ) ) ;
#34375 = CARTESIAN_POINT ( 'NONE',  ( 208.3408670980087152, 269.7900282237308147, 2.175586895783760077 ) ) ;
#34376 = CARTESIAN_POINT ( 'NONE',  ( 101.1217432541752856, 223.0643266524159571, -9.188101187500093303 ) ) ;
#34377 = ORIENTED_EDGE ( 'NONE', *, *, #46009, .F. ) ;
#34378 = VERTEX_POINT ( 'NONE', #19803 ) ;
#34379 = CARTESIAN_POINT ( 'NONE',  ( 24.69086998626516305, 38.90223361192549589, 10.00000000000000000 ) ) ;
#34380 = ORIENTED_EDGE ( 'NONE', *, *, #94976, .F. ) ;
#34381 = EDGE_CURVE ( 'NONE', #73648, #67744, #21291, .T. ) ;
#34382 = AXIS2_PLACEMENT_3D ( 'NONE', #12735, #87792, #65413 ) ;
#34383 = CARTESIAN_POINT ( 'NONE',  ( 75.72636783681542738, 65.12249353091223725, -14.45027308884206718 ) ) ;
#34384 = CARTESIAN_POINT ( 'NONE',  ( 94.74134171723733289, 237.0530062829862743, -4.648177544792955347E-16 ) ) ;
#34385 = CYLINDRICAL_SURFACE ( 'NONE', #95349, 10.00000000000010658 ) ;
#34387 = CARTESIAN_POINT ( 'NONE',  ( 69.45603412936870313, 62.99601925590414453, -13.63678823767287973 ) ) ;
#34386 = CARTESIAN_POINT ( 'NONE',  ( 133.0835800865360170, 238.4548013555409796, -4.594050593750042211 ) ) ;
#34388 = DIRECTION ( 'NONE',  ( -0.1032265479692960342, 0.9946578707245736783, 0.000000000000000000 ) ) ;
#34389 = FACE_OUTER_BOUND ( 'NONE', #73134, .T. ) ;
#34390 = ORIENTED_EDGE ( 'NONE', *, *, #59673, .T. ) ;
#34391 = CARTESIAN_POINT ( 'NONE',  ( 204.8467418195402843, 275.8420307340491036, 13.15258587511997135 ) ) ;
#34392 = CARTESIAN_POINT ( 'NONE',  ( 160.5681497667090980, 275.6440229244402644, 12.83602361646179801 ) ) ;
#34393 = CARTESIAN_POINT ( 'NONE',  ( 159.8597520197352537, 253.7617827468940277, -16.74905990210778839 ) ) ;
#34394 = CARTESIAN_POINT ( 'NONE',  ( 192.3665687060960465, 271.8525640515161967, 14.11498752457012351 ) ) ;
#34396 = EDGE_CURVE ( 'NONE', #26854, #44175, #39625, .T. ) ;
#34395 = CARTESIAN_POINT ( 'NONE',  ( 178.3938943706652651, 285.5145968506380996, 14.34020567925480982 ) ) ;
#34397 = DIRECTION ( 'NONE',  ( -0.3782958374750524655, 0.000000000000000000, -0.9256847516023197775 ) ) ;
#34398 = EDGE_CURVE ( 'NONE', #90851, #45207, #13685, .T. ) ;
#34399 = CARTESIAN_POINT ( 'NONE',  ( 40.70814378237798081, 60.14496435084704018, -10.00000000000000000 ) ) ;
#34400 = CARTESIAN_POINT ( 'NONE',  ( 78.86219776201926379, 59.55369065033507070, 16.50996775951928086 ) ) ;
#34401 = CARTESIAN_POINT ( 'NONE',  ( 200.6800100461949228, 283.0590218669948399, 18.32402613046234308 ) ) ;
#34402 = FACE_OUTER_BOUND ( 'NONE', #87386, .T. ) ;
#34403 = CARTESIAN_POINT ( 'NONE',  ( 206.8791291248445532, 272.3218326606039454, -10.16823074922856840 ) ) ;
#34404 = CARTESIAN_POINT ( 'NONE',  ( 178.5319624062738058, 291.5826149054348093, -6.133725113071555768 ) ) ;
#34405 = CARTESIAN_POINT ( 'NONE',  ( -27.42236680055714260, 166.5217562850347406, 1.224646799147364892E-15 ) ) ;
#34406 = CARTESIAN_POINT ( 'NONE',  ( 34.54807858326547176, 25.11029122506296929, -8.090169943749478065 ) ) ;
#34407 = CARTESIAN_POINT ( 'NONE',  ( 72.12429762571967728, 64.53244924666101667, -13.11970522421019503 ) ) ;
#34409 = CARTESIAN_POINT ( 'NONE',  ( 74.25393038840245197, 55.45593832152543712, 16.12141555578006447 ) ) ;
#34408 = CARTESIAN_POINT ( 'NONE',  ( 180.7138497164156661, 266.8527603518880937, -16.19060323297924242 ) ) ;
#34410 = CARTESIAN_POINT ( 'NONE',  ( 168.7933227874096929, 282.1232148736041268, 13.17276477419401459 ) ) ;
#34411 = CARTESIAN_POINT ( 'NONE',  ( 35.14347105191519205, 25.45404122711135741, -8.090169943749478065 ) ) ;
#34412 = CARTESIAN_POINT ( 'NONE',  ( 27.76992210170819675, 43.29297894285233639, -10.00000000000000000 ) ) ;
#34413 = CARTESIAN_POINT ( 'NONE',  ( 155.3716771045260714, 261.5353565282119348, -18.54934131471355840 ) ) ;
#34414 = PLANE ( 'NONE',  #25462 ) ;
#34415 = CYLINDRICAL_SURFACE ( 'NONE', #22634, 70.00000000000002842 ) ;
#34416 = CARTESIAN_POINT ( 'NONE',  ( 87.39545338979795019, 43.86517562418462290, -2.489615843231432368 ) ) ;
#34417 = EDGE_CURVE ( 'NONE', #47161, #82896, #98887, .T. ) ;
#34418 = CARTESIAN_POINT ( 'NONE',  ( 7.915412076110063033, 181.5024278399160664, -9.188101187500093303 ) ) ;
#34419 = CARTESIAN_POINT ( 'NONE',  ( 83.03097277809888510, 51.42467778882387819, 14.50400025335057208 ) ) ;
#34420 = EDGE_LOOP ( 'NONE', ( #53556, #82239, #63753, #53201 ) ) ;
#34421 = EDGE_CURVE ( 'NONE', #56117, #5319, #28715, .T. ) ;
#34422 = CARTESIAN_POINT ( 'NONE',  ( 87.25346308258933448, 46.04525953206349698, 8.773708642049088624 ) ) ;
#34423 = EDGE_CURVE ( 'NONE', #92377, #25562, #95722, .T. ) ;
#34424 = CARTESIAN_POINT ( 'NONE',  ( 184.5121120432382611, 270.3687502014600454, 16.77398936818960351 ) ) ;
#34425 = CARTESIAN_POINT ( 'NONE',  ( 81.92146693744936670, 41.17928938369797009, 5.561051477722002367 ) ) ;
#34426 = CARTESIAN_POINT ( 'NONE',  ( 30.29666933122289407, 197.4869531367911293, 4.594050593750046652 ) ) ;
#34427 = CARTESIAN_POINT ( 'NONE',  ( 161.7587802986029999, 250.4725692828850754, 14.33336164792646450 ) ) ;
#34428 = CARTESIAN_POINT ( 'NONE',  ( 190.7569505155522904, 300.2462651405980978, -5.670926626284815697 ) ) ;
#34429 = CARTESIAN_POINT ( 'NONE',  ( 40.24855657362158468, 31.43677371833804912, -10.00000000000000355 ) ) ;
#34430 = CARTESIAN_POINT ( 'NONE',  ( 178.4427175726033568, 291.7705066098333759, 5.794587143940031382 ) ) ;
#34431 = CARTESIAN_POINT ( 'NONE',  ( 191.0604813119340690, 299.7205343796033503, -9.270812881586136811 ) ) ;
#34432 = CARTESIAN_POINT ( 'NONE',  ( 160.0166746459236435, 283.6086068001695253, 2.232576205374148248 ) ) ;
#34433 = CARTESIAN_POINT ( 'NONE',  ( 5.618660645053492608, 25.01751292744054211, 6.180339887498949913 ) ) ;
#34434 = EDGE_CURVE ( 'NONE', #51782, #36590, #56368, .T. ) ;
#34435 = CARTESIAN_POINT ( 'NONE',  ( 165.0676804254514138, 257.0913205595731483, -14.93706007131700098 ) ) ;
#34436 = VECTOR ( 'NONE', #91425, 1000.000000000000000 ) ;
#34437 = EDGE_CURVE ( 'NONE', #47944, #37486, #96393, .T. ) ;
#34438 = CARTESIAN_POINT ( 'NONE',  ( 83.98894966577088894, 51.79070771454841804, 14.82098776213804392 ) ) ;
#34439 = CARTESIAN_POINT ( 'NONE',  ( 78.46959274032997200, 226.1115022471903160, -5.000000000000047962 ) ) ;
#34440 = PLANE ( 'NONE',  #96025 ) ;
#34441 = CARTESIAN_POINT ( 'NONE',  ( 162.1170296077141018, 267.9449120310337662, -16.75957877514680661 ) ) ;
#34442 = CARTESIAN_POINT ( 'NONE',  ( 54.03161192339643293, 195.8768266524159856, -9.188101187500091527 ) ) ;
#34443 = VERTEX_POINT ( 'NONE', #17671 ) ;
#34444 = CARTESIAN_POINT ( 'NONE',  ( 30.62489312496363425, 46.16797101519271962, 10.00000000000000000 ) ) ;
#34445 = CARTESIAN_POINT ( 'NONE',  ( 146.9709166616330549, 276.0859004375172390, 3.755270622130282732 ) ) ;
#34446 = CARTESIAN_POINT ( 'NONE',  ( 67.00965166525888606, 66.88736477923252721, -8.820170631815919648 ) ) ;
#34447 = ORIENTED_EDGE ( 'NONE', *, *, #45572, .T. ) ;
#34449 = CARTESIAN_POINT ( 'NONE',  ( 167.8870021103015233, 285.0517102558676470, 7.659404562680429684 ) ) ;
#34448 = CIRCLE ( 'NONE', #40936, 70.00000000000001421 ) ;
#34450 = CARTESIAN_POINT ( 'NONE',  ( 164.9404048476745004, 244.9618339132846074, -2.801285734921658666 ) ) ;
#34451 = CARTESIAN_POINT ( 'NONE',  ( 46.85966550219794158, 197.8615022471903728, 4.537668576076727938E-14 ) ) ;
#34452 = CARTESIAN_POINT ( 'NONE',  ( 26.56877070717806788, 23.84335787977763843, 9.188101187500006262 ) ) ;
#34453 = CARTESIAN_POINT ( 'NONE',  ( 73.09359486087168989, 70.66713452829003472, -7.730905117165903562 ) ) ;
#34454 = CARTESIAN_POINT ( 'NONE',  ( 196.2630260332681189, 290.7094625936034049, -17.43112004684450866 ) ) ;
#34455 = CARTESIAN_POINT ( 'NONE',  ( 171.3320430264542154, 255.7635525530785401, 11.44407331594274524 ) ) ;
#34456 = VERTEX_POINT ( 'NONE', #48571 ) ;
#34457 = CARTESIAN_POINT ( 'NONE',  ( 13.54711677929152636, 28.79752408145591858, -5.678558825948271327 ) ) ;
#34458 = CARTESIAN_POINT ( 'NONE',  ( 76.08054936894747300, 60.44165029396862820, 15.72172349425854065 ) ) ;
#34459 = CARTESIAN_POINT ( 'NONE',  ( 174.3675516979637905, 254.9025437404973218, 8.247627981828351551 ) ) ;
#34460 = CARTESIAN_POINT ( 'NONE',  ( 13.42817895373461390, 26.49103043416548076, -8.090169943749479842 ) ) ;
#34461 = VERTEX_POINT ( 'NONE', #80509 ) ;
#34462 = CARTESIAN_POINT ( 'NONE',  ( 71.96639307748559133, 71.49757472301891426, -5.734781593071442529 ) ) ;
#34463 = CARTESIAN_POINT ( 'NONE',  ( 151.4159295687746294, 268.3869122420484814, 14.78076517566594106 ) ) ;
#34464 = CARTESIAN_POINT ( 'NONE',  ( 177.3812267363185242, 255.8896424273514469, -7.004123935190221140 ) ) ;
#34465 = CARTESIAN_POINT ( 'NONE',  ( 74.73869185334548604, 64.10010416581232562, -14.66605532835945880 ) ) ;
#34466 = VERTEX_POINT ( 'NONE', #87140 ) ;
#34467 = ORIENTED_EDGE ( 'NONE', *, *, #77413, .F. ) ;
#34468 = CARTESIAN_POINT ( 'NONE',  ( 161.8839333999304415, 250.2557977526613229, -13.90128376743482441 ) ) ;
#34469 = CARTESIAN_POINT ( 'NONE',  ( 196.2379679265050925, 290.7528645076583871, -16.93678934971137906 ) ) ;
#34470 = EDGE_LOOP ( 'NONE', ( #79875, #88633 ) ) ;
#34471 = CARTESIAN_POINT ( 'NONE',  ( 66.17812102814201580, 68.61244640036318287, -2.189447319278969406 ) ) ;
#34472 = LINE ( 'NONE', #27869, #82030 ) ;
#34473 = CARTESIAN_POINT ( 'NONE',  ( 189.0689802957956260, 269.8288687927027354, -15.50864081522695415 ) ) ;
#34474 = CARTESIAN_POINT ( 'NONE',  ( 78.08890065365325484, 61.45839965263433413, -16.15943835942215756 ) ) ;
#34475 = EDGE_CURVE ( 'NONE', #33229, #26719, #25258, .T. ) ;
#34476 = CARTESIAN_POINT ( 'NONE',  ( 157.2777284163744582, 258.2339788142568864, -16.82360006463426316 ) ) ;
#34477 = CARTESIAN_POINT ( 'NONE',  ( 118.9295641673753181, 227.2202760586659736, -5.415160957724236172E-17 ) ) ;
#34478 = DIRECTION ( 'NONE',  ( 0.000000000000000000, 0.000000000000000000, 1.000000000000000000 ) ) ;
#34479 = ORIENTED_EDGE ( 'NONE', *, *, #34139, .T. ) ;
#34480 = CARTESIAN_POINT ( 'NONE',  ( 164.4817765375028102, 245.7562014482918755, -6.334578229142199035 ) ) ;
#34481 = EDGE_LOOP ( 'NONE', ( #34364, #32083, #27297, #96451 ) ) ;
#34482 = CARTESIAN_POINT ( 'NONE',  ( 38.16387531507685793, 24.96004757982092315, -5.678558825948276656 ) ) ;
#34483 = CARTESIAN_POINT ( 'NONE',  ( 198.4264492142971221, 286.9623037257889564, 17.00126466006521397 ) ) ;
#34484 = CARTESIAN_POINT ( 'NONE',  ( 71.67687952550437558, 206.0643266524160424, 9.188101187500095079 ) ) ;
#34485 = CARTESIAN_POINT ( 'NONE',  ( -31.59167490957833735, 96.33871916006887659, 12.21808272424466502 ) ) ;
#34486 = CARTESIAN_POINT ( 'NONE',  ( 105.0000000000000000, 0.000000000000000000, 14.21260523776213347 ) ) ;
#34487 = CARTESIAN_POINT ( 'NONE',  ( 204.1541407990405332, 272.6956988606675623, 11.22829397770025395 ) ) ;
#34489 = B_SPLINE_CURVE_WITH_KNOTS ( 'NONE', 3,
 ( #56709, #17204, #2018, #86177 ),
 .UNSPECIFIED., .F., .F.,
 ( 4, 4 ),
 ( 0.01333939463499779488, 0.01972261937988741692 ),
 .UNSPECIFIED. ) ;
#34488 = CARTESIAN_POINT ( 'NONE',  ( 175.6230877040034102, 278.4164368346121137, 15.50752949055044638 ) ) ;
#34490 = VERTEX_POINT ( 'NONE', #88129 ) ;
#34491 =( BOUNDED_CURVE ( )  B_SPLINE_CURVE ( 2, ( #54082, #64199, #41386, #80957, #2932, #65686, #4393, #66200, #27711 ),
 .UNSPECIFIED., .F., .T. ) 
 B_SPLINE_CURVE_WITH_KNOTS ( ( 3, 2, 2, 2, 3 ),
 ( 0.9637096774193548709, 0.9650537634408602461, 0.9677419354838709964, 0.9704301075268817467, 0.9717741935483871218 ),
 .UNSPECIFIED. ) 
 CURVE ( )  GEOMETRIC_REPRESENTATION_ITEM ( )  RATIONAL_B_SPLINE_CURVE ( ( 0.9330127018922194093, 0.9330127018922194093, 1.000000000000000000, 0.8660254037844387076, 1.000000000000000000, 0.8660254037844387076, 1.000000000000000000, 0.9330127018922194093, 0.9330127018922194093 ) ) 
 REPRESENTATION_ITEM ( '' )  );
#34492 = CARTESIAN_POINT ( 'NONE',  ( 181.4632975752175525, 255.1188003790442167, 1.936479460681336695 ) ) ;
#34493 = CARTESIAN_POINT ( 'NONE',  ( 155.5322964227545413, 261.2571557083629159, -18.35853982030605280 ) ) ;
#34494 = ORIENTED_EDGE ( 'NONE', *, *, #51324, .F. ) ;
#34495 = CARTESIAN_POINT ( 'NONE',  ( 72.19109158906036328, 71.10838548458626462, -5.953967166465967686 ) ) ;
#34496 = CARTESIAN_POINT ( 'NONE',  ( 173.9756991879395116, 277.8259260648333679, -15.76639585222196516 ) ) ;
#34497 = CARTESIAN_POINT ( 'NONE',  ( 162.8741883755088509, 259.8356047474810566, -16.24831708344704850 ) ) ;
#34498 = CARTESIAN_POINT ( 'NONE',  ( 84.14312167556933275, 48.98415679381830756, 0.000000000000000000 ) ) ;
#34499 = EDGE_CURVE ( 'NONE', #69721, #52564, #63764, .T. ) ;
#34500 = DIRECTION ( 'NONE',  ( 1.000000000000000000, 0.000000000000000000, 0.000000000000000000 ) ) ;
#34501 = CARTESIAN_POINT ( 'NONE',  ( 164.2545401858843945, 246.1497863546213978, 2.275217130759496609 ) ) ;
#34502 = CARTESIAN_POINT ( 'NONE',  ( 164.9617201910520237, 244.9249146555742414, 2.745022583679548767 ) ) ;
#34503 = DIRECTION ( 'NONE',  ( -0.000000000000000000, 0.000000000000000000, 1.000000000000000000 ) ) ;
#34504 = CARTESIAN_POINT ( 'NONE',  ( 167.3715206515632872, 256.4254025383586963, 13.71134816071423757 ) ) ;
#34505 = ORIENTED_EDGE ( 'NONE', *, *, #25170, .F. ) ;
#34506 = CARTESIAN_POINT ( 'NONE',  ( 1.094572704733512092, 182.9860189848785410, -2.679491924311240503 ) ) ;
#34507 = CARTESIAN_POINT ( 'NONE',  ( 129.7005815790617760, 239.5643266524159856, -9.188101187500093303 ) ) ;
#34508 = ORIENTED_EDGE ( 'NONE', *, *, #84930, .F. ) ;
#34509 = CARTESIAN_POINT ( 'NONE',  ( 146.6138605399200117, 276.7043397814778132, -0.5394499176159462950 ) ) ;
#34510 = PLANE ( 'NONE',  #30298 ) ;
#34511 = VECTOR ( 'NONE', #91279, 1000.000000000000227 ) ;
#34512 = CARTESIAN_POINT ( 'NONE',  ( 199.0532324483041009, 282.6079911291746498, -17.61480581509741583 ) ) ;
#34513 = EDGE_CURVE ( 'NONE', #11813, #7544, #5739, .T. ) ;
#34514 = CARTESIAN_POINT ( 'NONE',  ( 164.4864504671816690, 245.7481059646165704, 6.337356894698421783 ) ) ;
#34515 = ADVANCED_FACE ( 'NONE', ( #18170 ), #18675, .F. ) ;
#34516 = CARTESIAN_POINT ( 'NONE',  ( 74.14611568627913130, 58.01609043150301659, 15.90920405299479157 ) ) ;
#34517 = CARTESIAN_POINT ( 'NONE',  ( 49.17298586869600285, 105.8308522718264584, 177.5919119679930134 ) ) ;
#34518 = ORIENTED_EDGE ( 'NONE', *, *, #5142, .T. ) ;
#34519 = CARTESIAN_POINT ( 'NONE',  ( 80.26984573713558291, 57.41310870600725025, -16.58958131739138508 ) ) ;
#34520 = ADVANCED_FACE ( 'NONE', ( #49072 ), #56141, .F. ) ;
#34521 = DIRECTION ( 'NONE',  ( 0.1548189829846108034, -0.9879428538673736826, 0.000000000000000000 ) ) ;
#34522 = CARTESIAN_POINT ( 'NONE',  ( 42.65610334793077385, 64.00004027534475881, -10.00000000000000000 ) ) ;
#34523 = CARTESIAN_POINT ( 'NONE',  ( 206.7127649687076314, 272.6099838315917623, -10.35326570309970506 ) ) ;
#34524 = CARTESIAN_POINT ( 'NONE',  ( 140.0925393287100178, 257.8149278399160949, -9.188101187500095079 ) ) ;
#34525 = AXIS2_PLACEMENT_3D ( 'NONE', #15888, #30605, #47779 ) ;
#34526 = CARTESIAN_POINT ( 'NONE',  ( 190.0370014622527322, 286.8089957100377205, 16.96978714573610247 ) ) ;
#34527 = CARTESIAN_POINT ( 'NONE',  ( 13.75631770279070842, 31.55236904046465440, 177.5919119679930134 ) ) ;
#34528 = CARTESIAN_POINT ( 'NONE',  ( 170.6852122113414225, 250.4783651670598488, 3.454835134718858392 ) ) ;
#34529 = CARTESIAN_POINT ( 'NONE',  ( 14.87430715154758687, 30.36126292948894800, 6.180339887498949913 ) ) ;
#34530 = CARTESIAN_POINT ( 'NONE',  ( 190.4163244163388242, 300.8362468508201459, 4.691083071570470331 ) ) ;
#34531 = PLANE ( 'NONE',  #93619 ) ;
#34532 = CARTESIAN_POINT ( 'NONE',  ( 172.4392911513491242, 287.3831240604444588, -8.176537520936799197 ) ) ;
#34533 = B_SPLINE_CURVE_WITH_KNOTS ( 'NONE', 3,
 ( #55765, #31481, #14795, #45677, #76603, #88259, #33503, #88757, #32990, #49210, #79142, #18311, #11711, #71518, #48712, #18807, #10209, #25394, #26407, #42088, #40578, #80142, #2108, #87773, #64398, #94830, #95362, #72525, #3613, #56788, #63893, #73020, #56281, #10707, #87280, #49689, #26903, #86757, #17291, #27405, #57285, #80644, #11222, #17811, #42573, #79643 ),
 .UNSPECIFIED., .F., .F.,
 ( 4, 1, 1, 1, 2, 2, 1, 1, 1, 2, 2, 1, 1, 2, 2, 1, 1, 2, 2, 1, 1, 2, 2, 1, 2, 2, 1, 2, 2, 4 ),
 ( 0.000000000000000000, 0.06249999999998676059, 0.09374999999998205602, 0.1093749999999796968, 0.1171874999999787531, 0.1249999999999777955, 0.1874999999999881206, 0.2187499999999913958, 0.2343749999999911460, 0.2421874999999893974, 0.2499999999999876210, 0.3124999999999739098, 0.3437499999999689138, 0.3593749999999641953, 0.3749999999999594213, 0.4374999999999457656, 0.4687499999999393263, 0.4843749999999361622, 0.4999999999999329425, 0.5624999999999296119, 0.5937499999999259481, 0.6093749999999263922, 0.6249999999999268363, 0.6874999999999357181, 0.7187499999999398259, 0.7499999999999438227, 0.8124999999999519273, 0.8437499999999579225, 0.8749999999999639178, 1.000000000000000000 ),
 .UNSPECIFIED. ) ;
#34534 = CARTESIAN_POINT ( 'NONE',  ( 48.91560817564824504, 80.00000000000000000, -10.00000000000000178 ) ) ;
#34535 = CARTESIAN_POINT ( 'NONE',  ( 193.5083605049795210, 288.6373469989542855, 16.03391007790886391 ) ) ;
#34536 = ADVANCED_FACE ( 'NONE', ( #65259 ), #79510, .F. ) ;
#34537 = CARTESIAN_POINT ( 'NONE',  ( 136.3309150271299757, 239.5177522451417929, 5.000000000000051514 ) ) ;
#34538 = CARTESIAN_POINT ( 'NONE',  ( 173.4505375608857491, 284.9503170016366198, -13.05978560202663452 ) ) ;
#34539 = ORIENTED_EDGE ( 'NONE', *, *, #91745, .F. ) ;
#34540 = CARTESIAN_POINT ( 'NONE',  ( 196.4677102463732012, 290.3549391369982686, 16.45225250689336249 ) ) ;
#34541 = CARTESIAN_POINT ( 'NONE',  ( 190.5444288681022442, 300.6143634316900943, -1.000014190476072873 ) ) ;
#34542 = CARTESIAN_POINT ( 'NONE',  ( -1.394013918807642360, 163.8768266524159856, 9.188101187500096856 ) ) ;
#34543 = CARTESIAN_POINT ( 'NONE',  ( 35.81758128034870481, 200.6744531367911293, 4.594050593750047540 ) ) ;
#34544 = CARTESIAN_POINT ( 'NONE',  ( 178.4336282224923309, 273.6370629074921226, -17.24514701715171228 ) ) ;
#34545 = CARTESIAN_POINT ( 'NONE',  ( 21.91939736263385541, 14.78380873178786636, -6.180339887498949025 ) ) ;
#34546 = CARTESIAN_POINT ( 'NONE',  ( 188.0775634319173832, 267.1413101313072502, 14.31780989748781252 ) ) ;
#34547 = CARTESIAN_POINT ( 'NONE',  ( 69.03518170984699509, 64.49507618471645287, 12.45339560606362461 ) ) ;
#34548 = CARTESIAN_POINT ( 'NONE',  ( 72.08021828965947009, 72.40975849880194914, -3.082927075499598324 ) ) ;
#34549 = CARTESIAN_POINT ( 'NONE',  ( 146.7845206192450007, 276.4087478532630939, 4.443586170796542945 ) ) ;
#34550 = CARTESIAN_POINT ( 'NONE',  ( 73.83283565865448850, 55.23351700259583197, -16.12091336794239638 ) ) ;
#34552 = CARTESIAN_POINT ( 'NONE',  ( 73.03889176721723686, 199.6427522451417644, 1.119607411625061291E-15 ) ) ;
#34551 = CARTESIAN_POINT ( 'NONE',  ( 163.2942584940569191, 258.1478583562382028, 16.77787020301746779 ) ) ;
#34553 = CARTESIAN_POINT ( 'NONE',  ( 74.58922631747108767, 66.95469429158355013, 12.55546573254311937 ) ) ;
#34554 = CARTESIAN_POINT ( 'NONE',  ( 23.75126848931443746, 37.21091486745861943, 7.012934429366973338E-14 ) ) ;
#34555 = FACE_OUTER_BOUND ( 'NONE', #22119, .T. ) ;
#34556 = CARTESIAN_POINT ( 'NONE',  ( 181.1541159318895211, 294.6564104570541645, 1.018405793603249565 ) ) ;
#34557 = CARTESIAN_POINT ( 'NONE',  ( 51.26196130476894552, 193.7365022471901739, -10.00000000000009059 ) ) ;
#34558 = CARTESIAN_POINT ( 'NONE',  ( 57.60966550219797000, 179.2419560658249225, 17.47570218321535407 ) ) ;
#34559 = CARTESIAN_POINT ( 'NONE',  ( 149.7701467413202749, 271.6257199327137073, -11.62364177631229190 ) ) ;
#34560 = CARTESIAN_POINT ( 'NONE',  ( -4.533703103291247594, 174.3149278399161233, 9.188101187500093303 ) ) ;
#34561 = CARTESIAN_POINT ( 'NONE',  ( 39.87427548755113804, 25.94754757982092741, 5.678558825948272215 ) ) ;
#34562 = DIRECTION ( 'NONE',  ( -0.8660254037844387076, -0.4999999999999998890, -0.000000000000000000 ) ) ;
#34563 = CARTESIAN_POINT ( 'NONE',  ( 192.0712386031329686, 297.9698513971258649, 12.12276320360788873 ) ) ;
#34564 = CARTESIAN_POINT ( 'NONE',  ( 40.97001837269192492, 24.44966523072497822, -2.296566073217252530E-15 ) ) ;
#34565 = CARTESIAN_POINT ( 'NONE',  ( 26.76913962382671386, 17.58380873178787951, 6.180339887498953466 ) ) ;
#34566 = CARTESIAN_POINT ( 'NONE',  ( 180.0205270375271880, 277.0212420910811488, 16.30529632528782358 ) ) ;
#34567 = CARTESIAN_POINT ( 'NONE',  ( 193.7706395672514645, 295.0264025848412075, 15.16938698680137065 ) ) ;
#34568 = CARTESIAN_POINT ( 'NONE',  ( 76.20885775532401851, 203.2592609112379876, 2.679491924311254714 ) ) ;
#34569 = CARTESIAN_POINT ( 'NONE',  ( 179.7261617362159427, 262.7909812490211152, -12.86163648858739172 ) ) ;
#34570 = EDGE_CURVE ( 'NONE', #81007, #72976, #85569, .T. ) ;
#34571 = CARTESIAN_POINT ( 'NONE',  ( 14.66449673273962340, 9.262165230724928477, -2.296566073217252530E-15 ) ) ;
#34572 = CARTESIAN_POINT ( 'NONE',  ( 71.97141114645216931, 72.59821799906345063, 1.534520970786794836 ) ) ;
#34573 = CARTESIAN_POINT ( 'NONE',  ( 20.18540868186541459, 12.44966523072493914, -2.296566073217252530E-15 ) ) ;
#34574 = CIRCLE ( 'NONE', #60362, 16.10714546451156082 ) ;
#34575 = CARTESIAN_POINT ( 'NONE',  ( 153.1318494048608159, 277.9249485213736079, -4.812811992226706082 ) ) ;
#34576 = ORIENTED_EDGE ( 'NONE', *, *, #10692, .T. ) ;
#34577 = CARTESIAN_POINT ( 'NONE',  ( 156.9230943565391669, 276.4044123300005822, 10.58617205435853315 ) ) ;
#34578 = CARTESIAN_POINT ( 'NONE',  ( 206.3423291502491566, 273.2515974901050413, -10.76717883871977577 ) ) ;
#34579 = EDGE_LOOP ( 'NONE', ( #26031, #6327, #78343, #70844 ) ) ;
#34580 = CARTESIAN_POINT ( 'NONE',  ( -110.0000000000000142, 15.00000000000000000, -9.212605237762117483 ) ) ;
#34581 = CARTESIAN_POINT ( 'NONE',  ( 207.0200405408487541, 272.0777669287182334, 6.494273599193515878 ) ) ;
#34582 = CARTESIAN_POINT ( 'NONE',  ( 29.46552898026456546, 17.41603393254326093, -1.583844403245362020 ) ) ;
#34583 = CARTESIAN_POINT ( 'NONE',  ( 87.83187315495058556, 45.09740525803774602, 6.666720864128770074 ) ) ;
#34584 = EDGE_LOOP ( 'NONE', ( #46690, #51284, #42789, #71907, #55603 ) ) ;
#34585 = EDGE_LOOP ( 'NONE', ( #93818, #4464, #75491, #82315, #15870 ) ) ;
#34587 = FACE_OUTER_BOUND ( 'NONE', #64214, .T. ) ;
#34586 = CARTESIAN_POINT ( 'NONE',  ( 159.7567037358847699, 278.4970363524427626, -9.767935059668046094 ) ) ;
#34588 = VECTOR ( 'NONE', #4268, 1000.000000000000227 ) ;
#34589 = CARTESIAN_POINT ( 'NONE',  ( 192.1640094933931096, 297.8091675017319062, 12.36911124822534447 ) ) ;
#34590 = ORIENTED_EDGE ( 'NONE', *, *, #36828, .T. ) ;
#34591 = CARTESIAN_POINT ( 'NONE',  ( 76.62142590937760644, 52.12176499430435683, 15.74697333657635134 ) ) ;
#34592 = CARTESIAN_POINT ( 'NONE',  ( 178.2850679595637473, 263.9267319943502912, 15.11778687281824141 ) ) ;
#34593 = EDGE_LOOP ( 'NONE', ( #83458, #96676, #24165, #72659 ) ) ;
#34594 = CARTESIAN_POINT ( 'NONE',  ( -16.76269525828470464, 104.2312461070085021, 36.50000000000000000 ) ) ;
#34595 = CARTESIAN_POINT ( 'NONE',  ( 77.61054570139664577, 50.60100434898155441, -15.24042138154272763 ) ) ;
#34596 = CARTESIAN_POINT ( 'NONE',  ( 196.8363552541316324, 289.7164272536036265, -17.80258609350122967 ) ) ;
#34597 = CARTESIAN_POINT ( 'NONE',  ( 36.66582480827072743, 198.6427522451419350, -10.00000000000009592 ) ) ;
#34598 = ORIENTED_EDGE ( 'NONE', *, *, #80546, .F. ) ;
#34599 = CARTESIAN_POINT ( 'NONE',  ( 200.8828793852583203, 282.7076418644388696, 17.90302398138411633 ) ) ;
#34600 = CARTESIAN_POINT ( 'NONE',  ( 166.1395527380942667, 274.1522324139922944, -15.18991220291641575 ) ) ;
#34601 = DIRECTION ( 'NONE',  ( -0.8660254037844387076, -0.4999999999999998890, -0.000000000000000000 ) ) ;
#34602 = B_SPLINE_SURFACE_WITH_KNOTS ( 'NONE', 3, 1, ( 
 ( #46787, #77707 ),
 ( #8292, #70071 ),
 ( #686, #33596 ),
 ( #65481, #26497 ),
 ( #94925, #55854 ),
 ( #88349, #18908 ),
 ( #11317, #10295 ),
 ( #11805, #49784 ),
 ( #88856, #35074 ),
 ( #19422, #95452 ),
 ( #71608, #34103 ),
 ( #41168, #4175 ),
 ( #42661, #26992 ),
 ( #65980, #80745 ),
 ( #42175, #73595 ),
 ( #87375, #72105 ),
 ( #73110, #96933 ),
 ( #95938, #50277 ),
 ( #81230, #72617 ),
 ( #3703, #57878 ),
 ( #34581, #57376 ),
 ( #96428, #56874 ),
 ( #86849, #2708 ),
 ( #10800, #64491 ),
 ( #17382, #48293 ),
 ( #17904, #79239 ),
 ( #9811, #40671 ),
 ( #2205, #49293 ),
 ( #33086, #64995 ),
 ( #63982, #25486 ),
 ( #80232, #56377 ),
 ( #48801, #79734 ),
 ( #26004, #87858 ),
 ( #18401, #41673 ) ),
 .UNSPECIFIED., .T., .F., .F.,
 ( 4, 2, 2, 2, 2, 2, 2, 2, 2, 2, 2, 2, 2, 2, 2, 2, 4 ),
 ( 2, 2 ),
 ( 0.000000000000000000, 0.06250000000000000000, 0.1250000000000000000, 0.1875000000000000000, 0.2500000000000000000, 0.3125000000000000000, 0.3750000000000000000, 0.4375000000000000000, 0.5000000000000000000, 0.5625000000000000000, 0.6250000000000000000, 0.6875000000000000000, 0.7500000000000000000, 0.8125000000000000000, 0.8750000000000000000, 0.9375000000000000000, 1.000000000000000000 ),
 ( 0.000000000000000000, 1.000000000000000000 ),
 .UNSPECIFIED. ) ;
#34603 = ORIENTED_EDGE ( 'NONE', *, *, #38874, .T. ) ;
#34604 = CARTESIAN_POINT ( 'NONE',  ( 174.4470096775725096, 277.0272586029935269, -17.07083632119895356 ) ) ;
#34605 = DIRECTION ( 'NONE',  ( 0.000000000000000000, 0.000000000000000000, 1.000000000000000000 ) ) ;
#34606 = ORIENTED_EDGE ( 'NONE', *, *, #6611, .F. ) ;
#34607 = CARTESIAN_POINT ( 'NONE',  ( 156.7672756052014620, 266.5620104575966138, -16.23688817329552236 ) ) ;
#34608 = EDGE_LOOP ( 'NONE', ( #48573, #45785, #20387, #62580 ) ) ;
#34609 = CARTESIAN_POINT ( 'NONE',  ( -22.42236680055709641, 157.8615022471902591, 0.000000000000000000 ) ) ;
#34610 = EDGE_LOOP ( 'NONE', ( #21302, #56113, #46689 ) ) ;
#34611 = CARTESIAN_POINT ( 'NONE',  ( 159.2149555070472786, 259.5139964546949614, 16.68861687308905317 ) ) ;
#34612 = CARTESIAN_POINT ( 'NONE',  ( 147.8749077915786643, 274.5201418708599022, 7.075400916280408126 ) ) ;
#34613 = CARTESIAN_POINT ( 'NONE',  ( 180.2491029045606012, 291.6074392935250899, -9.950551294970233940 ) ) ;
#34614 = CARTESIAN_POINT ( 'NONE',  ( 70.06962527880796188, 66.55497806833156460, 10.52730242420649631 ) ) ;
#34615 = CARTESIAN_POINT ( 'NONE',  ( -44.67997007436067491, 47.78987728549608960, 59.99999999999999289 ) ) ;
#34616 = CARTESIAN_POINT ( 'NONE',  ( 176.9554221106268130, 290.7336789374555792, 6.091561936831863200 ) ) ;
#34617 = CARTESIAN_POINT ( 'NONE',  ( 197.1275133052921262, 289.2121267159609488, -18.14557307217323867 ) ) ;
#34618 = VERTEX_POINT ( 'NONE', #78997 ) ;
#34619 = CARTESIAN_POINT ( 'NONE',  ( 99.16399144804778132, 221.3927522451417929, -10.00000000000009237 ) ) ;
#34620 = CARTESIAN_POINT ( 'NONE',  ( 27.26159103020561147, 24.24335787977764767, -9.188101187500008038 ) ) ;
#34621 = CARTESIAN_POINT ( 'NONE',  ( 164.9103019330012216, 245.0139736909548560, 2.841678961959298810 ) ) ;
#34622 = CARTESIAN_POINT ( 'NONE',  ( 205.7639495959071212, 274.2533802642843170, 10.79039487422292432 ) ) ;
#34624 = EDGE_LOOP ( 'NONE', ( #20276, #86415, #99647, #59263 ) ) ;
#34623 = CARTESIAN_POINT ( 'NONE',  ( 160.0072461633487535, 253.5063153963366744, 16.23938890643736244 ) ) ;
#34625 = ORIENTED_EDGE ( 'NONE', *, *, #72061, .F. ) ;
#34626 = CARTESIAN_POINT ( 'NONE',  ( 187.6615196811425221, 277.1468961788498859, 17.16910232051792917 ) ) ;
#34627 = CARTESIAN_POINT ( 'NONE',  ( 69.71681968175923316, 62.66721131071562212, 13.91613743701406491 ) ) ;
#34628 = CARTESIAN_POINT ( 'NONE',  ( 164.2507602871578740, 247.8507055370842806, 8.654211643685846056 ) ) ;
#34629 = CARTESIAN_POINT ( 'NONE',  ( 18.87072174683323666, 11.86426979415088745, -3.090169943749474069 ) ) ;
#34630 = EDGE_CURVE ( 'NONE', #17546, #2384, #14182, .T. ) ;
#34631 = CARTESIAN_POINT ( 'NONE',  ( 198.6786699363856314, 286.5254446204100418, -18.23156697103042845 ) ) ;
#34632 = EDGE_CURVE ( 'NONE', #98268, #91064, #69310, .T. ) ;
#34633 = CARTESIAN_POINT ( 'NONE',  ( 189.9718059322956094, 301.6061754500863117, -1.293200095882213185 ) ) ;
#34634 = ORIENTED_EDGE ( 'NONE', *, *, #97626, .F. ) ;
#34635 = DIRECTION ( 'NONE',  ( -0.9413434404457865501, 0.3374500364938337049, 0.000000000000000000 ) ) ;
#34636 = DIRECTION ( 'NONE',  ( -0.9263643838751194348, -0.3766285016932073293, 0.000000000000000000 ) ) ;
#34637 = EDGE_CURVE ( 'NONE', #17528, #9585, #4456, .T. ) ;
#34638 = DIRECTION ( 'NONE',  ( 0.4999999999999992784, -0.8660254037844390407, 0.000000000000000000 ) ) ;
#34639 = EDGE_CURVE ( 'NONE', #20627, #7148, #50545, .T. ) ;
#34640 = CARTESIAN_POINT ( 'NONE',  ( 28.87159617421078295, 194.1427522451419350, -10.00000000000009415 ) ) ;
#34641 = CARTESIAN_POINT ( 'NONE',  ( 96.79126913948809374, 232.8149278399160949, 9.188101187500093303 ) ) ;
#34642 = CARTESIAN_POINT ( 'NONE',  ( 184.0204834781850423, 296.8556583875038086, -2.767185464358945524 ) ) ;
#34643 = CARTESIAN_POINT ( 'NONE',  ( 167.9076177050584704, 282.0442412872837394, -10.81069426134948763 ) ) ;
#34644 = CARTESIAN_POINT ( 'NONE',  ( 17.60357497223980516, 35.28838536716092023, -10.00000000000000000 ) ) ;
#34645 = DIRECTION ( 'NONE',  ( 0.000000000000000000, 0.000000000000000000, -1.000000000000000000 ) ) ;
#34646 = CARTESIAN_POINT ( 'NONE',  ( 21.36630299834339652, 173.9548013555409796, -4.594050593750042211 ) ) ;
#34647 = DIRECTION ( 'NONE',  ( 0.7490285521785712275, -0.6625377181876315191, 0.000000000000000000 ) ) ;
#34648 = VERTEX_POINT ( 'NONE', #28756 ) ;
#34649 = ORIENTED_EDGE ( 'NONE', *, *, #53380, .F. ) ;
#34650 = CARTESIAN_POINT ( 'NONE',  ( 185.6371458920492614, 259.0387137507489115, -5.368070696299057865 ) ) ;
#34651 = CARTESIAN_POINT ( 'NONE',  ( 79.58119954245727001, 47.14750477878121160, -13.19237880149493769 ) ) ;
#34652 = CARTESIAN_POINT ( 'NONE',  ( 193.1296824374275047, 263.5099161404405095, -3.843190626297300572 ) ) ;
#34653 = B_SPLINE_CURVE_WITH_KNOTS ( 'NONE', 3,
 ( #96464, #57408, #80779, #73627, #80268, #27030, #87411 ),
 .UNSPECIFIED., .F., .F.,
 ( 4, 3, 4 ),
 ( 0.001258777641685644277, 0.001498048468333237297, 0.002225082062310303373 ),
 .UNSPECIFIED. ) ;
#34654 = AXIS2_PLACEMENT_3D ( 'NONE', #59163, #90137, #20711 ) ;
#34655 = CARTESIAN_POINT ( 'NONE',  ( 161.8153478334749877, 250.3745914384277285, -14.21120979595050215 ) ) ;
#34656 = CARTESIAN_POINT ( 'NONE',  ( 22.66956910419568061, 38.88013629349136835, -10.00000000000000000 ) ) ;
#34657 = CARTESIAN_POINT ( 'NONE',  ( 74.17426598413138095, 67.86558882176393581, -11.66684587328573031 ) ) ;
#34658 = CARTESIAN_POINT ( 'NONE',  ( 40.58072100116311276, 203.4244531367911293, -4.594050593750046652 ) ) ;
#34659 = CARTESIAN_POINT ( 'NONE',  ( 93.02964483790795214, 234.5177522451419350, 5.000000000000046185 ) ) ;
#34660 = VERTEX_POINT ( 'NONE', #50062 ) ;
#34661 = CARTESIAN_POINT ( 'NONE',  ( 79.04869528564928771, 60.22382082520469737, -16.44980649040590492 ) ) ;
#34662 = VECTOR ( 'NONE', #56131, 1000.000000000000000 ) ;
#34663 = FACE_OUTER_BOUND ( 'NONE', #34344, .T. ) ;
#34664 = CARTESIAN_POINT ( 'NONE',  ( 4.614210867829412699, 161.2202760586659451, -5.415160957724236172E-17 ) ) ;
#34665 = CARTESIAN_POINT ( 'NONE',  ( 68.60506951895222016, 64.61196645306745268, -12.16704851705999957 ) ) ;
#34666 = CARTESIAN_POINT ( 'NONE',  ( 198.7829547491859330, 286.3448180261817129, -18.59838968157616179 ) ) ;
#34667 = CARTESIAN_POINT ( 'NONE',  ( 80.77040970686135779, 52.39315937341162055, 15.73168746087837810 ) ) ;
#34668 = CARTESIAN_POINT ( 'NONE',  ( 147.4323331177958494, 275.2867036919951147, -5.064030047414062707 ) ) ;
#34669 = LINE ( 'NONE', #33180, #10136 ) ;
#34670 = CARTESIAN_POINT ( 'NONE',  ( 164.3330377059402849, 246.0138246616164110, 7.208046019122525294 ) ) ;
#34671 = CARTESIAN_POINT ( 'NONE',  ( 78.92295937046175425, 204.8262482093457777, 3.021315404115420679E-15 ) ) ;
#34672 = CARTESIAN_POINT ( 'NONE',  ( 147.6121581866023007, 274.9752375363476631, 8.700660424766859080 ) ) ;
#34673 = VERTEX_POINT ( 'NONE', #27270 ) ;
#34674 = CARTESIAN_POINT ( 'NONE',  ( 164.3053959849042087, 246.0617015268593661, -7.251939739328854273 ) ) ;
#34675 = CARTESIAN_POINT ( 'NONE',  ( 9.548404355818492562, 162.9865022471901455, 1.119607411625061291E-15 ) ) ;
#34676 = CARTESIAN_POINT ( 'NONE',  ( -40.42249077443059235, 27.53003111760058630, -10.00000000000000000 ) ) ;
#34677 = CARTESIAN_POINT ( 'NONE',  ( 116.3579438323015012, 247.1744531367911293, 4.594050593750047540 ) ) ;
#34678 = CARTESIAN_POINT ( 'NONE',  ( 16.80672687576512203, 25.10171378149917842, 9.188101187500008038 ) ) ;
#34679 = CARTESIAN_POINT ( 'NONE',  ( 75.28650001057752661, 66.67572118895705557, 13.44401380721711270 ) ) ;
#34680 = CARTESIAN_POINT ( 'NONE',  ( 48.98007068238331385, 88.97864505566217019, -10.00000000000000000 ) ) ;
#34682 = CARTESIAN_POINT ( 'NONE',  ( 190.1893769843902362, 293.1304489240072257, 14.15308602958251250 ) ) ;
#34681 = CARTESIAN_POINT ( 'NONE',  ( 170.3290958195750022, 289.6815776661216546, -1.151831906498994140 ) ) ;
#34683 = CARTESIAN_POINT ( 'NONE',  ( 15.34872451668155868, 24.56454794089041016, 10.00000000000000355 ) ) ;
#34684 = ORIENTED_EDGE ( 'NONE', *, *, #95076, .T. ) ;
#34685 = CARTESIAN_POINT ( 'NONE',  ( 151.2057546125658973, 268.7509459446807227, 15.78031848731319187 ) ) ;
#34686 = CARTESIAN_POINT ( 'NONE',  ( 207.7656302052884598, 270.7863677483104539, -0.3981791975740528455 ) ) ;
#34687 = EDGE_CURVE ( 'NONE', #57805, #73019, #80731, .T. ) ;
#34688 = CARTESIAN_POINT ( 'NONE',  ( 190.1578907173511084, 300.2574240630518148, 3.242419245672157224 ) ) ;
#34689 = CARTESIAN_POINT ( 'NONE',  ( 175.6461609673314115, 292.5563777142869526, -1.142818921673324439 ) ) ;
#34690 = CARTESIAN_POINT ( 'NONE',  ( 81.78242120570297402, 55.48469546634665761, -15.94821833579707437 ) ) ;
#34691 = ORIENTED_EDGE ( 'NONE', *, *, #78170, .F. ) ;
#34692 = DIRECTION ( 'NONE',  ( 0.1039558454088763267, -0.1800568059919503139, 0.9781476007338069101 ) ) ;
#34693 = CARTESIAN_POINT ( 'NONE',  ( 167.6360249118671106, 271.0525740842397795, -16.39345155401522192 ) ) ;
#34694 = CARTESIAN_POINT ( 'NONE',  ( 82.53715491520738112, 41.41892551179127935, 3.500865685413612205 ) ) ;
#34695 = CARTESIAN_POINT ( 'NONE',  ( 80.15082809947642772, 54.47608182991538683, 15.87478864171170123 ) ) ;
#34696 = CARTESIAN_POINT ( 'NONE',  ( 29.90546183718886653, 199.6199935810940929, 2.679491924311251605 ) ) ;
#34697 = DIRECTION ( 'NONE',  ( -0.8660254037844378194, -0.5000000000000013323, 0.000000000000000000 ) ) ;
#34698 = CARTESIAN_POINT ( 'NONE',  ( 148.5199441514828891, 273.7928082822475062, -8.166875775410368021 ) ) ;
#34699 = ORIENTED_EDGE ( 'NONE', *, *, #98556, .F. ) ;
#34700 = CARTESIAN_POINT ( 'NONE',  ( 194.0821437630113451, 282.7473781295547610, 17.16106363911004351 ) ) ;
#34701 = CARTESIAN_POINT ( 'NONE',  ( 4.150881819241740267, 21.13478043621385538, 8.090169943749478065 ) ) ;
#34702 = DIRECTION ( 'NONE',  ( -1.000000000000000000, 0.000000000000000000, 0.000000000000000000 ) ) ;
#34703 = ORIENTED_EDGE ( 'NONE', *, *, #24044, .T. ) ;
#34704 = FACE_OUTER_BOUND ( 'NONE', #32724, .T. ) ;
#34705 = EDGE_CURVE ( 'NONE', #62607, #98890, #57770, .T. ) ;
#34706 = CARTESIAN_POINT ( 'NONE',  ( 147.9311236323648870, 274.4227731784279172, -7.799459659034405412 ) ) ;
#34707 = DIRECTION ( 'NONE',  ( -0.9999986627203611977, 0.001635407438350361181, 0.000000000000000000 ) ) ;
#34708 = ORIENTED_EDGE ( 'NONE', *, *, #28573, .F. ) ;
#34709 = CARTESIAN_POINT ( 'NONE',  ( 78.89591602029014439, 59.68745106357756924, 16.49891905133565473 ) ) ;
#34710 = CARTESIAN_POINT ( 'NONE',  ( 205.6855624989150044, 273.4764227299817207, -9.799032349006141729 ) ) ;
#34711 = CARTESIAN_POINT ( 'NONE',  ( 75.15191903148871688, 52.97183600646508239, -16.48001256418180915 ) ) ;
#34713 = ORIENTED_EDGE ( 'NONE', *, *, #55837, .T. ) ;
#34712 = B_SPLINE_CURVE_WITH_KNOTS ( 'NONE', 3,
 ( #4264, #27084, #19981, #50858 ),
 .UNSPECIFIED., .F., .F.,
 ( 4, 4 ),
 ( 0.02920254411432028976, 0.03834810336565397382 ),
 .UNSPECIFIED. ) ;
#34714 = CARTESIAN_POINT ( 'NONE',  ( 95.92559083146868204, 220.0643266524159856, -9.188101187500093303 ) ) ;
#34715 = CARTESIAN_POINT ( 'NONE',  ( 82.76821771688562990, 50.44192209291004048, -14.09389759779402063 ) ) ;
#34716 = CARTESIAN_POINT ( 'NONE',  ( 73.46468938206548671, 69.84266834477836028, -9.805732075891272714 ) ) ;
#34717 = CARTESIAN_POINT ( 'NONE',  ( 84.65536491870415148, 49.91664468313385328, -13.65730316586987669 ) ) ;
#34718 = CARTESIAN_POINT ( 'NONE',  ( 181.8377039732492904, 257.3392381919999821, -6.047806239234591708 ) ) ;
#34719 = ORIENTED_EDGE ( 'NONE', *, *, #33173, .F. ) ;
#34720 = VERTEX_POINT ( 'NONE', #84487 ) ;
#34721 = CARTESIAN_POINT ( 'NONE',  ( 178.3028575937270261, 261.0369606096485882, 12.20229237870471195 ) ) ;
#34722 = ORIENTED_EDGE ( 'NONE', *, *, #22284, .F. ) ;
#34723 = DIRECTION ( 'NONE',  ( -0.7492053821869066876, -0.6623377501714446947, 0.000000000000000000 ) ) ;
#34724 = AXIS2_PLACEMENT_3D ( 'NONE', #87905, #58892, #42704 ) ;
#34725 = VERTEX_POINT ( 'NONE', #60623 ) ;
#34726 = CARTESIAN_POINT ( 'NONE',  ( 75.80447387303706819, 62.76703707744994887, 15.01739634675713830 ) ) ;
#34727 = CARTESIAN_POINT ( 'NONE',  ( 202.8151641853381477, 279.3608264160075692, -16.28741359973609448 ) ) ;
#34728 = ORIENTED_EDGE ( 'NONE', *, *, #1377, .T. ) ;
#34729 = CARTESIAN_POINT ( 'NONE',  ( 165.0278996183383811, 244.8102885250982865, 2.103256185480505636 ) ) ;
#34730 = CARTESIAN_POINT ( 'NONE',  ( 190.0146931831988013, 301.5318925525250506, 2.191471318341308372 ) ) ;
#34731 = CARTESIAN_POINT ( 'NONE',  ( 161.5320111222139019, 277.4805626463597719, -13.30372288155974836 ) ) ;
#34732 = CARTESIAN_POINT ( 'NONE',  ( 152.8651171364917900, 265.8768457450651113, -16.25664868183201861 ) ) ;
#34733 = FACE_OUTER_BOUND ( 'NONE', #62075, .T. ) ;
#34734 = DIRECTION ( 'NONE',  ( -0.5000000000000005551, 0.8660254037844384856, 0.000000000000000000 ) ) ;
#34735 = CARTESIAN_POINT ( 'NONE',  ( 139.7681268980558968, 245.3768266524160140, -9.188101187500091527 ) ) ;
#34736 = CARTESIAN_POINT ( 'NONE',  ( 75.66673835297086725, 54.72918191672597743, 16.12085908788240474 ) ) ;
#34737 = B_SPLINE_CURVE_WITH_KNOTS ( 'NONE', 3,
 ( #24475, #93417, #1185, #32580 ),
 .UNSPECIFIED., .F., .F.,
 ( 4, 4 ),
 ( 0.01376870305819338433, 0.02013848192403042137 ),
 .UNSPECIFIED. ) ;
#34738 = CARTESIAN_POINT ( 'NONE',  ( 10.59299460361177125, 21.51421378149917274, -9.188101187500004485 ) ) ;
#34739 = VERTEX_POINT ( 'NONE', #77861 ) ;
#34741 = ORIENTED_EDGE ( 'NONE', *, *, #47664, .F. ) ;
#34740 = CARTESIAN_POINT ( 'NONE',  ( 204.0604753336787667, 271.4817813032398703, 9.862283393711939183 ) ) ;
#34742 = EDGE_CURVE ( 'NONE', #2437, #85768, #55235, .T. ) ;
#34743 = CARTESIAN_POINT ( 'NONE',  ( 2.001305964997000864, 160.4155109091896065, 2.679491924311254714 ) ) ;
#34744 = CARTESIAN_POINT ( 'NONE',  ( 76.04051017601332774, 65.42867741054584485, -13.97686685444981336 ) ) ;
#34745 = CARTESIAN_POINT ( 'NONE',  ( 156.5891564345135691, 279.5636921043310394, 7.514476345455489259 ) ) ;
#34746 = CARTESIAN_POINT ( 'NONE',  ( 164.4854433269806577, 246.2060377238486808, -1.879056492287135116 ) ) ;
#34747 = CARTESIAN_POINT ( 'NONE',  ( 174.8813198920379648, 282.2092175607240279, 14.35867413939171122 ) ) ;
#34748 = CARTESIAN_POINT ( 'NONE',  ( 86.90457605785044848, 44.29542909698827202, 4.965724379175460612 ) ) ;
#34749 = CARTESIAN_POINT ( 'NONE',  ( 88.44601041138486153, 44.07807065378580802, -2.614235559790803798 ) ) ;
#34750 = VERTEX_POINT ( 'NONE', #8943 ) ;
#34751 = CARTESIAN_POINT ( 'NONE',  ( -27.42236680055714260, 166.5217562850347406, 1.224646799147364892E-15 ) ) ;
#34752 = CARTESIAN_POINT ( 'NONE',  ( 65.92267706577344200, 69.18571671596606620, 0.2487269089564623503 ) ) ;
#34753 = VERTEX_POINT ( 'NONE', #25134 ) ;
#34754 = DIRECTION ( 'NONE',  ( -1.000000000000000000, 0.000000000000000000, 0.000000000000000000 ) ) ;
#34755 = EDGE_CURVE ( 'NONE', #32378, #62928, #85653, .T. ) ;
#34756 = CARTESIAN_POINT ( 'NONE',  ( 204.9919120605564444, 269.2057140325208593, -2.990236076290825107 ) ) ;
#34757 = CARTESIAN_POINT ( 'NONE',  ( 164.1222658720982963, 246.3788921866353405, -8.359706015582100136 ) ) ;
#34758 = CARTESIAN_POINT ( 'NONE',  ( 45.00959873851216031, 26.39040679176986970, 1.333680081654574804E-15 ) ) ;
#34759 = CARTESIAN_POINT ( 'NONE',  ( 163.1008115941903895, 248.1481028935802442, 11.25332017433677834 ) ) ;
#34761 = CARTESIAN_POINT ( 'NONE',  ( 88.29163947745264807, 44.34544895456824065, 2.315384907525153135 ) ) ;
#34760 = FACE_OUTER_BOUND ( 'NONE', #67782, .T. ) ;
#34762 = AXIS2_PLACEMENT_3D ( 'NONE', #26504, #43163, #11323 ) ;
#34763 = CARTESIAN_POINT ( 'NONE',  ( 203.9648368022151601, 269.0477214045654364, 5.644613064108824574 ) ) ;
#34764 = ORIENTED_EDGE ( 'NONE', *, *, #65731, .F. ) ;
#34765 = B_SPLINE_CURVE_WITH_KNOTS ( 'NONE', 3,
 ( #91812, #38050, #77591, #9696, #39047, #8178, #93304, #8673, #86230, #24376, #85214, #31957, #77065, #69959, #61854, #54752, #62860, #68963, #15759, #46148, #93817, #55248, #16765, #78084, #92803, #39543, #23861, #31458, #16267, #1079, #54241, #574, #24866, #30470, #47656, #85738, #47160, #7673, #69468, #79114, #70465, #46664, #78591, #9176, #40050, #70990 ),
 .UNSPECIFIED., .F., .F.,
 ( 4, 1, 2, 2, 1, 2, 2, 1, 1, 2, 2, 1, 1, 2, 2, 1, 1, 2, 2, 1, 1, 1, 2, 2, 1, 1, 1, 2, 2, 4 ),
 ( 0.007499696492506968508, 0.06953096546172284065, 0.1005465999463296539, 0.1315622344309364811, 0.1935935034001495803, 0.2246091378847561715, 0.2556247723693627072, 0.3176560413385787207, 0.3486716758231865332, 0.3641794930654918550, 0.3796873103077972322, 0.4417185792770212394, 0.4727342137616331597, 0.4882420310039392031, 0.5037498482462451355, 0.5657811172154665336, 0.5967967517000785094, 0.6123045689423857185, 0.6278123861846929277, 0.6898436551539256500, 0.7208592896385420667, 0.7363671068808488318, 0.7441210155020008266, 0.7518749241231527103, 0.8139061930923631172, 0.8449218275769683206, 0.8604296448192708668, 0.8681835534404220844, 0.8759374620615733020, 1.000000000000000000 ),
 .UNSPECIFIED. ) ;
#34766 = LINE ( 'NONE', #48986, #32218 ) ;
#34767 = CARTESIAN_POINT ( 'NONE',  ( 189.8468993113617955, 274.1474532089198419, -15.62931057064303708 ) ) ;
#34768 = CARTESIAN_POINT ( 'NONE',  ( 72.01549410641601412, 65.88731131220951909, -12.15293914534650277 ) ) ;
#34769 = CARTESIAN_POINT ( 'NONE',  ( 153.4242699508872647, 264.9083646613370320, 16.62000820703435267 ) ) ;
#34770 = CARTESIAN_POINT ( 'NONE',  ( 80.76710472214251979, 43.07881916343166750, -9.774221331374631561 ) ) ;
#34771 = DIRECTION ( 'NONE',  ( -0.7253665389804496710, -0.6883628288392130701, 0.000000000000000000 ) ) ;
#34772 = CARTESIAN_POINT ( 'NONE',  ( 1.258015332399702757, 171.5333772461660828, 9.188101187500095079 ) ) ;
#34773 = CARTESIAN_POINT ( 'NONE',  ( 105.2078667585768557, 240.7369531367911009, -4.594050593750048428 ) ) ;
#34774 = CARTESIAN_POINT ( 'NONE',  ( 154.9067123643522734, 262.3406990819208886, -18.18534662427576265 ) ) ;
#34775 = FACE_OUTER_BOUND ( 'NONE', #7466, .T. ) ;
#34776 = CARTESIAN_POINT ( 'NONE',  ( 179.9589285649147996, 254.9571903017543946, -2.426322644417845620 ) ) ;
#34777 = DIRECTION ( 'NONE',  ( 0.5000000000000014433, -0.8660254037844378194, 0.000000000000000000 ) ) ;
#34778 = CARTESIAN_POINT ( 'NONE',  ( 77.27856866401023694, 51.25232217808265034, 15.47710953478911655 ) ) ;
#34779 = CARTESIAN_POINT ( 'NONE',  ( -22.42236680055709641, 157.8615022471902591, 0.000000000000000000 ) ) ;
#34780 = CARTESIAN_POINT ( 'NONE',  ( 194.2154056360670040, 294.2560451561701029, -15.66696967429384557 ) ) ;
#34781 = CARTESIAN_POINT ( 'NONE',  ( -4.170157060006060235, 26.08383846222962887, -10.00000000000000000 ) ) ;
#34782 = B_SPLINE_CURVE_WITH_KNOTS ( 'NONE', 3,
 ( #51256, #43658, #59338, #90318 ),
 .UNSPECIFIED., .F., .F.,
 ( 4, 4 ),
 ( 0.01272487254098708317, 0.01903269051692836264 ),
 .UNSPECIFIED. ) ;
#34783 = CARTESIAN_POINT ( 'NONE',  ( 85.01541621076924571, 50.02003410940323391, 13.59443226853714926 ) ) ;
#34784 = CARTESIAN_POINT ( 'NONE',  ( 60.86586985908987657, 190.3595308348468791, 0.000000000000000000 ) ) ;
#34785 = CARTESIAN_POINT ( 'NONE',  ( 79.19548319422065674, 46.07689622240576455, -13.22575811200356810 ) ) ;
#34786 = CARTESIAN_POINT ( 'NONE',  ( 175.3120318915934490, 265.2928129103611923, -15.67177354101544395 ) ) ;
#34787 = B_SPLINE_CURVE_WITH_KNOTS ( 'NONE', 3,
 ( #38229, #90520, #28658, #29661, #98591, #83904, #75284, #100074, #5867, #91492, #45348, #15431, #76279, #52453, #6370, #6853, #22054, #46328, #30662, #36753, #5373, #21092, #29174, #44846, #36256, #98081, #91007, #51969, #83399, #37253, #68152, #37740, #53443, #30152, #63051, #55923 ),
 .UNSPECIFIED., .F., .F.,
 ( 4, 2, 2, 2, 2, 2, 2, 2, 2, 2, 2, 2, 2, 2, 2, 2, 2, 4 ),
 ( 0.003089973116247706104, 0.003286963708836297335, 0.003483954301424888132, 0.003582449597719183747, 0.003680944894013478928, 0.003877935486602134777, 0.004271916671779446908, 0.004665897856956759474, 0.005453860227311384604, 0.006241822597666009734, 0.007817747338375338056, 0.008014737930963938828, 0.008063985579110994478, 0.008113233227258048394, 0.008211728523552230818, 0.008605709708728910209, 0.008999690893905589600, 0.009393672079082267257 ),
 .UNSPECIFIED. ) ;
#34788 = CARTESIAN_POINT ( 'NONE',  ( 76.95378796010953693, 224.4244531367911293, -4.594050593750046652 ) ) ;
#34789 = CARTESIAN_POINT ( 'NONE',  ( 161.4143265314674522, 251.0691807084224365, -12.94469757303959234 ) ) ;
#34790 = VECTOR ( 'NONE', #82477, 1000.000000000000000 ) ;
#34791 = DIRECTION ( 'NONE',  ( -0.8660254037844379305, -0.5000000000000014433, -0.000000000000000000 ) ) ;
#34793 = CARTESIAN_POINT ( 'NONE',  ( 199.6932924450039764, 284.7680668849795325, 17.37765808470670237 ) ) ;
#34792 = CARTESIAN_POINT ( 'NONE',  ( 196.2609093297512857, 290.7131288316392670, 16.03897268885959448 ) ) ;
#34794 = CARTESIAN_POINT ( 'NONE',  ( 76.03019726450892790, 65.44783958900880805, 14.37600347258595690 ) ) ;
#34795 = CARTESIAN_POINT ( 'NONE',  ( 173.1680667592106317, 268.1563685006378819, -16.28935171270416404 ) ) ;
#34796 = ADVANCED_FACE ( 'NONE', ( #31719 ), #55518, .T. ) ;
#34797 = CARTESIAN_POINT ( 'NONE',  ( 34.67812306484451312, 22.94754757982092030, 5.678558825948272215 ) ) ;
#34798 = CARTESIAN_POINT ( 'NONE',  ( 79.57665710957374472, 49.21012782547803965, -14.80730596066503679 ) ) ;
#34799 = CARTESIAN_POINT ( 'NONE',  ( 74.71948287562122459, 57.03696899136454590, 16.52214785348690285 ) ) ;
#34800 = ORIENTED_EDGE ( 'NONE', *, *, #1818, .T. ) ;
#34801 = CARTESIAN_POINT ( 'NONE',  ( 20.04711164229383513, 17.28920272979926764, -7.433330006724141015 ) ) ;
#34802 = DIRECTION ( 'NONE',  ( 0.5000000000000005551, -0.8660254037844382635, -3.965082230804119373E-16 ) ) ;
#34803 = CARTESIAN_POINT ( 'NONE',  ( -30.05514682052448450, 94.68088024134054592, 12.56018961544704915 ) ) ;
#34804 = CARTESIAN_POINT ( 'NONE',  ( 54.63354020801843092, 213.8967562850347122, -4.648177544792955347E-16 ) ) ;
#34805 = EDGE_CURVE ( 'NONE', #53225, #1108, #8262, .T. ) ;
#34806 = CARTESIAN_POINT ( 'NONE',  ( 86.11363163537949106, 47.05074959952599301, 10.74854466831323840 ) ) ;
#34807 = CARTESIAN_POINT ( 'NONE',  ( 193.5618293018212910, 288.4941101508381394, 16.06832059134343282 ) ) ;
#34808 = LINE ( 'NONE', #50511, #32309 ) ;
#34809 = CARTESIAN_POINT ( 'NONE',  ( 87.38898754588738882, 44.84176836479306871, -6.666552467508535251 ) ) ;
#34810 = CARTESIAN_POINT ( 'NONE',  ( 113.6157903772484303, 249.7365022471903444, 2.944929066748280225E-16 ) ) ;
#34811 = CARTESIAN_POINT ( 'NONE',  ( 157.8429099974857195, 257.2550556002704525, -17.85752049034686095 ) ) ;
#34812 = CARTESIAN_POINT ( 'NONE',  ( 74.82756539338009816, 53.47993334157433765, 16.54385625414931837 ) ) ;
#34813 = EDGE_LOOP ( 'NONE', ( #34957, #25643, #53028, #67841 ) ) ;
#34814 = CARTESIAN_POINT ( 'NONE',  ( 85.50503765007894685, 46.43143530048178036, 9.878743384447044917 ) ) ;
#34815 = ORIENTED_EDGE ( 'NONE', *, *, #25118, .F. ) ;
#34816 = CARTESIAN_POINT ( 'NONE',  ( 202.8167949821795446, 279.3580017930215149, 15.61966256214195070 ) ) ;
#34817 = CARTESIAN_POINT ( 'NONE',  ( 179.0122920114791327, 284.0021645867860798, 15.65938388908703871 ) ) ;
#34818 = EDGE_CURVE ( 'NONE', #32492, #23972, #41839, .T. ) ;
#34819 = ORIENTED_EDGE ( 'NONE', *, *, #30860, .F. ) ;
#34820 = CARTESIAN_POINT ( 'NONE',  ( -19.51954277429316065, 93.11267011235696600, 59.99999999999999289 ) ) ;
#34821 = ORIENTED_EDGE ( 'NONE', *, *, #76722, .F. ) ;
#34822 = CARTESIAN_POINT ( 'NONE',  ( 189.8548326329087104, 290.2376382689330967, 14.46855031197147312 ) ) ;
#34823 = CARTESIAN_POINT ( 'NONE',  ( 3.011046308360212809, 25.23654200823200355, 1.583844403245364241 ) ) ;
#34824 = PLANE ( 'NONE',  #86638 ) ;
#34825 = CARTESIAN_POINT ( 'NONE',  ( 193.2460171754006808, 295.9350752223151062, -13.17791578539254083 ) ) ;
#34826 = CARTESIAN_POINT ( 'NONE',  ( 203.7690284654797210, 275.7086850192775955, -13.99192714286714612 ) ) ;
#34827 = AXIS2_PLACEMENT_3D ( 'NONE', #23792, #93232, #54676 ) ;
#34828 = CARTESIAN_POINT ( 'NONE',  ( 29.04415360562664361, 34.95586893147757479, 7.433330006724141015 ) ) ;
#34829 = CARTESIAN_POINT ( 'NONE',  ( 76.29760026105621762, 59.55922990308604170, -15.89113754366026576 ) ) ;
#34830 = CARTESIAN_POINT ( 'NONE',  ( 74.25393038840245197, 55.45593832152543712, 16.12141555578006091 ) ) ;
#34831 = EDGE_CURVE ( 'NONE', #19903, #67514, #25940, .T. ) ;
#34832 = CARTESIAN_POINT ( 'NONE',  ( 81.06766895168334486, 217.6115022471902591, 10.00000000000009592 ) ) ;
#34833 = ORIENTED_EDGE ( 'NONE', *, *, #46245, .F. ) ;
#34834 = ORIENTED_EDGE ( 'NONE', *, *, #86399, .T. ) ;
#34835 = CARTESIAN_POINT ( 'NONE',  ( 186.3625697200866114, 298.6552741896666703, 1.069755126919976096 ) ) ;
#34837 = CARTESIAN_POINT ( 'NONE',  ( 176.9569807898301974, 265.3464266694197136, -16.55715408367980501 ) ) ;
#34836 = CARTESIAN_POINT ( 'NONE',  ( 68.33081780576208075, 65.63013816376739840, 10.40955482511126107 ) ) ;
#34838 = CARTESIAN_POINT ( 'NONE',  ( 85.51062282364698319, 48.96702101389664108, -12.23238128493630583 ) ) ;
#34839 = CARTESIAN_POINT ( 'NONE',  ( 201.3559594018653911, 274.8723170797262583, -14.12745182062582394 ) ) ;
#34840 = LINE ( 'NONE', #88619, #27042 ) ;
#34841 = CARTESIAN_POINT ( 'NONE',  ( 70.47590555702623760, 60.94424470842204755, 14.96950124546868111 ) ) ;
#34842 = CARTESIAN_POINT ( 'NONE',  ( 163.9705683675892942, 246.6416399718259527, 5.157764633724318593 ) ) ;
#34843 = CARTESIAN_POINT ( 'NONE',  ( 166.6337920219200441, 265.6691252616788006, 16.54534502771603499 ) ) ;
#34844 = CARTESIAN_POINT ( 'NONE',  ( 180.2352183475922800, 256.5785695326966902, 4.914414593082182314 ) ) ;
#34845 = CARTESIAN_POINT ( 'NONE',  ( 107.7251869580316281, 226.8768266524160140, 9.188101187500098632 ) ) ;
#34846 = VERTEX_POINT ( 'NONE', #74765 ) ;
#34847 = CARTESIAN_POINT ( 'NONE',  ( 68.22375369157856539, 184.2153022007868799, 0.000000000000000000 ) ) ;
#34848 = CARTESIAN_POINT ( 'NONE',  ( 163.0197392065574604, 276.6372685320687310, -14.12728359470665751 ) ) ;
#34849 = ORIENTED_EDGE ( 'NONE', *, *, #24624, .F. ) ;
#34850 = VERTEX_POINT ( 'NONE', #74272 ) ;
#34851 = EDGE_CURVE ( 'NONE', #46284, #3544, #97565, .T. ) ;
#34852 = CARTESIAN_POINT ( 'NONE',  ( 87.23676543452685905, 46.07418070687454303, -8.827152287545313669 ) ) ;
#34853 = CARTESIAN_POINT ( 'NONE',  ( 176.9594653488500455, 293.0447406222712061, -2.803451863092930374 ) ) ;
#34854 = CARTESIAN_POINT ( 'NONE',  ( 196.1241105319816143, 290.9500712997905794, 15.97146679939154268 ) ) ;
#34855 = CARTESIAN_POINT ( 'NONE',  ( 206.5081929095101998, 272.9643130319303737, -9.215516226794479238 ) ) ;
#34856 = DIRECTION ( 'NONE',  ( 0.1162373735601320568, 0.9932214622066130039, 0.000000000000000000 ) ) ;
#34857 = CARTESIAN_POINT ( 'NONE',  ( 91.43256340568937901, 235.8464784336661353, 1.353441290958777327E-15 ) ) ;
#34858 = ORIENTED_EDGE ( 'NONE', *, *, #55939, .T. ) ;
#34859 = AXIS2_PLACEMENT_3D ( 'NONE', #93361, #16326, #27438 ) ;
#34860 = EDGE_CURVE ( 'NONE', #15908, #67111, #65635, .T. ) ;
#34861 = EDGE_LOOP ( 'NONE', ( #55789, #97363, #73390, #92979 ) ) ;
#34862 = CARTESIAN_POINT ( 'NONE',  ( -16.26211276271277839, 167.1916292661125283, 5.188172501216621122E-14 ) ) ;
#34863 = VERTEX_POINT ( 'NONE', #81879 ) ;
#34864 = EDGE_CURVE ( 'NONE', #89739, #84849, #42817, .T. ) ;
#34865 = CIRCLE ( 'NONE', #91526, 70.00000000000001421 ) ;
#34866 = EDGE_CURVE ( 'NONE', #12230, #62531, #77092, .T. ) ;
#34867 = CARTESIAN_POINT ( 'NONE',  ( 191.4086613504252341, 263.7107970214009924, -8.083176656581560593 ) ) ;
#34868 = DIRECTION ( 'NONE',  ( 0.6116140086401538056, -0.7911563084720502070, 0.000000000000000000 ) ) ;
#34869 = CARTESIAN_POINT ( 'NONE',  ( 71.39421488629903934, 69.39266753417868472, -8.110451711237608663 ) ) ;
#34871 = CARTESIAN_POINT ( 'NONE',  ( 69.79245252017108214, 62.76958509742000558, -13.30825049901474344 ) ) ;
#34870 = CARTESIAN_POINT ( 'NONE',  ( 133.1643360984345179, 253.8149278399160949, 9.188101187500093303 ) ) ;
#34872 = FACE_OUTER_BOUND ( 'NONE', #10526, .T. ) ;
#34873 = DIRECTION ( 'NONE',  ( -0.9514785060800255989, 0.3077152132536228879, 0.000000000000000000 ) ) ;
#34874 = ORIENTED_EDGE ( 'NONE', *, *, #42302, .F. ) ;
#34875 = CARTESIAN_POINT ( 'NONE',  ( 157.3370492947211119, 258.1312320390110244, 17.02065074437983228 ) ) ;
#34876 = EDGE_CURVE ( 'NONE', #77470, #10592, #896, .T. ) ;
#34877 = CARTESIAN_POINT ( 'NONE',  ( 81.53053605624106126, 48.05823170493817287, 13.08105315416342052 ) ) ;
#34878 = CARTESIAN_POINT ( 'NONE',  ( 81.95798892854801920, 41.01614721200600400, -3.218282653241920865 ) ) ;
#34879 = ADVANCED_FACE ( 'NONE', ( #84861 ), #39110, .T. ) ;
#34880 = FACE_OUTER_BOUND ( 'NONE', #72702, .T. ) ;
#34881 = CARTESIAN_POINT ( 'NONE',  ( 178.3194779259755194, 285.3457979227533770, 13.03892382964784069 ) ) ;
#34882 = CARTESIAN_POINT ( 'NONE',  ( -19.65312891409030271, 93.06504152958497400, -10.00000000000000888 ) ) ;
#34883 = CARTESIAN_POINT ( 'NONE',  ( 82.63281508726200286, 40.94328431233920895, -3.617117793111280122 ) ) ;
#34884 = PLANE ( 'NONE',  #85126 ) ;
#34885 = CARTESIAN_POINT ( 'NONE',  ( 200.6449165581618956, 283.1198055712825976, 18.35107460171532523 ) ) ;
#34886 = B_SPLINE_CURVE_WITH_KNOTS ( 'NONE', 3,
 ( #28310, #3549, #50609, #97742, #49622, #74451, #51624, #81563, #88189, #42995, #82576, #33950, #57214, #42505, #95784, #26338, #50127, #65327, #4519, #96266, #11645, #66325, #88690, #34911, #35913, #97257, #27824, #58700, #89674, #20235, #51107 ),
 .UNSPECIFIED., .F., .F.,
 ( 4, 3, 3, 3, 3, 3, 3, 3, 3, 3, 4 ),
 ( 0.000000000000000000, 0.1333490885032313222, 0.3007194338854242699, 0.4699862290244929963, 0.5844252810809240639, 0.6686540514502682386, 0.7354980260655500368, 0.8028463152565734617, 0.8633854507757154906, 0.9437142632667211428, 1.000000000000000000 ),
 .UNSPECIFIED. ) ;
#34887 = CARTESIAN_POINT ( 'NONE',  ( 70.46185687578375223, 70.52818721896052523, -4.697131730717588383 ) ) ;
#34888 = CARTESIAN_POINT ( 'NONE',  ( 167.8874878883961230, 249.4612090931145474, 8.049769325627208261 ) ) ;
#34889 = CARTESIAN_POINT ( 'NONE',  ( 83.20726942458908582, 52.32534163598141674, 14.85174634631042423 ) ) ;
#34890 = CARTESIAN_POINT ( 'NONE',  ( 162.7459776558209228, 248.7626933030860812, -9.895605163646791880 ) ) ;
#34891 = CARTESIAN_POINT ( 'NONE',  ( 163.2143008875826240, 247.9515336713096474, -10.88636441666107579 ) ) ;
#34892 = CIRCLE ( 'NONE', #60762, 70.00000000000001421 ) ;
#34893 = CARTESIAN_POINT ( 'NONE',  ( 181.9334155871473513, 264.0643945792503473, 13.76495337570946376 ) ) ;
#34894 = CARTESIAN_POINT ( 'NONE',  ( 80.05961770938091604, 205.4824982072973967, 3.021315404115420679E-15 ) ) ;
#34895 = CARTESIAN_POINT ( 'NONE',  ( 40.66614990564659138, 23.28848085856234817, 1.475505719884397138E-15 ) ) ;
#34896 = CARTESIAN_POINT ( 'NONE',  ( 152.7153488183568300, 266.1362520814392951, 17.33540622643059237 ) ) ;
#34897 = LINE ( 'NONE', #81068, #7232 ) ;
#34898 = CARTESIAN_POINT ( 'NONE',  ( 71.70501702668993005, 58.75402291411430156, -15.44053495759504457 ) ) ;
#34899 = CIRCLE ( 'NONE', #99576, 0.1418229129680897982 ) ;
#34900 = CARTESIAN_POINT ( 'NONE',  ( 205.9981425428302373, 272.8521996776938749, -9.276084512156598905 ) ) ;
#34901 = CARTESIAN_POINT ( 'NONE',  ( 12.94935828348961593, 178.2833772461660544, -9.188101187500095079 ) ) ;
#34902 = DIRECTION ( 'NONE',  ( 0.4999999999999998890, -0.8660254037844385966, 0.000000000000000000 ) ) ;
#34903 = ORIENTED_EDGE ( 'NONE', *, *, #5954, .T. ) ;
#34904 = CARTESIAN_POINT ( 'NONE',  ( 86.54292033101232562, 46.25028892199807729, 8.970843135639706034 ) ) ;
#34905 = CARTESIAN_POINT ( 'NONE',  ( 36.90037335867700818, 182.1115022471902023, -5.000000000000041744 ) ) ;
#34906 = CARTESIAN_POINT ( 'NONE',  ( 163.8398374448017591, 246.8680725722146008, -5.948785025486735378 ) ) ;
#34907 = CARTESIAN_POINT ( 'NONE',  ( 82.16658848853110442, 41.26547592452066482, 5.424318534973775030 ) ) ;
#34908 = CARTESIAN_POINT ( 'NONE',  ( 44.31597619863101301, 187.2048013555409796, 4.594050593750051981 ) ) ;
#34909 = B_SPLINE_CURVE_WITH_KNOTS ( 'NONE', 3,
 ( #92473, #93476, #30136, #47326, #22542, #100056, #238, #77235, #23515, #39210, #91990, #7842, #30643, #31615, #53428, #1241, #31120, #729, #84377, #62511, #14924, #45813, #8831, #62010, #85905, #92962, #85383, #46834, #78252, #8340, #24028, #54927, #16430, #39700, #70631, #32124, #82224, #51260, #90820, #60340, #52746, #83707, #21862, #68947, #97889, #84212 ),
 .UNSPECIFIED., .F., .F.,
 ( 4, 1, 1, 1, 2, 2, 1, 1, 1, 2, 2, 1, 1, 2, 2, 1, 1, 2, 2, 1, 1, 2, 2, 1, 2, 2, 1, 2, 2, 4 ),
 ( 0.000000000000000000, 0.06249999999998029354, 0.09374999999997030153, 0.1093749999999655692, 0.1171874999999649586, 0.1249999999999643618, 0.1874999999999631128, 0.2187499999999606426, 0.2343749999999612532, 0.2421874999999597267, 0.2499999999999581446, 0.3124999999999589773, 0.3437499999999574229, 0.3593749999999568678, 0.3749999999999562572, 0.4374999999999509837, 0.4687499999999500955, 0.4843749999999513722, 0.4999999999999525935, 0.5624999999999675815, 0.5937499999999736877, 0.6093749999999763522, 0.6249999999999791278, 0.6874999999999837907, 0.7187499999999863443, 0.7499999999999887867, 0.8124999999999932276, 0.8437499999999955591, 0.8749999999999977796, 1.000000000000000000 ),
 .UNSPECIFIED. ) ;
#34910 = EDGE_CURVE ( 'NONE', #91683, #14425, #70615, .T. ) ;
#34911 = CARTESIAN_POINT ( 'NONE',  ( 86.88058850597731464, 45.96296635460476665, 8.956153083123110648 ) ) ;
#34912 = CARTESIAN_POINT ( 'NONE',  ( 190.8957779480239765, 300.0058089740729770, -4.541438514207768229 ) ) ;
#34913 = CARTESIAN_POINT ( 'NONE',  ( 35.94483945213000453, 39.49103043416551628, -8.090169943749479842 ) ) ;
#34914 = CARTESIAN_POINT ( 'NONE',  ( 181.7846118114498495, 294.3892353584903390, 6.386930120770952790 ) ) ;
#34915 = CARTESIAN_POINT ( 'NONE',  ( 146.5095091551180815, 276.8850816817948726, 0.1418322875769769398 ) ) ;
#34916 = VECTOR ( 'NONE', #13840, 1000.000000000000000 ) ;
#34917 = AXIS2_PLACEMENT_3D ( 'NONE', #34784, #17601, #96641 ) ;
#34918 = CARTESIAN_POINT ( 'NONE',  ( 179.4052326654324929, 278.4640086126446477, -16.45363309275438013 ) ) ;
#34919 = CARTESIAN_POINT ( 'NONE',  ( 70.29670215996473814, 67.87645915626477233, -9.215380671816021163 ) ) ;
#34920 = CARTESIAN_POINT ( 'NONE',  ( 93.16602416993194424, 213.0494855054051584, -2.679491924311248496 ) ) ;
#34921 = ADVANCED_FACE ( 'NONE', ( #1228 ), #93965, .T. ) ;
#34922 = PLANE ( 'NONE',  #82317 ) ;
#34923 = AXIS2_PLACEMENT_3D ( 'NONE', #38892, #24695, #39872 ) ;
#34924 = CARTESIAN_POINT ( 'NONE',  ( 79.76863084600667264, 216.8615022471902591, -10.00000000000009592 ) ) ;
#34925 = DIRECTION ( 'NONE',  ( -0.8660254037844379305, -0.5000000000000014433, -0.000000000000000000 ) ) ;
#34926 = DIRECTION ( 'NONE',  ( -0.9762143704923794685, 0.2168075248790211351, 0.000000000000000000 ) ) ;
#34927 = ORIENTED_EDGE ( 'NONE', *, *, #29524, .F. ) ;
#34928 = CARTESIAN_POINT ( 'NONE',  ( 42.50247518763358556, 195.3458772461660544, 9.188101187500095079 ) ) ;
#34929 = ORIENTED_EDGE ( 'NONE', *, *, #73759, .F. ) ;
#34930 = CARTESIAN_POINT ( 'NONE',  ( -13.14524566621093626, 85.30073937114704563, 14.89871103469313951 ) ) ;
#34931 = CARTESIAN_POINT ( 'NONE',  ( 190.4976253092930278, 300.6954295735222900, -5.764807383508308902 ) ) ;
#34932 = EDGE_CURVE ( 'NONE', #39677, #65525, #86382, .T. ) ;
#34933 = CARTESIAN_POINT ( 'NONE',  ( 67.24893291460693945, 66.51310417600045355, -8.632834435144324914 ) ) ;
#34934 = VERTEX_POINT ( 'NONE', #9326 ) ;
#34935 = CARTESIAN_POINT ( 'NONE',  ( 171.3240658019900025, 286.5505184989698932, 7.546585824849171509 ) ) ;
#34936 = CARTESIAN_POINT ( 'NONE',  ( -10.54235908185773418, 24.92402704602492847, 10.00000000000000000 ) ) ;
#34937 = CARTESIAN_POINT ( 'NONE',  ( -112.5954152546897262, 74.04580364311806306, -30.52142883766498116 ) ) ;
#34938 = CARTESIAN_POINT ( 'NONE',  ( 35.31080938399455249, 26.10170272979929607, -7.433330006724141015 ) ) ;
#34939 = CARTESIAN_POINT ( 'NONE',  ( 185.7387126045402681, 263.0356376848994842, 11.21768123893770941 ) ) ;
#34940 = CARTESIAN_POINT ( 'NONE',  ( 178.9433923089253256, 286.0771944333194483, -14.51609702535374424 ) ) ;
#34941 = CARTESIAN_POINT ( 'NONE',  ( 171.2953940480069264, 255.8198119141705149, 11.80824276626711899 ) ) ;
#34942 = VERTEX_POINT ( 'NONE', #71649 ) ;
#34943 = CARTESIAN_POINT ( 'NONE',  ( 13.01786573420820403, 22.91421378149917842, 9.188101187500008038 ) ) ;
#34944 = DIRECTION ( 'NONE',  ( 0.000000000000000000, 0.000000000000000000, 1.000000000000000000 ) ) ;
#34945 = DIRECTION ( 'NONE',  ( -0.000000000000000000, -0.000000000000000000, 1.000000000000000000 ) ) ;
#34946 = EDGE_CURVE ( 'NONE', #7407, #34378, #48328, .T. ) ;
#34947 = ORIENTED_EDGE ( 'NONE', *, *, #75650, .T. ) ;
#34948 = PLANE ( 'NONE',  #40109 ) ;
#34949 = DIRECTION ( 'NONE',  ( 0.000000000000000000, 0.000000000000000000, 1.000000000000000000 ) ) ;
#34950 = EDGE_CURVE ( 'NONE', #11091, #20729, #61350, .T. ) ;
#34951 = CARTESIAN_POINT ( 'NONE',  ( -14.65312891409034535, 84.40478749174073414, 0.000000000000000000 ) ) ;
#34952 = ORIENTED_EDGE ( 'NONE', *, *, #62897, .F. ) ;
#34953 = ORIENTED_EDGE ( 'NONE', *, *, #48500, .T. ) ;
#34955 = DIRECTION ( 'NONE',  ( 0.4999999999999998890, -0.8660254037844385966, 0.000000000000000000 ) ) ;
#34954 = CARTESIAN_POINT ( 'NONE',  ( 207.2337123599961899, 271.7076764818092443, -5.443417788256701861 ) ) ;
#34956 = CARTESIAN_POINT ( 'NONE',  ( 149.2593905435863348, 272.1221474021800759, -12.98626158366800176 ) ) ;
#34957 = ORIENTED_EDGE ( 'NONE', *, *, #57791, .F. ) ;
#34958 = CARTESIAN_POINT ( 'NONE',  ( 66.38567292659833186, 68.74021793980560346, -2.134846014654135704 ) ) ;
#34959 = LINE ( 'NONE', #73985, #22180 ) ;
#34960 = CARTESIAN_POINT ( 'NONE',  ( 184.3563745939584919, 257.8924429673292025, 6.070039865595379780 ) ) ;
#34961 = DIRECTION ( 'NONE',  ( -0.8660254037844377084, -0.5000000000000014433, -0.000000000000000000 ) ) ;
#34962 = CARTESIAN_POINT ( 'NONE',  ( 32.06973406193871057, 92.10133962881208447, 59.99999999999999289 ) ) ;
#34963 = CARTESIAN_POINT ( 'NONE',  ( 113.3268549190559753, 245.4244531367911293, -4.594050593750046652 ) ) ;
#34964 = FACE_OUTER_BOUND ( 'NONE', #1774, .T. ) ;
#34965 = LINE ( 'NONE', #51684, #15570 ) ;
#34966 = AXIS2_PLACEMENT_3D ( 'NONE', #58985, #96567, #20034 ) ;
#34967 = VERTEX_POINT ( 'NONE', #65028 ) ;
#34968 = CARTESIAN_POINT ( 'NONE',  ( 164.4963285489318991, 245.7309966251440301, -6.672251175510283794 ) ) ;
#34969 = AXIS2_PLACEMENT_3D ( 'NONE', #55423, #55921, #78265 ) ;
#34970 = ORIENTED_EDGE ( 'NONE', *, *, #82290, .T. ) ;
#34971 = CARTESIAN_POINT ( 'NONE',  ( 29.04415360562664361, 34.95586893147757479, 7.433330006724141015 ) ) ;
#34972 = CARTESIAN_POINT ( 'NONE',  ( 198.3449891235413531, 287.1033967417670283, 16.95540786497457120 ) ) ;
#34973 = CARTESIAN_POINT ( 'NONE',  ( -19.65312891409030271, 93.06504152958497400, -10.00000000000000888 ) ) ;
#34974 = CARTESIAN_POINT ( 'NONE',  ( 81.44681538588882574, 208.6423013555409796, -4.594050593750043987 ) ) ;
#34975 = CARTESIAN_POINT ( 'NONE',  ( 174.9992441152388096, 285.3729034877181903, 13.43039555807443719 ) ) ;
#34976 = CARTESIAN_POINT ( 'NONE',  ( 191.5694459269389824, 298.8389818071599962, 7.944420692511652504 ) ) ;
#34977 = CARTESIAN_POINT ( 'NONE',  ( 151.0171360864231644, 269.0776428152087760, 14.21401713093731267 ) ) ;
#34978 = CIRCLE ( 'NONE', #77058, 70.00000000000001421 ) ;
#34979 = CARTESIAN_POINT ( 'NONE',  ( 171.8853837999505743, 276.6425513415854880, 16.11255734744161217 ) ) ;
#34980 = ORIENTED_EDGE ( 'NONE', *, *, #93239, .T. ) ;
#34981 = EDGE_CURVE ( 'NONE', #58917, #87772, #97835, .T. ) ;
#34982 = CARTESIAN_POINT ( 'NONE',  ( 79.70677143361787387, 46.01134058561531504, 12.98241517792750699 ) ) ;
#34983 = CARTESIAN_POINT ( 'NONE',  ( -32.57204513736933649, 62.44441720109064420, -10.00000000000000000 ) ) ;
#34984 = ORIENTED_EDGE ( 'NONE', *, *, #35995, .T. ) ;
#34985 = CARTESIAN_POINT ( 'NONE',  ( 194.7759874552263852, 293.2850889635864178, 15.50361547754712532 ) ) ;
#34986 = CARTESIAN_POINT ( 'NONE',  ( -19.74036418170400609, 92.95322137609242930, 59.99999999999999289 ) ) ;
#34987 = CARTESIAN_POINT ( 'NONE',  ( 163.6930646551726909, 260.3320553973381379, -16.18243281979474446 ) ) ;
#34988 = CARTESIAN_POINT ( 'NONE',  ( 93.96857342517719758, 15.00000000000000000, 0.000000000000000000 ) ) ;
#34989 = EDGE_CURVE ( 'NONE', #55973, #46528, #25116, .T. ) ;
#34990 = CARTESIAN_POINT ( 'NONE',  ( 160.5893190321802138, 270.9897182155185078, 16.60663562724527864 ) ) ;
#34991 = CARTESIAN_POINT ( 'NONE',  ( 206.2520115784021471, 273.4080321133600933, 11.69992874350409018 ) ) ;
#34992 = DIRECTION ( 'NONE',  ( -0.7691052716734865236, -0.08748735329024208418, 0.6331058711608359424 ) ) ;
#34993 = CARTESIAN_POINT ( 'NONE',  ( 127.5984922056368163, 251.1427522451419065, -10.00000000000009592 ) ) ;
#34994 = CARTESIAN_POINT ( 'NONE',  ( 164.1646814417103144, 253.9179673720841208, 14.54048895392611485 ) ) ;
#34995 = CARTESIAN_POINT ( 'NONE',  ( 109.9999999999999716, 10.00000000000004086, 14.21260523776213347 ) ) ;
#34996 = EDGE_CURVE ( 'NONE', #18309, #4228, #23845, .T. ) ;
#34997 = CARTESIAN_POINT ( 'NONE',  ( 134.5180214354952284, 236.2202760586659736, -5.415160957724236172E-17 ) ) ;
#34998 = ORIENTED_EDGE ( 'NONE', *, *, #78809, .F. ) ;
#34999 = CIRCLE ( 'NONE', #98159, 70.00000000000001421 ) ;
#35000 = CARTESIAN_POINT ( 'NONE',  ( 191.0702043019150835, 299.7036936669546776, -8.800021049343948576 ) ) ;
#35001 = DIRECTION ( 'NONE',  ( 0.8902628732232650277, -0.4554470513245822971, 0.000000000000000000 ) ) ;
#35002 = LINE ( 'NONE', #64419, #42460 ) ;
#35003 = VECTOR ( 'NONE', #59346, 1000.000000000000000 ) ;
#35004 = CARTESIAN_POINT ( 'NONE',  ( -110.0000000000000000, 0.000000000000000000, 59.99999999999999289 ) ) ;
#35005 = CARTESIAN_POINT ( 'NONE',  ( -26.59607535340071394, 23.41021043553328695, 177.5919119679930134 ) ) ;
#35006 = DIRECTION ( 'NONE',  ( -0.000000000000000000, -0.000000000000000000, -1.000000000000000000 ) ) ;
#35007 = VERTEX_POINT ( 'NONE', #74139 ) ;
#35008 = CARTESIAN_POINT ( 'NONE',  ( 77.33081455423041461, 59.48262537591812560, 16.03249298943872603 ) ) ;
#35009 = DIRECTION ( 'NONE',  ( 0.000000000000000000, -0.000000000000000000, -1.000000000000000000 ) ) ;
#35010 = CARTESIAN_POINT ( 'NONE',  ( 92.93017357788669131, 158.0650415295850735, -36.50000000000000000 ) ) ;
#35011 = CARTESIAN_POINT ( 'NONE',  ( 206.6347703933553532, 272.7450743988160866, -10.98802705318387574 ) ) ;
#35012 = CARTESIAN_POINT ( 'NONE',  ( 143.8274474304129171, 253.8458772461660260, 9.188101187500095079 ) ) ;
#35013 = CARTESIAN_POINT ( 'NONE',  ( 189.5059428776464756, 300.4130739301078279, -3.423561384717671796 ) ) ;
#35014 = CARTESIAN_POINT ( 'NONE',  ( 146.9709166616330549, 276.0859004375172390, 3.755270622130282732 ) ) ;
#35015 = CARTESIAN_POINT ( 'NONE',  ( 69.40490131253574191, 70.33133358430262660, 3.195916881608930726 ) ) ;
#35016 = CARTESIAN_POINT ( 'NONE',  ( 204.8057697639265768, 275.9129964160624695, -12.68356524114230766 ) ) ;
#35017 = CARTESIAN_POINT ( 'NONE',  ( 171.4502795663483994, 250.9255985275387104, 3.410053715956228970 ) ) ;
#35018 = CARTESIAN_POINT ( 'NONE',  ( 21.09856983598611535, 20.38052372038641025, 10.00000000000000533 ) ) ;
#35019 = CARTESIAN_POINT ( 'NONE',  ( 149.6896757981861583, 271.3768714794653647, 12.49809796062302603 ) ) ;
#35020 = DIRECTION ( 'NONE',  ( -0.8660254037844384856, -0.5000000000000002220, -3.252519625699449945E-16 ) ) ;
#35021 = CARTESIAN_POINT ( 'NONE',  ( 169.4056225884307310, 285.0682111663155638, -8.437954092449052368 ) ) ;
#35022 = CARTESIAN_POINT ( 'NONE',  ( 202.9490938173916561, 279.1288534886517709, -16.56031645010252973 ) ) ;
#35023 = CARTESIAN_POINT ( 'NONE',  ( 157.5068167110588035, 270.9949351285441708, -14.70592521109709416 ) ) ;
#35024 = CARTESIAN_POINT ( 'NONE',  ( 129.4027117968543621, 255.5177522451419350, 5.000000000000046185 ) ) ;
#35025 = CARTESIAN_POINT ( 'NONE',  ( 175.9979136080305011, 285.3618921757466182, -12.01256837341941086 ) ) ;
#35026 = ORIENTED_EDGE ( 'NONE', *, *, #57373, .T. ) ;
#35027 = ADVANCED_FACE ( 'NONE', ( #35110 ), #96466, .T. ) ;
#35028 = CARTESIAN_POINT ( 'NONE',  ( 157.2744851780909414, 258.2395962677452985, 18.17792129701959070 ) ) ;
#35029 = B_SPLINE_CURVE_WITH_KNOTS ( 'NONE', 3,
 ( #90567, #13528, #44396, #75331, #53979, #78317, #38285, #84937, #32194, #77823, #39767, #70697, #40279, #92540, #47393, #69196, #8405, #14990, #39276, #63597, #100124, #62579, #32697, #7394, #85452, #24096, #47880, #794, #55478, #30709, #1311, #8898, #1812, #61589, #31679, #22606, #62079, #70186, #31188, #53493, #23087, #93540, #93026, #86464, #94042, #7915 ),
 .UNSPECIFIED., .F., .F.,
 ( 4, 2, 2, 2, 2, 2, 2, 2, 2, 2, 2, 2, 2, 2, 2, 2, 2, 2, 2, 2, 2, 2, 4 ),
 ( 0.002409292539555501350, 0.002836404853134061061, 0.003049961009923312077, 0.003156739088317942355, 0.003263517166712573067, 0.003370295245107203345, 0.003477073323501833624, 0.003690629480291128875, 0.004117741793869665601, 0.004971966421026801503, 0.005826191048183937404, 0.006680415675341073306, 0.007107527988919563194, 0.007534640302498051348, 0.007641418380892598360, 0.007694807420089909596, 0.007748196459287221699, 0.007854974537681806007, 0.007961752616076388581, 0.008388864929654481217, 0.008815977243232575589, 0.009029533400021706041, 0.009243089556810838228 ),
 .UNSPECIFIED. ) ;
#35030 = CARTESIAN_POINT ( 'NONE',  ( 147.6207754342248961, 274.9603120256437592, 8.795690793376332195 ) ) ;
#35031 = CARTESIAN_POINT ( 'NONE',  ( -2.016382903836450691, 160.4548013555409796, -4.594050593750042211 ) ) ;
#35032 = VECTOR ( 'NONE', #10076, 1000.000000000000000 ) ;
#35033 = CARTESIAN_POINT ( 'NONE',  ( 42.82723471405275717, 195.5333772461660544, 9.188101187500095079 ) ) ;
#35034 = CARTESIAN_POINT ( 'NONE',  ( 178.7635222630899534, 259.0797437575516824, -11.44071160735324710 ) ) ;
#35035 = CARTESIAN_POINT ( 'NONE',  ( 21.90410768801267949, 17.81029122506294726, 8.090169943749479842 ) ) ;
#35036 = CARTESIAN_POINT ( 'NONE',  ( 67.91095298726213514, 65.32202572000780094, -10.47973064602391524 ) ) ;
#35037 = CARTESIAN_POINT ( 'NONE',  ( 204.6713671561005299, 276.1457885614869951, -12.94307097876490431 ) ) ;
#35038 = CARTESIAN_POINT ( 'NONE',  ( 188.7855976875974306, 290.4470481293840862, -14.77264779262060301 ) ) ;
#35039 = CARTESIAN_POINT ( 'NONE',  ( 190.3286155001717930, 300.9881631498979004, -5.624828231725103045 ) ) ;
#35040 = CARTESIAN_POINT ( 'NONE',  ( 73.86299659849926513, 55.57419400639425788, -16.58552430813258027 ) ) ;
#35042 = CARTESIAN_POINT ( 'NONE',  ( 70.51298433951257039, 211.5177522451418497, -10.00000000000009592 ) ) ;
#35041 = CARTESIAN_POINT ( 'NONE',  ( 171.2418428706442342, 258.0450685527933388, 14.49083553076813402 ) ) ;
#35043 = CARTESIAN_POINT ( 'NONE',  ( 77.23305886468027381, 62.39039902364388723, 15.82877784703884672 ) ) ;
#35044 = CARTESIAN_POINT ( 'NONE',  ( 157.7847820078105201, 257.3557362317297361, -18.02899742403477035 ) ) ;
#35045 = FACE_OUTER_BOUND ( 'NONE', #53473, .T. ) ;
#35046 = VECTOR ( 'NONE', #29465, 1000.000000000000114 ) ;
#35047 = CARTESIAN_POINT ( 'NONE',  ( 48.51954752611824517, 185.4865022471901739, 1.119607411625061291E-15 ) ) ;
#35048 = CARTESIAN_POINT ( 'NONE',  ( 184.6473554711987504, 293.6427102601792853, 9.570857982651210349 ) ) ;
#35049 = CARTESIAN_POINT ( 'NONE',  ( 163.3854574543125580, 247.6550818016845597, 10.82482370245618775 ) ) ;
#35050 = CARTESIAN_POINT ( 'NONE',  ( 3.802138503898990329, 166.8768266524160140, 9.188101187500098632 ) ) ;
#35051 = CARTESIAN_POINT ( 'NONE',  ( 166.9877576141370810, 285.6245928529402249, 4.094825844093839429 ) ) ;
#35052 = CARTESIAN_POINT ( 'NONE',  ( 153.4289928607825573, 264.9001843414388873, 17.27358709529985958 ) ) ;
#35053 = CARTESIAN_POINT ( 'NONE',  ( 30.99092310034283315, 39.93396525600392977, 2.839279412974139660 ) ) ;
#35054 = CARTESIAN_POINT ( 'NONE',  ( 84.23513719695283442, 207.8932355074535678, -2.679491924311248496 ) ) ;
#35055 = EDGE_CURVE ( 'NONE', #5025, #98414, #82269, .T. ) ;
#35056 = CARTESIAN_POINT ( 'NONE',  ( 180.5543891548928741, 277.3255815685567995, 16.32703862730248900 ) ) ;
#35057 = CARTESIAN_POINT ( 'NONE',  ( 193.8913555215501390, 294.8173164187117550, 15.40725395879721837 ) ) ;
#35058 = CARTESIAN_POINT ( 'NONE',  ( 148.9504735598738137, 272.6572073132907690, -11.88406006066344744 ) ) ;
#35059 = CARTESIAN_POINT ( 'NONE',  ( 177.3592972006726427, 260.4793513326881111, -13.85185052211657109 ) ) ;
#35060 = PRODUCT_CONTEXT ( 'NONE', #44826, 'mechanical' ) ;
#35061 = CARTESIAN_POINT ( 'NONE',  ( 7.821713311501573784, 19.91421378149916421, 9.188101187500008038 ) ) ;
#35062 = CARTESIAN_POINT ( 'NONE',  ( 115.5259514080638468, 249.0530062829863311, -4.648177544792955347E-16 ) ) ;
#35063 = CARTESIAN_POINT ( 'NONE',  ( 23.64951029700316099, 14.44966523072494802, -2.296566073217252530E-15 ) ) ;
#35064 = CARTESIAN_POINT ( 'NONE',  ( 82.86586985908988368, 152.2544130683315871, 0.000000000000000000 ) ) ;
#35065 = VECTOR ( 'NONE', #7737, 1000.000000000000000 ) ;
#35066 = CARTESIAN_POINT ( 'NONE',  ( 153.0818245731483103, 277.5927342487316878, -5.205759267561572479 ) ) ;
#35067 = ORIENTED_EDGE ( 'NONE', *, *, #8669, .F. ) ;
#35068 = AXIS2_PLACEMENT_3D ( 'NONE', #77869, #40828, #63650 ) ;
#35069 = DIRECTION ( 'NONE',  ( 0.000000000000000000, 1.000000000000000000, 0.000000000000000000 ) ) ;
#35070 = CARTESIAN_POINT ( 'NONE',  ( -19.65312891409030271, 93.06504152958497400, -10.00000000000000888 ) ) ;
#35071 = EDGE_CURVE ( 'NONE', #30332, #16059, #43703, .T. ) ;
#35072 = EDGE_LOOP ( 'NONE', ( #36352, #12435, #5422, #25491 ) ) ;
#35073 = CARTESIAN_POINT ( 'NONE',  ( 152.4703890395534813, 267.8466532369516813, 15.62370772889803128 ) ) ;
#35074 = CARTESIAN_POINT ( 'NONE',  ( 164.4781197247689306, 245.7625352337404649, -1.511762618280499515 ) ) ;
#35075 = VECTOR ( 'NONE', #42304, 1000.000000000000227 ) ;
#35076 = CARTESIAN_POINT ( 'NONE',  ( 66.58223749524904633, 68.25836364787168975, 4.558095512795234505 ) ) ;
#35077 = EDGE_CURVE ( 'NONE', #11388, #81557, #49330, .T. ) ;
#35078 = CARTESIAN_POINT ( 'NONE',  ( 87.33294734268929460, 44.88192199842170282, 6.808005391826769781 ) ) ;
#35079 = ORIENTED_EDGE ( 'NONE', *, *, #46640, .T. ) ;
#35080 =( BOUNDED_CURVE ( )  B_SPLINE_CURVE ( 2, ( #33927, #26312, #43484, #33404, #57187, #18714, #27804, #64305, #95257, #42481, #25824, #49108, #58677 ),
 .UNSPECIFIED., .F., .T. ) 
 B_SPLINE_CURVE_WITH_KNOTS ( ( 3, 2, 2, 2, 2, 2, 3 ),
 ( 0.3624999999999999889, 0.3649999999999999911, 0.3699999999999999956, 0.3750000000000000000, 0.3800000000000000044, 0.3850000000000000089, 0.3875000000000000111 ),
 .UNSPECIFIED. ) 
 CURVE ( )  GEOMETRIC_REPRESENTATION_ITEM ( )  RATIONAL_B_SPLINE_CURVE ( ( 0.9755282581475768211, 0.9755282581475768211, 1.000000000000000000, 0.9510565162951535312, 1.000000000000000000, 0.9510565162951535312, 1.000000000000000000, 0.9510565162951535312, 1.000000000000000000, 0.9510565162951535312, 1.000000000000000000, 0.9755282581475768211, 0.9755282581475768211 ) ) 
 REPRESENTATION_ITEM ( '' )  );
#35081 = ORIENTED_EDGE ( 'NONE', *, *, #46625, .F. ) ;
#35083 = CARTESIAN_POINT ( 'NONE',  ( 164.2712161151136172, 246.1209027979328710, 7.276091357954241445 ) ) ;
#35082 = CARTESIAN_POINT ( 'NONE',  ( 159.7776096774677228, 278.5608043355848622, -9.713761887137795981 ) ) ;
#35084 = CARTESIAN_POINT ( 'NONE',  ( 152.6656396574222754, 266.2223508737794759, 17.04346597795114349 ) ) ;
#35085 = VERTEX_POINT ( 'NONE', #84742 ) ;
#35086 = CARTESIAN_POINT ( 'NONE',  ( 17.70578863690133886, 169.4824982072973967, 3.021315404115420679E-15 ) ) ;
#35087 = CARTESIAN_POINT ( 'NONE',  ( 178.3153863976500588, 263.9796422997153513, 15.06320836021970067 ) ) ;
#35088 = ORIENTED_EDGE ( 'NONE', *, *, #42792, .T. ) ;
#35089 = CARTESIAN_POINT ( 'NONE',  ( -22.42236680055709641, 157.8615022471902591, 0.000000000000000000 ) ) ;
#35090 = CARTESIAN_POINT ( 'NONE',  ( 88.50942844660002606, 43.88426665780151836, -0.4971503815960297556 ) ) ;
#35091 = CARTESIAN_POINT ( 'NONE',  ( 27.53018959221258655, 41.35687530090521591, 10.00000000000000000 ) ) ;
#35092 = ORIENTED_EDGE ( 'NONE', *, *, #91935, .T. ) ;
#35093 = CARTESIAN_POINT ( 'NONE',  ( 177.1727833070994791, 269.3651756797060557, 16.08978429131461141 ) ) ;
#35094 = CARTESIAN_POINT ( 'NONE',  ( 166.2726692463831171, 274.2434846602475318, -15.18227389483641510 ) ) ;
#35095 = LINE ( 'NONE', #95958, #97945 ) ;
#35096 = ORIENTED_EDGE ( 'NONE', *, *, #96548, .F. ) ;
#35097 = CARTESIAN_POINT ( 'NONE',  ( 176.5585609647920364, 278.9355578903217747, -16.94606152164766755 ) ) ;
#35098 = ORIENTED_EDGE ( 'NONE', *, *, #81431, .T. ) ;
#35099 = CARTESIAN_POINT ( 'NONE',  ( 156.8295168708270069, 266.6489491931308180, -16.21854842269177510 ) ) ;
#35100 = VERTEX_POINT ( 'NONE', #46178 ) ;
#35101 = CARTESIAN_POINT ( 'NONE',  ( 157.5614123822272745, 268.8543676321601765, 15.62611732898177053 ) ) ;
#35102 = ORIENTED_EDGE ( 'NONE', *, *, #34192, .F. ) ;
#35103 = ADVANCED_FACE ( 'NONE', ( #83748 ), #98962, .F. ) ;
#35104 = CARTESIAN_POINT ( 'NONE',  ( 48.21858077004886667, 104.0489273421469818, -10.00000000000000000 ) ) ;
#35105 = CARTESIAN_POINT ( 'NONE',  ( 169.0307616625812557, 272.4356441479760633, 16.34146891005438818 ) ) ;
#35106 = CARTESIAN_POINT ( 'NONE',  ( 194.0554856868662057, 294.5330346333298053, 14.40212516007646038 ) ) ;
#35107 = CARTESIAN_POINT ( 'NONE',  ( 82.78422215508307147, 53.78621188977053436, 15.78456841880229078 ) ) ;
#35108 = CARTESIAN_POINT ( 'NONE',  ( 142.9884853222707477, 243.3615022471901739, 5.000000000000051514 ) ) ;
#35109 = CARTESIAN_POINT ( 'NONE',  ( 192.1396999271463812, 297.8512729055811974, 12.32430960859512403 ) ) ;
#35110 = FACE_OUTER_BOUND ( 'NONE', #8683, .T. ) ;
#35111 = CARTESIAN_POINT ( 'NONE',  ( 159.1219488725454028, 255.0396952838110849, -16.66430026305668122 ) ) ;
#35112 = ORIENTED_EDGE ( 'NONE', *, *, #46783, .F. ) ;
#35113 = CARTESIAN_POINT ( 'NONE',  ( 78.11054252755917560, 56.59592749652284027, -16.20240047345659207 ) ) ;
#35114 = AXIS2_PLACEMENT_3D ( 'NONE', #55275, #2111, #24892 ) ;
#35115 = CARTESIAN_POINT ( 'NONE',  ( 206.5479446040613141, 272.8954610772809133, 10.74757481123993230 ) ) ;
#35117 = CARTESIAN_POINT ( 'NONE',  ( 206.5571822944673670, 272.8794609281530938, 10.95833005210827515 ) ) ;
#35116 = CARTESIAN_POINT ( 'NONE',  ( 77.50559704200234989, 49.73895437837127531, -15.47469949631416952 ) ) ;
#35118 = CARTESIAN_POINT ( 'NONE',  ( 84.49887340489608789, 41.63797158674129406, -1.523898730005905255 ) ) ;
#35119 = AXIS2_PLACEMENT_3D ( 'NONE', #15254, #76110, #77068 ) ;
#35120 = ORIENTED_EDGE ( 'NONE', *, *, #46920, .F. ) ;
#35121 = CARTESIAN_POINT ( 'NONE',  ( 187.6284309019235366, 277.1362090929395663, 17.09713795014519988 ) ) ;
#35122 = CARTESIAN_POINT ( 'NONE',  ( 69.95523204135938045, 62.90150226501648234, 13.86126985460704297 ) ) ;
#35123 = ADVANCED_FACE ( 'NONE', ( #62380 ), #23891, .F. ) ;
#35124 = DIRECTION ( 'NONE',  ( 0.4999999999999992784, -0.8660254037844390407, 0.000000000000000000 ) ) ;
#35125 = CARTESIAN_POINT ( 'NONE',  ( 46.30674614090290220, 112.4688969640381231, -10.00000000000000000 ) ) ;
#35126 = CARTESIAN_POINT ( 'NONE',  ( 160.4256652780435672, 252.7815922308273002, -16.16855709575365552 ) ) ;
#35127 = CARTESIAN_POINT ( 'NONE',  ( 190.3940121281077893, 300.8748928676694163, 0.04809511090732299099 ) ) ;
#35128 = VERTEX_POINT ( 'NONE', #93337 ) ;
#35129 = DIRECTION ( 'NONE',  ( -0.4848096202463351156, -0.8746197071393968514, 1.049727191138617217E-16 ) ) ;
#35130 = VECTOR ( 'NONE', #95370, 1000.000000000000114 ) ;
#35131 = DIRECTION ( 'NONE',  ( 1.000000000000000000, 0.000000000000000000, 0.000000000000000000 ) ) ;
#35132 = CARTESIAN_POINT ( 'NONE',  ( 123.3201800421238090, 253.5530062829863311, -4.648177544792955347E-16 ) ) ;
#35133 = CARTESIAN_POINT ( 'NONE',  ( 207.6508796976096107, 270.9851214578045528, 6.713685698622268383 ) ) ;
#35134 = CARTESIAN_POINT ( 'NONE',  ( 29.01593374150816729, 200.8927522451419634, 2.944929066748280225E-16 ) ) ;
#35135 = CARTESIAN_POINT ( 'NONE',  ( 107.7251869580316281, 226.8768266524160140, 9.188101187500096856 ) ) ;
#35136 = CARTESIAN_POINT ( 'NONE',  ( 181.9644534062184107, 294.8608557540333663, -2.655205150443219697 ) ) ;
#35137 = CARTESIAN_POINT ( 'NONE',  ( 164.2913008600799287, 280.3343451829814512, -11.31047592362255827 ) ) ;
#35138 = CARTESIAN_POINT ( 'NONE',  ( 72.56680254073344827, 71.38637538794351656, 5.777867564336608197 ) ) ;
#35139 = CARTESIAN_POINT ( 'NONE',  ( 163.1611253217825492, 248.0436364529968216, 11.42797785440508029 ) ) ;
#35140 = CARTESIAN_POINT ( 'NONE',  ( 24.31594170816038059, 184.8458772461660544, 9.188101187500095079 ) ) ;
#35141 = LINE ( 'NONE', #87927, #88371 ) ;
#35142 = ORIENTED_EDGE ( 'NONE', *, *, #17605, .T. ) ;
#35143 = VECTOR ( 'NONE', #16195, 1000.000000000000000 ) ;
#35144 = B_SPLINE_CURVE_WITH_KNOTS ( 'NONE', 3,
 ( #74866, #21643, #12560, #66250, #89598, #52042 ),
 .UNSPECIFIED., .F., .F.,
 ( 4, 2, 4 ),
 ( 8.689474584194192324E-15, 0.0005080340594498560436, 0.001016068118891022640 ),
 .UNSPECIFIED. ) ;
#35145 = EDGE_LOOP ( 'NONE', ( #30371, #55936, #23034, #46145 ) ) ;
#35146 = CARTESIAN_POINT ( 'NONE',  ( -46.35039662390602899, 28.35603213498495023, 177.5919119679930134 ) ) ;
#35147 = CARTESIAN_POINT ( 'NONE',  ( 185.2951076684100258, 260.0657642104216052, -5.799074855275172524 ) ) ;
#35148 = CARTESIAN_POINT ( 'NONE',  ( -35.27139336136212933, 24.82964151130202879, -10.00000000000000000 ) ) ;
#35149 = CARTESIAN_POINT ( 'NONE',  ( 193.5052912260503888, 264.1446421622504204, -4.343934653911574628 ) ) ;
#35150 = ADVANCED_FACE ( 'NONE', ( #30996 ), #32998, .T. ) ;
#35151 = CARTESIAN_POINT ( 'NONE',  ( 207.8232941427535536, 270.6864908788566026, -6.505149060073906142 ) ) ;
#35152 = FACE_OUTER_BOUND ( 'NONE', #22101, .T. ) ;
#35153 = CARTESIAN_POINT ( 'NONE',  ( 84.60735463175657856, 50.53152741511170376, -13.60229262012000184 ) ) ;
#35154 = VECTOR ( 'NONE', #91513, 1000.000000000000000 ) ;
#35155 = CARTESIAN_POINT ( 'NONE',  ( 51.75829523846230273, 194.5643266524159856, -9.188101187500093303 ) ) ;
#35156 = CARTESIAN_POINT ( 'NONE',  ( 95.69988983291003137, 219.3927522451418213, 10.00000000000009592 ) ) ;
#35157 = VERTEX_POINT ( 'NONE', #54792 ) ;
#35158 = EDGE_CURVE ( 'NONE', #8078, #97948, #8208, .T. ) ;
#35159 = CARTESIAN_POINT ( 'NONE',  ( 180.4572463832561482, 261.7460625851787199, -13.63662180976220384 ) ) ;
#35160 = CARTESIAN_POINT ( 'NONE',  ( 178.8233793429807008, 259.2497683303841995, -10.29503125857851131 ) ) ;
#35161 = CARTESIAN_POINT ( 'NONE',  ( -9.892408837089961438, 177.3464784336661637, 1.353441290958777327E-15 ) ) ;
#35162 = CARTESIAN_POINT ( 'NONE',  ( 68.53472279406327061, 64.53069240858096123, -12.19966557917646988 ) ) ;
#35163 = CARTESIAN_POINT ( 'NONE',  ( 151.2646864780760723, 268.6488729594320830, -14.38346604407754548 ) ) ;
#35164 = LINE ( 'NONE', #74694, #82397 ) ;
#35165 = CARTESIAN_POINT ( 'NONE',  ( 192.5143468344189728, 297.2023654272867361, -12.06830393602581530 ) ) ;
#35166 = CARTESIAN_POINT ( 'NONE',  ( 194.9499559406243918, 279.5747724307917679, 17.51673600049429780 ) ) ;
#35167 = CARTESIAN_POINT ( 'NONE',  ( 164.4936379324916516, 245.7356569095223051, 6.719479797016231437 ) ) ;
#35168 = CARTESIAN_POINT ( 'NONE',  ( 70.82736078104210264, 70.74693773775240402, 4.782910273999081419 ) ) ;
#35169 = CARTESIAN_POINT ( 'NONE',  ( 164.6649740431187183, 245.4388940607451843, -1.430729255012818557 ) ) ;
#35170 = ORIENTED_EDGE ( 'NONE', *, *, #55441, .F. ) ;
#35171 = CARTESIAN_POINT ( 'NONE',  ( 165.1672732435949342, 269.2213042464348405, 17.45144253968057413 ) ) ;
#35172 = CARTESIAN_POINT ( 'NONE',  ( -3.369807917299440181, 168.8615022471902591, -10.00000000000009592 ) ) ;
#35173 = FACE_OUTER_BOUND ( 'NONE', #68124, .T. ) ;
#35174 = CARTESIAN_POINT ( 'NONE',  ( 130.3772506997096343, 236.8923013555409796, 4.594050593750050204 ) ) ;
#35175 = CARTESIAN_POINT ( 'NONE',  ( 24.28581821943125263, 16.94754757982090254, 5.678558825948272215 ) ) ;
#35177 = CARTESIAN_POINT ( 'NONE',  ( 74.68693990639053482, 67.13232622275778283, 12.47216552256462840 ) ) ;
#35176 = B_SPLINE_CURVE_WITH_KNOTS ( 'NONE', 3,
 ( #70360, #31848, #79514, #69858 ),
 .UNSPECIFIED., .F., .F.,
 ( 4, 4 ),
 ( 0.03943544382253093283, 0.04790621245170952752 ),
 .UNSPECIFIED. ) ;
#35178 = DIRECTION ( 'NONE',  ( -0.6681572590663601430, 0.7440200784635646603, 0.000000000000000000 ) ) ;
#35180 = CARTESIAN_POINT ( 'NONE',  ( 74.64154962151783934, 66.95428888261444911, 13.01658699031521671 ) ) ;
#35179 = CARTESIAN_POINT ( 'NONE',  ( 196.1573359623355088, 290.8925231663144473, 17.55680092534192482 ) ) ;
#35181 = CARTESIAN_POINT ( 'NONE',  ( 21.57298720112008894, 14.58380873178786885, 6.180339887498953466 ) ) ;
#35182 = ORIENTED_EDGE ( 'NONE', *, *, #5954, .F. ) ;
#35183 = CARTESIAN_POINT ( 'NONE',  ( 151.4384131719918685, 268.3479694989391078, 14.98299707687648841 ) ) ;
#35184 = CARTESIAN_POINT ( 'NONE',  ( 208.2268492240826561, 269.9875129743418256, -0.3614433915064274583 ) ) ;
#35185 = AXIS2_PLACEMENT_3D ( 'NONE', #53322, #91366, #84769 ) ;
#35186 = CARTESIAN_POINT ( 'NONE',  ( 105.0000000000000142, 93.06504152958497400, 54.99999999999999289 ) ) ;
#35187 = CARTESIAN_POINT ( 'NONE',  ( 172.6634619271783038, 267.9388633272891980, -16.30849192416249238 ) ) ;
#35188 = CARTESIAN_POINT ( 'NONE',  ( 81.68367041701041842, 55.79078710209740422, -16.00088945688137443 ) ) ;
#35189 = VERTEX_POINT ( 'NONE', #63403 ) ;
#35190 = CARTESIAN_POINT ( 'NONE',  ( 69.51993594036143520, 67.94519450850054909, 8.515667477277720110 ) ) ;
#35191 = CARTESIAN_POINT ( 'NONE',  ( 166.0350694293928768, 270.1027909330327930, -16.28260794856732119 ) ) ;
#35192 = CARTESIAN_POINT ( 'NONE',  ( 71.76139268086217271, 72.52520824035065061, 0.9833505332507517238 ) ) ;
#35193 = B_SPLINE_SURFACE_WITH_KNOTS ( 'NONE', 3, 1, ( 
 ( #1260, #32142 ),
 ( #47343, #25560 ),
 ( #62529, #746 ),
 ( #254, #32650 ),
 ( #93994, #17452 ),
 ( #46851, #92978 ),
 ( #48360, #78767 ),
 ( #31135, #24544 ),
 ( #8358, #39226 ),
 ( #2272, #94996 ),
 ( #94488, #16942 ),
 ( #55424, #31630 ),
 ( #56447, #16446 ),
 ( #93490, #86413 ),
 ( #70134, #54944 ),
 ( #17973, #24048 ),
 ( #9354, #85920 ),
 ( #40232, #71175 ),
 ( #47830, #79309 ),
 ( #78267, #87441 ),
 ( #8848, #70645 ),
 ( #40735, #23532 ),
 ( #69646, #1771 ),
 ( #62028, #25047 ),
 ( #71680, #77253 ),
 ( #7860, #54423 ),
 ( #85400, #38741 ),
 ( #97474, #57440 ),
 ( #64560, #89410 ),
 ( #27569, #18977 ),
 ( #58916, #96004 ),
 ( #48868, #89886 ),
 ( #95519, #42237 ),
 ( #10867, #88418 ) ),
 .UNSPECIFIED., .T., .F., .F.,
 ( 4, 2, 2, 2, 2, 2, 2, 2, 2, 2, 2, 2, 2, 2, 2, 2, 4 ),
 ( 2, 2 ),
 ( 0.000000000000000000, 0.06250000000000000000, 0.1250000000000000000, 0.1875000000000000000, 0.2500000000000000000, 0.3125000000000000000, 0.3750000000000000000, 0.4375000000000000000, 0.5000000000000000000, 0.5625000000000000000, 0.6250000000000000000, 0.6875000000000000000, 0.7500000000000000000, 0.8125000000000000000, 0.8750000000000000000, 0.9375000000000000000, 1.000000000000000000 ),
 ( 0.000000000000000000, 1.000000000000000000 ),
 .UNSPECIFIED. ) ;
#35194 = ADVANCED_FACE ( 'NONE', ( #31989 ), #69028, .F. ) ;
#35195 = DIRECTION ( 'NONE',  ( 0.4145187862775202015, -0.7179675985244525771, -0.5591929034707450175 ) ) ;
#35196 = CARTESIAN_POINT ( 'NONE',  ( 199.6745771582872351, 272.3907837538676517, 12.39460699429984203 ) ) ;
#35197 = CARTESIAN_POINT ( 'NONE',  ( 185.8859980584196023, 296.7027117258024873, 4.750670030249517950 ) ) ;
#35198 = ADVANCED_FACE ( 'NONE', ( #18812 ), #49697, .T. ) ;
#35199 = CARTESIAN_POINT ( 'NONE',  ( 72.23468229527969697, 71.59820328793978206, -5.860928441596811922 ) ) ;
#35200 = CARTESIAN_POINT ( 'NONE',  ( 148.6183282077989816, 273.6856180928681397, -8.486299949745918170 ) ) ;
#35201 = ORIENTED_EDGE ( 'NONE', *, *, #41154, .F. ) ;
#35202 = CARTESIAN_POINT ( 'NONE',  ( 157.5670606312586415, 279.0380996213595495, -9.710625198711769102 ) ) ;
#35203 = EDGE_CURVE ( 'NONE', #22789, #95233, #97324, .T. ) ;
#35204 = CARTESIAN_POINT ( 'NONE',  ( 8.129038565245441106, 16.64441083166258650, -10.00000000000000533 ) ) ;
#35205 = CARTESIAN_POINT ( 'NONE',  ( 89.99855592466245469, 222.7677522451418781, 10.00000000000009592 ) ) ;
#35206 = EDGE_LOOP ( 'NONE', ( #16827, #63009, #90470, #35933 ) ) ;
#35207 = CYLINDRICAL_SURFACE ( 'NONE', #99927, 10.00000000000001066 ) ;
#35208 = EDGE_CURVE ( 'NONE', #79294, #49558, #74675, .T. ) ;
#35209 = CARTESIAN_POINT ( 'NONE',  ( 194.3177355571849318, 294.0788045336591381, -15.93712594727561616 ) ) ;
#35210 = CARTESIAN_POINT ( 'NONE',  ( -31.49356256989596758, 94.88921800892812541, 43.89948692389422291 ) ) ;
#35211 = VERTEX_POINT ( 'NONE', #76500 ) ;
#35212 = CARTESIAN_POINT ( 'NONE',  ( 78.78511898078654951, 60.03407184738823332, 16.11193227242592840 ) ) ;
#35213 = CARTESIAN_POINT ( 'NONE',  ( 79.14312167556931854, 57.64441083166269664, 0.000000000000000000 ) ) ;
#35214 = AXIS2_PLACEMENT_3D ( 'NONE', #65732, #81488, #68222 ) ;
#35215 = CARTESIAN_POINT ( 'NONE',  ( 58.25437508341968851, 192.8932355074535678, -2.679491924311248496 ) ) ;
#35216 = ORIENTED_EDGE ( 'NONE', *, *, #92683, .T. ) ;
#35217 = CARTESIAN_POINT ( 'NONE',  ( 78.44218234892279895, 228.3464784336661637, 1.353441290958777525E-15 ) ) ;
#35218 = CARTESIAN_POINT ( 'NONE',  ( 81.38866437292413991, 50.91805390661637176, -14.64230100137327284 ) ) ;
#35219 = VECTOR ( 'NONE', #28375, 1000.000000000000000 ) ;
#35220 = CARTESIAN_POINT ( 'NONE',  ( 84.63506747414010079, 49.80695396426073529, -13.18143026763655534 ) ) ;
#35221 = DIRECTION ( 'NONE',  ( 0.4999999999999998890, -0.8660254037844385966, 0.000000000000000000 ) ) ;
#35222 = ORIENTED_EDGE ( 'NONE', *, *, #20105, .T. ) ;
#35223 = ORIENTED_EDGE ( 'NONE', *, *, #39155, .T. ) ;
#35224 = CARTESIAN_POINT ( 'NONE',  ( -3.194846457709630272, 157.4155109091896350, 2.679491924311251605 ) ) ;
#35225 = VERTEX_POINT ( 'NONE', #84623 ) ;
#35226 = CARTESIAN_POINT ( 'NONE',  ( 78.14015596324891533, 47.79605781560269406, 14.53813849190288465 ) ) ;
#35227 = ORIENTED_EDGE ( 'NONE', *, *, #91067, .F. ) ;
#35228 = CARTESIAN_POINT ( 'NONE',  ( 75.03406391020887156, 58.89278341677606221, 15.85403548772932503 ) ) ;
#35229 = CARTESIAN_POINT ( 'NONE',  ( 202.7754741559590173, 279.4295715634463022, -15.65855077192107636 ) ) ;
#35230 = EDGE_LOOP ( 'NONE', ( #73782, #50165, #30706, #96332 ) ) ;
#35231 = CARTESIAN_POINT ( 'NONE',  ( 182.9704806738767786, 279.7017868584060238, -16.88939609177110412 ) ) ;
#35232 = AXIS2_PLACEMENT_3D ( 'NONE', #5897, #28701, #29695 ) ;
#35233 = CARTESIAN_POINT ( 'NONE',  ( 81.90650872946123684, 41.09198023048384840, 3.645612064814079734 ) ) ;
#35234 = CARTESIAN_POINT ( 'NONE',  ( 151.8835309833198153, 268.6765239516433894, 14.96763668012306248 ) ) ;
#35235 = FACE_OUTER_BOUND ( 'NONE', #30868, .T. ) ;
#35236 = DIRECTION ( 'NONE',  ( 0.000000000000000000, -0.000000000000000000, -1.000000000000000000 ) ) ;
#35237 = CARTESIAN_POINT ( 'NONE',  ( 72.50222618693952370, 68.22314101123330943, -10.37516697382647024 ) ) ;
#35238 = CARTESIAN_POINT ( 'NONE',  ( 137.3322569020296555, 250.0958772461660544, -9.188101187500095079 ) ) ;
#35239 = CARTESIAN_POINT ( 'NONE',  ( 168.0351016175754637, 267.0074190867483708, -17.62211840267826091 ) ) ;
#35240 = CARTESIAN_POINT ( 'NONE',  ( 75.80125281519391933, 55.32059395707344152, 16.14277639286700605 ) ) ;
#35241 = CARTESIAN_POINT ( 'NONE',  ( 14.28983037092611319, 10.11110640527290627, -2.839279412974138328 ) ) ;
#35242 = ORIENTED_EDGE ( 'NONE', *, *, #62968, .T. ) ;
#35243 = CARTESIAN_POINT ( 'NONE',  ( 164.0398389372132044, 281.8052652109336691, 8.614039144221564470 ) ) ;
#35245 = VERTEX_POINT ( 'NONE', #51707 ) ;
#35244 = CARTESIAN_POINT ( 'NONE',  ( 85.39636071719610300, 48.32640963909398124, -12.26545443191636586 ) ) ;
#35246 = CARTESIAN_POINT ( 'NONE',  ( -14.72174178882247908, 105.5588735921874672, 10.69508629217443207 ) ) ;
#35247 = CARTESIAN_POINT ( 'NONE',  ( 78.38215086339779702, 48.00876806938738639, -14.02649451357657995 ) ) ;
#35248 = FACE_OUTER_BOUND ( 'NONE', #37631, .T. ) ;
#35249 = CARTESIAN_POINT ( 'NONE',  ( 156.4050736080099000, 278.8659540353394846, 7.272296007666364304 ) ) ;
#35250 = LINE ( 'NONE', #35751, #65852 ) ;
#35251 = DIRECTION ( 'NONE',  ( 0.000000000000000000, 0.000000000000000000, 1.000000000000000000 ) ) ;
#35252 = CARTESIAN_POINT ( 'NONE',  ( 85.20757786915602594, 42.65106006787098636, 2.242368550657015902 ) ) ;
#35253 = CARTESIAN_POINT ( 'NONE',  ( 88.14497077207560949, 43.82233299356100531, -2.120619512623201253 ) ) ;
#35254 = ORIENTED_EDGE ( 'NONE', *, *, #14414, .T. ) ;
#35255 = CARTESIAN_POINT ( 'NONE',  ( 185.1243922746118074, 273.1384459838623116, -16.79753314444298695 ) ) ;
#35256 = CARTESIAN_POINT ( 'NONE',  ( 66.07714878694351057, 69.27459742504910878, 0.2655349905647865771 ) ) ;
#35257 = ORIENTED_EDGE ( 'NONE', *, *, #39262, .F. ) ;
#35258 = CIRCLE ( 'NONE', #40076, 12.50000000000000000 ) ;
#35259 = CARTESIAN_POINT ( 'NONE',  ( 194.3452430042056847, 293.4673175397701357, -14.50972866970454866 ) ) ;
#35260 = CARTESIAN_POINT ( 'NONE',  ( 201.2772264434572946, 267.1716386788893942, -2.196353493170192905 ) ) ;
#35261 = PLANE ( 'NONE',  #98411 ) ;
#35262 = CARTESIAN_POINT ( 'NONE',  ( 80.32560484147226987, 44.93948968179056180, -11.21518412823304800 ) ) ;
#35264 = ADVANCED_FACE ( 'NONE', ( #82655 ), #77988, .T. ) ;
#35263 = AXIS2_PLACEMENT_3D ( 'NONE', #89653, #51086, #20715 ) ;
#35265 = DIRECTION ( 'NONE',  ( 0.3595896960900473172, 0.9331105242498700658, 0.000000000000000000 ) ) ;
#35267 = CARTESIAN_POINT ( 'NONE',  ( 88.47364309043327069, 44.01569472767099001, 2.145854971186514693 ) ) ;
#35266 = CARTESIAN_POINT ( 'NONE',  ( 161.4322953877310738, 281.4157690633189759, -6.765754283059072449 ) ) ;
#35268 = CARTESIAN_POINT ( 'NONE',  ( 203.3726069110276740, 270.0503998713792839, 5.990016924711733637 ) ) ;
#35269 = ORIENTED_EDGE ( 'NONE', *, *, #42370, .F. ) ;
#35270 = VECTOR ( 'NONE', #41821, 1000.000000000000114 ) ;
#35271 = ORIENTED_EDGE ( 'NONE', *, *, #39279, .F. ) ;
#35272 = CARTESIAN_POINT ( 'NONE',  ( -14.83894680564148238, 24.48641780169620219, -10.00000000000000000 ) ) ;
#35273 = CARTESIAN_POINT ( 'NONE',  ( 80.56697878876413199, 57.58860379435336796, 16.23401761274853428 ) ) ;
#35274 = CARTESIAN_POINT ( 'NONE',  ( 70.71537437633379852, 66.12099867655061303, -11.31749738359454760 ) ) ;
#35275 = CARTESIAN_POINT ( 'NONE',  ( -19.65312891409030271, 93.06504152958497400, -10.00000000000000888 ) ) ;
#35276 = CARTESIAN_POINT ( 'NONE',  ( 152.7153488183568300, 266.1362520814392951, 17.33540622643059237 ) ) ;
#35277 = AXIS2_PLACEMENT_3D ( 'NONE', #27322, #48109, #72443 ) ;
#35278 = CARTESIAN_POINT ( 'NONE',  ( 81.11567069824683074, 43.42565969520126856, -9.945124925201680455 ) ) ;
#35279 = CARTESIAN_POINT ( 'NONE',  ( 52.94219725692860834, 189.8262482093458061, 3.021315404115420679E-15 ) ) ;
#35280 = CARTESIAN_POINT ( 'NONE',  ( -0.9884983804899494242, 179.4244531367911577, -4.594050593750046652 ) ) ;
#35281 = CARTESIAN_POINT ( 'NONE',  ( 93.70588009062352342, 237.1589784336661637, -6.496448406907675876E-16 ) ) ;
#35282 = CARTESIAN_POINT ( 'NONE',  ( 87.70182765261645841, 44.38038868594539110, -4.004158056545790600 ) ) ;
#35283 = CARTESIAN_POINT ( 'NONE',  ( 186.3805910356028619, 295.6218943418388108, -7.683998803325324367 ) ) ;
#35284 = CARTESIAN_POINT ( 'NONE',  ( 79.14312167556931854, 57.64441083166269664, 0.000000000000000000 ) ) ;
#35285 = VECTOR ( 'NONE', #28401, 1000.000000000000000 ) ;
#35286 = CARTESIAN_POINT ( 'NONE',  ( 170.4623819437503016, 288.8056674672355939, -5.476885062779371260 ) ) ;
#35287 = CARTESIAN_POINT ( 'NONE',  ( 160.7713118735465230, 281.8391587724178748, 5.260302810648785687 ) ) ;
#35288 = CARTESIAN_POINT ( 'NONE',  ( 148.3253847707240141, 273.7398928553401447, -9.074433450356286457 ) ) ;
#35289 = CARTESIAN_POINT ( 'NONE',  ( 71.86256228778262312, 72.60615528678950170, -0.5650332253009007211 ) ) ;
#35290 = CARTESIAN_POINT ( 'NONE',  ( 84.66363459063573771, 50.58495542193022487, 13.62716051735802836 ) ) ;
#35291 = DIRECTION ( 'NONE',  ( 0.4999999999999992784, -0.8660254037844390407, 0.000000000000000000 ) ) ;
#35292 = CARTESIAN_POINT ( 'NONE',  ( 80.63310098719156827, 53.50240974728008325, -16.03299162280124435 ) ) ;
#35293 = AXIS2_PLACEMENT_3D ( 'NONE', #89239, #65370, #57759 ) ;
#35294 = CARTESIAN_POINT ( 'NONE',  ( -19.59289307225702714, 92.93664611688882360, 59.99999999999999289 ) ) ;
#35295 = CARTESIAN_POINT ( 'NONE',  ( 84.04489159724214176, 210.1423013555409796, -4.594050593750043987 ) ) ;
#35296 = CARTESIAN_POINT ( 'NONE',  ( 207.4218731373931632, 271.3817724553659332, -5.249531240730909154 ) ) ;
#35297 = DIRECTION ( 'NONE',  ( 0.5000000000000002220, -0.8660254037844384856, 0.000000000000000000 ) ) ;
#35298 = CARTESIAN_POINT ( 'NONE',  ( -15.49448615033923815, 102.7791273954868672, 12.38876935695490822 ) ) ;
#35300 = CARTESIAN_POINT ( 'NONE',  ( 200.0565326084237938, 284.1389164665869771, 16.92133041920757108 ) ) ;
#35299 = CARTESIAN_POINT ( 'NONE',  ( 195.8947060313465443, 291.3474115503753410, 16.07878593000791767 ) ) ;
#35301 = CARTESIAN_POINT ( 'NONE',  ( 150.9003228897357189, 269.2799692068659283, -14.30003212299500781 ) ) ;
#35302 = CARTESIAN_POINT ( 'NONE',  ( 173.5129947698212334, 267.4886862244790109, -17.45415247818019111 ) ) ;
#35303 = CARTESIAN_POINT ( 'NONE',  ( 36.84800447571193160, 26.98920272979929180, 7.433330006724137462 ) ) ;
#35304 = CARTESIAN_POINT ( 'NONE',  ( 147.1603453755519695, 275.7578002805973370, -5.230822882238410187 ) ) ;
#35305 = DIRECTION ( 'NONE',  ( -1.000000000000000000, 0.000000000000000000, 0.000000000000000000 ) ) ;
#35306 = VERTEX_POINT ( 'NONE', #47080 ) ;
#35307 = CARTESIAN_POINT ( 'NONE',  ( 25.00689474275853286, 16.29860640527292759, -2.839279412974138328 ) ) ;
#35308 = CARTESIAN_POINT ( 'NONE',  ( -110.0000000000000142, 10.00000000000000178, -14.21260523776211926 ) ) ;
#35309 = CARTESIAN_POINT ( 'NONE',  ( -19.65312891409030271, 93.06504152958497400, -10.00000000000000888 ) ) ;
#35310 = CARTESIAN_POINT ( 'NONE',  ( 189.7011281277219439, 286.7593913854856282, -15.88714824190844155 ) ) ;
#35311 = VERTEX_POINT ( 'NONE', #86152 ) ;
#35312 = CARTESIAN_POINT ( 'NONE',  ( 86.12260107077111115, 47.06852444819536885, 10.76136662946663947 ) ) ;
#35313 = CARTESIAN_POINT ( 'NONE',  ( -61.78156952962572035, 53.28125210322373562, 59.99999999999999289 ) ) ;
#35314 = EDGE_CURVE ( 'NONE', #98353, #65113, #51956, .T. ) ;
#35315 = CARTESIAN_POINT ( 'NONE',  ( 205.8099205723994203, 269.1131406545866298, -1.356034389334280776 ) ) ;
#35316 = CARTESIAN_POINT ( 'NONE',  ( 139.5243837071329267, 251.3615022471902307, -10.00000000000009592 ) ) ;
#35317 = CARTESIAN_POINT ( 'NONE',  ( 205.3943609285979051, 274.8935266139653777, -13.14270440534009943 ) ) ;
#35318 = CARTESIAN_POINT ( 'NONE',  ( 22.17949989257922283, 28.50829794293881037, -10.00000000000000355 ) ) ;
#35319 = VERTEX_POINT ( 'NONE', #64671 ) ;
#35320 = CIRCLE ( 'NONE', #4596, 70.00000000000001421 ) ;
#35321 = CARTESIAN_POINT ( 'NONE',  ( 85.80882896958009098, 47.30052720894016716, 10.64875693516724908 ) ) ;
#35322 = ORIENTED_EDGE ( 'NONE', *, *, #86050, .T. ) ;
#35323 = CARTESIAN_POINT ( 'NONE',  ( 197.0063477221338815, 265.1879394709707753, -4.577846407058970613 ) ) ;
#35324 = CARTESIAN_POINT ( 'NONE',  ( 84.79859407451725417, 42.50768657221069446, 2.813679082869662285 ) ) ;
#35325 = EDGE_CURVE ( 'NONE', #6085, #13462, #23269, .T. ) ;
#35326 = ORIENTED_EDGE ( 'NONE', *, *, #38266, .T. ) ;
#35327 = LINE ( 'NONE', #88103, #85578 ) ;
#35328 = ORIENTED_EDGE ( 'NONE', *, *, #58199, .F. ) ;
#35329 = AXIS2_PLACEMENT_3D ( 'NONE', #45146, #6659, #37536 ) ;
#35330 = CARTESIAN_POINT ( 'NONE',  ( 189.2647483391328933, 290.1520017563908596, 14.35190764732333690 ) ) ;
#35331 = CARTESIAN_POINT ( 'NONE',  ( -22.42236680055709641, 157.8615022471902591, 0.000000000000000000 ) ) ;
#35332 = CARTESIAN_POINT ( 'NONE',  ( 157.5052804517226264, 258.3460506454662777, -16.81904061521691673 ) ) ;
#35333 = CARTESIAN_POINT ( 'NONE',  ( 87.79556561918005286, 44.17086485108952587, -4.468589225908877971 ) ) ;
#35334 = DIRECTION ( 'NONE',  ( 1.000000000000000000, 0.000000000000000000, 0.000000000000000000 ) ) ;
#35335 = CIRCLE ( 'NONE', #25579, 60.00000000000002132 ) ;
#35336 = CIRCLE ( 'NONE', #77357, 70.00000000000001421 ) ;
#35337 = CARTESIAN_POINT ( 'NONE',  ( 35.92184506804998279, 29.24335787977765833, -9.188101187500008038 ) ) ;
#35338 = LINE ( 'NONE', #12056, #55883 ) ;
#35339 = DIRECTION ( 'NONE',  ( -0.9994538543569189137, 0.03304531753666254540, 0.000000000000000000 ) ) ;
#35340 = B_SPLINE_CURVE_WITH_KNOTS ( 'NONE', 3,
 ( #98735, #89660, #42982, #83546, #36898, #43985, #90663, #82564 ),
 .UNSPECIFIED., .F., .F.,
 ( 4, 2, 2, 4 ),
 ( 0.002053660639095798539, 0.002297581679447361584, 0.002541502719798924628, 0.003029344800502051585 ),
 .UNSPECIFIED. ) ;
#35341 = LINE ( 'NONE', #90084, #17327 ) ;
#35342 = ORIENTED_EDGE ( 'NONE', *, *, #98217, .T. ) ;
#35343 = VERTEX_POINT ( 'NONE', #23773 ) ;
#35344 = CARTESIAN_POINT ( 'NONE',  ( 81.09996276884294275, 42.55047014966801555, 7.932854448062508723 ) ) ;
#35345 = AXIS2_PLACEMENT_3D ( 'NONE', #75123, #40815, #95090 ) ;
#35347 = CARTESIAN_POINT ( 'NONE',  ( 164.6886454784808222, 273.3769192494668232, -15.25705676796773780 ) ) ;
#35346 = CARTESIAN_POINT ( 'NONE',  ( 68.35453417343933324, 65.67399229982113695, 10.37910612949749023 ) ) ;
#35348 = CARTESIAN_POINT ( 'NONE',  ( 165.3552783545318050, 246.2432519206945472, 4.078954813822171843 ) ) ;
#35349 = CARTESIAN_POINT ( 'NONE',  ( 193.9204722154232741, 294.7668848255750049, 15.43855698596013859 ) ) ;
#35350 = CARTESIAN_POINT ( 'NONE',  ( 126.3716228836088646, 243.7677522451418497, 10.00000000000009592 ) ) ;
#35351 = LINE ( 'NONE', #41445, #24207 ) ;
#35352 = CARTESIAN_POINT ( 'NONE',  ( 164.3666959528347320, 245.9555268679014830, 4.217718140385406933 ) ) ;
#35353 = CARTESIAN_POINT ( 'NONE',  ( -8.240413327673026700, 41.28378578775782159, 59.99999999999999289 ) ) ;
#35354 = CARTESIAN_POINT ( 'NONE',  ( 181.1216305184527471, 255.7546495805296161, 5.273460715939602750 ) ) ;
#35355 = CARTESIAN_POINT ( 'NONE',  ( 99.38934535084139554, 234.3149278399160949, 9.188101187500093303 ) ) ;
#35356 = VERTEX_POINT ( 'NONE', #79903 ) ;
#35357 = CARTESIAN_POINT ( 'NONE',  ( 73.73249371147525721, 55.30366856558931232, -16.59341848673177111 ) ) ;
#35358 = FACE_OUTER_BOUND ( 'NONE', #24447, .T. ) ;
#35359 = CARTESIAN_POINT ( 'NONE',  ( 166.6551839283834227, 278.1147546280273559, -13.36279048790327728 ) ) ;
#35360 = ORIENTED_EDGE ( 'NONE', *, *, #78472, .T. ) ;
#35361 = ORIENTED_EDGE ( 'NONE', *, *, #56548, .T. ) ;
#35362 = CARTESIAN_POINT ( 'NONE',  ( 87.04122873496829982, 46.31593380912286051, -9.298662157179396814 ) ) ;
#35363 = CARTESIAN_POINT ( 'NONE',  ( 176.9775198831545708, 292.4513829097897428, -2.718792113259059562 ) ) ;
#35364 = CARTESIAN_POINT ( 'NONE',  ( 157.2168982216852555, 258.3393398020932636, 18.09635675623264106 ) ) ;
#35365 = CARTESIAN_POINT ( 'NONE',  ( 47.97596991287763757, 210.0530062829863027, 1.101618078115930403E-13 ) ) ;
#35366 = CARTESIAN_POINT ( 'NONE',  ( 208.2512496840233496, 269.9452501379965952, 1.821023623773176947 ) ) ;
#35367 = ORIENTED_EDGE ( 'NONE', *, *, #40469, .T. ) ;
#35368 = DIRECTION ( 'NONE',  ( -0.9662637919863231728, -0.2575544297740022248, 0.000000000000000000 ) ) ;
#35369 = CARTESIAN_POINT ( 'NONE',  ( 163.4222916751007801, 247.5912830598222172, -10.52132777929285012 ) ) ;
#35370 = EDGE_LOOP ( 'NONE', ( #7918, #54106, #79016, #69605, #63955, #36591, #7735, #88459, #67846, #2234, #49322, #27021, #66629, #63124, #19892, #17998, #85066, #41691, #14181, #93705, #23370, #43214 ) ) ;
#35371 = CARTESIAN_POINT ( 'NONE',  ( 194.6938575426807745, 266.4053782337838356, -7.878287061657681889 ) ) ;
#35372 = CARTESIAN_POINT ( 'NONE',  ( 24.24733352825768407, 173.2592609112379876, 2.679491924311254714 ) ) ;
#35374 = ADVANCED_FACE ( 'NONE', ( #95620 ), #41851, .T. ) ;
#35373 = VECTOR ( 'NONE', #3893, 1000.000000000000000 ) ;
#35375 = CARTESIAN_POINT ( 'NONE',  ( 83.05052185759683425, 46.42945747414138680, 11.22551205484409564 ) ) ;
#35377 = CARTESIAN_POINT ( 'NONE',  ( 199.6189824786654299, 284.3965447663834425, 17.01103535422801727 ) ) ;
#35376 = CARTESIAN_POINT ( 'NONE',  ( 133.7059490715648167, 241.8768266524159856, 9.188101187500098632 ) ) ;
#35378 = CARTESIAN_POINT ( 'NONE',  ( -17.42236680055705023, 149.2012482093457777, 0.000000000000000000 ) ) ;
#35379 = ORIENTED_EDGE ( 'NONE', *, *, #74590, .F. ) ;
#35380 = CARTESIAN_POINT ( 'NONE',  ( 156.6941734481478079, 259.2447256682348211, 17.84224415335075520 ) ) ;
#35381 = DIRECTION ( 'NONE',  ( 0.4999999999999992784, -0.8660254037844390407, 0.000000000000000000 ) ) ;
#35382 = CARTESIAN_POINT ( 'NONE',  ( 81.97334639510765442, 41.04379167472870193, -3.293735024885245721 ) ) ;
#35383 = CARTESIAN_POINT ( 'NONE',  ( 189.9137270143924923, 269.8458973532920027, 15.23304003329433876 ) ) ;
#35384 = CARTESIAN_POINT ( 'NONE',  ( 161.3723466847356178, 279.8813218052029583, -11.31205495863178179 ) ) ;
#35385 =( BOUNDED_CURVE ( )  B_SPLINE_CURVE ( 2, ( #41397, #63713, #96151, #80967, #10522, #87083, #87593, #27222, #25205 ),
 .UNSPECIFIED., .F., .T. ) 
 B_SPLINE_CURVE_WITH_KNOTS ( ( 3, 2, 2, 2, 3 ),
 ( 0.1814516129032258118, 0.1827956989247311870, 0.1854838709677419373, 0.1881720430107526876, 0.1895161290322580627 ),
 .UNSPECIFIED. ) 
 CURVE ( )  GEOMETRIC_REPRESENTATION_ITEM ( )  RATIONAL_B_SPLINE_CURVE ( ( 0.9330127018922194093, 0.9330127018922194093, 1.000000000000000000, 0.8660254037844387076, 1.000000000000000000, 0.8660254037844387076, 1.000000000000000000, 0.9330127018922194093, 0.9330127018922194093 ) ) 
 REPRESENTATION_ITEM ( '' )  );
#35386 = FACE_OUTER_BOUND ( 'NONE', #98082, .T. ) ;
#35387 = EDGE_CURVE ( 'NONE', #68897, #24506, #988, .T. ) ;
#35388 = CARTESIAN_POINT ( 'NONE',  ( 196.1195470348416166, 280.1172796017575024, -16.75394804383025971 ) ) ;
#35389 = CARTESIAN_POINT ( 'NONE',  ( 145.0633378486230072, 247.8927522451418213, 10.00000000000009948 ) ) ;
#35390 = B_SPLINE_CURVE_WITH_KNOTS ( 'NONE', 3,
 ( #76730, #84865, #55401, #61010, #14441, #68623, #22532, #7323, #77748, #61520, #62499, #37714, #6829, #84370, #1232, #228, #70621, #53420, #721, #69121, #54918, #16422, #100048, #39199, #23506, #45806, #45323, #46825, #62002, #39692, #32115, #63024, #70111, #85375, #99545, #14917 ),
 .UNSPECIFIED., .F., .F.,
 ( 4, 2, 2, 2, 2, 2, 2, 2, 2, 2, 2, 2, 2, 2, 2, 2, 2, 4 ),
 ( 0.001249278581673068586, 0.001605651914841360042, 0.001962025248009651498, 0.002674771914346297727, 0.004100265247019663911, 0.004813011913356347003, 0.005169385246524688116, 0.005347571913108822676, 0.005436665246400925952, 0.005481211913047011851, 0.005525758579693097750, 0.005614851912985403988, 0.005703945246277711094, 0.005882131912862174385, 0.006060318579446638543, 0.006238505246031102701, 0.006594878579200030150, 0.006951251912368958466 ),
 .UNSPECIFIED. ) ;
#35391 = CARTESIAN_POINT ( 'NONE',  ( 79.98636212202836759, 50.06317686608937834, 14.58694793862931327 ) ) ;
#35392 = CARTESIAN_POINT ( 'NONE',  ( 67.02271111079838306, 69.26504780342379775, -0.6689381131363330013 ) ) ;
#35393 = AXIS2_PLACEMENT_3D ( 'NONE', #7836, #8332, #31609 ) ;
#35394 = CARTESIAN_POINT ( 'NONE',  ( 167.6327783924723178, 249.9043753111564570, 7.633368920509352229 ) ) ;
#35395 = CARTESIAN_POINT ( 'NONE',  ( -24.92236680055712483, 162.1916292661124999, 6.123233995736853057E-16 ) ) ;
#35396 = CARTESIAN_POINT ( 'NONE',  ( 207.5959034698703078, 271.0803430774575418, -1.830000129038042544 ) ) ;
#35397 = EDGE_CURVE ( 'NONE', #87650, #76499, #31870, .T. ) ;
#35399 = CARTESIAN_POINT ( 'NONE',  ( 33.32035334334607057, 27.43677371833803846, -10.00000000000000355 ) ) ;
#35398 = AXIS2_PLACEMENT_3D ( 'NONE', #61563, #68667, #83926 ) ;
#35400 = VECTOR ( 'NONE', #66748, 1000.000000000000000 ) ;
#35401 = CARTESIAN_POINT ( 'NONE',  ( 70.73808989031111594, 70.90155945549474836, -4.160261088369678006 ) ) ;
#35402 = CARTESIAN_POINT ( 'NONE',  ( -20.83177028255669683, 95.08444325421659471, 45.19948689642177442 ) ) ;
#35403 = CARTESIAN_POINT ( 'NONE',  ( 5.294102074706517058, 26.55466486950697558, -1.111400068045478839E-16 ) ) ;
#35404 = CARTESIAN_POINT ( 'NONE',  ( 39.11189823470242999, 30.78052372038643725, -10.00000000000000355 ) ) ;
#35405 = CARTESIAN_POINT ( 'NONE',  ( 72.55490714944258457, 58.69537080386778172, -16.07943689878887739 ) ) ;
#35406 =( NAMED_UNIT ( * ) SI_UNIT ( $, .STERADIAN. ) SOLID_ANGLE_UNIT ( ) );
#35407 = CARTESIAN_POINT ( 'NONE',  ( 157.6219484825743393, 270.8997167613374017, -14.79150089323977468 ) ) ;
#35408 = CARTESIAN_POINT ( 'NONE',  ( 206.0369695942839599, 273.2765813626796216, -9.363013045195234696 ) ) ;
#35409 = VECTOR ( 'NONE', #70996, 1000.000000000000000 ) ;
#35410 = CARTESIAN_POINT ( 'NONE',  ( 4.640666744108908226, 182.6744531367911577, 4.594050593750047540 ) ) ;
#35411 = CARTESIAN_POINT ( 'NONE',  ( 87.88902802526534686, 43.91876200309240375, 0.4180276961671919311 ) ) ;
#35412 = ORIENTED_EDGE ( 'NONE', *, *, #52830, .T. ) ;
#35413 = CARTESIAN_POINT ( 'NONE',  ( 86.85818799200686158, 46.48416747087964751, 9.041777841573095387 ) ) ;
#35414 = B_SPLINE_CURVE_WITH_KNOTS ( 'NONE', 3,
 ( #55147, #54646, #63768, #87144 ),
 .UNSPECIFIED., .F., .F.,
 ( 4, 4 ),
 ( 0.009333216069306437407, 0.01375087555092867168 ),
 .UNSPECIFIED. ) ;
#35415 = CARTESIAN_POINT ( 'NONE',  ( 191.3077102587145646, 274.7514833773715850, 16.90660339326615969 ) ) ;
#35416 = CARTESIAN_POINT ( 'NONE',  ( 71.75124654091098364, 72.49002453570855664, -1.344699539992842752 ) ) ;
#35417 = CARTESIAN_POINT ( 'NONE',  ( 43.63930707798317599, 189.8768266524159856, -9.188101187500093303 ) ) ;
#35418 = B_SPLINE_CURVE_WITH_KNOTS ( 'NONE', 3,
 ( #69886, #64297, #96736, #89168, #19715, #57180, #95750, #66295, #56689, #17703 ),
 .UNSPECIFIED., .F., .F.,
 ( 4, 2, 2, 2, 4 ),
 ( 0.000000000000000000, 0.2500000000000000000, 0.5000000000000000000, 0.7500000000000000000, 1.000000000000000000 ),
 .UNSPECIFIED. ) ;
#35419 = VECTOR ( 'NONE', #86683, 1000.000000000000227 ) ;
#35420 = CARTESIAN_POINT ( 'NONE',  ( 161.8873598795597388, 250.2498629158519350, 13.90822209621415873 ) ) ;
#35421 = CARTESIAN_POINT ( 'NONE',  ( 174.4935265407061706, 288.9661596538846879, 7.702119871588271494 ) ) ;
#35422 = CARTESIAN_POINT ( 'NONE',  ( 147.2443490232117256, 275.6123016948292275, 5.226063659459642352 ) ) ;
#35423 = CARTESIAN_POINT ( 'NONE',  ( 2.730238736670422384, 24.68290643055184574, 3.479690158560446702E-15 ) ) ;
#35424 = CARTESIAN_POINT ( 'NONE',  ( 200.4845243426100012, 268.5102331880001998, -6.465539202158884002 ) ) ;
#35425 = CARTESIAN_POINT ( 'NONE',  ( -70.89022602266993545, 47.22876919346843749, -10.00000000000000000 ) ) ;
#35426 = LINE ( 'NONE', #82079, #99113 ) ;
#35427 = LINE ( 'NONE', #66332, #8841 ) ;
#35428 = B_SPLINE_SURFACE_WITH_KNOTS ( 'NONE', 3, 1, ( 
 ( #11040, #57605 ),
 ( #33845, #49515 ),
 ( #95681, #41406 ),
 ( #72351, #2955 ),
 ( #26228, #57104 ),
 ( #41917, #72851 ),
 ( #3443, #60584 ),
 ( #68196, #99125 ),
 ( #20625, #75833 ),
 ( #5911, #68691 ),
 ( #4933, #30203 ),
 ( #76326, #91540 ),
 ( #97641, #28713 ),
 ( #21135, #28206 ),
 ( #6901, #37790 ),
 ( #29707, #52498 ),
 ( #21618, #52013 ),
 ( #37299, #5420 ),
 ( #36801, #36302 ),
 ( #99624, #91051 ),
 ( #82476, #92059 ),
 ( #61089, #22105 ),
 ( #82954, #59082 ),
 ( #53001, #83951 ),
 ( #51509, #6419 ),
 ( #67712, #43401 ),
 ( #51001, #90054 ),
 ( #74345, #44892 ),
 ( #83446, #14514 ),
 ( #14014, #45396 ),
 ( #81953, #35812 ),
 ( #29221, #12530 ),
 ( #98639, #59590 ),
 ( #13038, #66706 ) ),
 .UNSPECIFIED., .T., .F., .F.,
 ( 4, 2, 2, 2, 2, 2, 2, 2, 2, 2, 2, 2, 2, 2, 2, 2, 4 ),
 ( 2, 2 ),
 ( 0.000000000000000000, 0.06250000000000000000, 0.1250000000000000000, 0.1875000000000000000, 0.2500000000000000000, 0.3125000000000000000, 0.3750000000000000000, 0.4375000000000000000, 0.5000000000000000000, 0.5625000000000000000, 0.6250000000000000000, 0.6875000000000000000, 0.7500000000000000000, 0.8125000000000000000, 0.8750000000000000000, 0.9375000000000000000, 1.000000000000000000 ),
 ( 0.000000000000000000, 1.000000000000000000 ),
 .UNSPECIFIED. ) ;
#35429 = EDGE_CURVE ( 'NONE', #45858, #99079, #55166, .T. ) ;
#35430 = CARTESIAN_POINT ( 'NONE',  ( 167.0269342199107143, 257.9714305878135860, -15.35314806562867318 ) ) ;
#35431 = CARTESIAN_POINT ( 'NONE',  ( 175.0809028706871118, 261.2525943152746208, 15.25527675994286092 ) ) ;
#35432 = CARTESIAN_POINT ( 'NONE',  ( 86.26382137438992004, 230.6115022471902876, -5.000000000000047962 ) ) ;
#35433 = CARTESIAN_POINT ( 'NONE',  ( 44.18794977381974576, 118.5901545549086791, 10.00000000000000000 ) ) ;
#35434 = CARTESIAN_POINT ( 'NONE',  ( 161.6115930178048075, 267.7619094808129603, -17.27471002177463788 ) ) ;
#35435 = EDGE_LOOP ( 'NONE', ( #26892, #23990, #98141, #24093 ) ) ;
#35436 = CARTESIAN_POINT ( 'NONE',  ( 62.93552237999645627, 197.9548013555410080, -4.594050593750042211 ) ) ;
#35437 = ORIENTED_EDGE ( 'NONE', *, *, #59092, .F. ) ;
#35438 = LINE ( 'NONE', #80593, #10955 ) ;
#35439 = CARTESIAN_POINT ( 'NONE',  ( 183.9467679955122037, 297.5904300510428016, 0.04192798755140602490 ) ) ;
#35440 = CARTESIAN_POINT ( 'NONE',  ( 67.63792478863227586, 66.83026407364596366, -8.502183981914797073 ) ) ;
#35441 = ADVANCED_FACE ( 'NONE', ( #10468 ), #72287, .T. ) ;
#35442 = ORIENTED_EDGE ( 'NONE', *, *, #65746, .T. ) ;
#35443 = FACE_OUTER_BOUND ( 'NONE', #89216, .T. ) ;
#35444 = CARTESIAN_POINT ( 'NONE',  ( 164.3524132573224392, 245.9802652221976587, -2.749586949851067441 ) ) ;
#35445 = LINE ( 'NONE', #28336, #86430 ) ;
#35446 = CARTESIAN_POINT ( 'NONE',  ( 34.18979426048110781, 28.24335787977765122, -9.188101187500008038 ) ) ;
#35447 = CARTESIAN_POINT ( 'NONE',  ( 185.8388345170929199, 263.3051524106403463, 11.05951379595252071 ) ) ;
#35448 = LINE ( 'NONE', #51655, #19843 ) ;
#35449 = CARTESIAN_POINT ( 'NONE',  ( 174.5163211812949555, 257.2306003409090067, 11.39338901972694806 ) ) ;
#35450 = ORIENTED_EDGE ( 'NONE', *, *, #75734, .F. ) ;
#35451 = CARTESIAN_POINT ( 'NONE',  ( 17.99030130830579566, 16.10170272979926054, -7.433330006724141015 ) ) ;
#35452 = CARTESIAN_POINT ( 'NONE',  ( 68.79254404386716715, 64.26810367574286431, 12.51937741639473245 ) ) ;
#35453 = DIRECTION ( 'NONE',  ( 0.000000000000000000, 0.000000000000000000, -1.000000000000000000 ) ) ;
#35454 = CARTESIAN_POINT ( 'NONE',  ( 17.73189607522619582, 18.43677371833801359, -10.00000000000000355 ) ) ;
#35455 = VERTEX_POINT ( 'NONE', #26662 ) ;
#35456 = CARTESIAN_POINT ( 'NONE',  ( 77.47728950214126087, 59.35671389659360386, 16.44570396066454521 ) ) ;
#35457 = CARTESIAN_POINT ( 'NONE',  ( -48.47243291925849462, 30.64988553008148031, -10.00000000000000000 ) ) ;
#35458 = LINE ( 'NONE', #72499, #94974 ) ;
#35459 = ORIENTED_EDGE ( 'NONE', *, *, #62771, .T. ) ;
#35461 = CARTESIAN_POINT ( 'NONE',  ( -58.10760318826260118, 36.06970723555269842, 10.00000000000000000 ) ) ;
#35460 = CARTESIAN_POINT ( 'NONE',  ( 161.1750406344237661, 251.4836360396366501, -14.21198410781773802 ) ) ;
#35462 = CARTESIAN_POINT ( 'NONE',  ( 149.2923684163597784, 272.0650280510108701, -12.99082738998495756 ) ) ;
#35463 = ORIENTED_EDGE ( 'NONE', *, *, #71672, .T. ) ;
#35464 = CARTESIAN_POINT ( 'NONE',  ( 66.07037714390584426, 68.51423597247097064, -2.421109949964840524 ) ) ;
#35465 = VECTOR ( 'NONE', #33578, 1000.000000000000000 ) ;
#35466 = CARTESIAN_POINT ( 'NONE',  ( 159.4574711498080433, 254.4585536525209477, 16.86100557095418395 ) ) ;
#35467 = CARTESIAN_POINT ( 'NONE',  ( 6.147400554087897540, 72.11620600556240390, -10.00000000000000000 ) ) ;
#35468 = CARTESIAN_POINT ( 'NONE',  ( 77.91510949599519620, 62.18724900762369856, -15.97225761198294691 ) ) ;
#35469 = CARTESIAN_POINT ( 'NONE',  ( 117.8198823448352499, 229.6423013555409796, -4.594050593750043987 ) ) ;
#35470 = AXIS2_PLACEMENT_3D ( 'NONE', #25990, #26132, #33742 ) ;
#35471 = CARTESIAN_POINT ( 'NONE',  ( 79.14312167556931854, 57.64441083166269664, 0.000000000000000000 ) ) ;
#35472 = CARTESIAN_POINT ( 'NONE',  ( 183.5989898313927142, 289.9010940570624939, -13.66799045760379627 ) ) ;
#35473 = ORIENTED_EDGE ( 'NONE', *, *, #14166, .F. ) ;
#35474 = VECTOR ( 'NONE', #10101, 1000.000000000000114 ) ;
#35475 = CARTESIAN_POINT ( 'NONE',  ( 164.3602934812760452, 245.9666162739349318, -7.171958108566009571 ) ) ;
#35476 = ORIENTED_EDGE ( 'NONE', *, *, #93191, .F. ) ;
#35477 = ORIENTED_EDGE ( 'NONE', *, *, #2699, .F. ) ;
#35478 = CARTESIAN_POINT ( 'NONE',  ( 159.8416255366773839, 253.7931787365127434, 16.77980437810719394 ) ) ;
#35479 = CARTESIAN_POINT ( 'NONE',  ( 75.30099715557209095, 66.83639500800819633, -12.91230939377402542 ) ) ;
#35480 = CARTESIAN_POINT ( 'NONE',  ( 73.65258675182887771, 204.1423013555409796, -4.594050593750043987 ) ) ;
#35481 = ORIENTED_EDGE ( 'NONE', *, *, #80665, .T. ) ;
#35482 = DIRECTION ( 'NONE',  ( 0.8660254037844377084, 0.5000000000000016653, 0.000000000000000000 ) ) ;
#35483 = DIRECTION ( 'NONE',  ( 0.9086904199442095154, -0.4174706225611763410, 0.000000000000000000 ) ) ;
#35484 = CARTESIAN_POINT ( 'NONE',  ( 198.7520972810255842, 286.3982647288286785, 17.58825518441947722 ) ) ;
#35485 = CARTESIAN_POINT ( 'NONE',  ( 175.6165075620648963, 278.4664812795192574, 16.92304262170376461 ) ) ;
#35486 = ORIENTED_EDGE ( 'NONE', *, *, #1379, .F. ) ;
#35487 = VECTOR ( 'NONE', #82359, 1000.000000000000000 ) ;
#35488 = CARTESIAN_POINT ( 'NONE',  ( 76.11542371522575934, 62.61180736277591308, -15.13754670253717194 ) ) ;
#35489 = CARTESIAN_POINT ( 'NONE',  ( 203.3740894404336927, 278.3927394765486838, -15.19753795879846869 ) ) ;
#35490 = ORIENTED_EDGE ( 'NONE', *, *, #59890, .F. ) ;
#35491 = CARTESIAN_POINT ( 'NONE',  ( 147.9190624158496803, 274.4436638182332899, 9.640318987393841965 ) ) ;
#35492 = CARTESIAN_POINT ( 'NONE',  ( 81.89930626873778863, 42.21375885382297355, 7.647715624843501203 ) ) ;
#35493 = CARTESIAN_POINT ( 'NONE',  ( 161.8882824960653579, 250.2482648971885340, -13.83574485983625557 ) ) ;
#35494 = CARTESIAN_POINT ( 'NONE',  ( 78.92295937046175425, 204.8262482093457777, 3.021315404115420679E-15 ) ) ;
#35495 = CARTESIAN_POINT ( 'NONE',  ( 200.2074516942827245, 283.2632627625744135, -16.91194335012181327 ) ) ;
#35496 = CARTESIAN_POINT ( 'NONE',  ( 169.8069776206597226, 261.6727971985682757, -16.70353856883196286 ) ) ;
#35497 = CIRCLE ( 'NONE', #97017, 0.1418229129680845801 ) ;
#35498 = EDGE_CURVE ( 'NONE', #24001, #47421, #21347, .T. ) ;
#35499 = CARTESIAN_POINT ( 'NONE',  ( 205.8610808625997208, 274.0851439753691920, 10.38803237360972531 ) ) ;
#35500 = CARTESIAN_POINT ( 'NONE',  ( 134.7352435515850289, 237.0494855054051584, -2.679491924311248496 ) ) ;
#35501 = ORIENTED_EDGE ( 'NONE', *, *, #78238, .F. ) ;
#35502 = CARTESIAN_POINT ( 'NONE',  ( 208.3135187673106543, 269.8373969220020285, 2.829653198597726682 ) ) ;
#35503 = CARTESIAN_POINT ( 'NONE',  ( 114.8152493078691947, 249.3464784336661637, 1.353441290958777327E-15 ) ) ;
#35504 = ORIENTED_EDGE ( 'NONE', *, *, #22277, .T. ) ;
#35505 = CARTESIAN_POINT ( 'NONE',  ( 146.5157004908022031, 276.8743579738231233, -0.1877253132609108255 ) ) ;
#35506 = CARTESIAN_POINT ( 'NONE',  ( 85.48944666241685297, 43.63848491286618980, 5.277307547990027103 ) ) ;
#35507 = ADVANCED_FACE ( 'NONE', ( #67643 ), #50946, .F. ) ;
#35508 = CARTESIAN_POINT ( 'NONE',  ( 155.4495868485232108, 261.4004128932040203, -18.48326470492642315 ) ) ;
#35509 = LINE ( 'NONE', #3634, #54837 ) ;
#35510 = CARTESIAN_POINT ( 'NONE',  ( 73.95048969143448403, 57.13095431899427723, 16.00405266783817027 ) ) ;
#35511 = CARTESIAN_POINT ( 'NONE',  ( -41.08971556016342674, 38.44550953485882872, 59.99999999999999289 ) ) ;
#35512 = ORIENTED_EDGE ( 'NONE', *, *, #46263, .T. ) ;
#35513 = CARTESIAN_POINT ( 'NONE',  ( 76.59400919359040927, 55.08999672436397788, 16.14094864937774787 ) ) ;
#35514 = LINE ( 'NONE', #28925, #55444 ) ;
#35515 = CARTESIAN_POINT ( 'NONE',  ( 35.03822396736671152, 49.37458582131906581, 177.5919119679930134 ) ) ;
#35516 = CARTESIAN_POINT ( 'NONE',  ( 147.6729357283378192, 275.7175590154257065, 2.784006950529999358 ) ) ;
#35517 = CARTESIAN_POINT ( 'NONE',  ( 29.78943643340442549, 199.5530062829863027, -4.648177544792955347E-16 ) ) ;
#35518 = CARTESIAN_POINT ( 'NONE',  ( 198.5281735716552305, 266.2561165906912493, 0.8612751909359168678 ) ) ;
#35519 = EDGE_CURVE ( 'NONE', #87466, #1591, #89041, .T. ) ;
#35520 = CARTESIAN_POINT ( 'NONE',  ( 195.3315847523439004, 263.4512225432230252, 0.8630184002952996369 ) ) ;
#35521 = CARTESIAN_POINT ( 'NONE',  ( 147.2494378675467033, 275.6034875578896504, 3.639370109197119341 ) ) ;
#35522 = DIRECTION ( 'NONE',  ( -0.8660254037844379305, -0.5000000000000011102, -0.000000000000000000 ) ) ;
#35523 = CARTESIAN_POINT ( 'NONE',  ( 157.0978663001774862, 258.5455091378672137, -17.31223197570816552 ) ) ;
#35524 = CARTESIAN_POINT ( 'NONE',  ( 174.6782577430604420, 252.0113062779471989, 3.549132482648186482 ) ) ;
#35525 = EDGE_CURVE ( 'NONE', #34934, #65613, #33771, .T. ) ;
#35526 = CARTESIAN_POINT ( 'NONE',  ( 15.84452179826556417, 32.08080186712592763, -3.090169943749475845 ) ) ;
#35527 = EDGE_CURVE ( 'NONE', #983, #68725, #70881, .T. ) ;
#35528 = CARTESIAN_POINT ( 'NONE',  ( 190.4841013044967042, 300.7188538369516095, 4.682298117523464143 ) ) ;
#35529 = CARTESIAN_POINT ( 'NONE',  ( 110.0000000000000000, 0.000000000000000000, 59.99999999999999289 ) ) ;
#35530 = CARTESIAN_POINT ( 'NONE',  ( 198.0858447170796524, 287.5522480202560018, 18.44384186289807559 ) ) ;
#35531 = CARTESIAN_POINT ( 'NONE',  ( 157.0103870222185662, 271.9336101705912370, -15.05502374871075766 ) ) ;
#35532 = CARTESIAN_POINT ( 'NONE',  ( 141.9600801517288460, 242.7677522451417929, -5.000000000000041744 ) ) ;
#35533 = CARTESIAN_POINT ( 'NONE',  ( 175.7051557773955324, 285.9761665229386836, -11.83304049905165911 ) ) ;
#35534 = ORIENTED_EDGE ( 'NONE', *, *, #97146, .F. ) ;
#35535 = VECTOR ( 'NONE', #38828, 1000.000000000000000 ) ;
#35536 = DIRECTION ( 'NONE',  ( -1.000000000000000000, 0.000000000000000000, 0.000000000000000000 ) ) ;
#35537 = CARTESIAN_POINT ( 'NONE',  ( 151.2646864780760723, 268.6488729594320830, -14.38346604407754548 ) ) ;
#35538 = CARTESIAN_POINT ( 'NONE',  ( -2.801652295722365071, 175.3149278399160949, -9.188101187500095079 ) ) ;
#35539 = CARTESIAN_POINT ( 'NONE',  ( 53.57110205792969282, 210.9244531367911577, -4.594050593750046652 ) ) ;
#35540 = VECTOR ( 'NONE', #77014, 999.9999999999998863 ) ;
#35541 = CARTESIAN_POINT ( 'NONE',  ( 83.76030657582204242, 41.96383438897017726, 4.835547397684552884 ) ) ;
#35542 = CARTESIAN_POINT ( 'NONE',  ( 17.08077532425043543, 25.56454794089041727, 10.00000000000000355 ) ) ;
#35543 = CARTESIAN_POINT ( 'NONE',  ( 85.23821057327256767, 49.07543163279748910, 12.45235422365945510 ) ) ;
#35544 = FACE_OUTER_BOUND ( 'NONE', #79618, .T. ) ;
#35545 = CARTESIAN_POINT ( 'NONE',  ( 188.9222141114651947, 290.4608455028081266, -14.68227143028564008 ) ) ;
#35546 = CARTESIAN_POINT ( 'NONE',  ( 73.83032011078108781, 55.08034924954741740, -16.60147083384191902 ) ) ;
#35547 = EDGE_CURVE ( 'NONE', #45450, #37792, #31025, .T. ) ;
#35548 = CARTESIAN_POINT ( 'NONE',  ( 171.4108528510993210, 258.3780868124931089, 14.19704647611232140 ) ) ;
#35549 = CARTESIAN_POINT ( 'NONE',  ( 179.1925786807920815, 254.4794537879851362, -4.121526722083301841 ) ) ;
#35550 = CARTESIAN_POINT ( 'NONE',  ( 150.8677798231829570, 269.3363354515693118, 13.85464777478129150 ) ) ;
#35551 = AXIS2_PLACEMENT_3D ( 'NONE', #69161, #67680, #22573 ) ;
#35552 = EDGE_CURVE ( 'NONE', #98479, #1989, #77758, .T. ) ;
#35553 = CARTESIAN_POINT ( 'NONE',  ( 42.60170726692454224, 188.7365022471902023, 10.00000000000009592 ) ) ;
#35554 = CARTESIAN_POINT ( 'NONE',  ( 181.1401942789648558, 292.7476587285891583, 9.359391415499011657 ) ) ;
#35555 = CARTESIAN_POINT ( 'NONE',  ( 202.9685995779611858, 279.0950685203052899, 16.84977534244423580 ) ) ;
#35556 = CARTESIAN_POINT ( 'NONE',  ( 10.54098545103790840, 167.7048013555410080, 4.594050593750051981 ) ) ;
#35557 = CARTESIAN_POINT ( 'NONE',  ( 164.3059702326774243, 284.8567553647953332, 4.267327785685381514 ) ) ;
#35558 = CARTESIAN_POINT ( 'NONE',  ( 192.2185419806677942, 297.7147144631093170, 12.45868041609393728 ) ) ;
#35559 = CARTESIAN_POINT ( 'NONE',  ( 40.22068564906490451, 26.14754757982093381, -5.678558825948276656 ) ) ;
#35560 = CARTESIAN_POINT ( 'NONE',  ( 206.4229368915142686, 273.1119807867502800, 10.31819530520674810 ) ) ;
#35561 = CARTESIAN_POINT ( 'NONE',  ( 207.0548180518391916, 272.0175305127218053, 7.721676452263806389 ) ) ;
#35562 = EDGE_CURVE ( 'NONE', #20729, #62642, #45556, .T. ) ;
#35563 = CARTESIAN_POINT ( 'NONE',  ( 193.8365934467825298, 294.9121671145370556, 14.14845633038902584 ) ) ;
#35564 = CARTESIAN_POINT ( 'NONE',  ( 153.3682214589191517, 265.3887646446434587, -16.19041097722891109 ) ) ;
#35565 = CARTESIAN_POINT ( 'NONE',  ( 146.3569154618635366, 243.7592609112379876, 2.679491924311254714 ) ) ;
#35566 = DIRECTION ( 'NONE',  ( 1.000000000000000000, 0.000000000000000000, 0.000000000000000000 ) ) ;
#35567 = CARTESIAN_POINT ( 'NONE',  ( 16.48196734934595753, 24.91421378149918198, 9.188101187500008038 ) ) ;
#35568 = CARTESIAN_POINT ( 'NONE',  ( 71.53080809438635868, 72.38941617099001746, 1.021674839914414878 ) ) ;
#35569 = CARTESIAN_POINT ( 'NONE',  ( 82.17887732911846399, 54.20604701261002845, 15.63465942432049083 ) ) ;
#35570 = CIRCLE ( 'NONE', #1603, 60.00000000000002132 ) ;
#35571 = CARTESIAN_POINT ( 'NONE',  ( 71.63453813518020752, 72.07236434383467838, 0.7172108931481352423 ) ) ;
#35572 = EDGE_CURVE ( 'NONE', #89714, #73699, #83385, .T. ) ;
#35573 = CARTESIAN_POINT ( 'NONE',  ( 152.9138932732664671, 277.5051963946797287, -5.211359010245092627 ) ) ;
#35574 = ORIENTED_EDGE ( 'NONE', *, *, #2894, .F. ) ;
#35575 = CARTESIAN_POINT ( 'NONE',  ( 104.4503548538631463, 241.1115022471902876, -5.000000000000047962 ) ) ;
#35576 = ADVANCED_FACE ( 'NONE', ( #85384 ), #24596, .F. ) ;
#35577 = CARTESIAN_POINT ( 'NONE',  ( -66.34925969370661392, 42.61035540433362456, -10.00000000000000000 ) ) ;
#35578 = LINE ( 'NONE', #20392, #95004 ) ;
#35579 = AXIS2_PLACEMENT_3D ( 'NONE', #39993, #15705, #62296 ) ;
#35580 = ORIENTED_EDGE ( 'NONE', *, *, #94392, .T. ) ;
#35581 = CARTESIAN_POINT ( 'NONE',  ( 153.4242699508872647, 264.9083646613370320, 16.62000820703435267 ) ) ;
#35582 = CARTESIAN_POINT ( 'NONE',  ( 148.8004271348772249, 276.2543922634745286, -5.595754242233163644 ) ) ;
#35583 = CARTESIAN_POINT ( 'NONE',  ( 66.31130943496550856, 68.58487545890584158, 4.825481589580086883 ) ) ;
#35584 = CARTESIAN_POINT ( 'NONE',  ( 202.7676489560256528, 279.4431252073101746, -16.04062356091568020 ) ) ;
#35585 = EDGE_LOOP ( 'NONE', ( #34929, #9977, #93689, #43403 ) ) ;
#35586 = ORIENTED_EDGE ( 'NONE', *, *, #54717, .F. ) ;
#35588 = CARTESIAN_POINT ( 'NONE',  ( 163.8147431267737204, 246.9115372060205118, 7.125417796469586840 ) ) ;
#35587 = CARTESIAN_POINT ( 'NONE',  ( 165.1220565656817882, 246.3610340376649788, -4.369863341033457971 ) ) ;
#35589 = CARTESIAN_POINT ( 'NONE',  ( 153.0070714074088016, 265.6309737354857248, 17.74442213480098474 ) ) ;
#35590 = VERTEX_POINT ( 'NONE', #24530 ) ;
#35591 = CARTESIAN_POINT ( 'NONE',  ( 88.30455217607853058, 43.91915848855261828, -2.151936166193182398 ) ) ;
#35592 = CARTESIAN_POINT ( 'NONE',  ( 80.56743834928197145, 57.59328067535012252, 16.23428813468583698 ) ) ;
#35593 = ORIENTED_EDGE ( 'NONE', *, *, #46065, .T. ) ;
#35594 = LINE ( 'NONE', #74624, #79911 ) ;
#35595 = CARTESIAN_POINT ( 'NONE',  ( 82.37376302093576896, 49.21181299837914480, -13.53283297697456966 ) ) ;
#35596 = CARTESIAN_POINT ( 'NONE',  ( 81.28581595673009019, 43.24335794003573596, 9.611647108222669544 ) ) ;
#35597 = ORIENTED_EDGE ( 'NONE', *, *, #40551, .F. ) ;
#35598 = CARTESIAN_POINT ( 'NONE',  ( 177.0175048079005080, 269.3060889572638530, 16.09599001003793006 ) ) ;
#35599 = CARTESIAN_POINT ( 'NONE',  ( 165.0020474182383339, 244.8550658491588479, 1.825383354618924425 ) ) ;
#35600 = CARTESIAN_POINT ( 'NONE',  ( 73.71617248606330008, 59.79991374540308868, 15.48773420481832730 ) ) ;
#35601 = ORIENTED_EDGE ( 'NONE', *, *, #17188, .F. ) ;
#35602 = CARTESIAN_POINT ( 'NONE',  ( 174.7676448104877807, 277.4213516129615869, -15.64693699161624352 ) ) ;
#35603 = CARTESIAN_POINT ( 'NONE',  ( 169.6734611486750453, 261.6087119384134212, -16.67296044893563689 ) ) ;
#35604 = VERTEX_POINT ( 'NONE', #72160 ) ;
#35605 = CARTESIAN_POINT ( 'NONE',  ( 7.454216751344177716, 28.24511763804003195, 10.00000000000000000 ) ) ;
#35607 = ORIENTED_EDGE ( 'NONE', *, *, #38002, .F. ) ;
#35606 = B_SPLINE_CURVE_WITH_KNOTS ( 'NONE', 3,
 ( #21200, #12097, #13593, #36879 ),
 .UNSPECIFIED., .F., .F.,
 ( 4, 4 ),
 ( 0.01336260375758639186, 0.02197367245289875287 ),
 .UNSPECIFIED. ) ;
#35608 = FACE_OUTER_BOUND ( 'NONE', #70609, .T. ) ;
#35609 = EDGE_LOOP ( 'NONE', ( #94564, #23035, #2014, #43179 ) ) ;
#35610 = CARTESIAN_POINT ( 'NONE',  ( 156.3075079012271260, 267.3199146548383283, -16.47880472041608968 ) ) ;
#35611 = CARTESIAN_POINT ( 'NONE',  ( 190.6954410837624607, 300.3528026016029457, -5.728531842148099962 ) ) ;
#35612 = DIRECTION ( 'NONE',  ( 0.000000000000000000, 0.000000000000000000, 1.000000000000000000 ) ) ;
#35613 = CARTESIAN_POINT ( 'NONE',  ( -54.21831688459419496, 33.63902229265145394, -10.00000000000000000 ) ) ;
#35614 = CARTESIAN_POINT ( 'NONE',  ( 192.7944000592152634, 296.7172990131160759, 11.44860011299869740 ) ) ;
#35615 = DIRECTION ( 'NONE',  ( 0.02977611660965746518, -0.9995565931350001154, 0.000000000000000000 ) ) ;
#35616 = ORIENTED_EDGE ( 'NONE', *, *, #10119, .F. ) ;
#35617 = CARTESIAN_POINT ( 'NONE',  ( -7.136131074307646927, 62.27793715567937483, -10.00000000000000000 ) ) ;
#35618 = B_SPLINE_CURVE_WITH_KNOTS ( 'NONE', 3,
 ( #74049, #66433, #42616, #26941 ),
 .UNSPECIFIED., .F., .F.,
 ( 4, 4 ),
 ( 1.260064970365687123E-16, 0.004705947932869557031 ),
 .UNSPECIFIED. ) ;
#35619 = B_SPLINE_CURVE_WITH_KNOTS ( 'NONE', 3,
 ( #73973, #58735, #27368, #98276, #58251, #35456, #44535, #66359, #97292, #90710, #66850, #89711, #20272, #67859, #97778, #21266 ),
 .UNSPECIFIED., .F., .F.,
 ( 4, 1, 2, 2, 2, 1, 2, 2, 4 ),
 ( 0.000000000000000000, 0.1250000000000005551, 0.1875000000000007494, 0.2500000000000009437, 0.4999999999999994449, 0.6249999999999976685, 0.6874999999999981126, 0.7499999999999986677, 1.000000000000000000 ),
 .UNSPECIFIED. ) ;
#35620 = CARTESIAN_POINT ( 'NONE',  ( 206.4695239676918845, 273.0312896038346366, 10.41704154450801667 ) ) ;
#35622 = CARTESIAN_POINT ( 'NONE',  ( 176.1545129615995791, 279.8491840402730304, -16.65846268951813158 ) ) ;
#35621 = CARTESIAN_POINT ( 'NONE',  ( 149.4908848037268001, 271.7211875819559737, -12.92288068979413573 ) ) ;
#35624 = ORIENTED_EDGE ( 'NONE', *, *, #41974, .T. ) ;
#35623 = CARTESIAN_POINT ( 'NONE',  ( 159.6419305724666344, 254.1390605605417079, 16.92015248457581933 ) ) ;
#35625 = CARTESIAN_POINT ( 'NONE',  ( 176.5942392360894928, 290.0311217938273103, -9.473091939615279955 ) ) ;
#35626 = VERTEX_POINT ( 'NONE', #86396 ) ;
#35627 = CARTESIAN_POINT ( 'NONE',  ( 186.6370815005770112, 276.6162495332958997, 16.64778423223098613 ) ) ;
#35628 = CARTESIAN_POINT ( 'NONE',  ( 83.51092623577891061, 51.50185674319120466, -14.43088262691036583 ) ) ;
#35629 = CARTESIAN_POINT ( 'NONE',  ( 163.7412020991711756, 247.5884774922407416, 7.473643870864920657 ) ) ;
#35630 = CARTESIAN_POINT ( 'NONE',  ( 14.46184932687122604, 20.30066082961420904, -10.00000000000000533 ) ) ;
#35631 = CARTESIAN_POINT ( 'NONE',  ( 190.1092758455735918, 301.3680705757765850, -1.432918395251892019 ) ) ;
#35632 = ORIENTED_EDGE ( 'NONE', *, *, #95995, .T. ) ;
#35633 = CARTESIAN_POINT ( 'NONE',  ( 170.5400372565194971, 255.6862325933128659, -12.52260723181821156 ) ) ;
#35634 = LINE ( 'NONE', #29532, #19316 ) ;
#35635 = CARTESIAN_POINT ( 'NONE',  ( 53.71569994882479193, 208.4865022471902876, -10.00000000000009592 ) ) ;
#35636 = DIRECTION ( 'NONE',  ( 0.5000000000000001110, -0.8660254037844387076, -0.000000000000000000 ) ) ;
#35637 = CARTESIAN_POINT ( 'NONE',  ( 21.94339294393528306, 190.1427522451419350, 10.00000000000009237 ) ) ;
#35638 = CARTESIAN_POINT ( 'NONE',  ( 98.36111373172988692, 227.5958772461660260, -9.188101187500095079 ) ) ;
#35639 = ADVANCED_FACE ( 'NONE', ( #16928 ), #93374, .F. ) ;
#35640 = CARTESIAN_POINT ( 'NONE',  ( 169.5606897086885283, 261.7245448792994580, 16.76904778814408559 ) ) ;
#35641 = LINE ( 'NONE', #59412, #67506 ) ;
#35642 = CARTESIAN_POINT ( 'NONE',  ( 157.1606030646430554, 258.4368458743103361, 17.96998724893680688 ) ) ;
#35643 = CARTESIAN_POINT ( 'NONE',  ( 163.1394982460384995, 248.0810956470044175, 11.48951572717839298 ) ) ;
#35644 = CARTESIAN_POINT ( 'NONE',  ( 19.47135178391741661, 191.2369531367911293, -4.594050593750048428 ) ) ;
#35645 = FACE_OUTER_BOUND ( 'NONE', #73719, .T. ) ;
#35646 = ORIENTED_EDGE ( 'NONE', *, *, #23458, .T. ) ;
#35647 = ORIENTED_EDGE ( 'NONE', *, *, #37351, .T. ) ;
#35648 = CARTESIAN_POINT ( 'NONE',  ( -70.00000000000000000, 20.00000000000000000, 59.99999999999999289 ) ) ;
#35649 = CARTESIAN_POINT ( 'NONE',  ( 74.46690696312865043, 68.23757356209769398, -11.48548186069604782 ) ) ;
#35650 = EDGE_CURVE ( 'NONE', #10047, #95964, #40971, .T. ) ;
#35651 = CARTESIAN_POINT ( 'NONE',  ( 70.94579913988255271, 71.56585977893712425, -1.408710708485262586 ) ) ;
#35652 = EDGE_CURVE ( 'NONE', #16631, #20674, #7210, .T. ) ;
#35653 = LINE ( 'NONE', #88935, #27335 ) ;
#35654 = CARTESIAN_POINT ( 'NONE',  ( 81.98471768757296729, 41.36544628577401994, -5.913068783389250349 ) ) ;
#35655 = CARTESIAN_POINT ( 'NONE',  ( 161.8408514536557163, 250.3304178724980318, -14.12919723462510646 ) ) ;
#35656 = CARTESIAN_POINT ( 'NONE',  ( 179.1906477385719541, 287.9874793598855831, -12.80386165526534370 ) ) ;
#35657 = CARTESIAN_POINT ( 'NONE',  ( 168.1482817187297485, 251.7781618965069299, 10.54809081625006328 ) ) ;
#35658 = CARTESIAN_POINT ( 'NONE',  ( 42.82723471405275717, 195.5333772461660544, 9.188101187500095079 ) ) ;
#35659 = CARTESIAN_POINT ( 'NONE',  ( 89.99855592466245469, 222.7677522451418781, 10.00000000000009592 ) ) ;
#35660 = EDGE_LOOP ( 'NONE', ( #51543, #43856, #9727, #6446 ) ) ;
#35661 = CARTESIAN_POINT ( 'NONE',  ( 194.7854625312828887, 266.3706711642819300, -7.713939373946292477 ) ) ;
#35662 = CARTESIAN_POINT ( 'NONE',  ( 178.7744559918192806, 259.2102874926480354, -10.28428999224912843 ) ) ;
#35663 = FACE_OUTER_BOUND ( 'NONE', #1469, .T. ) ;
#35664 = CARTESIAN_POINT ( 'NONE',  ( 2.042590532755589994, 181.1744531367911577, 4.594050593750047540 ) ) ;
#35665 = CARTESIAN_POINT ( 'NONE',  ( 199.2383506163646132, 285.5560492466715345, -17.78808061564097898 ) ) ;
#35666 = CARTESIAN_POINT ( 'NONE',  ( -17.43550054826663498, 104.2312461070085021, 44.57229221387615326 ) ) ;
#35667 = CARTESIAN_POINT ( 'NONE',  ( 73.22997076551303053, 69.87431308930813145, 9.604659174840600500 ) ) ;
#35668 = CARTESIAN_POINT ( 'NONE',  ( 52.94873307290088604, 207.5024278399160949, 9.188101187500095079 ) ) ;
#35669 = CARTESIAN_POINT ( 'NONE',  ( 37.48526053816526371, 54.83666944042808922, -10.00000000000000000 ) ) ;
#35670 = CARTESIAN_POINT ( 'NONE',  ( 203.8280627875664663, 275.9321709329971100, 13.16261023213589709 ) ) ;
#35671 = CARTESIAN_POINT ( 'NONE',  ( 49.74924850768368145, 83.93760989710258968, 10.00000000000000000 ) ) ;
#35672 = CARTESIAN_POINT ( 'NONE',  ( 66.35038720663168021, 68.05568594965032503, -4.770468563139677265 ) ) ;
#35673 = ORIENTED_EDGE ( 'NONE', *, *, #79642, .T. ) ;
#35674 =( BOUNDED_CURVE ( )  B_SPLINE_CURVE ( 2, ( #91608, #67275, #98202, #68767, #59664, #27793, #29292, #82031, #44969 ),
 .UNSPECIFIED., .F., .T. ) 
 B_SPLINE_CURVE_WITH_KNOTS ( ( 3, 2, 2, 2, 3 ),
 ( 0.4717741935483871218, 0.4731182795698924970, 0.4758064516129032473, 0.4784946236559139976, 0.4798387096774193727 ),
 .UNSPECIFIED. ) 
 CURVE ( )  GEOMETRIC_REPRESENTATION_ITEM ( )  RATIONAL_B_SPLINE_CURVE ( ( 0.9330127018922194093, 0.9330127018922194093, 1.000000000000000000, 0.8660254037844387076, 1.000000000000000000, 0.8660254037844387076, 1.000000000000000000, 0.9330127018922194093, 0.9330127018922194093 ) ) 
 REPRESENTATION_ITEM ( '' )  );
#35675 = ADVANCED_FACE ( 'NONE', ( #54292 ), #98944, .T. ) ;
#35676 = CARTESIAN_POINT ( 'NONE',  ( 47.96820964746023463, 80.67316705762479501, -10.00000000000000000 ) ) ;
#35677 = CARTESIAN_POINT ( 'NONE',  ( 8.826716519331432309, 169.2365022471902023, 10.00000000000009592 ) ) ;
#35678 = CARTESIAN_POINT ( 'NONE',  ( 24.46206622376873696, 38.38158625946101665, 10.00000000000000000 ) ) ;
#35679 = CARTESIAN_POINT ( 'NONE',  ( 125.6948669907937415, 249.5024278399160949, 9.188101187500095079 ) ) ;
#35680 = CARTESIAN_POINT ( 'NONE',  ( 28.70736568013821355, 22.28920272979928185, -7.433330006724141015 ) ) ;
#35681 = CARTESIAN_POINT ( 'NONE',  ( 207.4646420400604541, 271.3076945429622242, -8.143883892282612891 ) ) ;
#35682 = CARTESIAN_POINT ( 'NONE',  ( 83.53204454370724363, 52.39401912150450613, -15.17729711222452416 ) ) ;
#35683 = B_SPLINE_CURVE_WITH_KNOTS ( 'NONE', 3,
 ( #48144, #31932, #16745, #78060 ),
 .UNSPECIFIED., .F., .F.,
 ( 4, 4 ),
 ( 0.007396415386818002910, 0.01554756812702462465 ),
 .UNSPECIFIED. ) ;
#35684 = CARTESIAN_POINT ( 'NONE',  ( 51.80235952159636525, 85.00000000000000000, -59.99999999999999289 ) ) ;
#35686 = CARTESIAN_POINT ( 'NONE',  ( 188.9633349269510632, 289.6955772790231549, 14.43551268334040749 ) ) ;
#35685 = CARTESIAN_POINT ( 'NONE',  ( -50.34886203176066033, 29.86533669878861375, -10.00000000000000000 ) ) ;
#35687 = EDGE_CURVE ( 'NONE', #18677, #20915, #21919, .T. ) ;
#35688 = CARTESIAN_POINT ( 'NONE',  ( 150.3969908582963342, 270.1517658583956631, -13.88764202390153990 ) ) ;
#35689 = ORIENTED_EDGE ( 'NONE', *, *, #54153, .F. ) ;
#35690 = CARTESIAN_POINT ( 'NONE',  ( 196.7232418867741046, 263.8072851099263403, -0.2693295688966246271 ) ) ;
#35691 = CARTESIAN_POINT ( 'NONE',  ( 207.6758789170519890, 270.9418215395808147, -0.5923825352568967695 ) ) ;
#35692 = CARTESIAN_POINT ( 'NONE',  ( 181.6045319792032444, 288.0095535211878541, 13.87245391538852601 ) ) ;
#35693 = CARTESIAN_POINT ( 'NONE',  ( 172.4831635826484444, 290.8796410925290843, -1.652085212636280609 ) ) ;
#35694 = CARTESIAN_POINT ( 'NONE',  ( 3.479571460297436136, 22.98502408145589726, -5.678558825948271327 ) ) ;
#35695 = ORIENTED_EDGE ( 'NONE', *, *, #84144, .T. ) ;
#35696 = CARTESIAN_POINT ( 'NONE',  ( 70.74552968606906234, 69.97318964771673677, 6.399120444304696953 ) ) ;
#35697 = CARTESIAN_POINT ( 'NONE',  ( 171.0717129997618144, 284.5853248254017558, -11.57144567159876836 ) ) ;
#35698 = EDGE_CURVE ( 'NONE', #33648, #99290, #63696, .T. ) ;
#35699 = CARTESIAN_POINT ( 'NONE',  ( 85.04775486883579561, 44.40351755419373347, 7.355666434035634360 ) ) ;
#35700 = DIRECTION ( 'NONE',  ( -0.4621356007560455392, 0.8868092729070039537, 0.000000000000000000 ) ) ;
#35701 = CARTESIAN_POINT ( 'NONE',  ( 182.1983635332545646, 295.7656116556308916, 4.955917269626422872 ) ) ;
#35702 = CARTESIAN_POINT ( 'NONE',  ( 70.78531041105927102, 71.56694630268400203, -0.1705850445758182454 ) ) ;
#35703 = AXIS2_PLACEMENT_3D ( 'NONE', #29601, #91432, #56881 ) ;
#35704 = CARTESIAN_POINT ( 'NONE',  ( 150.0648941724952863, 277.2273145327603174, -9.121012261533550361E-05 ) ) ;
#35705 = CARTESIAN_POINT ( 'NONE',  ( 193.1829427640170422, 282.2301301676865819, 16.90027158358297044 ) ) ;
#35706 = CARTESIAN_POINT ( 'NONE',  ( 3.304740145946305052, 26.00034080476288167, -1.878358725466461243E-16 ) ) ;
#35707 = CARTESIAN_POINT ( 'NONE',  ( 93.10181362155671536, 217.8927522451418213, 10.00000000000009948 ) ) ;
#35708 = VERTEX_POINT ( 'NONE', #45699 ) ;
#35709 = CARTESIAN_POINT ( 'NONE',  ( -59.84120265028303010, 60.49048082395207615, 59.99999999999999289 ) ) ;
#35710 = CARTESIAN_POINT ( 'NONE',  ( 156.0362208818770569, 261.9694580292082264, -16.96406285719872642 ) ) ;
#35711 = ORIENTED_EDGE ( 'NONE', *, *, #68305, .T. ) ;
#35712 = CARTESIAN_POINT ( 'NONE',  ( 146.6138605399200117, 276.7043397814778132, -0.5394499176159462950 ) ) ;
#35713 = CARTESIAN_POINT ( 'NONE',  ( 205.4834637267509549, 273.3784298103438459, -9.787331926331344079 ) ) ;
#35714 = CARTESIAN_POINT ( 'NONE',  ( 204.9608076533459950, 275.6444629144898499, 14.31488288944633069 ) ) ;
#35715 = CARTESIAN_POINT ( 'NONE',  ( 74.88534510618254103, 53.30470171424536829, 16.04906050052737498 ) ) ;
#35716 = EDGE_LOOP ( 'NONE', ( #56426, #81490, #33041, #89503 ) ) ;
#35717 = CARTESIAN_POINT ( 'NONE',  ( 78.06346978264959091, 222.0024278399160949, -9.188101187500093303 ) ) ;
#35718 = CARTESIAN_POINT ( 'NONE',  ( 203.4986178427917878, 278.1770499566792409, 15.08380016308619176 ) ) ;
#35719 = CARTESIAN_POINT ( 'NONE',  ( 80.33508072308799797, 44.92307697338561923, 11.19555900290710149 ) ) ;
#35720 = CARTESIAN_POINT ( 'NONE',  ( 84.57060543673907205, 49.80382465363337019, -13.20176661028953546 ) ) ;
#35721 = CARTESIAN_POINT ( 'NONE',  ( 184.9950698617867886, 259.9054437811999492, -5.827971615141458450 ) ) ;
#35722 = VERTEX_POINT ( 'NONE', #13824 ) ;
#35723 = VERTEX_POINT ( 'NONE', #98449 ) ;
#35724 = CARTESIAN_POINT ( 'NONE',  ( -97.59541525468981149, 48.06504152958505216, -36.50000000000000000 ) ) ;
#35725 = VERTEX_POINT ( 'NONE', #60399 ) ;
#35726 = CARTESIAN_POINT ( 'NONE',  ( 192.6537829138044344, 294.0124578573780241, 14.33366951991050442 ) ) ;
#35727 = B_SPLINE_CURVE_WITH_KNOTS ( 'NONE', 3,
 ( #16797, #93336, #54791, #8207 ),
 .UNSPECIFIED., .F., .F.,
 ( 4, 4 ),
 ( 0.009413270483557435037, 0.01469873868365958840 ),
 .UNSPECIFIED. ) ;
#35729 = ORIENTED_EDGE ( 'NONE', *, *, #65876, .T. ) ;
#35728 = EDGE_CURVE ( 'NONE', #78211, #51310, #29780, .T. ) ;
#35730 = CARTESIAN_POINT ( 'NONE',  ( 75.85732906438254020, 63.05884040557971559, 14.92899268908093013 ) ) ;
#35731 = DIRECTION ( 'NONE',  ( 0.8660254037844395958, 0.4999999999999985567, 0.000000000000000000 ) ) ;
#35732 = VERTEX_POINT ( 'NONE', #87793 ) ;
#35733 = CARTESIAN_POINT ( 'NONE',  ( 164.7596289686694888, 245.2749469205039929, 2.483240442660407776 ) ) ;
#35734 = CARTESIAN_POINT ( 'NONE',  ( 82.46767041311871083, 40.74398673389430314, 3.187025703938450416 ) ) ;
#35735 = CARTESIAN_POINT ( 'NONE',  ( 181.0193311394079103, 261.5502185760933003, 13.24438261311760812 ) ) ;
#35737 = EDGE_CURVE ( 'NONE', #57299, #14526, #95383, .T. ) ;
#35736 = CARTESIAN_POINT ( 'NONE',  ( 84.99999999999997158, 27.49999999999999645, -59.99999999999999289 ) ) ;
#35738 = CARTESIAN_POINT ( 'NONE',  ( 147.9133274879049793, 274.4535970048112290, -9.359166267164972908 ) ) ;
#35739 = CARTESIAN_POINT ( 'NONE',  ( 20.87599742628078303, 30.79103043416549568, 8.090169943749478065 ) ) ;
#35740 = CARTESIAN_POINT ( 'NONE',  ( 168.3561001772640680, 267.2114426321716110, -17.22163279015371629 ) ) ;
#35741 = ORIENTED_EDGE ( 'NONE', *, *, #50984, .F. ) ;
#35742 = CARTESIAN_POINT ( 'NONE',  ( 75.95592525424871155, 56.02552295162529816, 16.15038119120977100 ) ) ;
#35743 = CARTESIAN_POINT ( 'NONE',  ( 14.52619969316804394, 14.10170272979925699, -7.433330006724141015 ) ) ;
#35744 = ORIENTED_EDGE ( 'NONE', *, *, #53336, .T. ) ;
#35745 = DIRECTION ( 'NONE',  ( -0.9825427565607363078, 0.1860369090530955005, 0.000000000000000000 ) ) ;
#35747 = ORIENTED_EDGE ( 'NONE', *, *, #55395, .F. ) ;
#35746 = CARTESIAN_POINT ( 'NONE',  ( 200.9124443442758832, 270.6563311349291894, 9.292281936012786403 ) ) ;
#35748 = DIRECTION ( 'NONE',  ( 1.000000000000000000, 0.000000000000000000, 0.000000000000000000 ) ) ;
#35749 = CARTESIAN_POINT ( 'NONE',  ( 76.20329143637185609, 64.79007453736731748, -14.35255403285628795 ) ) ;
#35750 = CARTESIAN_POINT ( 'NONE',  ( 161.3049863899956335, 281.4170748028290063, -6.576827861606494352 ) ) ;
#35751 = CARTESIAN_POINT ( 'NONE',  ( -17.42236680055705023, 149.2012482093457777, 0.000000000000000000 ) ) ;
#35752 = B_SPLINE_CURVE_WITH_KNOTS ( 'NONE', 3,
 ( #40497, #1019, #3047, #16213, #32903, #16711, #31900, #78027, #70410, #62804, #49118, #32415, #80055, #24805, #2532, #72441, #33414, #33934, #17723, #93760, #63812, #48106, #79049, #78532, #56195, #94745 ),
 .UNSPECIFIED., .F., .F.,
 ( 4, 2, 2, 2, 2, 2, 2, 2, 2, 2, 2, 2, 4 ),
 ( 0.0002565227521606977881, 0.001765950409300323740, 0.001860289637871517755, 0.001907459252157120075, 0.001931044059299878409, 0.001954628866442637176, 0.002001798480728315607, 0.002048968095013994038, 0.002143307323585351334, 0.002331985780728105823, 0.002520664237870861180, 0.002898021152156497662, 0.003275378066442135010 ),
 .UNSPECIFIED. ) ;
#35753 = CARTESIAN_POINT ( 'NONE',  ( 41.50249547274756168, 124.4848494355456836, -10.00000000000000000 ) ) ;
#35754 = DIRECTION ( 'NONE',  ( 1.000000000000000000, 0.000000000000000000, 0.000000000000000000 ) ) ;
#35755 = CARTESIAN_POINT ( 'NONE',  ( -13.11024591527734628, 4.999999999999999112, 32.50000000000000000 ) ) ;
#35756 = ORIENTED_EDGE ( 'NONE', *, *, #87066, .T. ) ;
#35757 = CARTESIAN_POINT ( 'NONE',  ( 181.4793763127861439, 271.1882028957970761, -15.96622495013739673 ) ) ;
#35758 = CARTESIAN_POINT ( 'NONE',  ( 77.28846913097220295, 61.37098587332354072, -15.71112316387479879 ) ) ;
#35759 = ORIENTED_EDGE ( 'NONE', *, *, #25243, .T. ) ;
#35760 = CARTESIAN_POINT ( 'NONE',  ( 159.9950753608005130, 276.8117990079294373, 13.35014033362692487 ) ) ;
#35761 = EDGE_CURVE ( 'NONE', #73611, #97734, #79354, .T. ) ;
#35762 = CARTESIAN_POINT ( 'NONE',  ( 174.6037846674788341, 281.1587274802971592, -14.18186885202987924 ) ) ;
#35763 = CARTESIAN_POINT ( 'NONE',  ( 167.5505310038667517, 261.6318463984700315, 17.07012949051403439 ) ) ;
#35764 = CARTESIAN_POINT ( 'NONE',  ( 190.2389970918280540, 301.1433867864428748, 4.601241515604689525 ) ) ;
#35765 = CARTESIAN_POINT ( 'NONE',  ( 163.9695846725937542, 274.0645315248153224, 14.77959389856284389 ) ) ;
#35767 = CARTESIAN_POINT ( 'NONE',  ( 151.2850021181167222, 275.2870477160321343, -9.752878341108868199 ) ) ;
#35766 = LINE ( 'NONE', #79917, #89014 ) ;
#35768 = CYLINDRICAL_SURFACE ( 'NONE', #96448, 70.00000000000002842 ) ;
#35769 = EDGE_LOOP ( 'NONE', ( #40952, #98293, #2485, #66969 ) ) ;
#35770 = ORIENTED_EDGE ( 'NONE', *, *, #73409, .F. ) ;
#35771 = LINE ( 'NONE', #43857, #100147 ) ;
#35772 = CARTESIAN_POINT ( 'NONE',  ( 79.83821995607597444, 57.92396234388704102, 16.26578674484267495 ) ) ;
#35773 = EDGE_CURVE ( 'NONE', #8702, #29478, #93863, .T. ) ;
#35774 = CARTESIAN_POINT ( 'NONE',  ( 85.76569060431222624, 48.58547048772101107, -11.83440413304170846 ) ) ;
#35775 = CARTESIAN_POINT ( 'NONE',  ( 175.5786161558440881, 290.9456444599823044, 2.588591708581580608 ) ) ;
#35776 = CARTESIAN_POINT ( 'NONE',  ( 153.4619471835925708, 264.8431057800031567, 16.95044998314351758 ) ) ;
#35777 = ADVANCED_FACE ( 'NONE', ( #17832 ), #16499, .F. ) ;
#35778 = AXIS2_PLACEMENT_3D ( 'NONE', #46050, #60252, #6586 ) ;
#35779 = CARTESIAN_POINT ( 'NONE',  ( 81.03696130064014369, 43.68575652313568725, -9.501319341590960477 ) ) ;
#35780 = CARTESIAN_POINT ( 'NONE',  ( 162.1260167985288376, 266.6785162637209510, 17.71249957499354366 ) ) ;
#35781 = CARTESIAN_POINT ( 'NONE',  ( 10.18907585680922878, 170.5643266524159571, -9.188101187500093303 ) ) ;
#35782 = CARTESIAN_POINT ( 'NONE',  ( 108.5912123618160763, 227.3768266524159856, -9.188101187500091527 ) ) ;
#35783 = DIRECTION ( 'NONE',  ( -0.4272584830711198545, -0.9041295198387040433, 0.000000000000000000 ) ) ;
#35784 = CARTESIAN_POINT ( 'NONE',  ( 183.5370458253748041, 294.2335165497496519, -7.795347451710910924 ) ) ;
#35785 = CARTESIAN_POINT ( 'NONE',  ( 79.12246707933677214, 57.02010426323071357, 16.20246513760482543 ) ) ;
#35786 = CARTESIAN_POINT ( 'NONE',  ( 81.53115339410010165, 41.92267797703283350, -7.515177224638171616 ) ) ;
#35787 = CARTESIAN_POINT ( 'NONE',  ( 193.7901930790854976, 294.9925349088783264, 14.24765323155741115 ) ) ;
#35788 = CARTESIAN_POINT ( 'NONE',  ( 147.9133274879049793, 274.4535970048112290, -9.359166267164972908 ) ) ;
#35789 = CARTESIAN_POINT ( 'NONE',  ( 84.80172950927561715, 50.19486025153376829, 13.34007759942640803 ) ) ;
#35790 = CARTESIAN_POINT ( 'NONE',  ( 196.1785470034112109, 266.7132032025372723, 8.042115761827414389 ) ) ;
#35791 = CARTESIAN_POINT ( 'NONE',  ( 170.7191605745771597, 286.8649585537148710, -9.393374115909271183 ) ) ;
#35792 = CARTESIAN_POINT ( 'NONE',  ( -6.662747857324019307, 100.5650415295849029, 1.836970198720990540E-15 ) ) ;
#35793 = B_SPLINE_CURVE_WITH_KNOTS ( 'NONE', 3,
 ( #50940, #65151, #27164, #4868, #43836, #19079, #58052, #35247, #96098, #81890 ),
 .UNSPECIFIED., .F., .F.,
 ( 4, 2, 2, 2, 4 ),
 ( 0.000000000000000000, 0.2500000000000000000, 0.5000000000000000000, 0.7500000000000000000, 1.000000000000000000 ),
 .UNSPECIFIED. ) ;
#35794 = CARTESIAN_POINT ( 'NONE',  ( -51.75017079496729622, 30.85748650210271293, 10.00000000000000000 ) ) ;
#35795 = EDGE_CURVE ( 'NONE', #15777, #23431, #82161, .T. ) ;
#35796 = DIRECTION ( 'NONE',  ( -1.000000000000000000, 0.000000000000000000, 0.000000000000000000 ) ) ;
#35797 = CARTESIAN_POINT ( 'NONE',  ( 91.40610752940987993, 214.3923013555409796, 4.594050593750050204 ) ) ;
#35798 = CARTESIAN_POINT ( 'NONE',  ( 3.825981621811214151, 23.18502408145589300, 5.678558825948277544 ) ) ;
#35799 = FACE_OUTER_BOUND ( 'NONE', #25002, .T. ) ;
#35801 = CARTESIAN_POINT ( 'NONE',  ( 152.4488546850150499, 266.5978334603062194, 15.77325388060940625 ) ) ;
#35800 = CARTESIAN_POINT ( 'NONE',  ( 196.3021893095863959, 290.6416298092292436, 17.45656988653421138 ) ) ;
#35802 = CARTESIAN_POINT ( 'NONE',  ( 149.7453127691109387, 271.2805054190442888, 12.04833158289322981 ) ) ;
#35803 = B_SPLINE_CURVE_WITH_KNOTS ( 'NONE', 3,
 ( #32937, #86701, #24348, #17757 ),
 .UNSPECIFIED., .F., .F.,
 ( 4, 4 ),
 ( 0.007593230830505486723, 0.01264584417670786519 ),
 .UNSPECIFIED. ) ;
#35804 = CARTESIAN_POINT ( 'NONE',  ( 75.64192366613818308, 65.38353595949358521, 14.29496885373930226 ) ) ;
#35805 = DIRECTION ( 'NONE',  ( -0.5078630399532132467, -0.8614378286617561109, 0.000000000000000000 ) ) ;
#35806 = CARTESIAN_POINT ( 'NONE',  ( 30.99092310034283315, 39.93396525600392977, 2.839279412974139660 ) ) ;
#35807 = CARTESIAN_POINT ( 'NONE',  ( 147.4563929227680603, 275.2450308873625886, -3.847749617713808412 ) ) ;
#35808 = CARTESIAN_POINT ( 'NONE',  ( 86.41066968851905017, 46.49022025137010417, -9.329619672313064882 ) ) ;
#35809 = VERTEX_POINT ( 'NONE', #66901 ) ;
#35810 = CARTESIAN_POINT ( 'NONE',  ( 25.38156110457203241, 15.44966523072494624, -2.296566073217252530E-15 ) ) ;
#35811 = CARTESIAN_POINT ( 'NONE',  ( -76.49344163160110099, 52.20945622995200353, -10.00000000000000000 ) ) ;
#35812 = CARTESIAN_POINT ( 'NONE',  ( 146.8574506849497538, 276.2824292740633041, -4.888313306692038118 ) ) ;
#35813 = CARTESIAN_POINT ( 'NONE',  ( 191.3641415966465900, 288.6821316927074008, -16.06258504083237071 ) ) ;
#35814 = ORIENTED_EDGE ( 'NONE', *, *, #27330, .F. ) ;
#35815 = CARTESIAN_POINT ( 'NONE',  ( 70.33479273767041207, 61.15449313193268210, 14.84539183123301775 ) ) ;
#35816 = CARTESIAN_POINT ( 'NONE',  ( -79.43448886220070904, 56.15136215343108717, 10.00000000000000000 ) ) ;
#35817 = DIRECTION ( 'NONE',  ( -0.8660254037844387076, -0.4999999999999998890, -0.000000000000000000 ) ) ;
#35818 = DIRECTION ( 'NONE',  ( 1.000000000000000000, 0.000000000000000000, 0.000000000000000000 ) ) ;
#35819 = CARTESIAN_POINT ( 'NONE',  ( 85.69563749947228359, 42.25122789774620458, -8.045052972278457832E-08 ) ) ;
#35820 = CARTESIAN_POINT ( 'NONE',  ( 138.7305270869972560, 244.2365022471902023, 10.00000000000009592 ) ) ;
#35821 = CARTESIAN_POINT ( 'NONE',  ( 157.0978663001774862, 258.5455091378672137, -17.31223197570816552 ) ) ;
#35822 = ORIENTED_EDGE ( 'NONE', *, *, #18261, .T. ) ;
#35823 = CARTESIAN_POINT ( 'NONE',  ( 82.63766857847271297, 46.45602455969778788, -12.04605856197770031 ) ) ;
#35824 = CARTESIAN_POINT ( 'NONE',  ( 169.5921219636811657, 248.4220618532164906, -1.949161244724071151 ) ) ;
#35825 = ORIENTED_EDGE ( 'NONE', *, *, #17435, .F. ) ;
#35826 = FACE_OUTER_BOUND ( 'NONE', #10197, .T. ) ;
#35827 = CARTESIAN_POINT ( 'NONE',  ( 81.66745758616980311, 42.31905251298808679, -8.034357111095493664 ) ) ;
#35828 = ORIENTED_EDGE ( 'NONE', *, *, #93311, .F. ) ;
#35829 = CARTESIAN_POINT ( 'NONE',  ( 77.30903763899321746, 63.28101462763900997, -15.19399449308598804 ) ) ;
#35830 = EDGE_LOOP ( 'NONE', ( #41221, #1809, #75107, #10231 ) ) ;
#35831 = CARTESIAN_POINT ( 'NONE',  ( 192.6276150426703850, 292.1813556936259033, 14.97627272081470018 ) ) ;
#35832 = CARTESIAN_POINT ( 'NONE',  ( 2.966658798487924908, 25.21091486745858035, 1.000260061240931054E-15 ) ) ;
#35833 = CARTESIAN_POINT ( 'NONE',  ( 150.1064787036151245, 245.2202760586659736, -5.415160957724236172E-17 ) ) ;
#35834 = CARTESIAN_POINT ( 'NONE',  ( 204.0439772608724525, 272.7860293576995900, 11.11986000170599453 ) ) ;
#35835 = CARTESIAN_POINT ( 'NONE',  ( 192.6636420411112169, 296.3681834598817773, -11.78089681376212638 ) ) ;
#35836 = EDGE_CURVE ( 'NONE', #72480, #22609, #35509, .T. ) ;
#35837 = B_SPLINE_CURVE_WITH_KNOTS ( 'NONE', 3,
 ( #7883, #24563, #92997, #93509 ),
 .UNSPECIFIED., .F., .F.,
 ( 4, 4 ),
 ( 0.006163542666752603802, 0.01183985020392103529 ),
 .UNSPECIFIED. ) ;
#35838 = CARTESIAN_POINT ( 'NONE',  ( 40.42517716772906056, 31.84335787977767041, 9.188101187500006262 ) ) ;
#35839 = CARTESIAN_POINT ( 'NONE',  ( 76.00075513927814086, 59.66202446853887409, -15.83865532722460578 ) ) ;
#35840 = CARTESIAN_POINT ( 'NONE',  ( 165.5076143076621520, 274.9436888840691040, 14.75253031382487556 ) ) ;
#35841 = CARTESIAN_POINT ( 'NONE',  ( -20.01211276271284945, 173.6868197944959036, 22.50000000000001421 ) ) ;
#35842 = ORIENTED_EDGE ( 'NONE', *, *, #88198, .T. ) ;
#35843 = AXIS2_PLACEMENT_3D ( 'NONE', #67088, #90452, #1193 ) ;
#35844 = ORIENTED_EDGE ( 'NONE', *, *, #68247, .T. ) ;
#35845 = CARTESIAN_POINT ( 'NONE',  ( 81.61509234124716272, 42.58397340471713477, 7.503678272258770043 ) ) ;
#35846 = B_SPLINE_CURVE_WITH_KNOTS ( 'NONE', 3,
 ( #45425, #53527, #8437, #54010, #16030, #46932, #91569, #99653, #54505, #76360, #84968, #22141, #15513, #53031, #6931, #829, #83985, #85483, #84478, #31223, #39305, #69727, #93566, #45911, #332, #76830, #46415, #7427, #77849, #100156, #30742, #92574, #61619, #23118, #24133, #80382, #32727, #96079, #33753, #63631, #71252, #95082, #56006, #25646, #1342, #10952, #32227, #9437 ),
 .UNSPECIFIED., .F., .F.,
 ( 4, 2, 2, 2, 2, 2, 2, 2, 2, 2, 2, 2, 2, 2, 2, 2, 2, 2, 2, 2, 2, 2, 2, 4 ),
 ( 0.0002180751697494367309, 0.0006991417601631947807, 0.001180208350576952966, 0.001420741645783869843, 0.001541008293387322210, 0.001661274940990775011, 0.001781541588594227378, 0.001901808236197679962, 0.002142341531404522680, 0.002623408121818276203, 0.003104474712232029726, 0.004066607893059384984, 0.005028741073886740243, 0.005509807664300423076, 0.005750340959507223293, 0.005870607607110583069, 0.005990874254713943713, 0.006051007578515663066, 0.006111140902317381551, 0.006231407549920868830, 0.006471940845127756650, 0.006953007435541381370, 0.007434074025955006090, 0.007915140616368630810 ),
 .UNSPECIFIED. ) ;
#35848 = CARTESIAN_POINT ( 'NONE',  ( 162.4690895575259901, 272.5881697659471570, -16.26466664224244241 ) ) ;
#35847 = DIRECTION ( 'NONE',  ( -0.8660254037844387076, -0.4999999999999998890, -0.000000000000000000 ) ) ;
#35849 = CARTESIAN_POINT ( 'NONE',  ( 85.48805828002734586, 48.64268271054365300, 12.46980397201070900 ) ) ;
#35850 = DIRECTION ( 'NONE',  ( 0.4999999999999992784, -0.8660254037844390407, 0.000000000000000000 ) ) ;
#35851 = CARTESIAN_POINT ( 'NONE',  ( 152.9052392069962991, 268.7302753513774860, -15.74331135679841687 ) ) ;
#35852 = CARTESIAN_POINT ( 'NONE',  ( 82.36398727104865713, 40.36718183008564154, 1.065671972821284230 ) ) ;
#35853 = DIRECTION ( 'NONE',  ( 0.2113248654051652076, 0.7886751345948035397, 0.5773502691896466033 ) ) ;
#35854 = CARTESIAN_POINT ( 'NONE',  ( 169.7687919401275565, 267.4058426616630300, 17.40508201545849687 ) ) ;
#35855 = DIRECTION ( 'NONE',  ( 0.8660254037844395958, 0.4999999999999985567, 0.000000000000000000 ) ) ;
#35856 = CARTESIAN_POINT ( 'NONE',  ( 100.4182711614829486, 216.5327760586659451, 1.948934522072303157E-15 ) ) ;
#35857 = CARTESIAN_POINT ( 'NONE',  ( 148.4958247551113288, 275.2668892720577105, -7.172227964493664842 ) ) ;
#35858 = CARTESIAN_POINT ( 'NONE',  ( 166.6214840706217046, 278.0950532397310440, -13.36420821935662318 ) ) ;
#35859 = VERTEX_POINT ( 'NONE', #26923 ) ;
#35860 = VERTEX_POINT ( 'NONE', #97830 ) ;
#35861 = CARTESIAN_POINT ( 'NONE',  ( 87.08174047714162214, 46.31017841404310786, -9.261312696178791271 ) ) ;
#35862 = CARTESIAN_POINT ( 'NONE',  ( -22.42236680055709641, 157.8615022471902591, 0.000000000000000000 ) ) ;
#35863 = CARTESIAN_POINT ( 'NONE',  ( 196.4390255720217908, 290.4046224503736653, 16.34739044515864848 ) ) ;
#35864 = CARTESIAN_POINT ( 'NONE',  ( 164.0212554996149379, 272.3286311233993615, -16.82199824294186286 ) ) ;
#35865 = CARTESIAN_POINT ( 'NONE',  ( 73.67824366217406862, 55.52431661998092238, 16.58293631993679540 ) ) ;
#35866 = ORIENTED_EDGE ( 'NONE', *, *, #23427, .F. ) ;
#35867 = ORIENTED_EDGE ( 'NONE', *, *, #20698, .F. ) ;
#35868 = LINE ( 'NONE', #82531, #51087 ) ;
#35869 = VERTEX_POINT ( 'NONE', #57802 ) ;
#35870 = B_SPLINE_CURVE_WITH_KNOTS ( 'NONE', 3,
 ( #10002, #86550, #9503, #40865, #94626, #26196, #87570, #39858, #72314, #2408, #32780, #63689, #63186, #40369 ),
 .UNSPECIFIED., .F., .F.,
 ( 4, 2, 2, 2, 2, 2, 4 ),
 ( 0.001036889160286317679, 0.001285291995625097812, 0.001533694830963879029, 0.001782097666302660246, 0.002030500501641441247, 0.002527306172318979395, 0.003024111842996517977 ),
 .UNSPECIFIED. ) ;
#35871 = CARTESIAN_POINT ( 'NONE',  ( 191.4659329597417923, 264.0196791935998135, -7.956612423567304582 ) ) ;
#35872 = CARTESIAN_POINT ( 'NONE',  ( 103.4423036115607601, 218.9824982072974251, 3.021315404115420679E-15 ) ) ;
#35873 = LINE ( 'NONE', #5483, #24123 ) ;
#35875 = CARTESIAN_POINT ( 'NONE',  ( 198.9438511131552332, 284.5686006854416519, 17.54420169616632563 ) ) ;
#35874 = CARTESIAN_POINT ( 'NONE',  ( 127.9681836757279001, 250.8149278399160949, 9.188101187500093303 ) ) ;
#35876 = FACE_OUTER_BOUND ( 'NONE', #35230, .T. ) ;
#35877 = ORIENTED_EDGE ( 'NONE', *, *, #22608, .F. ) ;
#35878 = CARTESIAN_POINT ( 'NONE',  ( 190.7569505155522904, 300.2462651405980978, -5.670926626284815697 ) ) ;
#35879 = CARTESIAN_POINT ( 'NONE',  ( 81.86216086620987653, 49.16130738973323844, 13.63634663801094327 ) ) ;
#35880 = CARTESIAN_POINT ( 'NONE',  ( 82.33378460754960315, 40.34433662615649041, -0.9934756154102190040 ) ) ;
#35881 = DIRECTION ( 'NONE',  ( 0.4924038765061026779, -0.8528685319524446085, -0.1736481776669273058 ) ) ;
#35882 = CARTESIAN_POINT ( 'NONE',  ( 178.5664908309598218, 285.2175874337613664, 13.98765452350090577 ) ) ;
#35883 = ADVANCED_FACE ( 'NONE', ( #88781, #19351, #42594 ), #96861, .F. ) ;
#35884 = CARTESIAN_POINT ( 'NONE',  ( 71.93253201618666992, 72.27632922802737880, 3.295383250428975064 ) ) ;
#35885 = CARTESIAN_POINT ( 'NONE',  ( 198.8109706115596964, 282.3938570165372539, -17.09471128148272356 ) ) ;
#35886 = EDGE_CURVE ( 'NONE', #16015, #24489, #66031, .T. ) ;
#35887 = DIRECTION ( 'NONE',  ( -0.7490285521785782219, 0.6625377181876236365, 0.000000000000000000 ) ) ;
#35888 = CARTESIAN_POINT ( 'NONE',  ( 80.60695466096186124, 53.05637191785592677, 15.52015733122538244 ) ) ;
#35889 = CARTESIAN_POINT ( 'NONE',  ( 67.58545467128371342, 69.55077376957733293, -1.347700640191054289 ) ) ;
#35890 = EDGE_CURVE ( 'NONE', #54644, #19179, #95144, .T. ) ;
#35891 = CARTESIAN_POINT ( 'NONE',  ( 58.44249495421716745, 213.7369531367911293, -4.594050593750048428 ) ) ;
#35892 = CARTESIAN_POINT ( 'NONE',  ( 159.5221561062548972, 254.3465160214695118, -16.91023001054109542 ) ) ;
#35893 = CARTESIAN_POINT ( 'NONE',  ( 77.61092910917922438, 61.85833765720148847, 15.65612403738310476 ) ) ;
#35894 = CARTESIAN_POINT ( 'NONE',  ( 187.3153774383709163, 290.1783631386096545, -14.94016741271708248 ) ) ;
#35895 = EDGE_CURVE ( 'NONE', #72875, #49563, #37976, .T. ) ;
#35896 = CARTESIAN_POINT ( 'NONE',  ( 46.22371820283660782, 112.7232458147606451, -10.00000000000000000 ) ) ;
#35898 = CARTESIAN_POINT ( 'NONE',  ( 185.9435401644106776, 265.4574032316044168, 13.60664360879022716 ) ) ;
#35897 = CARTESIAN_POINT ( 'NONE',  ( 73.70226580840751751, 69.60776679690043522, -9.655525091778702773 ) ) ;
#35899 = CARTESIAN_POINT ( 'NONE',  ( 15.82880751958831667, 10.10801979619927415, 3.090169943749476733 ) ) ;
#35900 = CARTESIAN_POINT ( 'NONE',  ( 35.84185148634745843, 32.64441083166263979, -10.00000000000000533 ) ) ;
#35901 = CARTESIAN_POINT ( 'NONE',  ( -22.42236680055709641, 157.8615022471902591, 0.000000000000000000 ) ) ;
#35902 = CARTESIAN_POINT ( 'NONE',  ( 82.07265110639774264, 53.99302234254209054, 15.59308437138325587 ) ) ;
#35903 = CARTESIAN_POINT ( 'NONE',  ( 71.66453512356649469, 72.11062924793525042, 3.341973230705647335 ) ) ;
#35904 = CARTESIAN_POINT ( 'NONE',  ( 6.805730253569997501, 183.9244531367911293, -4.594050593750046652 ) ) ;
#35905 = CARTESIAN_POINT ( 'NONE',  ( 70.73562432741556449, 71.76670644637469820, 2.397384686151506905 ) ) ;
#35906 = VERTEX_POINT ( 'NONE', #6103 ) ;
#35907 = CARTESIAN_POINT ( 'NONE',  ( 157.8740713127050981, 257.2010826190796706, 17.31862062017425075 ) ) ;
#35908 = CARTESIAN_POINT ( 'NONE',  ( 87.05137182546295094, 46.44927321608544446, 8.839680459623687980 ) ) ;
#35909 = CARTESIAN_POINT ( 'NONE',  ( 35.67350403664903524, 184.7365022471902023, -10.00000000000009237 ) ) ;
#35910 = CARTESIAN_POINT ( 'NONE',  ( 164.2090401137261892, 246.2285947913476889, -5.787448100099915393 ) ) ;
#35911 = CARTESIAN_POINT ( 'NONE',  ( 35.84185148634745843, 32.64441083166263979, -10.00000000000000533 ) ) ;
#35912 = CARTESIAN_POINT ( 'NONE',  ( 51.05482314576993730, 188.0327760586659451, 1.948934522072302763E-15 ) ) ;
#35913 = CARTESIAN_POINT ( 'NONE',  ( 86.86399242946149002, 45.94634269538593685, 8.946615921987719489 ) ) ;
#35914 = DIRECTION ( 'NONE',  ( 0.000000000000000000, 0.000000000000000000, -1.000000000000000000 ) ) ;
#35915 = CARTESIAN_POINT ( 'NONE',  ( 146.8195026170398023, 276.3481572557323034, 4.765869558735466249 ) ) ;
#35916 = CARTESIAN_POINT ( 'NONE',  ( 6.332637391379750014, 21.84336893147753855, -7.433330006724137462 ) ) ;
#35917 = CARTESIAN_POINT ( 'NONE',  ( -6.175261138941928962, 62.68629713672868320, -10.00000000000000000 ) ) ;
#35918 = CARTESIAN_POINT ( 'NONE',  ( 191.3413020738616410, 299.2341385521244774, -8.295023558158421295 ) ) ;
#35919 = CARTESIAN_POINT ( 'NONE',  ( 177.2780219866808977, 275.6134775628974580, 17.64509040511156357 ) ) ;
#35920 = CARTESIAN_POINT ( 'NONE',  ( 72.90981660445726220, 62.57208767169331054, 14.37557442138605523 ) ) ;
#35921 = CARTESIAN_POINT ( 'NONE',  ( 72.29738803710162642, 67.68364943355766172, -10.75058748413067633 ) ) ;
#35922 = CARTESIAN_POINT ( 'NONE',  ( 86.93590031418035835, 45.88516064952855089, -8.148499982929045871 ) ) ;
#35923 = CARTESIAN_POINT ( 'NONE',  ( 81.96547941067910870, 41.17040324926905015, 3.814626384468428721 ) ) ;
#35924 = CARTESIAN_POINT ( 'NONE',  ( 97.88299554183117834, 233.9865022471902876, -10.00000000000009415 ) ) ;
#35925 = CARTESIAN_POINT ( 'NONE',  ( 74.98858861178062796, 53.12804837913225953, 16.50569088578514254 ) ) ;
#35926 = CARTESIAN_POINT ( 'NONE',  ( 163.3405847382477702, 268.5890301281064012, -16.46197277963260674 ) ) ;
#35927 = ORIENTED_EDGE ( 'NONE', *, *, #94458, .F. ) ;
#35928 = CARTESIAN_POINT ( 'NONE',  ( 60.41820218054165537, 211.8149278399160664, 9.188101187500093303 ) ) ;
#35929 = ORIENTED_EDGE ( 'NONE', *, *, #53379, .F. ) ;
#35930 = CARTESIAN_POINT ( 'NONE',  ( 165.9205590267122830, 265.2445089552724085, 16.56339371490548729 ) ) ;
#35931 = CARTESIAN_POINT ( 'NONE',  ( 190.6218339396177441, 300.4802939150614520, -4.178005820806754755 ) ) ;
#35932 = CARTESIAN_POINT ( 'NONE',  ( 67.36400621912697773, 67.24424126167714633, -8.606104698649938101 ) ) ;
#35933 = ORIENTED_EDGE ( 'NONE', *, *, #42865, .F. ) ;
#35934 = CARTESIAN_POINT ( 'NONE',  ( 71.12873073640183463, 200.3262482093457777, 3.021315404115420679E-15 ) ) ;
#35935 = CARTESIAN_POINT ( 'NONE',  ( 207.6209998424140792, 271.0368748851258260, 6.610167240481342965 ) ) ;
#35936 = CYLINDRICAL_SURFACE ( 'NONE', #23295, 70.00000000000002842 ) ;
#35937 = CARTESIAN_POINT ( 'NONE',  ( 25.67147243227365294, 35.79752408145593989, -5.678558825948271327 ) ) ;
#35938 = CARTESIAN_POINT ( 'NONE',  ( 186.0008503584107871, 263.4848601604851410, 10.99485596832306378 ) ) ;
#35939 = CARTESIAN_POINT ( 'NONE',  ( 152.5994661946046449, 279.2824469453463507, 2.533033137138181345 ) ) ;
#35940 = ADVANCED_FACE ( 'NONE', ( #59792 ), #62582, .T. ) ;
#35941 = CARTESIAN_POINT ( 'NONE',  ( 156.7786475906069938, 259.0984121615696836, 17.12081851550279055 ) ) ;
#35943 = ORIENTED_EDGE ( 'NONE', *, *, #1510, .T. ) ;
#35942 = VECTOR ( 'NONE', #27967, 1000.000000000000000 ) ;
#35944 = CARTESIAN_POINT ( 'NONE',  ( 13.73114039420206645, 19.87878583063839955, -9.188101187500006262 ) ) ;
#35945 = DIRECTION ( 'NONE',  ( -1.000000000000000000, 0.000000000000000000, 0.000000000000000000 ) ) ;
#35946 = CARTESIAN_POINT ( 'NONE',  ( 66.90480444531253568, 69.14389213734473572, -1.488062147591796114 ) ) ;
#35947 = CARTESIAN_POINT ( 'NONE',  ( -19.65312891409030271, 93.06504152958497400, 60.00000000000000000 ) ) ;
#35948 = ORIENTED_EDGE ( 'NONE', *, *, #8799, .T. ) ;
#35949 = CARTESIAN_POINT ( 'NONE',  ( 182.5313270724992663, 283.9550808915877269, 15.13072720056265297 ) ) ;
#35950 = CARTESIAN_POINT ( 'NONE',  ( 24.94106359012611307, 66.84403333601011354, 59.99999999999999289 ) ) ;
#35951 = CARTESIAN_POINT ( 'NONE',  ( 206.8106726053982811, 272.4404028303941914, -10.47827087991598560 ) ) ;
#35952 = ORIENTED_EDGE ( 'NONE', *, *, #80742, .F. ) ;
#35954 = FACE_OUTER_BOUND ( 'NONE', #40942, .T. ) ;
#35953 = CARTESIAN_POINT ( 'NONE',  ( 207.1019571622349815, 271.9358831784929293, -5.989975140547304733 ) ) ;
#35955 = CARTESIAN_POINT ( 'NONE',  ( 47.46694519036043403, 73.19305994210745325, 10.00000000000000000 ) ) ;
#35956 = VERTEX_POINT ( 'NONE', #31388 ) ;
#35957 = CARTESIAN_POINT ( 'NONE',  ( 66.07036783887816966, 68.50746885787836504, -2.462010881573316823 ) ) ;
#35958 = CARTESIAN_POINT ( 'NONE',  ( 198.0792648159935538, 287.5636447432459022, 17.04758482866669667 ) ) ;
#35959 = CARTESIAN_POINT ( 'NONE',  ( 156.3551087084618700, 261.3239775484371989, -17.56576820129662053 ) ) ;
#35960 = CARTESIAN_POINT ( 'NONE',  ( 204.7775947223805417, 271.9956584674009719, 9.991586326987553335 ) ) ;
#35961 = EDGE_CURVE ( 'NONE', #52858, #39606, #76515, .T. ) ;
#35962 = CARTESIAN_POINT ( 'NONE',  ( 122.0685591603289026, 241.2833772461660544, -9.188101187500095079 ) ) ;
#35963 = DIRECTION ( 'NONE',  ( 0.2033683215378999376, -0.3522442655536480172, -0.9135454576426004225 ) ) ;
#35964 = VERTEX_POINT ( 'NONE', #10104 ) ;
#35965 = DIRECTION ( 'NONE',  ( -0.8492021815265757834, 0.5280678506503729830, 0.000000000000000000 ) ) ;
#35966 = ORIENTED_EDGE ( 'NONE', *, *, #51197, .F. ) ;
#35967 = EDGE_LOOP ( 'NONE', ( #15127, #81972, #84813, #34819 ) ) ;
#35968 = CARTESIAN_POINT ( 'NONE',  ( 198.5966822647444587, 286.6674514332866579, 17.25284514431582750 ) ) ;
#35969 = CARTESIAN_POINT ( 'NONE',  ( 92.93017357788669131, 158.0650415295850735, -36.50000000000000000 ) ) ;
#35970 = CARTESIAN_POINT ( 'NONE',  ( 79.20030167299918844, 216.5333772461660544, 9.188101187500095079 ) ) ;
#35971 = DIRECTION ( 'NONE',  ( 0.4999999999999992784, -0.8660254037844390407, 0.000000000000000000 ) ) ;
#35972 = SHAPE_REPRESENTATION ( 'Lower Tilting Cradle Base Segment', ( #68784 ), #2502 ) ;
#35973 = CARTESIAN_POINT ( 'NONE',  ( 81.76364840784469834, 55.63774643643142781, 16.32517576395870407 ) ) ;
#35974 = CARTESIAN_POINT ( 'NONE',  ( 150.8677798231829570, 269.3363354515693118, 13.85464777478129150 ) ) ;
#35975 = CARTESIAN_POINT ( 'NONE',  ( 173.0842668126385888, 277.1454467833098079, 15.65064250236792809 ) ) ;
#35976 = CARTESIAN_POINT ( 'NONE',  ( 182.1335790983844163, 257.1430377582902338, -6.167898280431136193 ) ) ;
#35977 = EDGE_LOOP ( 'NONE', ( #27628, #15298, #8090, #41684 ) ) ;
#35978 = CARTESIAN_POINT ( 'NONE',  ( 77.73560472764970086, 61.98338471776878578, -15.62265401182667546 ) ) ;
#35979 = CARTESIAN_POINT ( 'NONE',  ( 66.26615415756170080, 68.24338033411152082, 4.053640967902321535 ) ) ;
#35980 = CARTESIAN_POINT ( 'NONE',  ( 155.5066938333533528, 261.3015006940112244, -18.40036130547566273 ) ) ;
#35981 = ORIENTED_EDGE ( 'NONE', *, *, #72576, .F. ) ;
#35982 = FACE_OUTER_BOUND ( 'NONE', #92992, .T. ) ;
#35983 = CARTESIAN_POINT ( 'NONE',  ( 76.23362574048000795, 51.00037424386685814, -15.55159192653386846 ) ) ;
#35984 = CARTESIAN_POINT ( 'NONE',  ( 165.1088727524893329, 246.3087121452358303, 4.054724759575032422 ) ) ;
#35985 = DIRECTION ( 'NONE',  ( -0.2197389712097134185, -0.9755587037855265597, 0.000000000000000000 ) ) ;
#35986 = CARTESIAN_POINT ( 'NONE',  ( 149.0244553356880886, 274.5290671187512999, 9.114935767028397251 ) ) ;
#35987 = CARTESIAN_POINT ( 'NONE',  ( 149.2593905435863348, 272.1221474021800759, -12.98626158366800176 ) ) ;
#35988 = CARTESIAN_POINT ( 'NONE',  ( 194.9232784475534856, 279.6201759093600572, 16.73569595568872614 ) ) ;
#35989 = EDGE_LOOP ( 'NONE', ( #84137, #11550, #51942, #75272 ) ) ;
#35990 = CARTESIAN_POINT ( 'NONE',  ( 207.5215400641004351, 271.2091442744748520, 2.886080616848571534 ) ) ;
#35991 = CARTESIAN_POINT ( 'NONE',  ( 135.2211464324225858, 255.0024278399160949, -9.188101187500093303 ) ) ;
#35992 = VERTEX_POINT ( 'NONE', #78011 ) ;
#35993 = CARTESIAN_POINT ( 'NONE',  ( 88.08546139208640113, 44.41188104239807188, 4.690966480777963632 ) ) ;
#35994 = CARTESIAN_POINT ( 'NONE',  ( 182.7048629724877742, 257.5630761932868609, 6.780981931134482110 ) ) ;
#35995 = EDGE_CURVE ( 'NONE', #60500, #30119, #47090, .T. ) ;
#35996 = CARTESIAN_POINT ( 'NONE',  ( 79.89568642616896454, 44.56385848865007659, -11.10247427051291957 ) ) ;
#35997 = CARTESIAN_POINT ( 'NONE',  ( 204.8523313866422484, 275.8323493198358847, 14.65426965484541100 ) ) ;
#35998 = DIRECTION ( 'NONE',  ( -0.8660254037844387076, -0.4999999999999998890, -0.000000000000000000 ) ) ;
#35999 = CARTESIAN_POINT ( 'NONE',  ( 178.7223853007603793, 254.2491090711346260, 4.616854984815845775 ) ) ;
#36000 = ORIENTED_EDGE ( 'NONE', *, *, #66927, .F. ) ;
#36001 = CARTESIAN_POINT ( 'NONE',  ( 77.29002174012607895, 59.18083051215872814, 16.06399558427829888 ) ) ;
#36002 = CARTESIAN_POINT ( 'NONE',  ( 182.3945381577018736, 275.1057528038260784, -16.87030083329184649 ) ) ;
#36003 = CARTESIAN_POINT ( 'NONE',  ( 167.1998709608827767, 248.9378275210275149, -5.484025092681479308 ) ) ;
#36004 = CARTESIAN_POINT ( 'NONE',  ( 164.3104563928357322, 246.0529366432151051, -1.966241142131954334 ) ) ;
#36005 = CARTESIAN_POINT ( 'NONE',  ( 73.53265170616339219, 69.21111818949283645, -10.01235007243518282 ) ) ;
#36006 = CARTESIAN_POINT ( 'NONE',  ( 198.4846960687163460, 266.2207596311699263, 0.7325185302305462498 ) ) ;
#36007 = ADVANCED_FACE ( 'NONE', ( #16198 ), #8602, .F. ) ;
#36008 = CARTESIAN_POINT ( 'NONE',  ( 147.4811722709131914, 275.2021117973970377, 3.890385073228495916 ) ) ;
#36009 = CARTESIAN_POINT ( 'NONE',  ( 182.8590536091604406, 280.6449140202259969, 16.90169854257041848 ) ) ;
#36010 = AXIS2_PLACEMENT_3D ( 'NONE', #35064, #57868, #19890 ) ;
#36011 = CARTESIAN_POINT ( 'NONE',  ( 157.3661765229227285, 258.0807821998820373, -18.27254492731150748 ) ) ;
#36012 = CARTESIAN_POINT ( 'NONE',  ( 196.3706589808440981, 270.6234002145578756, 11.85799053031749040 ) ) ;
#36013 = B_SPLINE_SURFACE_WITH_KNOTS ( 'NONE', 3, 1, ( 
 ( #66730, #44423 ),
 ( #90591, #67227 ),
 ( #97663, #59105 ),
 ( #28737, #21637 ),
 ( #20646, #21156 ),
 ( #82975, #75352 ),
 ( #34825, #3942 ),
 ( #36826, #91074 ),
 ( #80997, #42421 ),
 ( #45897, #46404 ),
 ( #91558, #99642 ),
 ( #77840, #39294 ),
 ( #7935, #92563 ),
 ( #22127, #92081 ),
 ( #31694, #76347 ),
 ( #7415, #15008 ),
 ( #84959, #37808 ),
 ( #8423, #14033 ),
 ( #69216, #84468 ),
 ( #53020, #68217 ),
 ( #6921, #61108 ),
 ( #46918, #83973 ),
 ( #62602, #77328 ),
 ( #70206, #38307 ),
 ( #45415, #100144 ),
 ( #14537, #15502 ),
 ( #23601, #69714 ),
 ( #38809, #44913 ),
 ( #30730, #99142 ),
 ( #30224, #52520 ),
 ( #68718, #75857 ),
 ( #61609, #23107 ),
 ( #322, #22629 ),
 ( #29729, #53998 ) ),
 .UNSPECIFIED., .T., .F., .F.,
 ( 4, 2, 2, 2, 2, 2, 2, 2, 2, 2, 2, 2, 2, 2, 2, 2, 4 ),
 ( 2, 2 ),
 ( 0.000000000000000000, 0.06250000000000000000, 0.1250000000000000000, 0.1875000000000000000, 0.2500000000000000000, 0.3125000000000000000, 0.3750000000000000000, 0.4375000000000000000, 0.5000000000000000000, 0.5625000000000000000, 0.6250000000000000000, 0.6875000000000000000, 0.7500000000000000000, 0.8125000000000000000, 0.8750000000000000000, 0.9375000000000000000, 1.000000000000000000 ),
 ( 0.000000000000000000, 1.000000000000000000 ),
 .UNSPECIFIED. ) ;
#36014 = CARTESIAN_POINT ( 'NONE',  ( 16.78929260308981952, 21.64441083166260427, -10.00000000000000533 ) ) ;
#36015 = CARTESIAN_POINT ( 'NONE',  ( 149.6036070299368532, 271.5259469590175740, 11.63513718912356865 ) ) ;
#36016 = CARTESIAN_POINT ( 'NONE',  ( 204.8583870631589150, 274.3003082388789267, 12.05194970354070527 ) ) ;
#36017 = CARTESIAN_POINT ( 'NONE',  ( 159.4230536986738400, 254.5181664265525683, 16.83068086755798376 ) ) ;
#36018 = CARTESIAN_POINT ( 'NONE',  ( 72.24373504362831966, 72.05182877291241539, -3.239030724485916224 ) ) ;
#36019 = B_SPLINE_CURVE_WITH_KNOTS ( 'NONE', 3,
 ( #32601, #48815, #63499, #24991, #55867, #33610, #64506, #26017, #56888, #22250, #27986, #34116, #89359, #68348, #50291, #35595, #26512, #19913, #49796, #74113, #19436, #82246, #99273, #29856, #60726, #45046, #73124, #91688, #50784, #42189, #27007, #53153, #6565, #37437, #20410, #3715, #89834, #10812, #81245, #57893, #18923, #34595, #81734, #80760, #4706, #65494 ),
 .UNSPECIFIED., .F., .F.,
 ( 4, 1, 2, 2, 1, 2, 2, 1, 1, 2, 2, 1, 1, 2, 2, 1, 1, 2, 2, 1, 1, 1, 2, 2, 1, 1, 1, 2, 2, 4 ),
 ( 0.000000000000000000, 0.06249999999998788469, 0.09374999999998182010, 0.1249999999999757694, 0.1874999999999677758, 0.2187499999999636402, 0.2499999999999595324, 0.3124999999999504841, 0.3437499999999476530, 0.3593749999999477085, 0.3749999999999477640, 0.4374999999999529265, 0.4687499999999537037, 0.4843749999999523159, 0.4999999999999509281, 0.5624999999999494849, 0.5937499999999465983, 0.6093749999999452660, 0.6249999999999439337, 0.6874999999999414912, 0.7187499999999403810, 0.7343749999999413802, 0.7421874999999418243, 0.7499999999999422684, 0.8124999999999472644, 0.8437499999999513722, 0.8593749999999534817, 0.8671874999999562572, 0.8749999999999590328, 1.000000000000000000 ),
 .UNSPECIFIED. ) ;
#36020 = CARTESIAN_POINT ( 'NONE',  ( 145.7850256851100994, 241.6427522451417644, 1.119607411625061291E-15 ) ) ;
#36021 = CARTESIAN_POINT ( 'NONE',  ( 175.9868547499085025, 285.4643737892969853, -11.94532051846830534 ) ) ;
#36022 = ORIENTED_EDGE ( 'NONE', *, *, #44100, .F. ) ;
#36024 = CARTESIAN_POINT ( 'NONE',  ( 157.5710319558766344, 257.7259621817996162, 18.28704422422941533 ) ) ;
#36023 = AXIS2_PLACEMENT_3D ( 'NONE', #43210, #3264, #49836 ) ;
#36025 = CARTESIAN_POINT ( 'NONE',  ( 198.4782858197754649, 286.8725200914082620, -17.44895083299520522 ) ) ;
#36026 = CARTESIAN_POINT ( 'NONE',  ( 13.92363686274711299, 178.8458772461660544, 9.188101187500095079 ) ) ;
#36027 = CARTESIAN_POINT ( 'NONE',  ( 51.92050145378936321, 200.7833772461660828, -9.188101187500095079 ) ) ;
#36028 = CARTESIAN_POINT ( 'NONE',  ( 86.70911053808110580, 46.89117940024963360, 10.21290512048939547 ) ) ;
#36029 = CARTESIAN_POINT ( 'NONE',  ( 27.43138059761189496, 24.03677371833802923, 10.00000000000000533 ) ) ;
#36030 = CARTESIAN_POINT ( 'NONE',  ( 170.7953178271928039, 255.2457615276028093, -12.92277808742838374 ) ) ;
#36031 = CARTESIAN_POINT ( 'NONE',  ( 157.7733463334721478, 257.3755434007023268, -16.94489513499352995 ) ) ;
#36032 = CARTESIAN_POINT ( 'NONE',  ( 192.1286794796571940, 293.2256832552722017, -14.46936029153980918 ) ) ;
#36033 = CARTESIAN_POINT ( 'NONE',  ( 150.0733278132864541, 276.4838168200450355, 3.709811967872132410 ) ) ;
#36035 = CARTESIAN_POINT ( 'NONE',  ( 65.38900070045460211, 221.8927522451419350, 2.944929066748280225E-16 ) ) ;
#36034 = CARTESIAN_POINT ( 'NONE',  ( 167.4857222457644070, 256.6955868355478287, 13.86207597102780653 ) ) ;
#36036 = CARTESIAN_POINT ( 'NONE',  ( 75.12850925987632422, 67.10442048360499712, 12.66444045603761026 ) ) ;
#36037 = CARTESIAN_POINT ( 'NONE',  ( 198.7255181831150423, 286.4443010768291629, 17.42756903872921725 ) ) ;
#36038 = CARTESIAN_POINT ( 'NONE',  ( 49.89075441544353851, 199.6115022471902591, 10.00000000000009592 ) ) ;
#36039 = CARTESIAN_POINT ( 'NONE',  ( 181.8203573988056121, 291.6320214270799625, 9.291447165319489443 ) ) ;
#36040 = CARTESIAN_POINT ( 'NONE',  ( 163.3706531435203146, 247.6807236201477735, 10.06957846017757241 ) ) ;
#36041 = CARTESIAN_POINT ( 'NONE',  ( 18.76822678699008051, 172.4548013555409796, -4.594050593750042211 ) ) ;
#36042 = CARTESIAN_POINT ( 'NONE',  ( 167.9632374571382343, 286.8488433775840463, 5.051339247087953233 ) ) ;
#36043 = CARTESIAN_POINT ( 'NONE',  ( 3.558395312976033065, 182.8615022471903444, 5.000000000000046185 ) ) ;
#36044 = CARTESIAN_POINT ( 'NONE',  ( 41.44275701717577221, 32.43085787977767609, -9.188101187500008038 ) ) ;
#36045 = CARTESIAN_POINT ( 'NONE',  ( -56.29836151245349640, 34.88994676555962116, -10.00000000000000000 ) ) ;
#36046 = CARTESIAN_POINT ( 'NONE',  ( 164.9586510554008782, 244.9302305544571823, -1.717556444319656039 ) ) ;
#36047 = CARTESIAN_POINT ( 'NONE',  ( 21.39005255714673126, 24.30066082961421969, -10.00000000000000533 ) ) ;
#36048 = CARTESIAN_POINT ( 'NONE',  ( 153.2765620691255322, 265.6467114966280860, -16.15333212972641519 ) ) ;
#36049 = CARTESIAN_POINT ( 'NONE',  ( 178.5819917554228482, 262.0706330385751812, -12.89024234665558488 ) ) ;
#36050 = PRODUCT_CONTEXT ( 'NONE', #65412, 'mechanical' ) ;
#36051 = CARTESIAN_POINT ( 'NONE',  ( 14.44441505419593064, 16.84335787977761711, 9.188101187500006262 ) ) ;
#36052 = CARTESIAN_POINT ( 'NONE',  ( 71.64147408072076928, 72.45736481867631085, 0.9627058344235117637 ) ) ;
#36053 = LINE ( 'NONE', #44639, #14393 ) ;
#36054 = DIRECTION ( 'NONE',  ( 1.000000000000000000, 0.000000000000000000, 0.000000000000000000 ) ) ;
#36055 = EDGE_CURVE ( 'NONE', #59501, #83319, #93879, .T. ) ;
#36056 = CARTESIAN_POINT ( 'NONE',  ( 155.0929244053699847, 262.0181703658971628, 18.51426604808664678 ) ) ;
#36057 = ORIENTED_EDGE ( 'NONE', *, *, #67447, .T. ) ;
#36058 = DIRECTION ( 'NONE',  ( -0.000000000000000000, -0.000000000000000000, -1.000000000000000000 ) ) ;
#36059 = CARTESIAN_POINT ( 'NONE',  ( 156.7566617110267941, 276.4792909723148568, 10.26919381664546194 ) ) ;
#36060 = B_SPLINE_CURVE_WITH_KNOTS ( 'NONE', 3,
 ( #66989, #35603, #51810, #89368, #4199, #73617, #43691, #82752, #75118, #36086, #81745, #12318, #74631, #42686, #74124, #19922, #66007, #28490, #43181, #96958, #59371, #27523, #50795, #89845, #66501, #97427, #58876, #6193, #20419, #90850, #83227, #27997, #13319, #90348, #51286, #20927, #5694, #29493, #36584, #67489, #98419, #29012, #59883, #21403, #52286, #13793, #44672, #75605, #37088, #67992 ),
 .UNSPECIFIED., .F., .F.,
 ( 4, 2, 2, 2, 2, 2, 2, 2, 2, 2, 2, 2, 2, 2, 2, 2, 2, 2, 2, 2, 2, 2, 2, 2, 4 ),
 ( 0.0004617987126954396912, 0.0009154468224893198055, 0.001142270877386221753, 0.001369094932283123917, 0.001482506959731604273, 0.001595918987180085062, 0.001709331014628565418, 0.001822743042077045773, 0.002276391151870667522, 0.003183687371458009466, 0.004090983591045351843, 0.004998279810632693353, 0.005451927920426320739, 0.005678751975323090631, 0.005792164002771485118, 0.005848870016495731801, 0.005905576030219976749, 0.005962282043944223432, 0.006018988057668470115, 0.006132400085116827305, 0.006359224140013545155, 0.006812872249806967845, 0.007266520359600390534, 0.007493344414497106649, 0.007720168469393822765 ),
 .UNSPECIFIED. ) ;
#36061 = B_SPLINE_CURVE_WITH_KNOTS ( 'NONE', 3,
 ( #90393, #74168, #76163, #37617 ),
 .UNSPECIFIED., .F., .F.,
 ( 4, 4 ),
 ( 1.255848744284461856E-16, 0.002095492171155140856 ),
 .UNSPECIFIED. ) ;
#36062 = CARTESIAN_POINT ( 'NONE',  ( 81.35882998133553201, 42.02707565754876384, 7.853547620083842773 ) ) ;
#36063 = ADVANCED_FACE ( 'NONE', ( #9101 ), #70908, .F. ) ;
#36064 = VERTEX_POINT ( 'NONE', #40483 ) ;
#36065 = CARTESIAN_POINT ( 'NONE',  ( 72.26191451101281871, 71.91445694603925176, -5.118044210176698527 ) ) ;
#36066 = CARTESIAN_POINT ( 'NONE',  ( 81.40501017803065054, 206.2592609112379876, 2.679491924311254714 ) ) ;
#36067 = CARTESIAN_POINT ( 'NONE',  ( 66.46432511499183704, 68.67385870075324306, 4.823677987632845721 ) ) ;
#36068 = CARTESIAN_POINT ( 'NONE',  ( 155.6569868912636991, 261.0411854816857158, -17.75433477650897984 ) ) ;
#36069 = ORIENTED_EDGE ( 'NONE', *, *, #28692, .T. ) ;
#36070 = ORIENTED_EDGE ( 'NONE', *, *, #60429, .F. ) ;
#36072 = CARTESIAN_POINT ( 'NONE',  ( 204.3574891606595827, 276.6894411969685166, 13.41627538812899978 ) ) ;
#36071 = CARTESIAN_POINT ( 'NONE',  ( 159.5819137999480120, 278.9358841718408257, -9.468475011818437537 ) ) ;
#36073 = CARTESIAN_POINT ( 'NONE',  ( 153.3127735718713609, 265.1014820546527631, 17.57722645152040641 ) ) ;
#36074 = ORIENTED_EDGE ( 'NONE', *, *, #97454, .T. ) ;
#36075 = CARTESIAN_POINT ( 'NONE',  ( 88.23959751488011705, 43.87687695675944610, -2.120018653157903721 ) ) ;
#36076 = CARTESIAN_POINT ( 'NONE',  ( 80.42870892512175374, 57.78063267130219316, 16.59889063300756717 ) ) ;
#36077 = CARTESIAN_POINT ( 'NONE',  ( 174.3461956351267474, 262.5478167486214716, 14.75061405228954747 ) ) ;
#36079 = ADVANCED_FACE ( 'NONE', ( #2003 ), #32889, .T. ) ;
#36078 = ORIENTED_EDGE ( 'NONE', *, *, #60759, .F. ) ;
#36080 = CARTESIAN_POINT ( 'NONE',  ( 87.54964925812681997, 45.08772413541393576, -6.108523167108508289 ) ) ;
#36081 = ORIENTED_EDGE ( 'NONE', *, *, #54687, .F. ) ;
#36082 = CARTESIAN_POINT ( 'NONE',  ( 205.8452707775803390, 274.1125278458945900, 11.42742867493066328 ) ) ;
#36083 = CARTESIAN_POINT ( 'NONE',  ( 30.83629047462941486, 109.2621690313456924, 59.99999999999999289 ) ) ;
#36084 = ORIENTED_EDGE ( 'NONE', *, *, #19129, .F. ) ;
#36085 = CARTESIAN_POINT ( 'NONE',  ( 177.7120326079455594, 279.3125840650498617, -16.15421593783462484 ) ) ;
#36086 = CARTESIAN_POINT ( 'NONE',  ( 168.9473062510006116, 261.3660218479304831, -16.26153824055670327 ) ) ;
#36087 = VECTOR ( 'NONE', #58573, 1000.000000000000000 ) ;
#36088 = ORIENTED_EDGE ( 'NONE', *, *, #98481, .T. ) ;
#36089 = EDGE_CURVE ( 'NONE', #41047, #90969, #96739, .T. ) ;
#36090 = CARTESIAN_POINT ( 'NONE',  ( 34.99667586858890900, 35.90829794293883737, 10.00000000000000355 ) ) ;
#36091 = CARTESIAN_POINT ( 'NONE',  ( 192.4212750754384160, 297.3635704425909125, -12.73704185013552248 ) ) ;
#36092 = VERTEX_POINT ( 'NONE', #64299 ) ;
#36093 = CARTESIAN_POINT ( 'NONE',  ( 157.6602107013036402, 268.8732101254922213, 15.63420833100257212 ) ) ;
#36094 = ORIENTED_EDGE ( 'NONE', *, *, #56933, .T. ) ;
#36095 = CARTESIAN_POINT ( 'NONE',  ( 156.2392164662131790, 267.4395022997947535, -16.72994906840104790 ) ) ;
#36096 = CARTESIAN_POINT ( 'NONE',  ( 146.9324727656309335, 276.1524872186338371, 3.813717745456558728 ) ) ;
#36097 = CARTESIAN_POINT ( 'NONE',  ( 188.6207918642060406, 298.5847884678960895, -4.298219847241822933 ) ) ;
#36098 = DIRECTION ( 'NONE',  ( 0.000000000000000000, 0.000000000000000000, 1.000000000000000000 ) ) ;
#36099 = CARTESIAN_POINT ( 'NONE',  ( 153.1314981037513121, 265.4154603756023789, 17.73969815997475408 ) ) ;
#36100 = CARTESIAN_POINT ( 'NONE',  ( 31.19903945042937465, 195.4865022471903160, 10.00000000000009415 ) ) ;
#36101 = CARTESIAN_POINT ( 'NONE',  ( 146.8859094598974480, 276.2331372299326517, -0.7994986043261681496 ) ) ;
#36102 = ORIENTED_EDGE ( 'NONE', *, *, #28240, .F. ) ;
#36103 = CARTESIAN_POINT ( 'NONE',  ( 74.16082345638017159, 57.99061582411809468, -15.91439080673301731 ) ) ;
#36105 = CARTESIAN_POINT ( 'NONE',  ( 206.1215120922853146, 273.6340638536760821, 10.12238414215620885 ) ) ;
#36104 = CARTESIAN_POINT ( 'NONE',  ( 149.1486417047969155, 272.3139700178423368, -11.47583619705022606 ) ) ;
#36107 = ORIENTED_EDGE ( 'NONE', *, *, #16674, .F. ) ;
#36106 = CARTESIAN_POINT ( 'NONE',  ( 198.4334039703542771, 286.9502577349437615, 18.47706603442866680 ) ) ;
#36108 = CARTESIAN_POINT ( 'NONE',  ( 167.9901196014850484, 286.8200544026590251, 3.506790081298479134 ) ) ;
#36109 = CARTESIAN_POINT ( 'NONE',  ( 177.2041192817024182, 288.9686198354513635, -9.145765595030599826 ) ) ;
#36110 = ORIENTED_EDGE ( 'NONE', *, *, #87057, .F. ) ;
#36111 = ADVANCED_FACE ( 'NONE', ( #35386 ), #26306, .T. ) ;
#36112 = CARTESIAN_POINT ( 'NONE',  ( 71.31535561598460049, 67.97248318114000654, 9.859851264107916791 ) ) ;
#36113 = EDGE_CURVE ( 'NONE', #7411, #84127, #19226, .T. ) ;
#36114 = CARTESIAN_POINT ( 'NONE',  ( 84.02521314179199408, 41.77600783192887945, 3.730838443793543568 ) ) ;
#36115 = CARTESIAN_POINT ( 'NONE',  ( 199.3683090308842907, 285.3309546698520762, -17.40861982076147285 ) ) ;
#36116 = DIRECTION ( 'NONE',  ( -0.000000000000000000, 0.000000000000000000, -1.000000000000000000 ) ) ;
#36117 = ORIENTED_EDGE ( 'NONE', *, *, #7089, .F. ) ;
#36119 = EDGE_CURVE ( 'NONE', #65992, #66239, #33834, .T. ) ;
#36118 = CARTESIAN_POINT ( 'NONE',  ( 169.6774685567663710, 254.9819702002519932, -11.65141391084731026 ) ) ;
#36120 = CARTESIAN_POINT ( 'NONE',  ( 84.67893657527464768, 44.90132223245755227, 9.238919453567655538 ) ) ;
#36121 = CARTESIAN_POINT ( 'NONE',  ( 200.8251833487811666, 282.8075743310126882, -16.74393672780000131 ) ) ;
#36122 = CARTESIAN_POINT ( 'NONE',  ( 206.9408877595175511, 272.2148635675444552, 6.707071080545934372 ) ) ;
#36123 = CARTESIAN_POINT ( 'NONE',  ( 30.24280306353617576, 188.2677522451418497, 10.00000000000009592 ) ) ;
#36124 = CARTESIAN_POINT ( 'NONE',  ( 126.3990332750161087, 231.5327760586659736, 1.948934522072302763E-15 ) ) ;
#36125 = CARTESIAN_POINT ( 'NONE',  ( 180.8688118873734254, 294.1367794693202313, -2.657154044881775867 ) ) ;
#36126 = ADVANCED_FACE ( 'NONE', ( #41480 ), #50096, .F. ) ;
#36127 = CARTESIAN_POINT ( 'NONE',  ( 167.8634577855056875, 282.1373012281606520, -10.74177425913053163 ) ) ;
#36128 = CARTESIAN_POINT ( 'NONE',  ( 100.5532405368332007, 228.8615022471902591, -10.00000000000009592 ) ) ;
#36129 = CARTESIAN_POINT ( 'NONE',  ( 162.4993287900620942, 249.1899016702093661, 10.54298717179175071 ) ) ;
#36130 = CARTESIAN_POINT ( 'NONE',  ( 45.85867072306329817, 185.0327760586659451, 1.948934522072303157E-15 ) ) ;
#36131 = DIRECTION ( 'NONE',  ( -0.9522021074858073586, -0.3054687324417786343, 0.000000000000000000 ) ) ;
#36132 = ORIENTED_EDGE ( 'NONE', *, *, #32635, .T. ) ;
#36134 = EDGE_CURVE ( 'NONE', #67607, #87878, #77506, .T. ) ;
#36133 = DIRECTION ( 'NONE',  ( 0.000000000000000000, 0.000000000000000000, 1.000000000000000000 ) ) ;
#36135 = CARTESIAN_POINT ( 'NONE',  ( 178.0914043118813765, 265.4878125568229166, 15.91409428133586168 ) ) ;
#36136 = EDGE_CURVE ( 'NONE', #91686, #48945, #80811, .T. ) ;
#36137 = CARTESIAN_POINT ( 'NONE',  ( 69.57285913202781558, 70.79546693701125548, 0.5177190112630815078 ) ) ;
#36138 = CARTESIAN_POINT ( 'NONE',  ( 146.8516045228164160, 276.2925551239072774, 3.995954059407343273 ) ) ;
#36139 = CARTESIAN_POINT ( 'NONE',  ( 81.86430770026659332, 41.23265223418440684, -5.767287080406577893 ) ) ;
#36140 = CARTESIAN_POINT ( 'NONE',  ( 10.70626499057286196, 14.38052372038638893, 10.00000000000000533 ) ) ;
#36141 = CARTESIAN_POINT ( 'NONE',  ( 179.2274323333295740, 287.9912526978436063, -12.78748593997733352 ) ) ;
#36142 = CARTESIAN_POINT ( 'NONE',  ( 164.1808077535702921, 250.0262784942443091, 10.25442190752840865 ) ) ;
#36143 = CARTESIAN_POINT ( 'NONE',  ( 91.29759403033908427, 223.5177522451418781, -10.00000000000009592 ) ) ;
#36144 = B_SPLINE_CURVE_WITH_KNOTS ( 'NONE', 3,
 ( #66928, #20860, #11276, #13259, #44119, #36526, #42137, #73068, #3666, #34544, #44613, #6643, #30928, #37518, #61319, #45614, #99351, #46618, #60806, #84670, #15212, #91766, #21833, #7627, #22331, #53230, #90790, #38518, #84182, #44, #54205, #85173, #15717, #39012, #77548, #69918, #6133, #52226, #28947, #59825, #52718, #21342, #83171, #37030, #67938, #47121, #2548, #48125, #47619, #9134 ),
 .UNSPECIFIED., .F., .F.,
 ( 4, 2, 2, 2, 2, 2, 2, 2, 2, 2, 2, 2, 2, 2, 2, 2, 2, 2, 2, 2, 2, 2, 2, 2, 4 ),
 ( 0.0004837326417408448816, 0.001489169143744289948, 0.001991887394746087725, 0.002117566957496566822, 0.002243246520247045919, 0.002368926082997524583, 0.002494605645748003246, 0.002745964771248944961, 0.002997323896749886675, 0.003500042147751701582, 0.004505478649755411194, 0.005510915151759121673, 0.006013633402760975612, 0.006264992528261860948, 0.006516351653762746284, 0.006579191435137916877, 0.006642031216513087470, 0.006704870997888258931, 0.006767710779263429524, 0.007019069904763931486, 0.007521788155764807908, 0.007773147281265280380, 0.008024506406765751984, 0.008275865532266224456, 0.008527224657766695193 ),
 .UNSPECIFIED. ) ;
#36145 = VERTEX_POINT ( 'NONE', #80544 ) ;
#36146 = CARTESIAN_POINT ( 'NONE',  ( 196.0351912666876615, 267.0317724427966368, -7.782412515619550497 ) ) ;
#36147 = CARTESIAN_POINT ( 'NONE',  ( 155.4523213358487794, 279.7030401036391254, -1.715928067515927413 ) ) ;
#36148 = CARTESIAN_POINT ( 'NONE',  ( 162.6757594134126350, 248.8843148665554281, -10.86406770146305867 ) ) ;
#36149 = CLOSED_SHELL ( 'NONE', ( #5593, #58964, #22914, #21404, #10394, #9002, #3354, #93783, #48551, #43723, #72414, #47780, #49821, #8055, #72966 ) ) ;
#36150 = CARTESIAN_POINT ( 'NONE',  ( 13.46382118881039602, 169.3923013555410080, 4.594050593750050204 ) ) ;
#36151 = CARTESIAN_POINT ( 'NONE',  ( 5.995650155809630455, 19.16454794089039382, -10.00000000000000355 ) ) ;
#36152 = CARTESIAN_POINT ( 'NONE',  ( 80.95016728299943054, 53.58696901841446447, 16.00970915675678796 ) ) ;
#36153 = CARTESIAN_POINT ( 'NONE',  ( 71.80310585937155565, 59.28703135751661790, -15.30483328490166706 ) ) ;
#36154 = CARTESIAN_POINT ( 'NONE',  ( 73.63016447670500497, 69.73264996670253879, 9.457047152984245031 ) ) ;
#36155 = CARTESIAN_POINT ( 'NONE',  ( 48.80796233711527776, 208.1744531367911293, 4.594050593750047540 ) ) ;
#36156 = CARTESIAN_POINT ( 'NONE',  ( 196.1985894344492465, 280.6689076705129651, 17.57724957243723551 ) ) ;
#36157 = CARTESIAN_POINT ( 'NONE',  ( 204.9780665305064531, 275.6145696623662502, 14.10615427165218883 ) ) ;
#36158 = CARTESIAN_POINT ( 'NONE',  ( 186.2798660816079632, 264.0713031700501006, -12.82791401631097550 ) ) ;
#36159 = CARTESIAN_POINT ( 'NONE',  ( 66.36918592400230921, 68.05458625204849454, -4.804853499357824020 ) ) ;
#36160 = ORIENTED_EDGE ( 'NONE', *, *, #20042, .T. ) ;
#36161 = CARTESIAN_POINT ( 'NONE',  ( 17.41480177352709191, 180.8615022471902591, -10.00000000000009592 ) ) ;
#36162 = DIRECTION ( 'NONE',  ( -0.000000000000000000, -0.000000000000000000, -1.000000000000000000 ) ) ;
#36163 = VECTOR ( 'NONE', #52380, 1000.000000000000000 ) ;
#36164 = CARTESIAN_POINT ( 'NONE',  ( 127.8056303646358032, 256.8464784336661637, 1.353441290958777327E-15 ) ) ;
#36165 = CARTESIAN_POINT ( 'NONE',  ( 18.69336236660381090, 32.83396525600390703, -2.839279412974133887 ) ) ;
#36166 = CARTESIAN_POINT ( 'NONE',  ( 164.8719015746727621, 245.0804850626086022, 0.9827678719136201391 ) ) ;
#36167 = DIRECTION ( 'NONE',  ( -0.8660254037844387076, -0.4999999999999998890, -0.000000000000000000 ) ) ;
#36168 = DIRECTION ( 'NONE',  ( -0.7235470741700464892, -0.1663964660674591423, -0.6699192843471715175 ) ) ;
#36169 = VECTOR ( 'NONE', #158, 1000.000000000000000 ) ;
#36171 = CARTESIAN_POINT ( 'NONE',  ( 74.76437051368166919, 67.10386306624577912, 12.96231939749656270 ) ) ;
#36170 = CARTESIAN_POINT ( 'NONE',  ( 196.4982648257524147, 290.3020170531091821, 16.69353242256149628 ) ) ;
#36172 = CARTESIAN_POINT ( 'NONE',  ( 69.11514122063265120, 64.27165015964561690, 12.02313996166621024 ) ) ;
#36173 = ORIENTED_EDGE ( 'NONE', *, *, #70539, .T. ) ;
#36174 = CARTESIAN_POINT ( 'NONE',  ( 191.0816511748900268, 299.6838671013740623, 7.311127128005925790 ) ) ;
#36175 = CARTESIAN_POINT ( 'NONE',  ( 207.6937983729889368, 270.9107841314541929, -1.514855854672175761 ) ) ;
#36176 = CARTESIAN_POINT ( 'NONE',  ( 68.82950249375011254, 67.23871426837432352, -9.720984335491779760 ) ) ;
#36177 = CARTESIAN_POINT ( 'NONE',  ( 172.9630369837942965, 268.1244351977575207, -16.30034978024972858 ) ) ;
#36178 = CARTESIAN_POINT ( 'NONE',  ( 195.4726663938093054, 272.0961244453007453, -13.40964562940238913 ) ) ;
#36179 = ORIENTED_EDGE ( 'NONE', *, *, #62011, .T. ) ;
#36180 = CARTESIAN_POINT ( 'NONE',  ( 71.11409818138567118, 70.51317934531886067, 5.732207205114195681 ) ) ;
#36181 = CARTESIAN_POINT ( 'NONE',  ( -86.81108781737714253, 10.00000000000000178, 0.000000000000000000 ) ) ;
#36182 = CARTESIAN_POINT ( 'NONE',  ( 83.03454124716056128, 41.89555541620175205, 4.196031385176040018 ) ) ;
#36183 = CYLINDRICAL_SURFACE ( 'NONE', #35843, 10.00000000000010658 ) ;
#36184 = CARTESIAN_POINT ( 'NONE',  ( 182.0881301589248551, 295.0157003455848894, 4.784192560878642198 ) ) ;
#36185 = CARTESIAN_POINT ( 'NONE',  ( 163.0424334805279045, 248.2492167524936804, -9.671494865076915914 ) ) ;
#36186 = DIRECTION ( 'NONE',  ( -0.8660254037844377084, -0.5000000000000014433, -0.000000000000000000 ) ) ;
#36187 = CARTESIAN_POINT ( 'NONE',  ( 25.96864935082050252, 154.0458036431183189, -22.49999999999984013 ) ) ;
#36188 = CYLINDRICAL_SURFACE ( 'NONE', #17933, 3.300000000000010925 ) ;
#36189 = CARTESIAN_POINT ( 'NONE',  ( 10.64836937555893570, 29.08080186712591697, -3.090169943749475845 ) ) ;
#36190 = DIRECTION ( 'NONE',  ( -0.4621356007560455392, 0.8868092729070038427, 0.000000000000000000 ) ) ;
#36191 = ORIENTED_EDGE ( 'NONE', *, *, #35652, .T. ) ;
#36192 = CARTESIAN_POINT ( 'NONE',  ( 164.2981700896163773, 253.9203781951923133, 14.63367134977796802 ) ) ;
#36193 = CARTESIAN_POINT ( 'NONE',  ( 86.50731970396800818, 47.43598145919347786, -10.90780039058066997 ) ) ;
#36194 = CARTESIAN_POINT ( 'NONE',  ( 156.1569981892633621, 261.6699882273320554, -17.05379912710613510 ) ) ;
#36196 = EDGE_CURVE ( 'NONE', #81759, #86838, #50011, .T. ) ;
#36195 = VERTEX_POINT ( 'NONE', #11122 ) ;
#36197 = CARTESIAN_POINT ( 'NONE',  ( 147.3047606266276546, 275.5076657283461827, -0.02269072295920609994 ) ) ;
#36198 = CARTESIAN_POINT ( 'NONE',  ( 185.1256672880319911, 291.5517695480672842, 11.95305935706613276 ) ) ;
#36199 = CARTESIAN_POINT ( 'NONE',  ( 204.7235752877335244, 276.0553614249301972, 14.82397698933823271 ) ) ;
#36200 = DIRECTION ( 'NONE',  ( -5.984665299743594308E-16, 0.000000000000000000, -1.000000000000000000 ) ) ;
#36201 = CARTESIAN_POINT ( 'NONE',  ( 189.5698839646237843, 268.9756110371309887, -14.78084782106435391 ) ) ;
#36202 = VERTEX_POINT ( 'NONE', #3519 ) ;
#36203 = CARTESIAN_POINT ( 'NONE',  ( 92.94880205384217220, 212.2202760586659167, -5.415160957724236172E-17 ) ) ;
#36204 = CARTESIAN_POINT ( 'NONE',  ( 155.4641461872872981, 261.3751953787398179, 17.01821821352853092 ) ) ;
#36205 = CARTESIAN_POINT ( 'NONE',  ( 73.29675513422920119, 69.64584746942686877, -9.922798968680028864 ) ) ;
#36206 = CARTESIAN_POINT ( 'NONE',  ( 181.2844587369501141, 271.1666661326591452, -15.98216304377438490 ) ) ;
#36207 = CARTESIAN_POINT ( 'NONE',  ( 185.6377146029830385, 259.0204853581686280, -6.791722753532964951 ) ) ;
#36208 = VERTEX_POINT ( 'NONE', #19717 ) ;
#36209 = ADVANCED_FACE ( 'NONE', ( #74421 ), #5006, .T. ) ;
#36210 = ORIENTED_EDGE ( 'NONE', *, *, #93638, .F. ) ;
#36211 = B_SPLINE_CURVE_WITH_KNOTS ( 'NONE', 3,
 ( #63612, #71237, #16512, #94058 ),
 .UNSPECIFIED., .F., .F.,
 ( 4, 4 ),
 ( 0.03345425586890212605, 0.04234520293996446583 ),
 .UNSPECIFIED. ) ;
#36212 = CARTESIAN_POINT ( 'NONE',  ( -3.965200385949115169, 158.5177522451418213, 5.000000000000051514 ) ) ;
#36213 = EDGE_CURVE ( 'NONE', #4429, #23644, #96237, .T. ) ;
#36214 = EDGE_LOOP ( 'NONE', ( #25008, #22123, #56999, #91439 ) ) ;
#36215 = CARTESIAN_POINT ( 'NONE',  ( 81.76857307223471594, 51.79620215026877617, 14.92011331900278925 ) ) ;
#36216 = ORIENTED_EDGE ( 'NONE', *, *, #24872, .F. ) ;
#36217 = CARTESIAN_POINT ( 'NONE',  ( 75.40712543759373432, 60.69022127545543555, 15.54263831071833479 ) ) ;
#36218 = CARTESIAN_POINT ( 'NONE',  ( 155.3716771045260714, 261.5353565282119348, -18.54934131471355840 ) ) ;
#36219 = VERTEX_POINT ( 'NONE', #11615 ) ;
#36220 = CARTESIAN_POINT ( 'NONE',  ( 182.9620665166839899, 279.7200058654210579, -17.04853919723895572 ) ) ;
#36221 = DIRECTION ( 'NONE',  ( -0.2837547813814367825, -0.9281390619545411003, 0.2409172175609656796 ) ) ;
#36222 = CARTESIAN_POINT ( 'NONE',  ( 201.0356089830534643, 282.4431064412383989, -18.18835788025466371 ) ) ;
#36223 = CARTESIAN_POINT ( 'NONE',  ( -23.53961575219861402, 99.77347671786461092, 45.19948544083312214 ) ) ;
#36224 = CARTESIAN_POINT ( 'NONE',  ( 71.50952208868150706, 68.35890179303125080, -9.555329829617408066 ) ) ;
#36225 = CARTESIAN_POINT ( 'NONE',  ( 166.1354066105388654, 265.9557281117362209, -16.63352449353996576 ) ) ;
#36226 = ORIENTED_EDGE ( 'NONE', *, *, #14543, .F. ) ;
#36227 = CARTESIAN_POINT ( 'NONE',  ( 76.18443605400364049, 57.11110936434808849, 16.13045278074740452 ) ) ;
#36228 = CARTESIAN_POINT ( 'NONE',  ( 8.534987971495436199, 16.87878583063839599, -9.188101187500006262 ) ) ;
#36229 = ORIENTED_EDGE ( 'NONE', *, *, #64011, .T. ) ;
#36230 = CARTESIAN_POINT ( 'NONE',  ( 167.4082149272132085, 284.2775854637627049, 9.280720086700116056 ) ) ;
#36232 = EDGE_LOOP ( 'NONE', ( #69268, #100182, #52508, #72395, #16543 ) ) ;
#36231 = CARTESIAN_POINT ( 'NONE',  ( 201.1438721331022350, 270.7680306690247676, 9.304748580235882471 ) ) ;
#36233 = CARTESIAN_POINT ( 'NONE',  ( -15.75121124376761905, 105.6236688776997710, 11.47872565613448614 ) ) ;
#36234 = DIRECTION ( 'NONE',  ( 0.8660254037844387076, 0.4999999999999998890, 0.000000000000000000 ) ) ;
#36235 = LINE ( 'NONE', #45810, #99710 ) ;
#36236 = CARTESIAN_POINT ( 'NONE',  ( 161.1037025896568764, 281.9537687873744289, -6.124960680995634732 ) ) ;
#36237 = CARTESIAN_POINT ( 'NONE',  ( 177.3334602733804104, 257.8359255682534581, -11.87082999068797484 ) ) ;
#36238 = CARTESIAN_POINT ( 'NONE',  ( 157.7111038903397571, 257.9445160749222055, 16.71092927711721998 ) ) ;
#36239 = VECTOR ( 'NONE', #21167, 1000.000000000000227 ) ;
#36240 = CARTESIAN_POINT ( 'NONE',  ( 85.58674419670936118, 42.96232126506118476, 2.800701338658758921 ) ) ;
#36241 = CARTESIAN_POINT ( 'NONE',  ( 88.44819812734249354, 44.06706281553302773, -2.545729839345954204 ) ) ;
#36242 = ORIENTED_EDGE ( 'NONE', *, *, #85069, .F. ) ;
#36244 = ADVANCED_FACE ( 'NONE', ( #81532 ), #57682, .F. ) ;
#36243 = CARTESIAN_POINT ( 'NONE',  ( 181.8129903383622263, 270.5352787916219199, -16.24512204374439861 ) ) ;
#36245 = CARTESIAN_POINT ( 'NONE',  ( 71.28447224701196205, 63.33288523720543850, -13.51654472431917497 ) ) ;
#36246 = VERTEX_POINT ( 'NONE', #73410 ) ;
#36247 = CARTESIAN_POINT ( 'NONE',  ( 193.1030321335636586, 294.1827325794992021, -14.54662778306917481 ) ) ;
#36248 = AXIS2_PLACEMENT_3D ( 'NONE', #64631, #9423, #64118 ) ;
#36249 = EDGE_CURVE ( 'NONE', #39006, #49112, #49169, .T. ) ;
#36250 = CARTESIAN_POINT ( 'NONE',  ( 193.5354321533228301, 263.1006045986919730, 5.857068979672426678 ) ) ;
#36251 = CARTESIAN_POINT ( 'NONE',  ( 32.30839531297598910, 123.0650415295850593, -40.00000000000000000 ) ) ;
#36252 = CARTESIAN_POINT ( 'NONE',  ( 87.69503266575394207, 44.73314950816818936, -5.003925075596086458 ) ) ;
#36253 = CARTESIAN_POINT ( 'NONE',  ( 160.8894027367712454, 272.6494381571178565, 15.39890601372860957 ) ) ;
#36255 = CARTESIAN_POINT ( 'NONE',  ( 88.03161368674544462, 43.80918251920726902, 2.446934266190721186 ) ) ;
#36254 = CARTESIAN_POINT ( 'NONE',  ( -0.9067010812963882671, 158.0327760586659451, 1.948934522072303157E-15 ) ) ;
#36256 = CARTESIAN_POINT ( 'NONE',  ( 189.0443830094626207, 297.0343580855736150, 8.140033191741938623 ) ) ;
#36257 = ORIENTED_EDGE ( 'NONE', *, *, #38257, .F. ) ;
#36258 = EDGE_CURVE ( 'NONE', #47682, #17413, #87675, .T. ) ;
#36259 = B_SPLINE_SURFACE_WITH_KNOTS ( 'NONE', 3, 1, ( 
 ( #40562, #63379 ),
 ( #10190, #17793 ),
 ( #96316, #81129 ),
 ( #94318, #80125 ),
 ( #41056, #26387 ),
 ( #10687, #71498 ),
 ( #71992, #88240 ),
 ( #19311, #2598 ),
 ( #42073, #26884 ),
 ( #3117, #17274 ),
 ( #88739, #41566 ),
 ( #50176, #73006 ),
 ( #80628, #2092 ),
 ( #70997, #33483 ),
 ( #79122, #34476 ),
 ( #3595, #18791 ),
 ( #95343, #87259 ),
 ( #25900, #72509 ),
 ( #25375, #56773 ),
 ( #24873, #11203 ),
 ( #1600, #32969 ),
 ( #49671, #57763 ),
 ( #65374, #32484 ),
 ( #63877, #11696 ),
 ( #55746, #94813 ),
 ( #87754, #56266 ),
 ( #79627, #34003 ),
 ( #64888, #57265 ),
 ( #22140, #22640 ),
 ( #6930, #36837 ),
 ( #29739, #29251 ),
 ( #44922, #12184 ),
 ( #42555, #21647 ),
 ( #60119, #73489 ) ),
 .UNSPECIFIED., .T., .F., .F.,
 ( 4, 2, 2, 2, 2, 2, 2, 2, 2, 2, 2, 2, 2, 2, 2, 2, 4 ),
 ( 2, 2 ),
 ( 0.000000000000000000, 0.06250000000000000000, 0.1250000000000000000, 0.1875000000000000000, 0.2500000000000000000, 0.3125000000000000000, 0.3750000000000000000, 0.4375000000000000000, 0.5000000000000000000, 0.5625000000000000000, 0.6250000000000000000, 0.6875000000000000000, 0.7500000000000000000, 0.8125000000000000000, 0.8750000000000000000, 0.9375000000000000000, 1.000000000000000000 ),
 ( 0.000000000000000000, 1.000000000000000000 ),
 .UNSPECIFIED. ) ;
#36261 = ORIENTED_EDGE ( 'NONE', *, *, #71633, .F. ) ;
#36260 = B_SPLINE_CURVE_WITH_KNOTS ( 'NONE', 3,
 ( #34526, #80174, #73051, #81664 ),
 .UNSPECIFIED., .F., .F.,
 ( 4, 4 ),
 ( 0.006461935089719096983, 0.01455589064683252346 ),
 .UNSPECIFIED. ) ;
#36262 = LINE ( 'NONE', #92015, #53257 ) ;
#36263 = CARTESIAN_POINT ( 'NONE',  ( 189.8274365450016319, 274.1967410140837274, -15.63878423788518290 ) ) ;
#36264 = ADVANCED_FACE ( 'NONE', ( #10606 ), #83028, .T. ) ;
#36265 = CARTESIAN_POINT ( 'NONE',  ( 85.74281436412356072, 48.57633205417285893, -12.30481470458759929 ) ) ;
#36266 = CARTESIAN_POINT ( 'NONE',  ( 175.3208435976894179, 291.5367879113061917, 3.470880399820767348 ) ) ;
#36267 = CARTESIAN_POINT ( 'NONE',  ( 133.4825598088814047, 236.3262482093457493, 3.021315404115420679E-15 ) ) ;
#36268 =( BOUNDED_CURVE ( )  B_SPLINE_CURVE ( 2, ( #1504, #24291, #32879, #55168, #25805, #47577, #90115, #42951, #43466, #96725, #65767, #58173, #73890 ),
 .UNSPECIFIED., .F., .T. ) 
 B_SPLINE_CURVE_WITH_KNOTS ( ( 3, 2, 2, 2, 2, 2, 3 ),
 ( 0.5125000000000000666, 0.5150000000000000133, 0.5200000000000000178, 0.5250000000000000222, 0.5300000000000000266, 0.5350000000000000311, 0.5375000000000000888 ),
 .UNSPECIFIED. ) 
 CURVE ( )  GEOMETRIC_REPRESENTATION_ITEM ( )  RATIONAL_B_SPLINE_CURVE ( ( 0.9755282581475767101, 0.9755282581475772652, 1.000000000000000000, 0.9510565162951535312, 1.000000000000000000, 0.9510565162951535312, 1.000000000000000000, 0.9510565162951535312, 1.000000000000000000, 0.9510565162951535312, 1.000000000000000000, 0.9755282581475761550, 0.9755282581475767101 ) ) 
 REPRESENTATION_ITEM ( '' )  );
#36269 = CARTESIAN_POINT ( 'NONE',  ( 81.19656099882028855, 43.43094936609876555, -9.896970666369856673 ) ) ;
#36270 = CARTESIAN_POINT ( 'NONE',  ( 156.6812872898450735, 261.2670451491295012, 0.000000000000000000 ) ) ;
#36271 = CARTESIAN_POINT ( 'NONE',  ( 3.585285057187872937, 179.0024278399160949, 9.188101187500095079 ) ) ;
#36272 = CARTESIAN_POINT ( 'NONE',  ( 96.30395630197683943, 238.6589784336661637, -6.496448406907675876E-16 ) ) ;
#36273 = CARTESIAN_POINT ( 'NONE',  ( 41.86197723097736656, 201.6427522451419350, -10.00000000000009592 ) ) ;
#36274 = CARTESIAN_POINT ( 'NONE',  ( 186.7353386538602251, 295.9631457000137402, -7.534418545603307038 ) ) ;
#36275 = CARTESIAN_POINT ( 'NONE',  ( 78.44929255208916175, 53.32820552639820733, 15.80390961651161419 ) ) ;
#36276 = DIRECTION ( 'NONE',  ( -0.000000000000000000, -0.000000000000000000, -1.000000000000000000 ) ) ;
#36277 = CARTESIAN_POINT ( 'NONE',  ( 78.96891143551646053, 53.97097611525893512, -15.87805625008014943 ) ) ;
#36278 = DIRECTION ( 'NONE',  ( 0.000000000000000000, 0.000000000000000000, 1.000000000000000000 ) ) ;
#36279 = CARTESIAN_POINT ( 'NONE',  ( 180.5329152982068877, 273.0640148049105278, 16.87540567491608101 ) ) ;
#36280 = CARTESIAN_POINT ( 'NONE',  ( 194.7900911235093133, 293.2606606935473792, -14.66228443412922999 ) ) ;
#36281 = FACE_OUTER_BOUND ( 'NONE', #54374, .T. ) ;
#36282 = CARTESIAN_POINT ( 'NONE',  ( 84.38707503008889432, 50.04123336203296901, 13.82163251822127670 ) ) ;
#36283 = CARTESIAN_POINT ( 'NONE',  ( 192.8548134607404165, 265.3588860054690031, 7.786932206011543123 ) ) ;
#36284 = DIRECTION ( 'NONE',  ( 8.673617379884080832E-16, -0.000000000000000000, -1.000000000000000000 ) ) ;
#36285 = CARTESIAN_POINT ( 'NONE',  ( 184.4700260883318492, 268.6843530457092015, -15.41494737780146629 ) ) ;
#36286 = CARTESIAN_POINT ( 'NONE',  ( 42.89584289395545369, 207.1199935810940929, 2.679491924311251605 ) ) ;
#36287 = CARTESIAN_POINT ( 'NONE',  ( 172.5927298621351156, 263.8025790245163194, -15.44835621726458008 ) ) ;
#36288 = EDGE_CURVE ( 'NONE', #24906, #100286, #75404, .T. ) ;
#36289 = CARTESIAN_POINT ( 'NONE',  ( 74.35571174875622091, 222.9244531367911293, -4.594050593750046652 ) ) ;
#36290 = CARTESIAN_POINT ( 'NONE',  ( 14.98925625915878079, 9.449665230724930254, -2.296566073217252530E-15 ) ) ;
#36291 = CYLINDRICAL_SURFACE ( 'NONE', #54660, 17.82106496071139645 ) ;
#36293 = CARTESIAN_POINT ( 'NONE',  ( 152.5098501883502706, 266.4921861494963196, 16.07965188502810605 ) ) ;
#36292 = CARTESIAN_POINT ( 'NONE',  ( 157.4656258344471098, 257.9085309395441641, 18.30485740784190796 ) ) ;
#36294 = CARTESIAN_POINT ( 'NONE',  ( 196.9367784295097579, 289.5424892115916577, 16.51204079746186437 ) ) ;
#36295 = CARTESIAN_POINT ( 'NONE',  ( 151.2646864780760723, 268.6488729594320830, -14.38346604407754548 ) ) ;
#36296 = CARTESIAN_POINT ( 'NONE',  ( -55.59287931351116896, 32.99562883703961802, 177.5919119679930134 ) ) ;
#36297 = CARTESIAN_POINT ( 'NONE',  ( 39.17063663036994114, 34.56628583063844928, 9.188101187500006262 ) ) ;
#36298 = CARTESIAN_POINT ( 'NONE',  ( 192.4743214706506365, 297.2716913909250707, -12.17804856100553046 ) ) ;
#36299 = DIRECTION ( 'NONE',  ( 0.3978777116982076811, 0.7304723483372488335, -0.5550706935593547886 ) ) ;
#36300 = CARTESIAN_POINT ( 'NONE',  ( 23.73493010604062192, 29.10171378149919974, 9.188101187500008038 ) ) ;
#36301 = CARTESIAN_POINT ( 'NONE',  ( 44.47956695515382108, 64.36960560548604349, 10.00000000000000000 ) ) ;
#36302 = CARTESIAN_POINT ( 'NONE',  ( 147.3379027498079381, 275.4502618871274535, -3.695260257281167249 ) ) ;
#36303 = CARTESIAN_POINT ( 'NONE',  ( 191.6794403243964950, 288.1292005957208744, -15.80774595056399434 ) ) ;
#36304 = ORIENTED_EDGE ( 'NONE', *, *, #28127, .T. ) ;
#36305 = CARTESIAN_POINT ( 'NONE',  ( 67.53167658295855347, 67.09922345392760690, 8.942594108559754673 ) ) ;
#36306 = CARTESIAN_POINT ( 'NONE',  ( 159.9307118030769175, 253.6388767968520881, 16.60600887889890487 ) ) ;
#36307 = MECHANICAL_DESIGN_GEOMETRIC_PRESENTATION_REPRESENTATION (  '', ( #23353 ), #799 ) ;
#36308 = CARTESIAN_POINT ( 'NONE',  ( 153.6507061805664307, 266.9580362223465499, 16.55103579890343113 ) ) ;
#36309 = CARTESIAN_POINT ( 'NONE',  ( 169.9051147537142299, 251.0516595293013040, -8.602792619013742481 ) ) ;
#36310 = CARTESIAN_POINT ( 'NONE',  ( 149.8445197688975838, 243.9865022471901455, 1.119607411625061291E-15 ) ) ;
#36311 = CARTESIAN_POINT ( 'NONE',  ( 69.99818716782885986, 62.70504339187703380, 13.41613852849032362 ) ) ;
#36312 = EDGE_LOOP ( 'NONE', ( #92551, #43604, #38174, #89485 ) ) ;
#36313 = CARTESIAN_POINT ( 'NONE',  ( 193.0622221429366050, 289.4054684591471300, 16.71589558189321778 ) ) ;
#36314 = VERTEX_POINT ( 'NONE', #13598 ) ;
#36315 = CARTESIAN_POINT ( 'NONE',  ( 196.6281177133425899, 264.5552008573027933, -4.675636469121769778 ) ) ;
#36316 = CARTESIAN_POINT ( 'NONE',  ( 82.90570422835274655, 41.17580535834989064, 0.2246636192497151185 ) ) ;
#36317 = VERTEX_POINT ( 'NONE', #5987 ) ;
#36318 = CARTESIAN_POINT ( 'NONE',  ( 185.3004367499268596, 292.5792462585945373, -10.68249092389169519 ) ) ;
#36321 = EDGE_CURVE ( 'NONE', #28659, #98547, #99199, .T. ) ;
#36320 = ORIENTED_EDGE ( 'NONE', *, *, #96297, .F. ) ;
#36319 = AXIS2_PLACEMENT_3D ( 'NONE', #4031, #58223, #12140 ) ;
#36322 = CARTESIAN_POINT ( 'NONE',  ( 188.7930588916510999, 290.9633865388665299, 14.97457979531618832 ) ) ;
#36323 = CARTESIAN_POINT ( 'NONE',  ( 13.78829669240011135, 8.364779650996389648, 1.583844403245363130 ) ) ;
#36324 = CARTESIAN_POINT ( 'NONE',  ( 157.5695214119805598, 258.1165995213424367, -16.71692661953962400 ) ) ;
#36325 = CARTESIAN_POINT ( 'NONE',  ( 204.3267329952771831, 273.2094209704910099, 10.93732012634468909 ) ) ;
#36326 = CARTESIAN_POINT ( 'NONE',  ( 153.1983976505312626, 265.2995869615763809, -17.69657798691567763 ) ) ;
#36327 = DIRECTION ( 'NONE',  ( 0.8806841296921896767, -0.4737039832092512226, 0.000000000000000000 ) ) ;
#36328 = CARTESIAN_POINT ( 'NONE',  ( 39.38594668318775405, 31.24335787977766188, -9.188101187500008038 ) ) ;
#36329 = DIRECTION ( 'NONE',  ( 1.000000000000000000, 0.000000000000000000, 0.000000000000000000 ) ) ;
#36331 = ADVANCED_FACE ( 'NONE', ( #84523 ), #74909, .T. ) ;
#36330 = FACE_OUTER_BOUND ( 'NONE', #66983, .T. ) ;
#36332 = CARTESIAN_POINT ( 'NONE',  ( 110.0000000000000000, -8.000000000000000000, 14.21260523776213347 ) ) ;
#36333 = ADVANCED_FACE ( 'NONE', ( #82546 ), #29785, .T. ) ;
#36334 = ORIENTED_EDGE ( 'NONE', *, *, #72781, .T. ) ;
#36335 = ORIENTED_EDGE ( 'NONE', *, *, #45931, .F. ) ;
#36336 = CARTESIAN_POINT ( 'NONE',  ( 87.17963343274935539, 46.25680430639528140, -9.118192349661992324 ) ) ;
#36338 = CARTESIAN_POINT ( 'NONE',  ( 194.2154056360670040, 294.2560451561701029, -15.66696967429384557 ) ) ;
#36337 = CARTESIAN_POINT ( 'NONE',  ( 164.3853877993040840, 245.9231516401292197, 5.995325337583643943 ) ) ;
#36339 = CARTESIAN_POINT ( 'NONE',  ( -22.42236680055709641, 157.8615022471902591, 0.000000000000000000 ) ) ;
#36340 = CARTESIAN_POINT ( 'NONE',  ( 155.0929244053699847, 262.0181703658971628, 18.51426604808664678 ) ) ;
#36341 = CARTESIAN_POINT ( 'NONE',  ( 78.94131938193116582, 59.19540273697393928, -16.19806489488007983 ) ) ;
#36342 = CARTESIAN_POINT ( 'NONE',  ( 148.2980785574368952, 273.7871886041155562, 9.134436720559454770 ) ) ;
#36343 = CARTESIAN_POINT ( 'NONE',  ( 168.7909529993691251, 286.6037707115942226, -4.663693738437698855 ) ) ;
#36344 = CARTESIAN_POINT ( 'NONE',  ( 76.80517106979452535, 63.30872754350402687, -15.45635652541256455 ) ) ;
#36345 = CARTESIAN_POINT ( 'NONE',  ( 181.9115977867584775, 256.5621209711902679, 5.178624687905984736 ) ) ;
#36346 = CARTESIAN_POINT ( 'NONE',  ( 105.9931361504627603, 225.8768266524159856, -9.188101187500091527 ) ) ;
#36347 = ORIENTED_EDGE ( 'NONE', *, *, #13609, .T. ) ;
#36348 = FACE_OUTER_BOUND ( 'NONE', #97045, .T. ) ;
#36349 = CARTESIAN_POINT ( 'NONE',  ( 165.2491185908025102, 271.0061427863645349, 16.55936586366629015 ) ) ;
#36350 = CARTESIAN_POINT ( 'NONE',  ( 191.9323033642516805, 275.2179287646682724, 16.63116605495289946 ) ) ;
#36351 = ORIENTED_EDGE ( 'NONE', *, *, #62771, .F. ) ;
#36352 = ORIENTED_EDGE ( 'NONE', *, *, #48776, .F. ) ;
#36353 = CARTESIAN_POINT ( 'NONE',  ( 180.1168005803277481, 295.2192856762299016, -2.191971455912026467 ) ) ;
#36354 = CARTESIAN_POINT ( 'NONE',  ( 177.4877928417686803, 293.5951873982637608, -2.837372163671336267 ) ) ;
#36355 = CARTESIAN_POINT ( 'NONE',  ( 157.1338510812060747, 258.4831816688264325, 17.88958125218800888 ) ) ;
#36356 = CARTESIAN_POINT ( 'NONE',  ( 159.9470087484377814, 253.6106496594791508, -16.54933891566789939 ) ) ;
#36357 = LINE ( 'NONE', #67262, #72275 ) ;
#36358 = ORIENTED_EDGE ( 'NONE', *, *, #13240, .F. ) ;
#36359 = EDGE_LOOP ( 'NONE', ( #27517, #82606, #8270, #58657 ) ) ;
#36360 = EDGE_CURVE ( 'NONE', #76328, #77324, #67276, .T. ) ;
#36361 = CARTESIAN_POINT ( 'NONE',  ( 163.4218292706009095, 247.5920839679097014, -10.44611490715852042 ) ) ;
#36362 = ORIENTED_EDGE ( 'NONE', *, *, #70999, .F. ) ;
#36363 = DIRECTION ( 'NONE',  ( 0.000000000000000000, 0.4385670422228000742, -0.8986984752829754175 ) ) ;
#36364 = CARTESIAN_POINT ( 'NONE',  ( 101.7620676594010973, 222.8927522451417929, -10.00000000000009237 ) ) ;
#36365 = CARTESIAN_POINT ( 'NONE',  ( 191.8812340238766581, 261.0126994209120426, -0.1972034713832918895 ) ) ;
#36367 = CARTESIAN_POINT ( 'NONE',  ( 69.60454156778966706, 62.55713719731701161, -13.37071440263582112 ) ) ;
#36366 = CARTESIAN_POINT ( 'NONE',  ( 184.3049839938290972, 288.8408771957522276, -13.19264464187155639 ) ) ;
#36368 = CARTESIAN_POINT ( 'NONE',  ( 67.86860378221429357, 65.58690806574966814, -10.91583492536020472 ) ) ;
#36369 = VERTEX_POINT ( 'NONE', #43970 ) ;
#36370 = CARTESIAN_POINT ( 'NONE',  ( 205.0418338828961851, 275.5041213681629984, 14.30558627745945266 ) ) ;
#36371 = CARTESIAN_POINT ( 'NONE',  ( 82.78345634833958400, 53.69061190982763776, 15.38144188222361386 ) ) ;
#36372 = CARTESIAN_POINT ( 'NONE',  ( 82.56326814738740438, 40.91834736438271136, -3.675696166060102854 ) ) ;
#36373 = EDGE_CURVE ( 'NONE', #18632, #34200, #10414, .T. ) ;
#36374 = CARTESIAN_POINT ( 'NONE',  ( 173.2783483489837408, 251.6438032808846970, -0.4401592383492047289 ) ) ;
#36375 = CARTESIAN_POINT ( 'NONE',  ( 48.48788556946983874, 102.1758113618167982, -10.00000000000000000 ) ) ;
#36376 = CARTESIAN_POINT ( 'NONE',  ( 72.06396613292808695, 72.31755342346831128, 3.440598478083111367 ) ) ;
#36377 = VECTOR ( 'NONE', #79656, 1000.000000000000227 ) ;
#36378 = FACE_OUTER_BOUND ( 'NONE', #79743, .T. ) ;
#36379 = PLANE ( 'NONE',  #36553 ) ;
#36380 = CARTESIAN_POINT ( 'NONE',  ( 180.8044385370616567, 286.7361374272969101, 14.76499878110572439 ) ) ;
#36381 = CARTESIAN_POINT ( 'NONE',  ( 206.4097941777342839, 271.6911524580777382, 7.546727351666162598 ) ) ;
#36382 = CARTESIAN_POINT ( 'NONE',  ( 62.93552237999645627, 197.9548013555410080, -4.594050593750042211 ) ) ;
#36383 = CARTESIAN_POINT ( 'NONE',  ( 206.0946696452135427, 273.6805563358039421, -10.19627505985792837 ) ) ;
#36384 = CARTESIAN_POINT ( 'NONE',  ( 77.60205039494942980, 61.82655112718389034, 15.66204818029991941 ) ) ;
#36385 = FACE_OUTER_BOUND ( 'NONE', #67015, .T. ) ;
#36386 = CIRCLE ( 'NONE', #94645, 0.1418229129681557177 ) ;
#36387 = EDGE_CURVE ( 'NONE', #13192, #84442, #72153, .T. ) ;
#36388 = CARTESIAN_POINT ( 'NONE',  ( 161.3145230519951951, 251.2420454056404822, -14.44869077440025151 ) ) ;
#36389 = CARTESIAN_POINT ( 'NONE',  ( 66.86272913223326952, 69.17654172454702177, 0.7859538092876443560 ) ) ;
#36391 = FACE_OUTER_BOUND ( 'NONE', #91968, .T. ) ;
#36390 = CARTESIAN_POINT ( 'NONE',  ( 73.37704433742356969, 70.12506801342537699, -9.398789138188929471 ) ) ;
#36392 = CARTESIAN_POINT ( 'NONE',  ( 160.7489855951974675, 254.2215850144021658, 15.85577744295692248 ) ) ;
#36393 = DIRECTION ( 'NONE',  ( 1.000000000000000000, 0.000000000000000000, -0.000000000000000000 ) ) ;
#36394 = DIRECTION ( 'NONE',  ( 1.000000000000000000, 7.137148015447434001E-15, 0.000000000000000000 ) ) ;
#36395 = CARTESIAN_POINT ( 'NONE',  ( 180.2261984326610218, 279.1782745765357276, -17.42438828499370729 ) ) ;
#36396 = CARTESIAN_POINT ( 'NONE',  ( 72.06501183224497709, 72.04686745563701322, 2.871359202350765472 ) ) ;
#36397 = CARTESIAN_POINT ( 'NONE',  ( 26.96797095936772237, 192.5024278399160949, 9.188101187500095079 ) ) ;
#36398 = EDGE_CURVE ( 'NONE', #23710, #27141, #3120, .T. ) ;
#36399 = CARTESIAN_POINT ( 'NONE',  ( 196.1573359623355088, 290.8925231663144473, 17.55680092534192482 ) ) ;
#36400 = CARTESIAN_POINT ( 'NONE',  ( 166.1309782654906257, 249.2029336093187339, -9.347746458946922132 ) ) ;
#36401 = CARTESIAN_POINT ( 'NONE',  ( 207.6172352878830907, 271.0433952848413810, 3.316653249540578496 ) ) ;
#36402 = CARTESIAN_POINT ( 'NONE',  ( 71.79363655647949827, 72.51690322118082577, -1.318798153274830076 ) ) ;
#36403 = CARTESIAN_POINT ( 'NONE',  ( 51.08127902204942927, 209.4869531367911009, 4.594050593750046652 ) ) ;
#36404 = B_SPLINE_CURVE_WITH_KNOTS ( 'NONE', 3,
 ( #90516, #52449, #75279, #13963, #55301, #98587 ),
 .UNSPECIFIED., .F., .F.,
 ( 4, 2, 4 ),
 ( 0.01937495045225347615, 0.02390856016151878677, 0.02844216987078409392 ),
 .UNSPECIFIED. ) ;
#36405 = AXIS2_PLACEMENT_3D ( 'NONE', #62461, #93427, #23979 ) ;
#36406 = CARTESIAN_POINT ( 'NONE',  ( 17.13451663979182626, 31.93396525600390135, 2.839279412974139660 ) ) ;
#36407 = CARTESIAN_POINT ( 'NONE',  ( 199.1526122334580862, 285.7045524820243259, -17.32174362185583050 ) ) ;
#36408 = DIRECTION ( 'NONE',  ( 0.000000000000000000, -0.000000000000000000, 1.000000000000000000 ) ) ;
#36409 = CARTESIAN_POINT ( 'NONE',  ( 39.57658603661993624, 34.80066082961425877, 10.00000000000000533 ) ) ;
#36410 = CARTESIAN_POINT ( 'NONE',  ( 202.9861313035285377, 270.0111324708095708, -7.109816141738001249 ) ) ;
#36411 = CARTESIAN_POINT ( 'NONE',  ( 78.05817343695024135, 58.35059340816943774, -16.56781068415745750 ) ) ;
#36412 = CARTESIAN_POINT ( 'NONE',  ( 179.8822850121538863, 276.6405008247433557, 16.37156656675600885 ) ) ;
#36413 = CARTESIAN_POINT ( 'NONE',  ( 158.2129804214947058, 265.2348010298870236, 17.61986633405762603 ) ) ;
#36414 = CARTESIAN_POINT ( 'NONE',  ( 71.04687822819680321, 67.82841818693096059, -9.805517038057930179 ) ) ;
#36415 = CARTESIAN_POINT ( 'NONE',  ( 192.6633363462123043, 266.5854721252571267, 11.55478091722345901 ) ) ;
#36416 = CARTESIAN_POINT ( 'NONE',  ( 82.37267291861169838, 41.27180535394074923, 3.277253532406301684 ) ) ;
#36417 = CARTESIAN_POINT ( 'NONE',  ( 87.53583079710631409, 45.45925790797146249, -6.823327534849012110 ) ) ;
#36418 = CARTESIAN_POINT ( 'NONE',  ( 107.0484310652165476, 222.6115022471901739, -5.000000000000041744 ) ) ;
#36419 = CARTESIAN_POINT ( 'NONE',  ( 179.4404154152157105, 291.3709498135804097, -10.08759257512885199 ) ) ;
#36420 = CARTESIAN_POINT ( 'NONE',  ( 164.0800018754982261, 268.9966071389823696, -16.36617084150674728 ) ) ;
#36421 = ORIENTED_EDGE ( 'NONE', *, *, #53266, .F. ) ;
#36422 = CARTESIAN_POINT ( 'NONE',  ( 65.10058588945754821, 199.2048013555409796, 4.594050593750051981 ) ) ;
#36423 = ORIENTED_EDGE ( 'NONE', *, *, #17236, .T. ) ;
#36424 = CARTESIAN_POINT ( 'NONE',  ( 165.2047206435933902, 264.8326349929704406, 16.61084491559804732 ) ) ;
#36425 = CARTESIAN_POINT ( 'NONE',  ( 190.1813752874636805, 301.2431906792259042, -4.710625539811892359 ) ) ;
#36426 = B_SPLINE_CURVE_WITH_KNOTS ( 'NONE', 3,
 ( #96881, #12756, #42127, #73059 ),
 .UNSPECIFIED., .F., .F.,
 ( 4, 4 ),
 ( 0.009399112305859652974, 0.01497842902758104652 ),
 .UNSPECIFIED. ) ;
#36427 = LINE ( 'NONE', #7527, #30480 ) ;
#36428 = VERTEX_POINT ( 'NONE', #40360 ) ;
#36429 = DIRECTION ( 'NONE',  ( -0.000000000000000000, -0.000000000000000000, -1.000000000000000000 ) ) ;
#36430 = CARTESIAN_POINT ( 'NONE',  ( 79.15324990756228374, 45.89422231479612435, -13.12042404536878237 ) ) ;
#36431 = CARTESIAN_POINT ( 'NONE',  ( 39.77289032284285497, 58.49985355908045648, 10.00000000000000000 ) ) ;
#36432 = CARTESIAN_POINT ( 'NONE',  ( 187.7918093292738604, 264.8259943713989060, 10.76435498059212925 ) ) ;
#36433 = DIRECTION ( 'NONE',  ( -0.8660254037844378194, -0.5000000000000014433, -0.000000000000000000 ) ) ;
#36434 = CARTESIAN_POINT ( 'NONE',  ( 205.0418338828961851, 275.5041213681629984, 14.30558627745945266 ) ) ;
#36435 = ORIENTED_EDGE ( 'NONE', *, *, #26184, .T. ) ;
#36436 = CARTESIAN_POINT ( 'NONE',  ( 27.42516030814983807, 18.76004757982090609, 5.678558825948272215 ) ) ;
#36437 = CARTESIAN_POINT ( 'NONE',  ( 76.35345023940182330, 62.28244966075228461, 15.31341552635249137 ) ) ;
#36438 = CARTESIAN_POINT ( 'NONE',  ( 70.44627411417100404, 70.20050130344810668, -5.575475040495237344 ) ) ;
#36439 = CARTESIAN_POINT ( 'NONE',  ( 172.2467550100553808, 258.4300157609564508, -14.58559033337875377 ) ) ;
#36440 = B_SPLINE_CURVE_WITH_KNOTS ( 'NONE', 3,
 ( #71090, #71590, #17885, #62442 ),
 .UNSPECIFIED., .F., .F.,
 ( 4, 4 ),
 ( 0.01214016279898067277, 0.01831897122411682219 ),
 .UNSPECIFIED. ) ;
#36441 = ORIENTED_EDGE ( 'NONE', *, *, #7280, .T. ) ;
#36443 = EDGE_CURVE ( 'NONE', #19809, #41237, #22607, .T. ) ;
#36442 = CARTESIAN_POINT ( 'NONE',  ( 182.6210901421643769, 283.8088811521847106, 15.95401699950471652 ) ) ;
#36444 = CARTESIAN_POINT ( 'NONE',  ( 159.4491226731523454, 254.4730136382542582, -15.39140229921534520 ) ) ;
#36445 = CIRCLE ( 'NONE', #93106, 0.1418229129681522482 ) ;
#36446 = EDGE_CURVE ( 'NONE', #73023, #40420, #86716, .T. ) ;
#36447 = EDGE_LOOP ( 'NONE', ( #26275, #47678, #52174, #10053 ) ) ;
#36448 = ORIENTED_EDGE ( 'NONE', *, *, #41229, .F. ) ;
#36450 = CARTESIAN_POINT ( 'NONE',  ( 165.4187906757635460, 280.8472404715405446, -12.62740765345973415 ) ) ;
#36449 = CARTESIAN_POINT ( 'NONE',  ( 159.2440537178480042, 282.4524729739796385, -3.288764571076911114 ) ) ;
#36451 = CARTESIAN_POINT ( 'NONE',  ( 70.07987635803645787, 71.18405689213730625, -3.399692208177651942 ) ) ;
#36452 = CARTESIAN_POINT ( 'NONE',  ( 65.86595443870683653, 68.98825277307732051, -2.186046751764159080 ) ) ;
#36453 = EDGE_CURVE ( 'NONE', #98021, #86016, #26202, .T. ) ;
#36454 = DIRECTION ( 'NONE',  ( -0.7278481391575704063, 0.6857383512133925496, 0.000000000000000000 ) ) ;
#36455 = CARTESIAN_POINT ( 'NONE',  ( 81.83839218517164227, 55.52280113860526711, 16.29901351018851230 ) ) ;
#36456 = CARTESIAN_POINT ( 'NONE',  ( 163.7356037823865336, 264.5711151872889673, -16.68138376633201148 ) ) ;
#36457 = EDGE_CURVE ( 'NONE', #36668, #99538, #90219, .T. ) ;
#36459 = CARTESIAN_POINT ( 'NONE',  ( 129.7005815790617760, 239.5643266524159856, -9.188101187500093303 ) ) ;
#36458 =( GEOMETRIC_REPRESENTATION_CONTEXT ( 3 ) GLOBAL_UNCERTAINTY_ASSIGNED_CONTEXT ( ( #93996 ) ) GLOBAL_UNIT_ASSIGNED_CONTEXT ( ( #678, #38152, #22966 ) ) REPRESENTATION_CONTEXT ( 'NONE', 'WORKASPACE' ) );
#36460 = PLANE ( 'NONE',  #37517 ) ;
#36461 = VERTEX_POINT ( 'NONE', #86048 ) ;
#36462 = CARTESIAN_POINT ( 'NONE',  ( 173.7177128658787240, 265.2567829307042757, 16.88771258197816039 ) ) ;
#36463 = CARTESIAN_POINT ( 'NONE',  ( 27.19136022205111658, 198.0530062829863311, -4.648177544792955347E-16 ) ) ;
#36464 = ORIENTED_EDGE ( 'NONE', *, *, #43884, .F. ) ;
#36465 = DIRECTION ( 'NONE',  ( -0.000000000000000000, 0.000000000000000000, -1.000000000000000000 ) ) ;
#36466 = VERTEX_POINT ( 'NONE', #63679 ) ;
#36467 = ORIENTED_EDGE ( 'NONE', *, *, #61621, .F. ) ;
#36468 = CARTESIAN_POINT ( 'NONE',  ( 198.6587626159274294, 286.5599251108861267, 17.99840276545888784 ) ) ;
#36469 = CARTESIAN_POINT ( 'NONE',  ( -59.29375005653867703, 35.37083770076973366, 10.00000000000000000 ) ) ;
#36470 = CARTESIAN_POINT ( 'NONE',  ( 74.76226857436894591, 201.7202760586659167, -5.415160957724236172E-17 ) ) ;
#36471 = CARTESIAN_POINT ( 'NONE',  ( -30.28621228554850831, 95.69946231200637499, 12.75647095971420697 ) ) ;
#36472 = FACE_OUTER_BOUND ( 'NONE', #80606, .T. ) ;
#36473 = CARTESIAN_POINT ( 'NONE',  ( 155.3017250444513024, 261.6565170503553190, 18.58368563027307374 ) ) ;
#36474 = CARTESIAN_POINT ( 'NONE',  ( -13.11024591527734628, 6.000000000000000000, 20.00000000000000000 ) ) ;
#36475 = CARTESIAN_POINT ( 'NONE',  ( 87.59998515009166908, 45.09196136326726645, 6.914658723149491593 ) ) ;
#36476 = EDGE_LOOP ( 'NONE', ( #256, #7541, #79033, #42455 ) ) ;
#36477 = DIRECTION ( 'NONE',  ( 0.5295078238379054003, 0.5024823063053049932, 0.6834712842135706179 ) ) ;
#36478 = CARTESIAN_POINT ( 'NONE',  ( 152.7375212135632125, 266.0978483664162582, -16.47968945089317572 ) ) ;
#36479 = CARTESIAN_POINT ( 'NONE',  ( 66.12762260262825009, 68.48100856943257497, -4.819680968675389643 ) ) ;
#36480 = ORIENTED_EDGE ( 'NONE', *, *, #77420, .F. ) ;
#36481 = DIRECTION ( 'NONE',  ( 0.8660254037844395958, 0.4999999999999985567, 0.000000000000000000 ) ) ;
#36482 = CARTESIAN_POINT ( 'NONE',  ( 76.14419419685665957, 51.07260177014754987, -15.57971481703006766 ) ) ;
#36483 = CARTESIAN_POINT ( 'NONE',  ( 174.7480863157453825, 254.3094501535669849, -7.405053707554171361 ) ) ;
#36485 = CARTESIAN_POINT ( 'NONE',  ( 79.65227431844175499, 50.82673930868438816, 15.43633079355379145 ) ) ;
#36484 = B_SPLINE_CURVE_WITH_KNOTS ( 'NONE', 3,
 ( #83124, #12205, #73022, #12715, #96336, #59262, #3614, #44069 ),
 .UNSPECIFIED., .F., .F.,
 ( 4, 2, 2, 4 ),
 ( 0.4743034264391701171, 0.7371517132195847255, 0.8685758566097923072, 1.000000000000000000 ),
 .UNSPECIFIED. ) ;
#36486 = B_SPLINE_CURVE_WITH_KNOTS ( 'NONE', 3,
 ( #58538, #36237, #28149, #57542 ),
 .UNSPECIFIED., .F., .F.,
 ( 4, 4 ),
 ( 0.009348827086400075120, 0.01504353011265674271 ),
 .UNSPECIFIED. ) ;
#36487 = CARTESIAN_POINT ( 'NONE',  ( 205.8452707775803390, 274.1125278458945900, 11.42742867493066328 ) ) ;
#36488 = VECTOR ( 'NONE', #49841, 1000.000000000000000 ) ;
#36489 = CARTESIAN_POINT ( 'NONE',  ( 167.6278246310154714, 282.5728663012718584, -12.21306354836790220 ) ) ;
#36490 = CARTESIAN_POINT ( 'NONE',  ( 194.9948854055928678, 279.4939489864826783, 16.52961264899888150 ) ) ;
#36491 = ORIENTED_EDGE ( 'NONE', *, *, #6397, .T. ) ;
#36492 = CARTESIAN_POINT ( 'NONE',  ( 2.890834060677622830, 179.1427522451419350, -10.00000000000009592 ) ) ;
#36493 = CARTESIAN_POINT ( 'NONE',  ( 139.3076170325891212, 260.4244531367911577, -4.594050593750046652 ) ) ;
#36494 = ORIENTED_EDGE ( 'NONE', *, *, #70780, .T. ) ;
#36495 = CARTESIAN_POINT ( 'NONE',  ( 88.24246443646677562, 44.29974554292944333, 4.047255302186847814 ) ) ;
#36496 = CARTESIAN_POINT ( 'NONE',  ( 85.22637764667558713, 43.33431299993616648, 4.849872636722851738 ) ) ;
#36497 = CARTESIAN_POINT ( 'NONE',  ( 155.9594927221938292, 261.9410314534172244, -16.96711934140056499 ) ) ;
#36498 = AXIS2_PLACEMENT_3D ( 'NONE', #97822, #19819, #51712 ) ;
#36499 = CARTESIAN_POINT ( 'NONE',  ( 79.51018340840847998, 59.27997616101576028, -16.21944250808304133 ) ) ;
#36500 = CARTESIAN_POINT ( 'NONE',  ( 6.752405126987250483, 41.48691455871444589, 59.99999999999999289 ) ) ;
#36501 = VERTEX_POINT ( 'NONE', #8977 ) ;
#36502 = CARTESIAN_POINT ( 'NONE',  ( 76.17916984540215708, 53.15653679037458801, 15.96716164428893947 ) ) ;
#36503 = CARTESIAN_POINT ( 'NONE',  ( 182.4344152771883500, 275.0372901602324873, -17.25385560252001937 ) ) ;
#36504 = CARTESIAN_POINT ( 'NONE',  ( 167.5910006351356287, 249.2382425172987723, -5.800627538551558438 ) ) ;
#36505 = CARTESIAN_POINT ( 'NONE',  ( 81.48851436888811861, 54.04920842346697896, 15.64857177594916315 ) ) ;
#36506 = CARTESIAN_POINT ( 'NONE',  ( 73.71556180253553237, 69.43794663908232678, -9.869968096196300777 ) ) ;
#36507 = DIRECTION ( 'NONE',  ( -0.000000000000000000, -0.000000000000000000, -1.000000000000000000 ) ) ;
#36508 = CARTESIAN_POINT ( 'NONE',  ( 70.46332345186002044, 71.25533206547748932, 1.570548084703874858 ) ) ;
#36509 = EDGE_CURVE ( 'NONE', #27272, #17277, #167, .T. ) ;
#36510 = VECTOR ( 'NONE', #76414, 1000.000000000000000 ) ;
#36511 = CARTESIAN_POINT ( 'NONE',  ( 157.5487431480040925, 257.7645675294749594, -18.29554785922338311 ) ) ;
#36512 = CARTESIAN_POINT ( 'NONE',  ( 172.3986314675530309, 263.7922717222033384, -16.89442142407995107 ) ) ;
#36513 = CARTESIAN_POINT ( 'NONE',  ( 21.14026940803790566, 27.90829794293880539, 10.00000000000000355 ) ) ;
#36514 = CARTESIAN_POINT ( 'NONE',  ( 48.88270317314112390, 187.4824982072973967, 3.021315404115420679E-15 ) ) ;
#36515 = CARTESIAN_POINT ( 'NONE',  ( -68.37628875030422648, 42.44405361048389125, 10.00000000000000000 ) ) ;
#36516 = DIRECTION ( 'NONE',  ( -0.8660254037844387076, -0.4999999999999998890, -0.000000000000000000 ) ) ;
#36517 = CARTESIAN_POINT ( 'NONE',  ( 159.8655504377736918, 253.7517395922482706, 15.51368179719542262 ) ) ;
#36518 = CARTESIAN_POINT ( 'NONE',  ( 72.30516432241840619, 72.03273627914288113, -3.489044445822598650 ) ) ;
#36519 = CARTESIAN_POINT ( 'NONE',  ( 128.4645176094212502, 251.6427522451419350, 10.00000000000009237 ) ) ;
#36520 = CARTESIAN_POINT ( 'NONE',  ( 175.5561847466084657, 285.0769009925375599, -12.03860467003484835 ) ) ;
#36521 = ORIENTED_EDGE ( 'NONE', *, *, #25003, .T. ) ;
#36522 = EDGE_CURVE ( 'NONE', #77213, #1361, #18595, .T. ) ;
#36523 = CARTESIAN_POINT ( 'NONE',  ( 67.14020853625015661, 67.74426869623036396, -6.533592144312494909 ) ) ;
#36524 = CARTESIAN_POINT ( 'NONE',  ( 198.4860348845112981, 286.8590983175747056, -18.20461732983060088 ) ) ;
#36525 = CARTESIAN_POINT ( 'NONE',  ( 8.998290926605621465, 169.8768266524160140, 9.188101187500096856 ) ) ;
#36526 = CARTESIAN_POINT ( 'NONE',  ( 178.5956384695835482, 273.7284866639749907, -17.41459860866446263 ) ) ;
#36527 = CARTESIAN_POINT ( 'NONE',  ( 26.58620497985335973, 27.30066082961423035, -10.00000000000000533 ) ) ;
#36528 = CARTESIAN_POINT ( 'NONE',  ( -58.10760318826260118, 36.06970723555269842, -10.00000000000000000 ) ) ;
#36529 = CARTESIAN_POINT ( 'NONE',  ( 157.3029956111992362, 258.1902147490555421, -18.22269824972649843 ) ) ;
#36530 = CARTESIAN_POINT ( 'NONE',  ( 24.55112987542764458, 40.41347472807389352, -10.00000000000000000 ) ) ;
#36531 = CARTESIAN_POINT ( 'NONE',  ( -22.42236680055709641, 157.8615022471902591, 0.000000000000000000 ) ) ;
#36533 = CARTESIAN_POINT ( 'NONE',  ( 78.23504418992386888, 202.6427522451417644, 1.119607411625061291E-15 ) ) ;
#36532 = CARTESIAN_POINT ( 'NONE',  ( 196.2686502133740305, 269.5362150063830882, -10.79322297891937588 ) ) ;
#36534 = CARTESIAN_POINT ( 'NONE',  ( 179.4307333220020553, 254.8376236813717526, -4.075317600375849558 ) ) ;
#36535 = CARTESIAN_POINT ( 'NONE',  ( 197.9723018751917039, 287.7489099912414758, 17.92592712455262571 ) ) ;
#36536 = CARTESIAN_POINT ( 'NONE',  ( 59.05618993882887224, 198.2365022471902023, -10.00000000000009059 ) ) ;
#36537 = CARTESIAN_POINT ( 'NONE',  ( 42.68871737883920048, 29.81029122506298634, 8.090169943749479842 ) ) ;
#36538 = CARTESIAN_POINT ( 'NONE',  ( 189.8147415777049218, 301.8782188922952514, -0.5019643756309712934 ) ) ;
#36539 = CARTESIAN_POINT ( 'NONE',  ( 15.06046875309669630, 173.3768266524159856, -9.188101187500091527 ) ) ;
#36540 = CARTESIAN_POINT ( 'NONE',  ( 164.2551198995763002, 284.9701055883606386, 4.298724141468182935 ) ) ;
#36541 = CARTESIAN_POINT ( 'NONE',  ( 192.1883190596398094, 297.7670620978826150, 12.41391288785556668 ) ) ;
#36542 = CARTESIAN_POINT ( 'NONE',  ( 36.73494696561986217, 42.18502408145594984, 5.678558825948277544 ) ) ;
#36543 = CARTESIAN_POINT ( 'NONE',  ( 202.0335144746401284, 280.3352735051682885, -15.85562724245423105 ) ) ;
#36544 = CARTESIAN_POINT ( 'NONE',  ( 164.2953672501826929, 246.0790718049323687, -2.576662677987826111 ) ) ;
#36545 = DIRECTION ( 'NONE',  ( -0.8660254037844359321, -0.5000000000000051070, -0.000000000000000000 ) ) ;
#36546 = LINE ( 'NONE', #67453, #91386 ) ;
#36547 = CARTESIAN_POINT ( 'NONE',  ( 163.9286547936508782, 281.4788881291187863, 8.857336398642782882 ) ) ;
#36548 = DIRECTION ( 'NONE',  ( 1.000000000000000000, 0.000000000000000000, 0.000000000000000000 ) ) ;
#36549 = CARTESIAN_POINT ( 'NONE',  ( 11.28581492663933084, 21.91421378149917487, 9.188101187500008038 ) ) ;
#36550 = CARTESIAN_POINT ( 'NONE',  ( 164.9043417134678577, 286.5925546497160212, 0.04530247668140159611 ) ) ;
#36551 = CARTESIAN_POINT ( 'NONE',  ( 83.01487341893997041, 53.35419878647658720, 15.61608225115200987 ) ) ;
#36552 = CARTESIAN_POINT ( 'NONE',  ( 72.97386446981147401, 70.68132344495337804, 8.316175787459499702 ) ) ;
#36553 = AXIS2_PLACEMENT_3D ( 'NONE', #67283, #30284, #46983 ) ;
#36554 = CARTESIAN_POINT ( 'NONE',  ( 194.4889937320412230, 293.7821766735966662, 14.99892588346621380 ) ) ;
#36555 = ORIENTED_EDGE ( 'NONE', *, *, #93118, .F. ) ;
#36556 = CARTESIAN_POINT ( 'NONE',  ( 181.5481620411168819, 289.3862663955354719, 12.74148585560425140 ) ) ;
#36557 = CARTESIAN_POINT ( 'NONE',  ( 2.780145572064765425, 23.64646525600387506, -2.839279412974133887 ) ) ;
#36558 = DIRECTION ( 'NONE',  ( -0.000000000000000000, -0.000000000000000000, -1.000000000000000000 ) ) ;
#36559 = ORIENTED_EDGE ( 'NONE', *, *, #87110, .T. ) ;
#36561 = CARTESIAN_POINT ( 'NONE',  ( 155.6368094659423207, 263.0761338075079721, 17.69820953191020152 ) ) ;
#36560 =( BOUNDED_CURVE ( )  B_SPLINE_CURVE ( 2, ( #75213, #13895, #37673, #90947, #68583, #28096, #60973, #6296, #37187 ),
 .UNSPECIFIED., .F., .T. ) 
 B_SPLINE_CURVE_WITH_KNOTS ( ( 3, 2, 2, 2, 3 ),
 ( 0.2459677419354838745, 0.2473118279569892497, 0.2500000000000000000, 0.2526881720430107503, 0.2540322580645161255 ),
 .UNSPECIFIED. ) 
 CURVE ( )  GEOMETRIC_REPRESENTATION_ITEM ( )  RATIONAL_B_SPLINE_CURVE ( ( 0.9330127018922194093, 0.9330127018922194093, 1.000000000000000000, 0.8660254037844387076, 1.000000000000000000, 0.8660254037844387076, 1.000000000000000000, 0.9330127018922194093, 0.9330127018922194093 ) ) 
 REPRESENTATION_ITEM ( '' )  );
#36562 = CARTESIAN_POINT ( 'NONE',  ( 66.66465390997532836, 68.91090369052673736, 2.096634673789778969 ) ) ;
#36563 = LINE ( 'NONE', #44160, #93073 ) ;
#36564 = CARTESIAN_POINT ( 'NONE',  ( 155.3513572141771704, 261.5705516107003064, -17.00592413546589299 ) ) ;
#36565 = ORIENTED_EDGE ( 'NONE', *, *, #39754, .F. ) ;
#36566 = ORIENTED_EDGE ( 'NONE', *, *, #25371, .F. ) ;
#36568 = CARTESIAN_POINT ( 'NONE',  ( 204.8189571845487080, 275.8901551335242175, 13.43702398685204358 ) ) ;
#36567 = CARTESIAN_POINT ( 'NONE',  ( -22.42236680055709641, 157.8615022471902591, 0.000000000000000000 ) ) ;
#36569 = CARTESIAN_POINT ( 'NONE',  ( 153.3703256797887775, 265.0017988796566897, 16.44314709207578318 ) ) ;
#36570 = ORIENTED_EDGE ( 'NONE', *, *, #19714, .T. ) ;
#36571 = CARTESIAN_POINT ( 'NONE',  ( 88.42385336119198769, 44.01808410483894107, -2.342466917228906098 ) ) ;
#36572 = CARTESIAN_POINT ( 'NONE',  ( 80.14460775109067470, 57.42271260518928244, -16.59269094194095473 ) ) ;
#36573 = CARTESIAN_POINT ( 'NONE',  ( 28.94742091202107304, 40.21091486745862653, 7.012934429366973338E-14 ) ) ;
#36574 = EDGE_LOOP ( 'NONE', ( #18160, #32019, #18192 ) ) ;
#36576 = EDGE_CURVE ( 'NONE', #79632, #21527, #89058, .T. ) ;
#36575 = CARTESIAN_POINT ( 'NONE',  ( 87.27117856089937220, 44.98890866680353895, -6.231534082530021834 ) ) ;
#36577 = CARTESIAN_POINT ( 'NONE',  ( 81.20226410207193624, 43.14699957628030802, 9.552668276955921911 ) ) ;
#36578 = VERTEX_POINT ( 'NONE', #57566 ) ;
#36579 = CARTESIAN_POINT ( 'NONE',  ( 164.6869624841032191, 245.4008089637804346, 1.435659848726088317 ) ) ;
#36580 = AXIS2_PLACEMENT_3D ( 'NONE', #90739, #22278, #14685 ) ;
#36581 = CARTESIAN_POINT ( 'NONE',  ( 74.34749166363997119, 62.52556080777176106, 14.76429959425114546 ) ) ;
#36582 = ORIENTED_EDGE ( 'NONE', *, *, #84624, .T. ) ;
#36583 = CARTESIAN_POINT ( 'NONE',  ( 176.2580550267919932, 278.7780497695933946, -16.99066290002705060 ) ) ;
#36584 = CARTESIAN_POINT ( 'NONE',  ( 172.3315061660855463, 263.8993054968007641, -15.56597864815643639 ) ) ;
#36585 = ORIENTED_EDGE ( 'NONE', *, *, #48483, .F. ) ;
#36586 = CYLINDRICAL_SURFACE ( 'NONE', #31942, 17.82106496071139645 ) ;
#36587 = CARTESIAN_POINT ( 'NONE',  ( 39.82000823235115661, 28.15404122711136736, 8.090169943749479842 ) ) ;
#36588 = CARTESIAN_POINT ( 'NONE',  ( 147.4323331177958494, 275.2867036919951147, -5.064030047414062707 ) ) ;
#36589 = VECTOR ( 'NONE', #71923, 1000.000000000000114 ) ;
#36590 = VERTEX_POINT ( 'NONE', #41877 ) ;
#36591 = ORIENTED_EDGE ( 'NONE', *, *, #59293, .T. ) ;
#36592 = CARTESIAN_POINT ( 'NONE',  ( 73.27173416076851709, 69.81779851018656302, 9.109861862100318675 ) ) ;
#36593 = CARTESIAN_POINT ( 'NONE',  ( 168.9557235653834368, 272.5620232158073009, 16.16789404307498046 ) ) ;
#36594 = CARTESIAN_POINT ( 'NONE',  ( 190.9586609929293104, 299.8968923453624598, -4.970176667899034229 ) ) ;
#36595 = CARTESIAN_POINT ( 'NONE',  ( 82.53276180672601470, 53.86864964727562466, 15.84768121842076916 ) ) ;
#36596 = CARTESIAN_POINT ( 'NONE',  ( 190.0226014859668453, 301.5181949703289774, 3.835066345245774500 ) ) ;
#36597 = CARTESIAN_POINT ( 'NONE',  ( 152.7153488183568300, 266.1362520814392951, 17.33540622643059237 ) ) ;
#36598 = CARTESIAN_POINT ( 'NONE',  ( 191.1017707189859038, 299.6490190287749442, 8.670441576909594161 ) ) ;
#36599 = CARTESIAN_POINT ( 'NONE',  ( 147.3047606266276546, 275.5076657283461827, -0.02269072295920609994 ) ) ;
#36600 = VERTEX_POINT ( 'NONE', #50468 ) ;
#36601 = CARTESIAN_POINT ( 'NONE',  ( 161.4250356354754672, 267.9004136800010656, 17.49898951125957680 ) ) ;
#36602 = LINE ( 'NONE', #66025, #97988 ) ;
#36603 = CARTESIAN_POINT ( 'NONE',  ( 164.3754245770190039, 245.9404084473339083, 1.667926061651832992 ) ) ;
#36604 = CARTESIAN_POINT ( 'NONE',  ( 67.31000428200415797, 66.58791411670934224, 8.576130451932648668 ) ) ;
#36605 = CARTESIAN_POINT ( 'NONE',  ( 169.7005567072155259, 288.7155782076579271, 4.430715832634252394 ) ) ;
#36606 = CARTESIAN_POINT ( 'NONE',  ( 86.81972942635061941, 43.51551237735639432, 4.206298849977907039 ) ) ;
#36607 = ORIENTED_EDGE ( 'NONE', *, *, #18318, .F. ) ;
#36608 = CARTESIAN_POINT ( 'NONE',  ( 190.1097268253669199, 301.3672894558616804, -3.549398112984228248 ) ) ;
#36609 = CARTESIAN_POINT ( 'NONE',  ( 80.43292161432816556, 52.70566313880177489, -15.44327005087032134 ) ) ;
#36610 = CARTESIAN_POINT ( 'NONE',  ( 202.9764883503618478, 278.1159216087813775, 15.04054422000245594 ) ) ;
#36611 = CARTESIAN_POINT ( 'NONE',  ( 79.32679490348121476, 45.77422221639383082, 12.97016535827635408 ) ) ;
#36612 = CARTESIAN_POINT ( 'NONE',  ( 179.5901059084964118, 282.7925552602970924, -15.57911077479886863 ) ) ;
#36613 = CARTESIAN_POINT ( 'NONE',  ( 189.8565127379117428, 301.8058691205260402, -0.2865444372480985269 ) ) ;
#36614 = ORIENTED_EDGE ( 'NONE', *, *, #92160, .F. ) ;
#36615 = CARTESIAN_POINT ( 'NONE',  ( 208.3790849386676598, 269.7238329819538762, -1.525282248498321946 ) ) ;
#36616 = DIRECTION ( 'NONE',  ( 0.5000000000000014433, -0.8660254037844378194, 0.000000000000000000 ) ) ;
#36617 = CARTESIAN_POINT ( 'NONE',  ( 155.4926790358130688, 262.9189171763118225, 17.50096092146387505 ) ) ;
#36618 = CARTESIAN_POINT ( 'NONE',  ( 41.93414601462609426, 195.0177522451418781, -10.00000000000009592 ) ) ;
#36619 = CARTESIAN_POINT ( 'NONE',  ( 119.6601863278771845, 230.7048013555409796, 4.594050593750051981 ) ) ;
#36620 = CARTESIAN_POINT ( 'NONE',  ( 151.3681950933278983, 268.4695907787949523, -15.50699599486383917 ) ) ;
#36621 = LINE ( 'NONE', #21929, #17326 ) ;
#36622 = CARTESIAN_POINT ( 'NONE',  ( 96.08673418588705317, 237.8297689869269220, -2.679491924311252493 ) ) ;
#36623 = CYLINDRICAL_SURFACE ( 'NONE', #23968, 16.60714546451156792 ) ;
#36624 = CARTESIAN_POINT ( 'NONE',  ( 29.24128764430186322, 193.8149278399160664, 9.188101187500093303 ) ) ;
#36626 = ADVANCED_FACE ( 'NONE', ( #97125 ), #57066, .F. ) ;
#36625 = VECTOR ( 'NONE', #82373, 1000.000000000000114 ) ;
#36627 = PLANE ( 'NONE',  #31652 ) ;
#36628 = AXIS2_PLACEMENT_3D ( 'NONE', #26162, #18570, #89511 ) ;
#36629 = VERTEX_POINT ( 'NONE', #42361 ) ;
#36630 = LINE ( 'NONE', #35648, #67292 ) ;
#36631 = CARTESIAN_POINT ( 'NONE',  ( -13.11024591527734628, 0.000000000000000000, 20.00000000000000000 ) ) ;
#36632 = CARTESIAN_POINT ( 'NONE',  ( -22.42236680055709641, 157.8615022471902591, 0.000000000000000000 ) ) ;
#36633 = VECTOR ( 'NONE', #58156, 1000.000000000000000 ) ;
#36634 = CARTESIAN_POINT ( 'NONE',  ( 76.61888230025124358, 51.35972145274618583, 16.07233720520855158 ) ) ;
#36635 = CARTESIAN_POINT ( 'NONE',  ( 81.67228854796844928, 59.26376530784745711, -0.4806308479691611679 ) ) ;
#36636 = EDGE_CURVE ( 'NONE', #39677, #14660, #41364, .T. ) ;
#36637 = CARTESIAN_POINT ( 'NONE',  ( -15.65624769481498468, 157.2602562327093381, -7.250946663043509766 ) ) ;
#36638 = CARTESIAN_POINT ( 'NONE',  ( 68.64667992883292413, 198.8932355074535394, -2.679491924311248496 ) ) ;
#36639 = CARTESIAN_POINT ( 'NONE',  ( 182.2453976510401219, 262.6361998111093499, 12.88021352968282152 ) ) ;
#36640 = CARTESIAN_POINT ( 'NONE',  ( 97.79278455872238851, 227.2677522451418497, 10.00000000000009592 ) ) ;
#36641 = EDGE_LOOP ( 'NONE', ( #6960, #52750, #7674, #9946 ) ) ;
#36642 = ADVANCED_FACE ( 'NONE', ( #58564 ), #81422, .T. ) ;
#36643 = CARTESIAN_POINT ( 'NONE',  ( 78.92023586790456591, 59.45316570216661489, -16.52216786098995982 ) ) ;
#36644 = CARTESIAN_POINT ( 'NONE',  ( 158.7916629078209496, 282.1994322289544925, -1.630852128393389666 ) ) ;
#36645 = CARTESIAN_POINT ( 'NONE',  ( 80.57044917996766742, 47.48882946736131316, -13.61647149455460060 ) ) ;
#36646 = CARTESIAN_POINT ( 'NONE',  ( 5.696048431029936410, 186.3464784336661637, 1.353441290958777327E-15 ) ) ;
#36647 = VECTOR ( 'NONE', #93080, 1000.000000000000114 ) ;
#36648 = CARTESIAN_POINT ( 'NONE',  ( 195.7970677195757219, 273.6457781951527295, 14.65595583657620615 ) ) ;
#36649 = CARTESIAN_POINT ( 'NONE',  ( 71.54138597657106402, 59.45382740952452849, -15.71570434403627914 ) ) ;
#36650 = CARTESIAN_POINT ( 'NONE',  ( 180.9072258576007073, 278.7294345915424287, 17.56943982383666736 ) ) ;
#36651 = CARTESIAN_POINT ( 'NONE',  ( 58.41569198217266035, 204.5333772461660544, 9.188101187500095079 ) ) ;
#36652 = CARTESIAN_POINT ( 'NONE',  ( 207.5570596878370679, 271.1476224814971374, 2.444960520848353358 ) ) ;
#36653 = CARTESIAN_POINT ( 'NONE',  ( 41.35966550219792026, 207.3877816888192172, 4.672379723982937232E-14 ) ) ;
#36654 = CARTESIAN_POINT ( 'NONE',  ( 70.08103292479646029, 69.71338913789749370, 6.159423539454167873 ) ) ;
#36655 = CARTESIAN_POINT ( 'NONE',  ( 207.6900289502458179, 270.9173129631602706, 7.178327969100043227 ) ) ;
#36656 = ORIENTED_EDGE ( 'NONE', *, *, #41013, .T. ) ;
#36657 = VECTOR ( 'NONE', #65263, 1000.000000000000227 ) ;
#36658 = CARTESIAN_POINT ( 'NONE',  ( 25.13686162393838330, 171.9865022471901739, 1.119607411625061291E-15 ) ) ;
#36659 = CARTESIAN_POINT ( 'NONE',  ( 207.6172352878830907, 271.0433952848413810, 3.316653249540578496 ) ) ;
#36660 = CARTESIAN_POINT ( 'NONE',  ( 144.1522069568320887, 254.0333772461660260, 9.188101187500095079 ) ) ;
#36661 = CARTESIAN_POINT ( 'NONE',  ( 27.74991983456899902, 18.94754757982090254, 5.678558825948272215 ) ) ;
#36662 = CARTESIAN_POINT ( 'NONE',  ( 164.8095417749603939, 245.1884954040601201, 0.9289438697355421048 ) ) ;
#36663 = CARTESIAN_POINT ( 'NONE',  ( 87.97782240006738164, 43.76496563450898236, 2.369043524150744595 ) ) ;
#36664 = CARTESIAN_POINT ( 'NONE',  ( 63.56442718099752653, 219.0530062829863027, -4.648177544792955347E-16 ) ) ;
#36666 = CARTESIAN_POINT ( 'NONE',  ( 186.7527615248176858, 288.4939651830034677, 14.54212105726466753 ) ) ;
#36665 = CARTESIAN_POINT ( 'NONE',  ( -31.49356256989596758, 94.88921800892812541, 45.19948692389422717 ) ) ;
#36667 = CARTESIAN_POINT ( 'NONE',  ( 68.72121773276600720, 64.08709895911447063, 11.99045797092632526 ) ) ;
#36668 = VERTEX_POINT ( 'NONE', #72815 ) ;
#36669 = CARTESIAN_POINT ( 'NONE',  ( 80.04149297081583825, 46.93512272770157523, 13.46944761230850141 ) ) ;
#36670 = CARTESIAN_POINT ( 'NONE',  ( 207.7185302857748468, 270.8679472019405239, -1.571522964764315855 ) ) ;
#36671 = CARTESIAN_POINT ( 'NONE',  ( 181.7713838635636137, 288.0101961225868763, 13.76523526626820626 ) ) ;
#36672 = CYLINDRICAL_SURFACE ( 'NONE', #15955, 16.60714546451156792 ) ;
#36673 = CARTESIAN_POINT ( 'NONE',  ( 197.2954959431661450, 273.3383094587030655, -14.52450022571995447 ) ) ;
#36674 = ORIENTED_EDGE ( 'NONE', *, *, #72032, .F. ) ;
#36675 = DIRECTION ( 'NONE',  ( 0.3037402332698211915, 0.8935232438716343983, -0.3306933373297781809 ) ) ;
#36676 = CARTESIAN_POINT ( 'NONE',  ( 84.07593154235651411, 41.67012449508333560, -3.184661558897835310 ) ) ;
#36677 = EDGE_CURVE ( 'NONE', #30899, #11943, #34280, .T. ) ;
#36678 = EDGE_CURVE ( 'NONE', #50208, #93313, #41905, .T. ) ;
#36679 = DIRECTION ( 'NONE',  ( -0.8660254037844377084, -0.5000000000000014433, -0.000000000000000000 ) ) ;
#36680 = PLANE ( 'NONE',  #86095 ) ;
#36681 = LINE ( 'NONE', #98520, #20234 ) ;
#36682 = CARTESIAN_POINT ( 'NONE',  ( 67.29718787697062510, 68.46426409671040858, 5.180099965221677927 ) ) ;
#36683 = CARTESIAN_POINT ( 'NONE',  ( 153.2906404175950854, 265.1398178023911782, -17.60231834963988007 ) ) ;
#36684 = EDGE_LOOP ( 'NONE', ( #2767, #44779, #80103, #24392 ) ) ;
#36685 = CARTESIAN_POINT ( 'NONE',  ( 163.9961211234992788, 256.9275610305372766, 16.20495027727189807 ) ) ;
#36686 = CARTESIAN_POINT ( 'NONE',  ( 9.347034241948367850, 24.13478043621386604, 8.090169943749478065 ) ) ;
#36687 = CARTESIAN_POINT ( 'NONE',  ( 169.5762389015176552, 277.3387613457686030, 16.19092595284562108 ) ) ;
#36688 = ORIENTED_EDGE ( 'NONE', *, *, #48703, .T. ) ;
#36689 = CARTESIAN_POINT ( 'NONE',  ( 42.76202708541288899, 64.24573752441608576, 10.00000000000000000 ) ) ;
#36690 = CARTESIAN_POINT ( 'NONE',  ( 86.47758924397189162, 47.47278051051635117, -10.96120693267980784 ) ) ;
#36691 = CARTESIAN_POINT ( 'NONE',  ( 85.66574015724606284, 45.04611075343164117, -7.902063309705260608 ) ) ;
#36692 = ORIENTED_EDGE ( 'NONE', *, *, #54036, .T. ) ;
#36694 = EDGE_CURVE ( 'NONE', #27723, #87428, #90013, .T. ) ;
#36693 = CARTESIAN_POINT ( 'NONE',  ( 147.0276296945837373, 275.9876705829954062, 0.7617065417431535534 ) ) ;
#36695 = CARTESIAN_POINT ( 'NONE',  ( 185.4098756247172162, 291.0786892564822210, 12.10185257883743759 ) ) ;
#36696 = CARTESIAN_POINT ( 'NONE',  ( 163.8040269124969939, 246.9300982336122559, 6.025552750865228013 ) ) ;
#36697 = CARTESIAN_POINT ( 'NONE',  ( 189.5154352181616844, 269.0707619020402035, -14.34315308920730558 ) ) ;
#36698 = ORIENTED_EDGE ( 'NONE', *, *, #393, .T. ) ;
#36699 = CARTESIAN_POINT ( 'NONE',  ( 88.80803131805656392, 212.8923013555409796, 4.594050593750050204 ) ) ;
#36700 = CARTESIAN_POINT ( 'NONE',  ( 199.4204983887044591, 283.3295232521138587, 17.12415080298291059 ) ) ;
#36701 = AXIS2_PLACEMENT_3D ( 'NONE', #15633, #93180, #100268 ) ;
#36702 = CARTESIAN_POINT ( 'NONE',  ( 73.24862708662814725, 69.62355710376385787, -9.916407523326116191 ) ) ;
#36703 = CARTESIAN_POINT ( 'NONE',  ( 177.9519160049562743, 269.0639553700436863, -16.55811740720082526 ) ) ;
#36704 = CARTESIAN_POINT ( 'NONE',  ( -19.65312891409030271, 93.06504152958497400, -10.00000000000000888 ) ) ;
#36705 = EDGE_CURVE ( 'NONE', #84611, #7688, #77128, .T. ) ;
#36706 = ORIENTED_EDGE ( 'NONE', *, *, #65851, .F. ) ;
#36707 = EDGE_CURVE ( 'NONE', #21557, #78500, #64781, .T. ) ;
#36708 = ORIENTED_EDGE ( 'NONE', *, *, #62706, .F. ) ;
#36709 = CARTESIAN_POINT ( 'NONE',  ( 88.30697365647166919, 43.76017805630483792, 0.1929712240254211064 ) ) ;
#36710 = EDGE_LOOP ( 'NONE', ( #56666, #34903, #16903, #80116, #93178, #57287 ) ) ;
#36711 = CARTESIAN_POINT ( 'NONE',  ( 81.71781958264638490, 51.51165968475822865, 14.81913671552966782 ) ) ;
#36712 = ORIENTED_EDGE ( 'NONE', *, *, #37351, .F. ) ;
#36713 = CARTESIAN_POINT ( 'NONE',  ( 75.46810260959550476, 60.99596198493017596, 15.47750355691660928 ) ) ;
#36714 = CARTESIAN_POINT ( 'NONE',  ( 87.89611104468033886, 44.97730679797474806, 6.346758332113888734 ) ) ;
#36715 = ORIENTED_EDGE ( 'NONE', *, *, #49270, .F. ) ;
#36716 = CARTESIAN_POINT ( 'NONE',  ( 165.0017188223714868, 244.8556349938953929, 2.184410744653827674 ) ) ;
#36717 = AXIS2_PLACEMENT_3D ( 'NONE', #49452, #40337, #87538 ) ;
#36718 = CARTESIAN_POINT ( 'NONE',  ( 49.10122569834316408, 93.29622288527660601, 10.00000000000000000 ) ) ;
#36719 = CARTESIAN_POINT ( 'NONE',  ( 45.19716250472275476, 70.24742367233086782, -10.00000000000000000 ) ) ;
#36720 = CARTESIAN_POINT ( 'NONE',  ( -23.57665515266768352, 99.71860730699962971, 45.19943101769310090 ) ) ;
#36721 = CARTESIAN_POINT ( 'NONE',  ( 68.17914949951172332, 68.35117902963239089, -6.585394223376196621 ) ) ;
#36722 = CARTESIAN_POINT ( 'NONE',  ( 195.7108479875464297, 291.6658630236173622, -17.27467541470428714 ) ) ;
#36723 = ORIENTED_EDGE ( 'NONE', *, *, #82786, .F. ) ;
#36724 = CARTESIAN_POINT ( 'NONE',  ( 66.10925264684654223, 68.74481801009629578, 0.07444925924169307208 ) ) ;
#36725 = CARTESIAN_POINT ( 'NONE',  ( 7.128892988474023085, 19.51421378149916563, -9.188101187500004485 ) ) ;
#36726 = ORIENTED_EDGE ( 'NONE', *, *, #8783, .F. ) ;
#36727 = CARTESIAN_POINT ( 'NONE',  ( 165.7352987039666061, 282.5727979134155134, 8.872472809700889584 ) ) ;
#36729 = ORIENTED_EDGE ( 'NONE', *, *, #62706, .T. ) ;
#36728 = DIRECTION ( 'NONE',  ( -0.8660254037844378194, -0.5000000000000014433, -0.000000000000000000 ) ) ;
#36730 = AXIS2_PLACEMENT_3D ( 'NONE', #17307, #86771, #79658 ) ;
#36731 = CARTESIAN_POINT ( 'NONE',  ( 202.2712651538608668, 280.3028871727136675, 16.13191389836473988 ) ) ;
#36732 = CARTESIAN_POINT ( 'NONE',  ( 188.2057398500588192, 260.7838726571292227, 2.785644019878456668 ) ) ;
#36733 = CARTESIAN_POINT ( 'NONE',  ( 152.0629200551952351, 277.0898023037734674, -5.235464967198216080 ) ) ;
#36734 = CARTESIAN_POINT ( 'NONE',  ( 58.47569090598248209, 179.7419560658249509, 18.47570218321542868 ) ) ;
#36735 = DIRECTION ( 'NONE',  ( 1.000000000000000000, 0.000000000000000000, 0.000000000000000000 ) ) ;
#36736 = CARTESIAN_POINT ( 'NONE',  ( 84.19323161989967730, 41.93389703806564484, 0.8519107653881009545 ) ) ;
#36737 = CARTESIAN_POINT ( 'NONE',  ( 157.8229873034836999, 281.2890896376861747, 1.531573202618901508 ) ) ;
#36738 = ORIENTED_EDGE ( 'NONE', *, *, #85057, .T. ) ;
#36739 = CARTESIAN_POINT ( 'NONE',  ( 181.8744732730408487, 270.4285964791639572, -16.45852818176540922 ) ) ;
#36740 = VECTOR ( 'NONE', #26978, 1000.000000000000000 ) ;
#36741 = CARTESIAN_POINT ( 'NONE',  ( 71.33397847007799442, 63.32150720262168164, -13.53983176248328313 ) ) ;
#36742 = VERTEX_POINT ( 'NONE', #98088 ) ;
#36743 = CARTESIAN_POINT ( 'NONE',  ( 7.022496928113825199, 174.8615022471902591, -10.00000000000009592 ) ) ;
#36744 = CARTESIAN_POINT ( 'NONE',  ( 0.2927578493243879754, 157.6427522451417360, 1.119607411625061291E-15 ) ) ;
#36745 = CARTESIAN_POINT ( 'NONE',  ( 192.8093881745433578, 266.9317635038931940, -11.27160849829442668 ) ) ;
#36746 = LINE ( 'NONE', #22551, #72968 ) ;
#36747 = CARTESIAN_POINT ( 'NONE',  ( 170.1404595856897686, 280.7340597449264692, -14.11196382480607170 ) ) ;
#36748 = CARTESIAN_POINT ( 'NONE',  ( 86.26929602985893553, 44.64143340914854718, -6.561271146724712011 ) ) ;
#36749 = CARTESIAN_POINT ( 'NONE',  ( 161.3667600300080380, 272.7931144062943076, 15.17166901843044080 ) ) ;
#36751 = CARTESIAN_POINT ( 'NONE',  ( -4.037369169597886831, 175.1427522451419065, 10.00000000000009415 ) ) ;
#36750 = CARTESIAN_POINT ( 'NONE',  ( 1.691375130056927079, 159.5327760586659451, 1.948934522072303157E-15 ) ) ;
#36752 = EDGE_CURVE ( 'NONE', #1290, #76499, #97605, .T. ) ;
#36753 = CARTESIAN_POINT ( 'NONE',  ( 187.9452548533183460, 296.3769502305851233, 8.122909483408376374 ) ) ;
#36754 = ORIENTED_EDGE ( 'NONE', *, *, #15155, .T. ) ;
#36755 = ORIENTED_EDGE ( 'NONE', *, *, #70139, .F. ) ;
#36756 = FACE_BOUND ( 'NONE', #39541, .T. ) ;
#36757 = CARTESIAN_POINT ( 'NONE',  ( -19.65312891409030271, 93.06504152958497400, 10.00000000000000888 ) ) ;
#36758 = EDGE_CURVE ( 'NONE', #88888, #38611, #59044, .T. ) ;
#36759 = CARTESIAN_POINT ( 'NONE',  ( 67.07192012151503491, 67.07552343309768617, -8.606452331924455024 ) ) ;
#36760 = CARTESIAN_POINT ( 'NONE',  ( 20.28716687417668751, 35.21091486745861232, 7.012934429366973338E-14 ) ) ;
#36761 = CARTESIAN_POINT ( 'NONE',  ( 202.5853389232562733, 279.7588954467959752, -15.97445231646760178 ) ) ;
#36762 = CARTESIAN_POINT ( 'NONE',  ( 46.28462696178780789, 185.9824982072973967, 3.021315404115420679E-15 ) ) ;
#36763 = CARTESIAN_POINT ( 'NONE',  ( 153.4741497343565868, 278.8061389251365654, 3.770324642130308934 ) ) ;
#36764 = CARTESIAN_POINT ( 'NONE',  ( 20.58138070222250349, 176.5643266524160140, -9.188101187500093303 ) ) ;
#36765 = CARTESIAN_POINT ( 'NONE',  ( 113.7873647845227225, 230.3768266524160140, -9.188101187500091527 ) ) ;
#36766 = DIRECTION ( 'NONE',  ( -0.9634819383873037824, 0.2491829092639717136, 0.09803281150812255540 ) ) ;
#36767 = DIRECTION ( 'NONE',  ( -0.8660254037844387076, -0.4999999999999998890, -0.000000000000000000 ) ) ;
#36768 = ADVANCED_FACE ( 'NONE', ( #38621 ), #47232, .T. ) ;
#36769 = CARTESIAN_POINT ( 'NONE',  ( 206.2370539054256824, 271.7243903019979143, -8.078859316864654971 ) ) ;
#36770 = CARTESIAN_POINT ( 'NONE',  ( 175.4961364399792672, 281.6643638624120172, -14.18804244962221794 ) ) ;
#36771 = VECTOR ( 'NONE', #69676, 1000.000000000000000 ) ;
#36772 = CARTESIAN_POINT ( 'NONE',  ( 65.31683191680592415, 208.5177522451418497, -10.00000000000009592 ) ) ;
#36773 = VECTOR ( 'NONE', #70859, 1000.000000000000114 ) ;
#36774 = CARTESIAN_POINT ( 'NONE',  ( 154.8838596469624349, 262.3802811495310152, 18.07457254681616021 ) ) ;
#36775 = CARTESIAN_POINT ( 'NONE',  ( 184.4288184562230697, 274.3616139070439317, 17.06261365940633468 ) ) ;
#36776 = CARTESIAN_POINT ( 'NONE',  ( 81.80713581745879992, 45.61783045263506864, 11.73987135276072280 ) ) ;
#36777 = CARTESIAN_POINT ( 'NONE',  ( -89.11465314115667979, 93.37593066204033221, -30.52142883766496695 ) ) ;
#36778 = EDGE_CURVE ( 'NONE', #77944, #96074, #17693, .T. ) ;
#36779 = CARTESIAN_POINT ( 'NONE',  ( 84.54065070028998718, 50.22889876405420040, 13.87834917160721737 ) ) ;
#36780 = CARTESIAN_POINT ( 'NONE',  ( 186.7681815113486437, 299.1371796739298361, -0.6084766120471760686 ) ) ;
#36781 = DIRECTION ( 'NONE',  ( 0.5906904945688935538, 0.000000000000000000, -0.8068982213550578431 ) ) ;
#36782 = CARTESIAN_POINT ( 'NONE',  ( 67.06923665261433598, 197.9824982072973967, 3.021315404115420679E-15 ) ) ;
#36783 = ADVANCED_FACE ( 'NONE', ( #16331 ), #94214, .F. ) ;
#36784 = DIRECTION ( 'NONE',  ( -0.8660254037844387076, -0.4999999999999998890, -0.000000000000000000 ) ) ;
#36785 = CARTESIAN_POINT ( 'NONE',  ( 84.14312167556933275, 48.98415679381830756, 0.000000000000000000 ) ) ;
#36786 = CARTESIAN_POINT ( 'NONE',  ( 96.08779704679574252, 226.2833772461660260, -9.188101187500095079 ) ) ;
#36787 = CARTESIAN_POINT ( 'NONE',  ( 5.558032429380089567, 24.18502408145590010, 5.678558825948277544 ) ) ;
#36788 = LINE ( 'NONE', #22091, #51622 ) ;
#36790 = CARTESIAN_POINT ( 'NONE',  ( 152.0771670635943451, 267.2416153051512424, 17.00512325015557380 ) ) ;
#36789 = CARTESIAN_POINT ( 'NONE',  ( 187.6937625757019248, 280.4432552554100653, 17.79435256663161624 ) ) ;
#36791 = CARTESIAN_POINT ( 'NONE',  ( 196.3641580329410203, 290.5342968318988142, 17.59485314755329810 ) ) ;
#36792 = CARTESIAN_POINT ( 'NONE',  ( 151.4428545556028780, 268.3402767968688067, -15.03309903163500749 ) ) ;
#36793 = CARTESIAN_POINT ( 'NONE',  ( 173.4712241781546993, 267.5592519596314673, -16.59005366076430477 ) ) ;
#36794 = CARTESIAN_POINT ( 'NONE',  ( 45.07042791025775585, 28.94754757982093452, 5.678558825948272215 ) ) ;
#36795 = CARTESIAN_POINT ( 'NONE',  ( 193.0142717932987182, 296.3364699985351081, -13.30037542329744937 ) ) ;
#36796 = DIRECTION ( 'NONE',  ( 0.5000000000000014433, -0.8660254037844378194, 0.000000000000000000 ) ) ;
#36797 = VERTEX_POINT ( 'NONE', #86097 ) ;
#36798 = CARTESIAN_POINT ( 'NONE',  ( 26.01786902700012405, 17.94754757982089899, 5.678558825948272215 ) ) ;
#36799 = CIRCLE ( 'NONE', #28711, 0.1418229129680828593 ) ;
#36800 = DIRECTION ( 'NONE',  ( -1.000000000000000000, 1.957058632818291033E-13, 0.000000000000000000 ) ) ;
#36801 = CARTESIAN_POINT ( 'NONE',  ( 193.0761489135300906, 296.2292956824684893, -11.99675185248219655 ) ) ;
#36802 = CARTESIAN_POINT ( 'NONE',  ( 197.0184425104562820, 289.4010428742387262, -16.90752553128928426 ) ) ;
#36803 = EDGE_CURVE ( 'NONE', #23266, #76921, #47519, .T. ) ;
#36804 = B_SPLINE_CURVE_WITH_KNOTS ( 'NONE', 3,
 ( #45384, #14501, #13516, #22593 ),
 .UNSPECIFIED., .F., .F.,
 ( 4, 4 ),
 ( 0.009404506255995710717, 0.01466610642007075069 ),
 .UNSPECIFIED. ) ;
#36805 = CARTESIAN_POINT ( 'NONE',  ( 70.42108267803217814, 60.99865500005843444, 14.93332735863378780 ) ) ;
#36806 = CARTESIAN_POINT ( 'NONE',  ( 198.6755293322981117, 286.5308843062557571, 17.86676876308990103 ) ) ;
#36807 = CARTESIAN_POINT ( 'NONE',  ( 157.5527251258240256, 268.7623409241362538, 15.65735544631393772 ) ) ;
#36808 = CARTESIAN_POINT ( 'NONE',  ( -17.42236680055705023, 149.2012482093457777, 0.000000000000000000 ) ) ;
#36809 = CARTESIAN_POINT ( 'NONE',  ( 139.5965524907817041, 244.7365022471902023, -10.00000000000009059 ) ) ;
#36810 = EDGE_CURVE ( 'NONE', #58510, #55501, #44834, .T. ) ;
#36811 = VECTOR ( 'NONE', #72091, 1000.000000000000000 ) ;
#36812 = ORIENTED_EDGE ( 'NONE', *, *, #88511, .T. ) ;
#36813 = CARTESIAN_POINT ( 'NONE',  ( 190.2187748366491178, 299.5345473012424691, -6.575473572855297100 ) ) ;
#36814 = ORIENTED_EDGE ( 'NONE', *, *, #27456, .F. ) ;
#36815 = DIRECTION ( 'NONE',  ( -0.5078630399532131356, -0.8614378286617561109, 0.000000000000000000 ) ) ;
#36816 = CARTESIAN_POINT ( 'NONE',  ( 167.6278246310154714, 282.5728663012718584, -12.21306354836790220 ) ) ;
#36817 = VERTEX_POINT ( 'NONE', #57614 ) ;
#36819 = EDGE_CURVE ( 'NONE', #76358, #10367, #43489, .T. ) ;
#36818 = CARTESIAN_POINT ( 'NONE',  ( 87.92095387379619353, 44.55545140323351205, 4.092705293591274440 ) ) ;
#36821 = ORIENTED_EDGE ( 'NONE', *, *, #15771, .F. ) ;
#36820 = B_SPLINE_CURVE_WITH_KNOTS ( 'NONE', 3,
 ( #54770, #47173, #39057, #86745 ),
 .UNSPECIFIED., .F., .F.,
 ( 4, 4 ),
 ( 0.01222404534472665630, 0.01842418820188282402 ),
 .UNSPECIFIED. ) ;
#36823 = ADVANCED_FACE ( 'NONE', ( #64741 ), #95051, .T. ) ;
#36822 = CARTESIAN_POINT ( 'NONE',  ( 39.16110834368297589, 204.9637435831424739, 2.679491924311251605 ) ) ;
#36824 = DIRECTION ( 'NONE',  ( 0.5000000000000007772, -0.8660254037844381525, 0.000000000000000000 ) ) ;
#36825 = CARTESIAN_POINT ( 'NONE',  ( 191.6668504928946959, 279.4506890766722904, -16.59293083056063267 ) ) ;
#36826 = CARTESIAN_POINT ( 'NONE',  ( 193.2920900494724492, 295.8552746635717767, -12.94670270598705031 ) ) ;
#36827 = CARTESIAN_POINT ( 'NONE',  ( 152.6621968174709991, 266.2283140474973493, -17.02835521334403168 ) ) ;
#36828 = EDGE_CURVE ( 'NONE', #51434, #76991, #72451, .T. ) ;
#36829 = EDGE_CURVE ( 'NONE', #61284, #82304, #65203, .T. ) ;
#36830 = CARTESIAN_POINT ( 'NONE',  ( 38.30580752471379213, 37.51421378149922958, -9.188101187500004485 ) ) ;
#36831 = CARTESIAN_POINT ( 'NONE',  ( 78.59762652305811059, 58.68933280073064651, -16.17866137717102148 ) ) ;
#36832 = EDGE_CURVE ( 'NONE', #62465, #94177, #87808, .T. ) ;
#36833 = CYLINDRICAL_SURFACE ( 'NONE', #22260, 17.82106496071139645 ) ;
#36834 = LINE ( 'NONE', #82504, #43205 ) ;
#36835 = VERTEX_POINT ( 'NONE', #26212 ) ;
#36836 = VERTEX_POINT ( 'NONE', #7625 ) ;
#36837 = CARTESIAN_POINT ( 'NONE',  ( 157.6500260163024620, 257.5891404556457474, -18.23450497588216379 ) ) ;
#36838 = CARTESIAN_POINT ( 'NONE',  ( 87.23676543452685905, 46.07418070687454303, -8.827152287545313669 ) ) ;
#36840 = CARTESIAN_POINT ( 'NONE',  ( 165.7305853283280612, 273.9508576969337241, -15.18882091205272289 ) ) ;
#36839 = CARTESIAN_POINT ( 'NONE',  ( 173.8469137325424185, 256.4471593116459189, -12.44389045026504270 ) ) ;
#36841 = CARTESIAN_POINT ( 'NONE',  ( -19.65312891409030271, 93.06504152958497400, 10.00000000000000888 ) ) ;
#36842 = CARTESIAN_POINT ( 'NONE',  ( 197.6251864986240889, 273.3509762406971504, -13.38841307642727863 ) ) ;
#36843 = CARTESIAN_POINT ( 'NONE',  ( 157.8143401782468800, 281.6959594171767662, 4.961866816185521500 ) ) ;
#36844 = CARTESIAN_POINT ( 'NONE',  ( 82.40498086807166089, 40.38612597002704518, 0.9999930885993705276 ) ) ;
#36845 = VECTOR ( 'NONE', #97230, 1000.000000000000114 ) ;
#36846 = CARTESIAN_POINT ( 'NONE',  ( 170.5559173367651340, 288.6221555414043678, -4.098126037284842482 ) ) ;
#36847 = CARTESIAN_POINT ( 'NONE',  ( 77.30322683057316624, 63.13261582766239854, -15.24451728302370235 ) ) ;
#36848 = CARTESIAN_POINT ( 'NONE',  ( 78.89591602029014439, 59.68745106357756924, 16.49891905133565118 ) ) ;
#36849 = CARTESIAN_POINT ( 'NONE',  ( 117.4951228184160783, 229.4548013555409796, -4.594050593750042211 ) ) ;
#36850 = CARTESIAN_POINT ( 'NONE',  ( 148.1723659060776299, 275.6436025059589383, -5.668295273900294085 ) ) ;
#36851 = CARTESIAN_POINT ( 'NONE',  ( 35.38177548881301249, 32.37878583063844218, 9.188101187500006262 ) ) ;
#36852 = CARTESIAN_POINT ( 'NONE',  ( 191.8882076080898003, 275.3147623427439044, 16.31405584673956355 ) ) ;
#36853 = VECTOR ( 'NONE', #53188, 1000.000000000000114 ) ;
#36854 = EDGE_LOOP ( 'NONE', ( #41671, #16027, #96193, #17265 ) ) ;
#36855 = AXIS2_PLACEMENT_3D ( 'NONE', #55224, #30943, #8648 ) ;
#36856 = CARTESIAN_POINT ( 'NONE',  ( 74.21225604557145061, 68.54784490154126786, -11.57567064299385784 ) ) ;
#36858 = B_SPLINE_SURFACE_WITH_KNOTS ( 'NONE', 3, 1, ( 
 ( #82866, #13439 ),
 ( #81862, #44305 ),
 ( #3353, #66122 ),
 ( #12439, #34229 ),
 ( #43306, #97071 ),
 ( #28613, #74253 ),
 ( #65124, #28116 ),
 ( #59497, #89959 ),
 ( #20538, #51417 ),
 ( #99034, #45305 ),
 ( #14424, #60491 ),
 ( #75733, #98541 ),
 ( #83858, #60994 ),
 ( #7305, #13920 ),
 ( #83354, #53887 ),
 ( #38186, #29131 ),
 ( #46282, #6318 ),
 ( #85352, #75235 ),
 ( #76240, #22011 ),
 ( #21525, #37695 ),
 ( #6814, #208 ),
 ( #84847, #69604 ),
 ( #44798, #37209 ),
 ( #92450, #68606 ),
 ( #99529, #52907 ),
 ( #68110, #29618 ),
 ( #30112, #59998 ),
 ( #91449, #52408 ),
 ( #91962, #5816 ),
 ( #22510, #69102 ),
 ( #90967, #53404 ) ),
 .UNSPECIFIED., .F., .F., .F.,
 ( 4, 3, 3, 3, 3, 3, 3, 3, 3, 3, 4 ),
 ( 2, 2 ),
 ( 0.000000000000000000, 0.1122669598086762227, 0.2243161639709647659, 0.3396355846219160091, 0.4553962076585160723, 0.5677860799922405111, 0.6749047109689648716, 0.7773884377078511543, 0.8775581155834262237, 0.9782364162378021089, 1.000000000000000000 ),
 ( 0.000000000000000000, 1.000000000000000000 ),
 .UNSPECIFIED. ) ;
#36857 = CARTESIAN_POINT ( 'NONE',  ( 180.7471050872008220, 294.1104588566450388, -2.489982966172171075 ) ) ;
#36859 = CARTESIAN_POINT ( 'NONE',  ( 195.6986305151803549, 291.6870243064952888, 16.84182339398051909 ) ) ;
#36860 = CARTESIAN_POINT ( 'NONE',  ( 190.4322164364161836, 300.4051867369805109, -0.3674591292211766835 ) ) ;
#36861 = CARTESIAN_POINT ( 'NONE',  ( 73.81768256443291421, 55.15394748217288878, -16.12362769555734943 ) ) ;
#36862 = VERTEX_POINT ( 'NONE', #94642 ) ;
#36863 = AXIS2_PLACEMENT_3D ( 'NONE', #99458, #76171, #70025 ) ;
#36864 =( BOUNDED_CURVE ( )  B_SPLINE_CURVE ( 2, ( #8753, #61444, #31045, #39624, #61932, #77151, #92396, #53832, #48254 ),
 .UNSPECIFIED., .F., .T. ) 
 B_SPLINE_CURVE_WITH_KNOTS ( ( 3, 2, 2, 2, 3 ),
 ( 0.3024193548387096864, 0.3037634408602150615, 0.3064516129032258118, 0.3091397849462365621, 0.3104838709677419373 ),
 .UNSPECIFIED. ) 
 CURVE ( )  GEOMETRIC_REPRESENTATION_ITEM ( )  RATIONAL_B_SPLINE_CURVE ( ( 0.9330127018922194093, 0.9330127018922194093, 1.000000000000000000, 0.8660254037844387076, 1.000000000000000000, 0.8660254037844387076, 1.000000000000000000, 0.9330127018922194093, 0.9330127018922194093 ) ) 
 REPRESENTATION_ITEM ( '' )  );
#36865 = ORIENTED_EDGE ( 'NONE', *, *, #88365, .T. ) ;
#36866 = LINE ( 'NONE', #59655, #12363 ) ;
#36867 = EDGE_LOOP ( 'NONE', ( #6928, #90987, #19374, #84015 ) ) ;
#36868 = VECTOR ( 'NONE', #86722, 1000.000000000000000 ) ;
#36869 = B_SPLINE_CURVE_WITH_KNOTS ( 'NONE', 3,
 ( #7045, #8061, #14155, #92201 ),
 .UNSPECIFIED., .F., .F.,
 ( 4, 4 ),
 ( 0.009708450334000175153, 0.01488528937472419038 ),
 .UNSPECIFIED. ) ;
#36870 = CARTESIAN_POINT ( 'NONE',  ( 192.0312662756419968, 263.6944243638656644, -8.255564916146489907 ) ) ;
#36871 = CARTESIAN_POINT ( 'NONE',  ( 191.2622316156482043, 288.8574828335728171, -16.55244734589887656 ) ) ;
#36872 = CARTESIAN_POINT ( 'NONE',  ( 83.12870697588047619, 46.63866199349129715, 11.37677525845150406 ) ) ;
#36874 = CARTESIAN_POINT ( 'NONE',  ( 160.3427821849308827, 281.3332481746720646, 5.617732255323795165 ) ) ;
#36873 = CARTESIAN_POINT ( 'NONE',  ( 185.8658015726157942, 289.8550116424679572, -13.28855460030198188 ) ) ;
#36875 = CARTESIAN_POINT ( 'NONE',  ( 201.2535035105529744, 282.0657020489176716, -18.08976065250591958 ) ) ;
#36876 = ORIENTED_EDGE ( 'NONE', *, *, #2303, .F. ) ;
#36877 = CARTESIAN_POINT ( 'NONE',  ( 147.4811722709131914, 275.2021117973970377, 3.890385073228495916 ) ) ;
#36879 = CARTESIAN_POINT ( 'NONE',  ( 182.4502886106904214, 259.6876753163259650, 10.69873880494191631 ) ) ;
#36878 = B_SPLINE_SURFACE_WITH_KNOTS ( 'NONE', 3, 1, ( 
 ( #92631, #31773 ),
 ( #23180, #16590 ),
 ( #47142, #9679 ),
 ( #8654, #2574 ),
 ( #17769, #2067 ),
 ( #25349, #63851 ),
 ( #47639, #64864 ),
 ( #78573, #71474 ),
 ( #94790, #41033 ),
 ( #33980, #93798 ),
 ( #25875, #24848 ),
 ( #62843, #40540 ),
 ( #56242, #39525 ),
 ( #3089, #71970 ),
 ( #70450, #16252 ),
 ( #9157, #32458 ),
 ( #79095, #32947 ),
 ( #33458, #31938 ),
 ( #86213, #95811 ),
 ( #10666, #48152 ),
 ( #87235, #56750 ),
 ( #1059, #70973 ),
 ( #64354, #48670 ),
 ( #40033, #87732 ),
 ( #79603, #55723 ),
 ( #1575, #63355 ),
 ( #10166, #95318 ),
 ( #16751, #24359 ),
 ( #72487, #94294 ),
 ( #55230, #18270 ),
 ( #49164, #86711 ),
 ( #17247, #80100 ),
 ( #41542, #54734 ),
 ( #85717, #78067 ) ),
 .UNSPECIFIED., .T., .F., .F.,
 ( 4, 2, 2, 2, 2, 2, 2, 2, 2, 2, 2, 2, 2, 2, 2, 2, 4 ),
 ( 2, 2 ),
 ( 0.000000000000000000, 0.06250000000000000000, 0.1250000000000000000, 0.1875000000000000000, 0.2500000000000000000, 0.3125000000000000000, 0.3750000000000000000, 0.4375000000000000000, 0.5000000000000000000, 0.5625000000000000000, 0.6250000000000000000, 0.6875000000000000000, 0.7500000000000000000, 0.8125000000000000000, 0.8750000000000000000, 0.9375000000000000000, 1.000000000000000000 ),
 ( 0.000000000000000000, 1.000000000000000000 ),
 .UNSPECIFIED. ) ;
#36880 = CARTESIAN_POINT ( 'NONE',  ( 82.00520898190409014, 41.07855118830696028, -3.357997168065204541 ) ) ;
#36881 = CARTESIAN_POINT ( 'NONE',  ( 170.3483830181634744, 248.6468970521230517, -0.2708202233927377578 ) ) ;
#36882 = CARTESIAN_POINT ( 'NONE',  ( 189.1385169928410050, 270.1064989654813644, -14.07419399057638643 ) ) ;
#36883 = DIRECTION ( 'NONE',  ( 0.000000000000000000, 0.000000000000000000, 1.000000000000000000 ) ) ;
#36884 = CARTESIAN_POINT ( 'NONE',  ( 84.20320819077289798, 44.90490820053396703, 8.816900774186109402 ) ) ;
#36885 = AXIS2_PLACEMENT_3D ( 'NONE', #42246, #73182, #57449 ) ;
#36886 = CARTESIAN_POINT ( 'NONE',  ( 71.24663194959873636, 70.66145086035419354, -5.577829393062136099 ) ) ;
#36887 = CARTESIAN_POINT ( 'NONE',  ( 75.51934661115029712, 226.6589784336661637, -6.496448406907675876E-16 ) ) ;
#36888 = CARTESIAN_POINT ( 'NONE',  ( 206.6703863510205679, 272.6833857505801006, -10.72500664779635393 ) ) ;
#36889 = CARTESIAN_POINT ( 'NONE',  ( 77.82724693974202523, 61.74329194277088106, 16.06526602017299865 ) ) ;
#36890 = LINE ( 'NONE', #85545, #59194 ) ;
#36891 = ADVANCED_FACE ( 'NONE', ( #42 ), #96144, .T. ) ;
#36892 = CARTESIAN_POINT ( 'NONE',  ( 207.1007598919583472, 271.9379569114424271, -6.086525981869248092 ) ) ;
#36893 = CARTESIAN_POINT ( 'NONE',  ( 65.75540090923432501, 69.08964119695666284, -0.2331724888047134736 ) ) ;
#36895 = CARTESIAN_POINT ( 'NONE',  ( -20.85314014021869866, 95.07777941523956144, 45.19947629006753687 ) ) ;
#36894 = CARTESIAN_POINT ( 'NONE',  ( 73.31376544620394498, 70.15701068496694859, -9.311920139903870464 ) ) ;
#36896 = EDGE_CURVE ( 'NONE', #63534, #31479, #27384, .T. ) ;
#36897 = CARTESIAN_POINT ( 'NONE',  ( 45.44687632901609931, 27.20801979619932709, -3.090169943749474069 ) ) ;
#36898 = CARTESIAN_POINT ( 'NONE',  ( 149.7629758376029656, 272.4687595327688996, -11.42952473512502465 ) ) ;
#36899 = CARTESIAN_POINT ( 'NONE',  ( 82.36286381532451628, 54.25719919591043805, 15.61971488265658792 ) ) ;
#36900 = CARTESIAN_POINT ( 'NONE',  ( 71.83801353683954005, 72.23051172126305630, 3.257724734605899730 ) ) ;
#36901 = ADVANCED_FACE ( 'NONE', ( #4396 ), #67187, .T. ) ;
#36902 = CARTESIAN_POINT ( 'NONE',  ( 23.88258191050314494, 196.8464784336661637, 1.353441290958777327E-15 ) ) ;
#36903 = CARTESIAN_POINT ( 'NONE',  ( 196.2255671652529259, 290.7743432561995860, 16.01325193769018185 ) ) ;
#36904 = DIRECTION ( 'NONE',  ( -0.000000000000000000, 0.000000000000000000, -1.000000000000000000 ) ) ;
#36905 = CARTESIAN_POINT ( 'NONE',  ( 77.61091722901258549, 51.28954777400819864, -15.42868554443497153 ) ) ;
#36906 = CARTESIAN_POINT ( 'NONE',  ( 71.68975264095180933, 72.03364086010030576, -1.589174013277645958 ) ) ;
#36907 = CARTESIAN_POINT ( 'NONE',  ( 54.19381813872350762, 202.0958772461660544, -9.188101187500095079 ) ) ;
#36908 = VECTOR ( 'NONE', #89408, 1000.000000000000000 ) ;
#36909 = CARTESIAN_POINT ( 'NONE',  ( 24.83368966200164607, 16.19860640527292261, 2.839279412974134775 ) ) ;
#36910 = CARTESIAN_POINT ( 'NONE',  ( 151.4376533647338476, 268.3492855237141725, -15.16853828792834236 ) ) ;
#36911 = DIRECTION ( 'NONE',  ( 0.2803049773603250028, -0.9599109957006575211, 0.000000000000000000 ) ) ;
#36912 = CARTESIAN_POINT ( 'NONE',  ( 46.58353466793526110, 27.86426979415093896, -3.090169943749474069 ) ) ;
#36913 = CARTESIAN_POINT ( 'NONE',  ( 204.9463377925012253, 275.6695254486514841, -14.15865086131798378 ) ) ;
#36914 = CARTESIAN_POINT ( 'NONE',  ( 159.7106966763185483, 255.6638636138267486, -16.45402655586279650 ) ) ;
#36915 = CARTESIAN_POINT ( 'NONE',  ( -13.93676304270635136, 104.6887507934693105, 43.89948692389422291 ) ) ;
#36916 = VECTOR ( 'NONE', #98041, 1000.000000000000000 ) ;
#36917 = EDGE_LOOP ( 'NONE', ( #51542, #79550, #58050, #82506 ) ) ;
#36918 = CARTESIAN_POINT ( 'NONE',  ( 72.35426931885450585, 60.46654658139856053, 15.04702401992514282 ) ) ;
#36919 = CARTESIAN_POINT ( 'NONE',  ( 71.29849878737984170, 67.80657138214567681, -10.00003097478887959 ) ) ;
#36920 = CARTESIAN_POINT ( 'NONE',  ( 163.8070446421170629, 255.0663642890118581, -15.42060242571707818 ) ) ;
#36921 = DIRECTION ( 'NONE',  ( 0.4999999999999998335, -0.8660254037844389297, 0.000000000000000000 ) ) ;
#36922 = CARTESIAN_POINT ( 'NONE',  ( 91.45997379709659469, 223.6115022471902307, 10.00000000000009592 ) ) ;
#36923 = CARTESIAN_POINT ( 'NONE',  ( 161.7910648966377209, 250.4166507187868831, 13.19274492748169436 ) ) ;
#36924 = EDGE_CURVE ( 'NONE', #89008, #47179, #85411, .T. ) ;
#36925 = CARTESIAN_POINT ( 'NONE',  ( 194.6544274154721563, 285.5701803447823295, -17.66485059694058180 ) ) ;
#36926 = ORIENTED_EDGE ( 'NONE', *, *, #95791, .F. ) ;
#36927 = CARTESIAN_POINT ( 'NONE',  ( 56.95410056540389832, 209.8149278399160949, -9.188101187500095079 ) ) ;
#36928 = VERTEX_POINT ( 'NONE', #97624 ) ;
#36929 = CARTESIAN_POINT ( 'NONE',  ( 166.2602210121610256, 265.2243045114799429, 16.56391771334216756 ) ) ;
#36930 = CARTESIAN_POINT ( 'NONE',  ( 17.00529913897481293, 33.43149683636511327, 10.00000000000000000 ) ) ;
#36931 = FACE_OUTER_BOUND ( 'NONE', #97223, .T. ) ;
#36932 = ORIENTED_EDGE ( 'NONE', *, *, #99358, .T. ) ;
#36933 = VECTOR ( 'NONE', #52318, 1000.000000000000114 ) ;
#36934 = B_SPLINE_CURVE_WITH_KNOTS ( 'NONE', 3,
 ( #50035, #78968, #40417, #87614 ),
 .UNSPECIFIED., .F., .F.,
 ( 4, 4 ),
 ( 0.007229077686816304769, 0.01226561482239176340 ),
 .UNSPECIFIED. ) ;
#36935 = LINE ( 'NONE', #13165, #37810 ) ;
#36937 = EDGE_CURVE ( 'NONE', #84233, #94567, #65689, .T. ) ;
#36936 = CARTESIAN_POINT ( 'NONE',  ( 79.32306449657336600, 46.19060395113251616, -13.25186856088700615 ) ) ;
#36938 = LINE ( 'NONE', #5546, #52444 ) ;
#36939 = CARTESIAN_POINT ( 'NONE',  ( 86.84624261559693537, 44.08215787897474058, 5.733795036492094432 ) ) ;
#36940 = CARTESIAN_POINT ( 'NONE',  ( 206.7789538869637909, 271.7428703762204805, -6.364171105215885582 ) ) ;
#36941 = EDGE_LOOP ( 'NONE', ( #5293, #44038, #80261, #21786, #90483, #66503, #23748, #60991, #93560, #75484, #61592, #13924, #54614, #22797, #39412, #57515, #73350, #81818, #98508, #31585 ) ) ;
#36942 = CARTESIAN_POINT ( 'NONE',  ( 28.52090319329062851, 17.26216523072495690, -2.296566073217252530E-15 ) ) ;
#36943 = CARTESIAN_POINT ( 'NONE',  ( 69.43213248134874505, 70.01719979072606748, -4.434620404520505765 ) ) ;
#36944 = CARTESIAN_POINT ( 'NONE',  ( 157.7255603307123408, 268.5163524934444013, 16.86592485641857309 ) ) ;
#36945 = EDGE_CURVE ( 'NONE', #45639, #75490, #54606, .T. ) ;
#36946 = VERTEX_POINT ( 'NONE', #5404 ) ;
#36947 = LINE ( 'NONE', #453, #32013 ) ;
#36948 = CARTESIAN_POINT ( 'NONE',  ( 206.8851632406098702, 272.3113812655195716, -9.957011741946159233 ) ) ;
#36949 = ORIENTED_EDGE ( 'NONE', *, *, #14689, .F. ) ;
#36950 = ORIENTED_EDGE ( 'NONE', *, *, #15399, .F. ) ;
#36951 = VECTOR ( 'NONE', #35020, 1000.000000000000227 ) ;
#36953 = DIRECTION ( 'NONE',  ( 0.000000000000000000, 1.000000000000000000, 0.000000000000000000 ) ) ;
#36952 = CARTESIAN_POINT ( 'NONE',  ( 160.4221878081525858, 282.4388110396778870, -3.172333647399238732 ) ) ;
#36954 = CARTESIAN_POINT ( 'NONE',  ( 208.3764315856425640, 269.7284287242038658, -1.833640725398759441 ) ) ;
#36955 = CARTESIAN_POINT ( 'NONE',  ( 204.6427704787179493, 276.1953194596412118, 13.28850621060895953 ) ) ;
#36956 = CARTESIAN_POINT ( 'NONE',  ( 198.4334039703542771, 286.9502577349437615, 18.47706603442866680 ) ) ;
#36957 = CARTESIAN_POINT ( 'NONE',  ( 81.66071111044179531, 55.73219010195405332, 16.34934455148813370 ) ) ;
#36958 = CARTESIAN_POINT ( 'NONE',  ( 204.2708887182014337, 271.6324151636133593, 9.900201553234905916 ) ) ;
#36959 = CARTESIAN_POINT ( 'NONE',  ( 130.3772506997096343, 236.8923013555409796, 4.594050593750050204 ) ) ;
#36960 = CARTESIAN_POINT ( 'NONE',  ( 83.28711936893076029, 209.7048013555409796, 4.594050593750051981 ) ) ;
#36961 = ORIENTED_EDGE ( 'NONE', *, *, #3349, .F. ) ;
#36962 = CARTESIAN_POINT ( 'NONE',  ( 173.8944842169933906, 265.3883602040215237, 16.80249544060196598 ) ) ;
#36963 = CARTESIAN_POINT ( 'NONE',  ( 75.12366170154771794, 59.47066623895606341, -16.21752462648118964 ) ) ;
#36964 = CARTESIAN_POINT ( 'NONE',  ( -19.34860767484687116, 59.83210158341513818, -10.00000000000000000 ) ) ;
#36965 = AXIS2_PLACEMENT_3D ( 'NONE', #70399, #47595, #38491 ) ;
#36966 = ORIENTED_EDGE ( 'NONE', *, *, #97182, .T. ) ;
#36967 = CARTESIAN_POINT ( 'NONE',  ( 161.1048434630436077, 252.8929743723557522, 14.67917439587344397 ) ) ;
#36968 = EDGE_LOOP ( 'NONE', ( #72749, #80, #91580, #48060 ) ) ;
#36969 = VERTEX_POINT ( 'NONE', #98111 ) ;
#36970 = CARTESIAN_POINT ( 'NONE',  ( 76.19402696226363503, 65.29190987809512592, 14.49924708549197128 ) ) ;
#36971 = DIRECTION ( 'NONE',  ( 1.000000000000000000, 0.000000000000000000, 0.000000000000000000 ) ) ;
#36972 = CARTESIAN_POINT ( 'NONE',  ( 194.3054841547469778, 284.7826021230907259, 17.31190127946796409 ) ) ;
#36973 = CARTESIAN_POINT ( 'NONE',  ( 83.61477352437640320, 42.16507195651136897, -5.583216967882105308 ) ) ;
#36974 = CARTESIAN_POINT ( 'NONE',  ( 81.37395530686723077, 56.14341791244839186, 16.08471380636200365 ) ) ;
#36975 = CARTESIAN_POINT ( 'NONE',  ( 193.9495889092963807, 294.7164532324382549, 15.46986001312306058 ) ) ;
#36976 = CARTESIAN_POINT ( 'NONE',  ( 72.80787385069068307, 70.05095376960370857, 8.379579475240937825 ) ) ;
#36977 = CARTESIAN_POINT ( 'NONE',  ( 87.34977546134365411, 44.90968568749349288, 6.842696035241853103 ) ) ;
#36978 = ORIENTED_EDGE ( 'NONE', *, *, #53061, .T. ) ;
#36979 = CARTESIAN_POINT ( 'NONE',  ( 16.25994779760268827, 31.16126292948894871, -6.180339887498951690 ) ) ;
#36980 = CARTESIAN_POINT ( 'NONE',  ( 153.2583947049096764, 265.1956690150883560, -17.64103123457563882 ) ) ;
#36981 = CARTESIAN_POINT ( 'NONE',  ( 200.6563829895864615, 283.0999451294737241, -16.73778976840113586 ) ) ;
#36982 = CIRCLE ( 'NONE', #30473, 70.00000000000001421 ) ;
#36983 = ORIENTED_EDGE ( 'NONE', *, *, #54186, .T. ) ;
#36984 = LINE ( 'NONE', #34986, #32359 ) ;
#36985 = EDGE_CURVE ( 'NONE', #24595, #45905, #28694, .T. ) ;
#36986 = CARTESIAN_POINT ( 'NONE',  ( 163.8003088823192286, 260.8948240748503054, -17.39314492925268141 ) ) ;
#36987 = CARTESIAN_POINT ( 'NONE',  ( 164.1360809937824001, 246.7355779274738268, 4.829182325609949089 ) ) ;
#36988 = CARTESIAN_POINT ( 'NONE',  ( 206.5117639185820906, 272.9581278627833285, 11.28485531511759099 ) ) ;
#36989 = CARTESIAN_POINT ( 'NONE',  ( 196.2379679265050925, 290.7528645076583871, -16.93678934971137906 ) ) ;
#36990 = CARTESIAN_POINT ( 'NONE',  ( 38.99326808448932979, 199.9865022471903160, 10.00000000000009415 ) ) ;
#36991 = CARTESIAN_POINT ( 'NONE',  ( 159.3000756570304475, 259.5621139873742322, 16.68461091752545755 ) ) ;
#36992 = VECTOR ( 'NONE', #72626, 1000.000000000000227 ) ;
#36993 = CARTESIAN_POINT ( 'NONE',  ( 137.4948102131217524, 244.0643266524159856, -9.188101187500093303 ) ) ;
#36994 = EDGE_LOOP ( 'NONE', ( #41042, #98761, #67235, #64032 ) ) ;
#36995 = CARTESIAN_POINT ( 'NONE',  ( 88.26872550477153823, 44.38513711945522289, 4.282355379009171514 ) ) ;
#36996 = CARTESIAN_POINT ( 'NONE',  ( 86.66434744208947905, 45.32692126891454620, 7.428864611774582905 ) ) ;
#36997 = CARTESIAN_POINT ( 'NONE',  ( 80.16100348863038505, 44.92770494338710563, -11.28789370626155097 ) ) ;
#36998 = CARTESIAN_POINT ( 'NONE',  ( 79.11723855630626190, 59.11194703662724237, -16.21433712332713029 ) ) ;
#36999 = CARTESIAN_POINT ( 'NONE',  ( 74.02530730923707836, 66.66790563868377717, -12.50284404751719691 ) ) ;
#37000 = ORIENTED_EDGE ( 'NONE', *, *, #83628, .T. ) ;
#37001 = PLANE ( 'NONE',  #8948 ) ;
#37002 = AXIS2_PLACEMENT_3D ( 'NONE', #38543, #77044, #75572 ) ;
#37003 = CARTESIAN_POINT ( 'NONE',  ( 182.1292595431042400, 275.5821809811551475, -16.44815416891946569 ) ) ;
#37004 = CARTESIAN_POINT ( 'NONE',  ( 72.60568633014737827, 71.36030734738318415, -5.924380567679106591 ) ) ;
#37005 = CARTESIAN_POINT ( 'NONE',  ( 81.53074493407929424, 54.33667322198162708, 15.71405181651475047 ) ) ;
#37006 = CARTESIAN_POINT ( 'NONE',  ( 49.19475937879462890, 79.05079877653317055, 10.00000000000000000 ) ) ;
#37007 = CARTESIAN_POINT ( 'NONE',  ( 198.4797950122827217, 266.2212529384890445, 0.7508312083940900106 ) ) ;
#37008 = CARTESIAN_POINT ( 'NONE',  ( 190.8683709797118411, 300.0532792356709706, -4.461919767133968762 ) ) ;
#37009 = CARTESIAN_POINT ( 'NONE',  ( 186.8391812638637077, 282.1527847936219473, 16.55419741524866595 ) ) ;
#37010 = VECTOR ( 'NONE', #41000, 1000.000000000000114 ) ;
#37011 = CARTESIAN_POINT ( 'NONE',  ( 157.1002372043759010, 258.5414026113353430, -17.73553732786789539 ) ) ;
#37012 = CARTESIAN_POINT ( 'NONE',  ( 195.5754259164033897, 270.4482758609249800, 12.00730134518774683 ) ) ;
#37013 = EDGE_CURVE ( 'NONE', #22248, #59341, #27712, .T. ) ;
#37014 = CARTESIAN_POINT ( 'NONE',  ( 26.80974344509558449, 15.28848085856231798, 1.475505719884397138E-15 ) ) ;
#37015 = DIRECTION ( 'NONE',  ( 1.000000000000000000, 0.000000000000000000, 0.000000000000000000 ) ) ;
#37016 = CARTESIAN_POINT ( 'NONE',  ( 205.4596735342297791, 274.3777508883674727, 10.94792961590592029 ) ) ;
#37017 = CARTESIAN_POINT ( 'NONE',  ( 26.55243232390424879, 15.73415679381822585, 1.333680081654574804E-15 ) ) ;
#37018 = CARTESIAN_POINT ( 'NONE',  ( 198.5966822647444587, 286.6674514332866579, 17.25284514431582750 ) ) ;
#37019 = ADVANCED_FACE ( 'NONE', ( #57588 ), #88567, .T. ) ;
#37020 = CARTESIAN_POINT ( 'NONE',  ( 207.1728383846156589, 271.8131133000269983, 5.812426782309712436 ) ) ;
#37021 = CARTESIAN_POINT ( 'NONE',  ( -2.801305199957352166, 163.0643266524159571, -9.188101187500093303 ) ) ;
#37022 = B_SPLINE_CURVE_WITH_KNOTS ( 'NONE', 3,
 ( #8244, #17329, #39109, #48235 ),
 .UNSPECIFIED., .F., .F.,
 ( 4, 4 ),
 ( 0.008522409322521112135, 0.01490883787878987191 ),
 .UNSPECIFIED. ) ;
#37023 = CARTESIAN_POINT ( 'NONE',  ( 175.5585873154026046, 286.2329552154398584, -11.98263329848505698 ) ) ;
#37024 = ORIENTED_EDGE ( 'NONE', *, *, #77318, .F. ) ;
#37025 = DIRECTION ( 'NONE',  ( -0.5000000000000014433, 0.8660254037844378194, 0.000000000000000000 ) ) ;
#37026 = CARTESIAN_POINT ( 'NONE',  ( 72.69592421641888791, 70.74456683587563077, -7.971905174712497377 ) ) ;
#37027 = CARTESIAN_POINT ( 'NONE',  ( 65.93257831369518840, 197.3262482093457777, 3.021315404115420679E-15 ) ) ;
#37028 = CARTESIAN_POINT ( 'NONE',  ( 150.6916211261701619, 269.6414512649903941, -15.44346024757110847 ) ) ;
#37029 = CARTESIAN_POINT ( 'NONE',  ( 6.129408228687162286, 174.3458772461660828, 9.188101187500095079 ) ) ;
#37030 = CARTESIAN_POINT ( 'NONE',  ( 181.6389525841213128, 276.3973689590053482, -17.23735931286679346 ) ) ;
#37031 = CARTESIAN_POINT ( 'NONE',  ( 27.94640178401474273, 15.94473085651393340, 1.475505719884397138E-15 ) ) ;
#37032 = CARTESIAN_POINT ( 'NONE',  ( 85.88643775857894980, 48.50416193104786799, 12.18167088616390537 ) ) ;
#37033 = DIRECTION ( 'NONE',  ( -0.000000000000000000, -0.000000000000000000, 1.000000000000000000 ) ) ;
#37034 = DIRECTION ( 'NONE',  ( 0.9659258262890695335, -0.2588190451025159655, 8.659560562354867531E-17 ) ) ;
#37035 = CARTESIAN_POINT ( 'NONE',  ( 150.1477792844964938, 276.5081346559795747, 3.786615811811071541 ) ) ;
#37036 = CARTESIAN_POINT ( 'NONE',  ( 179.2145810957732692, 255.1730852940781062, -3.979500447435403210 ) ) ;
#37037 = CARTESIAN_POINT ( 'NONE',  ( 197.9637121306999461, 287.7637878651254937, 17.83088679657193865 ) ) ;
#37038 = CARTESIAN_POINT ( 'NONE',  ( 47.72569090598240393, 208.3615022471902876, 5.000000000000046185 ) ) ;
#37039 = CARTESIAN_POINT ( 'NONE',  ( 82.24832262017582707, 41.31296476174959764, 5.425068656990536198 ) ) ;
#37040 = EDGE_CURVE ( 'NONE', #15680, #59906, #33486, .T. ) ;
#37041 = CARTESIAN_POINT ( 'NONE',  ( 148.1634546024981205, 274.0203641339852538, 9.324875965062235039 ) ) ;
#37042 = AXIS2_PLACEMENT_3D ( 'NONE', #79793, #80803, #9869 ) ;
#37043 = CARTESIAN_POINT ( 'NONE',  ( 10.18872876104421366, 182.8149278399160949, -9.188101187500095079 ) ) ;
#37044 = CARTESIAN_POINT ( 'NONE',  ( 164.7946292899401328, 284.8120369531133633, 4.194565866339356575 ) ) ;
#37045 = PLANE ( 'NONE',  #40328 ) ;
#37046 = CARTESIAN_POINT ( 'NONE',  ( 39.71070620960689723, 31.43085787977766898, -9.188101187500008038 ) ) ;
#37047 = CARTESIAN_POINT ( 'NONE',  ( 133.8285102913215212, 259.6199935810940929, 2.679491924311251605 ) ) ;
#37049 = CARTESIAN_POINT ( 'NONE',  ( 164.2578067403839555, 246.1441285162624126, -2.322300236470859591 ) ) ;
#37048 = AXIS2_PLACEMENT_3D ( 'NONE', #87576, #57081, #71313 ) ;
#37050 = CARTESIAN_POINT ( 'NONE',  ( 187.7682546158083881, 267.7859742100430935, 13.35512656275608734 ) ) ;
#37051 = DIRECTION ( 'NONE',  ( -0.000000000000000000, -0.000000000000000000, -1.000000000000000000 ) ) ;
#37052 = CARTESIAN_POINT ( 'NONE',  ( 164.1994998312905807, 281.4989144817481588, 9.158350551505991533 ) ) ;
#37053 = ITEM_DEFINED_TRANSFORMATION ( 'NONE', 'NONE', #52649,  #68784 ) ;
#37054 = VECTOR ( 'NONE', #76405, 1000.000000000000000 ) ;
#37055 = CARTESIAN_POINT ( 'NONE',  ( 13.34565549823491004, 29.74646525600389424, 2.839279412974139660 ) ) ;
#37056 = CARTESIAN_POINT ( 'NONE',  ( 147.6857584380539095, 274.8477581613835810, 8.112022437684441201 ) ) ;
#37057 = CARTESIAN_POINT ( 'NONE',  ( 71.44576612263118420, 59.19700591949954571, 15.27431131414821586 ) ) ;
#37058 = CARTESIAN_POINT ( 'NONE',  ( 194.4165969972361552, 293.9075714965812267, 14.23342188338008718 ) ) ;
#37059 = ORIENTED_EDGE ( 'NONE', *, *, #96740, .T. ) ;
#37060 = VECTOR ( 'NONE', #23031, 1000.000000000000114 ) ;
#37061 = CARTESIAN_POINT ( 'NONE',  ( 185.3905017119345473, 290.9592364371351323, 12.17893237875644452 ) ) ;
#37062 = CARTESIAN_POINT ( 'NONE',  ( 41.37327796571899796, 124.7191351846657028, -10.00000000000000000 ) ) ;
#37063 = CARTESIAN_POINT ( 'NONE',  ( 75.05139128669955539, 53.58935898396480724, -16.54232114207730930 ) ) ;
#37064 = CARTESIAN_POINT ( 'NONE',  ( 4.262040950003053830, 163.2677522451418213, -5.000000000000041744 ) ) ;
#37065 = ORIENTED_EDGE ( 'NONE', *, *, #18261, .F. ) ;
#37066 = DIRECTION ( 'NONE',  ( -0.5000000000000013323, 0.8660254037844379305, 0.000000000000000000 ) ) ;
#37067 = CARTESIAN_POINT ( 'NONE',  ( 68.67636306517070466, 70.25541593756011594, -0.5330109424154759745 ) ) ;
#37068 = CARTESIAN_POINT ( 'NONE',  ( 10.06845959268932411, 31.07446838803122446, -10.00000000000000000 ) ) ;
#37069 = CARTESIAN_POINT ( 'NONE',  ( 203.0498946958275326, 278.9542612457532869, -15.11479947333269003 ) ) ;
#37070 = EDGE_LOOP ( 'NONE', ( #18921, #66390, #84222, #74508 ) ) ;
#37071 = VECTOR ( 'NONE', #48672, 1000.000000000000114 ) ;
#37072 = VERTEX_POINT ( 'NONE', #7898 ) ;
#37074 = CARTESIAN_POINT ( 'NONE',  ( 204.7610021263893429, 275.9905362388115577, 13.36619428527026976 ) ) ;
#37073 = CARTESIAN_POINT ( 'NONE',  ( 186.5027827276450409, 272.0212515145463499, -16.58127060163710098 ) ) ;
#37075 = ORIENTED_EDGE ( 'NONE', *, *, #4862, .F. ) ;
#37076 = CARTESIAN_POINT ( 'NONE',  ( 88.35080703960181836, 43.95228889933407856, -2.194260235337642140 ) ) ;
#37077 = DIRECTION ( 'NONE',  ( 0.000000000000000000, 0.5247752241694969566, -0.8512408378936329179 ) ) ;
#37078 = CARTESIAN_POINT ( 'NONE',  ( 80.37878231636271664, 58.00653726389809606, 16.25895090469026627 ) ) ;
#37079 = CARTESIAN_POINT ( 'NONE',  ( 67.99156343939851865, 69.54710374710430187, -4.850653214453461537 ) ) ;
#37080 = VERTEX_POINT ( 'NONE', #46882 ) ;
#37081 = CARTESIAN_POINT ( 'NONE',  ( 189.8123550829396891, 301.8823524224806647, -0.5679054518196169354 ) ) ;
#37082 = EDGE_CURVE ( 'NONE', #48590, #59818, #14102, .T. ) ;
#37083 = VERTEX_POINT ( 'NONE', #84428 ) ;
#37084 = CARTESIAN_POINT ( 'NONE',  ( 205.7576124508049418, 274.2643565215761328, 10.88614016733041545 ) ) ;
#37085 = FACE_OUTER_BOUND ( 'NONE', #16310, .T. ) ;
#37086 = EDGE_LOOP ( 'NONE', ( #40687, #23091, #67461, #2352 ) ) ;
#37087 = CARTESIAN_POINT ( 'NONE',  ( 190.8153366230912411, 300.1451374358846920, 3.771947273125533684 ) ) ;
#37088 = CARTESIAN_POINT ( 'NONE',  ( 172.3662264184933406, 263.8501619316954248, -16.86127397973819697 ) ) ;
#37089 = EDGE_LOOP ( 'NONE', ( #10339, #95178, #76860, #3392 ) ) ;
#37090 = CARTESIAN_POINT ( 'NONE',  ( -14.16662337007866057, 72.61341060738401154, 13.96608703042485011 ) ) ;
#37091 = CARTESIAN_POINT ( 'NONE',  ( -13.86269525828471849, 104.2312461070085021, 36.50000000000000000 ) ) ;
#37092 = FACE_OUTER_BOUND ( 'NONE', #48091, .T. ) ;
#37093 = DIRECTION ( 'NONE',  ( 0.000000000000000000, -0.000000000000000000, 1.000000000000000000 ) ) ;
#37094 = ORIENTED_EDGE ( 'NONE', *, *, #85187, .F. ) ;
#37095 = EDGE_LOOP ( 'NONE', ( #50077, #3748, #90836, #92733 ) ) ;
#37096 = B_SPLINE_CURVE_WITH_KNOTS ( 'NONE', 3,
 ( #8812, #55885, #32617, #94452, #49321, #86880, #39681, #9840, #40699, #64522, #71641, #41196, #2235, #94955, #95479, #26032, #72648, #95965, #70608, #89849, #88887, #88383, #20424, #28496, #58880, #36093, #59376, #51290, #18936, #35101, #42201, #12833, #49813, #82261, #43695, #74636, #73621, #5211, #4725, #66994, #57907, #57402, #96458, #97920 ),
 .UNSPECIFIED., .F., .F.,
 ( 4, 2, 2, 2, 2, 2, 2, 2, 2, 2, 2, 2, 2, 2, 2, 2, 2, 2, 2, 2, 2, 4 ),
 ( 0.002595982006264980872, 0.003006620947792503981, 0.003211940418556245153, 0.003314600153938147831, 0.003417259889320051376, 0.003622579360083736169, 0.003827898830847421829, 0.004238537772374822640, 0.005059815655429624262, 0.005881093538484426751, 0.006702371421539228373, 0.007523649304594030862, 0.007626309039975908387, 0.007677638907666772990, 0.007728968775357637593, 0.007780298643048502195, 0.007831628510739365931, 0.007934288246121141974, 0.008139607716884652427, 0.008344927187648159411, 0.008755566129175173379, 0.009166205070702187346 ),
 .UNSPECIFIED. ) ;
#37097 = CARTESIAN_POINT ( 'NONE',  ( 78.08015083193882333, 52.07315780664882254, -16.04342292210628784 ) ) ;
#37098 = CARTESIAN_POINT ( 'NONE',  ( 190.8907028847385448, 300.0145992415348815, -5.421341690443150618 ) ) ;
#37099 = CARTESIAN_POINT ( 'NONE',  ( 188.6208318395044614, 298.5876672984960010, -4.287592830512637398 ) ) ;
#37100 = CARTESIAN_POINT ( 'NONE',  ( 153.1164404339926080, 265.4415410246681972, 16.15325778160653414 ) ) ;
#37101 = CARTESIAN_POINT ( 'NONE',  ( 146.7529223504909908, 276.4634776601763519, 0.7434588459654100090 ) ) ;
#37102 = CARTESIAN_POINT ( 'NONE',  ( 191.0933613939813540, 299.6635844069401173, -8.689828987424775164 ) ) ;
#37103 = CARTESIAN_POINT ( 'NONE',  ( 66.10228174255657052, 68.64626758096548542, 4.271897712742705799 ) ) ;
#37104 = CARTESIAN_POINT ( 'NONE',  ( 45.57373283677818421, 114.7827874512443032, -10.00000000000000000 ) ) ;
#37106 = CARTESIAN_POINT ( 'NONE',  ( -19.55550329252533004, 92.96216793405713474, 59.99999999999999289 ) ) ;
#37105 = CARTESIAN_POINT ( 'NONE',  ( 149.2765980486851731, 272.0923431290771646, -11.40617906909507973 ) ) ;
#37107 = CARTESIAN_POINT ( 'NONE',  ( 72.84093999290328725, 56.97456911652175648, -16.40692799624908815 ) ) ;
#37108 = FACE_OUTER_BOUND ( 'NONE', #9553, .T. ) ;
#37109 = LINE ( 'NONE', #41849, #31726 ) ;
#37110 = CARTESIAN_POINT ( 'NONE',  ( 103.7198194655286017, 224.5643266524159856, -9.188101187500093303 ) ) ;
#37111 = ORIENTED_EDGE ( 'NONE', *, *, #97554, .F. ) ;
#37112 = CARTESIAN_POINT ( 'NONE',  ( 149.6870021971257643, 271.3815022923409401, -11.82311727174023552 ) ) ;
#37113 = DIRECTION ( 'NONE',  ( -0.8660254037844359321, -0.5000000000000051070, -0.000000000000000000 ) ) ;
#37114 = CARTESIAN_POINT ( 'NONE',  ( 149.3865244398207892, 273.6028616444142472, 10.34018256803319069 ) ) ;
#37115 = CARTESIAN_POINT ( 'NONE',  ( 79.62260391557677508, 45.88305127798363259, 12.92706424833072631 ) ) ;
#37116 = CARTESIAN_POINT ( 'NONE',  ( 183.0283589768903028, 284.4709846154196953, -14.99738598492708341 ) ) ;
#37117 = CARTESIAN_POINT ( 'NONE',  ( 147.9781162831602899, 274.3413795196678961, -10.04506445315961294 ) ) ;
#37118 = ORIENTED_EDGE ( 'NONE', *, *, #91055, .T. ) ;
#37119 = CARTESIAN_POINT ( 'NONE',  ( 167.3377213335115812, 253.1226028751397621, -12.07944002830884678 ) ) ;
#37120 = CARTESIAN_POINT ( 'NONE',  ( 205.7188332128827994, 273.9225886963720882, 10.29739696992246856 ) ) ;
#37121 = CARTESIAN_POINT ( 'NONE',  ( 72.46567298678348834, 71.74231227323613780, 5.836615459846361098 ) ) ;
#37122 = CARTESIAN_POINT ( 'NONE',  ( 47.05812965368407674, 184.6427522451417360, 1.119607411625061291E-15 ) ) ;
#37123 = CARTESIAN_POINT ( 'NONE',  ( 110.8370318831756975, 243.9869531367911009, 4.594050593750046652 ) ) ;
#37124 = DIRECTION ( 'NONE',  ( -1.000000000000000000, 0.000000000000000000, 0.000000000000000000 ) ) ;
#37125 = AXIS2_PLACEMENT_3D ( 'NONE', #55960, #95554, #79340 ) ;
#37126 = CARTESIAN_POINT ( 'NONE',  ( 88.02796755599807454, 43.59779901362369259, -1.172627947537940913E-07 ) ) ;
#37127 = CARTESIAN_POINT ( 'NONE',  ( 195.6986305151803549, 291.6870243064952888, 16.84182339398051909 ) ) ;
#37128 = CARTESIAN_POINT ( 'NONE',  ( 175.6656071552219487, 253.2019425609971393, -4.750314916192522219 ) ) ;
#37129 = CARTESIAN_POINT ( 'NONE',  ( 36.00728465925030974, 191.5958772461660544, -9.188101187500095079 ) ) ;
#37130 = CARTESIAN_POINT ( 'NONE',  ( 75.84856439504059722, 51.76521084193598909, 15.76359423700355755 ) ) ;
#37131 = VECTOR ( 'NONE', #11147, 1000.000000000000000 ) ;
#37132 = ORIENTED_EDGE ( 'NONE', *, *, #15275, .T. ) ;
#37133 = CARTESIAN_POINT ( 'NONE',  ( 72.80948310655894318, 68.89414242203731931, 9.865878564760034664 ) ) ;
#37134 = CARTESIAN_POINT ( 'NONE',  ( 181.4829458551834591, 267.5981693230167480, 14.92975384738928213 ) ) ;
#37135 = ADVANCED_FACE ( 'NONE', ( #22087 ), #85434, .F. ) ;
#37136 = FACE_OUTER_BOUND ( 'NONE', #85985, .T. ) ;
#37137 = CARTESIAN_POINT ( 'NONE',  ( 146.8201187048455267, 276.3470901603510015, 4.112223577763169047 ) ) ;
#37138 = LINE ( 'NONE', #91378, #48243 ) ;
#37139 = DIRECTION ( 'NONE',  ( -0.8660254037844387076, -0.4999999999999998890, -0.000000000000000000 ) ) ;
#37140 = EDGE_CURVE ( 'NONE', #55652, #19593, #38308, .T. ) ;
#37141 = CIRCLE ( 'NONE', #41995, 0.1418229129680863287 ) ;
#37142 =( BOUNDED_CURVE ( )  B_SPLINE_CURVE ( 2, ( #51442, #3859, #88518, #26657, #50445, #89510, #34253, #34743, #74284 ),
 .UNSPECIFIED., .F., .T. ) 
 B_SPLINE_CURVE_WITH_KNOTS ( ( 3, 2, 2, 2, 3 ),
 ( 0.05241935483870967943, 0.05376344086021505458, 0.05645161290322580488, 0.05913978494623656212, 0.06048387096774193727 ),
 .UNSPECIFIED. ) 
 CURVE ( )  GEOMETRIC_REPRESENTATION_ITEM ( )  RATIONAL_B_SPLINE_CURVE ( ( 0.9330127018922194093, 0.9330127018922194093, 1.000000000000000000, 0.8660254037844387076, 1.000000000000000000, 0.8660254037844387076, 1.000000000000000000, 0.9330127018922194093, 0.9330127018922194093 ) ) 
 REPRESENTATION_ITEM ( '' )  );
#37143 = CARTESIAN_POINT ( 'NONE',  ( 176.4843944339568793, 285.6110925004390992, -12.05111447379141154 ) ) ;
#37144 = DIRECTION ( 'NONE',  ( 0.000000000000000000, 0.000000000000000000, 1.000000000000000000 ) ) ;
#37145 = CARTESIAN_POINT ( 'NONE',  ( 107.6799079185947221, 239.6427522451419065, 10.00000000000009237 ) ) ;
#37146 = EDGE_CURVE ( 'NONE', #14672, #14901, #20215, .T. ) ;
#37147 = EDGE_LOOP ( 'NONE', ( #58527, #33213, #72176, #55276, #14567, #10459 ) ) ;
#37148 = CARTESIAN_POINT ( 'NONE',  ( 198.7985463335893996, 267.7170212918624088, -8.201462806822382490 ) ) ;
#37149 = ADVANCED_FACE ( 'NONE', ( #41774, #47863 ), #56969, .F. ) ;
#37150 = CARTESIAN_POINT ( 'NONE',  ( 155.8667045217748637, 279.9326319796254552, -1.585803574218712875 ) ) ;
#37151 = CARTESIAN_POINT ( 'NONE',  ( 208.3764315856425640, 269.7284287242038658, -1.833640725398759441 ) ) ;
#37152 = VECTOR ( 'NONE', #38554, 1000.000000000000000 ) ;
#37153 = CARTESIAN_POINT ( 'NONE',  ( 6.183361268541195166, 180.5024278399160949, 9.188101187500095079 ) ) ;
#37154 = CARTESIAN_POINT ( 'NONE',  ( 13.24385365016830107, 12.81029122506292772, 8.090169943749479842 ) ) ;
#37155 = CARTESIAN_POINT ( 'NONE',  ( 192.1472537951952972, 272.2648030127336369, 14.59637687883535229 ) ) ;
#37156 = CARTESIAN_POINT ( 'NONE',  ( 192.4663556654298588, 297.2854885702906245, -12.98646995774174684 ) ) ;
#37157 = LINE ( 'NONE', #83299, #62041 ) ;
#37159 = CARTESIAN_POINT ( 'NONE',  ( 55.54680928425421627, 209.0024278399160949, 9.188101187500095079 ) ) ;
#37158 = CARTESIAN_POINT ( 'NONE',  ( 198.2327445038538087, 277.3384089221707427, -15.34475411346854834 ) ) ;
#37160 = CARTESIAN_POINT ( 'NONE',  ( 164.1146561143383167, 246.3920726737087534, -7.362905700427413436 ) ) ;
#37161 = CARTESIAN_POINT ( 'NONE',  ( 73.13293788966299758, 57.38693783170513996, 15.88898962805959947 ) ) ;
#37162 = CARTESIAN_POINT ( 'NONE',  ( -29.92656730811346222, 96.39204771392240900, 44.61692575031640473 ) ) ;
#37163 = CARTESIAN_POINT ( 'NONE',  ( 66.31927393682876470, 68.07635084991424890, -4.657035190530372404 ) ) ;
#37164 =( BOUNDED_CURVE ( )  B_SPLINE_CURVE ( 2, ( #18186, #10085, #63273, #40948, #24769, #34373, #3008, #71895, #25793, #94215, #11592, #49567, #25270 ),
 .UNSPECIFIED., .F., .T. ) 
 B_SPLINE_CURVE_WITH_KNOTS ( ( 3, 2, 2, 2, 2, 2, 3 ),
 ( 0.7125000000000000222, 0.7149999999999999689, 0.7199999999999999734, 0.7249999999999999778, 0.7299999999999999822, 0.7349999999999999867, 0.7375000000000000444 ),
 .UNSPECIFIED. ) 
 CURVE ( )  GEOMETRIC_REPRESENTATION_ITEM ( )  RATIONAL_B_SPLINE_CURVE ( ( 0.9755282581475767101, 0.9755282581475772652, 1.000000000000000000, 0.9510565162951535312, 1.000000000000000000, 0.9510565162951535312, 1.000000000000000000, 0.9510565162951535312, 1.000000000000000000, 0.9510565162951535312, 1.000000000000000000, 0.9755282581475761550, 0.9755282581475767101 ) ) 
 REPRESENTATION_ITEM ( '' )  );
#37165 = EDGE_LOOP ( 'NONE', ( #61586, #96612, #2614, #90050 ) ) ;
#37166 = CARTESIAN_POINT ( 'NONE',  ( 19.94070920123175839, 168.9865022471901455, 1.119607411625061291E-15 ) ) ;
#37167 = CARTESIAN_POINT ( 'NONE',  ( 207.6590484093196096, 270.9709728340903894, 3.402057849327809524 ) ) ;
#37168 = CARTESIAN_POINT ( 'NONE',  ( 131.9464011004214115, 256.1744531367911009, 4.594050593750047540 ) ) ;
#37169 = CARTESIAN_POINT ( 'NONE',  ( 22.71615395846560759, 25.06628583063842086, -9.188101187500006262 ) ) ;
#37170 = DIRECTION ( 'NONE',  ( 0.8035972437015812542, 0.5951734788405995680, 0.000000000000000000 ) ) ;
#37171 = CARTESIAN_POINT ( 'NONE',  ( 83.61062943468348863, 51.62670160475642689, -14.84472182808584328 ) ) ;
#37172 = CARTESIAN_POINT ( 'NONE',  ( 72.31720393073018727, 205.8927522451418213, 10.00000000000009948 ) ) ;
#37174 = CARTESIAN_POINT ( 'NONE',  ( 189.5357902666890482, 289.6679798450429075, 15.45925615865311009 ) ) ;
#37173 = CARTESIAN_POINT ( 'NONE',  ( 71.22741938756782076, 71.63657105851643792, 4.191086611024891440 ) ) ;
#37175 = CARTESIAN_POINT ( 'NONE',  ( 68.92286145178795209, 64.34567850579628612, 12.51761414217151014 ) ) ;
#37176 = ORIENTED_EDGE ( 'NONE', *, *, #15710, .F. ) ;
#37177 = CARTESIAN_POINT ( 'NONE',  ( -75.69529296620470404, 50.68926341652933587, 10.00000000000000000 ) ) ;
#37178 = SHAPE_REPRESENTATION_RELATIONSHIP ( 'NONE' , 'NONE' ,  #78010, #484 ) ;
#37179 = DIRECTION ( 'NONE',  ( -0.6835488936653838499, -0.7299047266382303611, 0.000000000000000000 ) ) ;
#37180 = CARTESIAN_POINT ( 'NONE',  ( 169.5394568650638121, 265.9945832123831906, -17.16958432082164876 ) ) ;
#37181 = CARTESIAN_POINT ( 'NONE',  ( 5.120201826081539842, 21.14336893147752861, 7.433330006724141015 ) ) ;
#37182 = VERTEX_POINT ( 'NONE', #70679 ) ;
#37183 = DIRECTION ( 'NONE',  ( 0.000000000000000000, 0.3470917258701589625, 0.9378311862123557274 ) ) ;
#37184 = CARTESIAN_POINT ( 'NONE',  ( 172.6012549852709412, 290.2025030293380610, -5.021894074213228087 ) ) ;
#37185 = CARTESIAN_POINT ( 'NONE',  ( 75.46326934582160106, 53.27636971386139209, 16.49311846759427524 ) ) ;
#37186 = CARTESIAN_POINT ( 'NONE',  ( 148.7640267652926411, 273.4591307251904482, -8.961959150306132216 ) ) ;
#37187 = CARTESIAN_POINT ( 'NONE',  ( 32.15758756610207314, 177.8262482093457777, 3.021315404115420679E-15 ) ) ;
#37188 = CARTESIAN_POINT ( 'NONE',  ( 149.8622666665893632, 273.0779353264732663, 11.47145096717591528 ) ) ;
#37189 = CARTESIAN_POINT ( 'NONE',  ( 67.28342065528214277, 68.44788263265014905, 5.200797640023791857 ) ) ;
#37190 = CARTESIAN_POINT ( 'NONE',  ( 153.4495116231415750, 264.8646448025247082, -16.73555355292144498 ) ) ;
#37191 = CARTESIAN_POINT ( 'NONE',  ( 155.8152618860606253, 260.7670451491295012, 0.000000000000000000 ) ) ;
#37192 = CARTESIAN_POINT ( 'NONE',  ( 7.599693759758306300, 26.16126292948893806, -6.180339887498951690 ) ) ;
#37193 = DIRECTION ( 'NONE',  ( 0.000000000000000000, 0.000000000000000000, 1.000000000000000000 ) ) ;
#37194 = VERTEX_POINT ( 'NONE', #25593 ) ;
#37195 = CARTESIAN_POINT ( 'NONE',  ( 190.8138402884741254, 300.1477291634665789, 4.037153726988762514 ) ) ;
#37196 = CARTESIAN_POINT ( 'NONE',  ( 86.32721218574307898, 47.55264674982593931, -11.12316258729871699 ) ) ;
#37197 = CARTESIAN_POINT ( 'NONE',  ( 189.0975612648258846, 297.0756752416021982, 8.129472812105014157 ) ) ;
#37198 = VERTEX_POINT ( 'NONE', #31664 ) ;
#37199 = VECTOR ( 'NONE', #47193, 1000.000000000000227 ) ;
#37200 = CARTESIAN_POINT ( 'NONE',  ( 191.8456210280128005, 298.3606325003146367, -9.135603544929113085 ) ) ;
#37201 = CARTESIAN_POINT ( 'NONE',  ( 79.04869528564927350, 60.22382082520471158, -16.44980649040591913 ) ) ;
#37202 = CARTESIAN_POINT ( 'NONE',  ( 163.9587364689194260, 246.6621334214722481, 5.816126667419880825 ) ) ;
#37203 = EDGE_CURVE ( 'NONE', #75103, #88081, #79810, .T. ) ;
#37204 = CARTESIAN_POINT ( 'NONE',  ( 69.34550779939547738, 62.84827203527775197, 13.68706312608789410 ) ) ;
#37205 = ORIENTED_EDGE ( 'NONE', *, *, #81541, .T. ) ;
#37206 = CARTESIAN_POINT ( 'NONE',  ( 99.63334886536203783, 219.1423013555409796, -4.594050593750043987 ) ) ;
#37207 = CARTESIAN_POINT ( 'NONE',  ( 199.6663384057308690, 283.4776756693757420, 17.08414512188284817 ) ) ;
#37208 = CARTESIAN_POINT ( 'NONE',  ( 178.0354895240675717, 269.1313736818431721, -16.48722257503622757 ) ) ;
#37209 = CARTESIAN_POINT ( 'NONE',  ( 81.47434785457708983, 42.60586634565555642, -7.670369333657699684 ) ) ;
#37210 = ORIENTED_EDGE ( 'NONE', *, *, #82047, .T. ) ;
#37211 = EDGE_LOOP ( 'NONE', ( #82648, #51281, #28106, #78224 ) ) ;
#37212 = ORIENTED_EDGE ( 'NONE', *, *, #24989, .T. ) ;
#37213 = CARTESIAN_POINT ( 'NONE',  ( 81.48310626213188357, 50.36142246172222769, 14.37505545833610654 ) ) ;
#37215 = EDGE_CURVE ( 'NONE', #76961, #46907, #41265, .T. ) ;
#37214 = EDGE_LOOP ( 'NONE', ( #51649, #61984, #40811, #30154 ) ) ;
#37216 = CARTESIAN_POINT ( 'NONE',  ( 68.92177428303565989, 69.37112163852187052, 5.346089011964235027 ) ) ;
#37217 = VECTOR ( 'NONE', #75791, 1000.000000000000227 ) ;
#37218 = ORIENTED_EDGE ( 'NONE', *, *, #36321, .F. ) ;
#37219 = CARTESIAN_POINT ( 'NONE',  ( 207.6172352878830907, 271.0433952848413810, 3.316653249540578496 ) ) ;
#37220 = CARTESIAN_POINT ( 'NONE',  ( 82.41510281465942001, 41.30975657737747753, 3.334936686815145546 ) ) ;
#37222 = EDGE_CURVE ( 'NONE', #44273, #80416, #65555, .T. ) ;
#37221 = LINE ( 'NONE', #59004, #10704 ) ;
#37223 = CARTESIAN_POINT ( 'NONE',  ( 12.14648056717172686, 184.4865022471903160, -10.00000000000009592 ) ) ;
#37224 = CARTESIAN_POINT ( 'NONE',  ( 70.54788803024760568, 68.42927960339889637, -8.732180548009763399 ) ) ;
#37225 = CARTESIAN_POINT ( 'NONE',  ( 165.0834163913522445, 264.4347080444321136, -17.19626994086416261 ) ) ;
#37226 = ORIENTED_EDGE ( 'NONE', *, *, #33570, .F. ) ;
#37227 = CARTESIAN_POINT ( 'NONE',  ( 175.3932935011599170, 269.2958584618301643, -17.65833184418574930 ) ) ;
#37228 = CARTESIAN_POINT ( 'NONE',  ( 16.32921660555538423, 21.37878583063840310, 9.188101187500006262 ) ) ;
#37229 = ORIENTED_EDGE ( 'NONE', *, *, #80178, .T. ) ;
#37230 = LINE ( 'NONE', #74280, #42914 ) ;
#37231 = CARTESIAN_POINT ( 'NONE',  ( 80.28041774221068749, 57.81736701477464635, 16.60186235868146909 ) ) ;
#37233 = ORIENTED_EDGE ( 'NONE', *, *, #53520, .T. ) ;
#37232 = CARTESIAN_POINT ( 'NONE',  ( 200.0873701903009021, 269.9495076100124038, 10.38151539442265836 ) ) ;
#37234 = CARTESIAN_POINT ( 'NONE',  ( 162.9148248802443106, 248.4702413316674381, 9.709394404200100581 ) ) ;
#37235 = CARTESIAN_POINT ( 'NONE',  ( 187.7932394204981676, 260.5612834524825416, 2.855965374582485783 ) ) ;
#37236 = CARTESIAN_POINT ( 'NONE',  ( 161.2744700912414828, 281.3972689067473993, -6.583020311435618943 ) ) ;
#37237 = CARTESIAN_POINT ( 'NONE',  ( 77.13638489036750912, 49.40795610031250362, -15.43467937247702793 ) ) ;
#37238 = DIRECTION ( 'NONE',  ( 0.5000000000000001110, -0.8660254037844384856, -0.000000000000000000 ) ) ;
#37239 = CARTESIAN_POINT ( 'NONE',  ( 168.5965412549398366, 253.6680249988097557, 11.50723466791552418 ) ) ;
#37240 = LINE ( 'NONE', #67644, #6208 ) ;
#37241 = ORIENTED_EDGE ( 'NONE', *, *, #87263, .F. ) ;
#37242 = CARTESIAN_POINT ( 'NONE',  ( 181.6615078939564398, 271.3508032046874519, -15.97858828533330744 ) ) ;
#37243 = CARTESIAN_POINT ( 'NONE',  ( 69.30281931169795939, 63.72880281195976693, -12.52001448712189635 ) ) ;
#37244 = CARTESIAN_POINT ( 'NONE',  ( 194.0351660592638439, 293.9963875260016266, -14.11356425598665432 ) ) ;
#37245 = CARTESIAN_POINT ( 'NONE',  ( -0.5010987708114443828, 180.5177522451419350, 5.000000000000046185 ) ) ;
#37246 = CARTESIAN_POINT ( 'NONE',  ( 192.9670459817621975, 266.8960202017726147, -11.36568172326798276 ) ) ;
#37247 = PLANE ( 'NONE',  #63251 ) ;
#37248 = CARTESIAN_POINT ( 'NONE',  ( 163.3597984219556167, 247.6995245493996833, -8.443090267489184342 ) ) ;
#37249 = CARTESIAN_POINT ( 'NONE',  ( 86.69791442786498692, 44.65922259563325269, -6.119518264180448419 ) ) ;
#37250 = CARTESIAN_POINT ( 'NONE',  ( 160.7871907424899689, 272.7125984083364187, 15.60852731400909299 ) ) ;
#37252 = CARTESIAN_POINT ( 'NONE',  ( 76.16027975956328078, 65.34306562879338287, 14.46508190410747119 ) ) ;
#37251 = CARTESIAN_POINT ( 'NONE',  ( -3.911334118262431936, 177.7369531367911293, -4.594050593750048428 ) ) ;
#37253 = CARTESIAN_POINT ( 'NONE',  ( 189.1195168369542330, 296.9633965794964752, 8.417122978416381684 ) ) ;
#37254 = VERTEX_POINT ( 'NONE', #93522 ) ;
#37255 = ORIENTED_EDGE ( 'NONE', *, *, #69608, .T. ) ;
#37256 = CYLINDRICAL_SURFACE ( 'NONE', #71151, 70.00000000000002842 ) ;
#37257 = CARTESIAN_POINT ( 'NONE',  ( -34.73454462704830803, 165.1868197944959036, 8.171888229646977204E-14 ) ) ;
#37258 = EDGE_CURVE ( 'NONE', #15783, #2857, #16972, .T. ) ;
#37259 = CARTESIAN_POINT ( 'NONE',  ( 171.8934052655434073, 290.0727470064276190, 2.730291690633440016 ) ) ;
#37260 = CARTESIAN_POINT ( 'NONE',  ( -31.49356256989596758, 94.88921800892812541, 45.19948692389422717 ) ) ;
#37261 = CARTESIAN_POINT ( 'NONE',  ( 162.4245261485180833, 249.3194636459039941, -11.14613848230852611 ) ) ;
#37262 = DIRECTION ( 'NONE',  ( 0.000000000000000000, 0.000000000000000000, 1.000000000000000000 ) ) ;
#37263 = LINE ( 'NONE', #69654, #41831 ) ;
#37264 = CARTESIAN_POINT ( 'NONE',  ( 22.31343150979137846, 177.5643266524160708, 9.188101187500095079 ) ) ;
#37265 = CARTESIAN_POINT ( 'NONE',  ( 120.1739550416679378, 246.3149278399160949, 9.188101187500093303 ) ) ;
#37266 = CARTESIAN_POINT ( 'NONE',  ( 181.7448665231346467, 294.6636721014451155, -6.562496048646235813 ) ) ;
#37267 = CARTESIAN_POINT ( 'NONE',  ( 65.96731655693133689, 68.98875292917840341, 2.536705629638577264 ) ) ;
#37269 = CARTESIAN_POINT ( 'NONE',  ( 206.6891045971790390, 272.2264157197300847, -7.035468968906900322 ) ) ;
#37268 = VECTOR ( 'NONE', #49518, 1000.000000000000114 ) ;
#37270 = EDGE_CURVE ( 'NONE', #81649, #48297, #74593, .T. ) ;
#37271 = ADVANCED_FACE ( 'NONE', ( #97990 ), #27599, .F. ) ;
#37272 = CYLINDRICAL_SURFACE ( 'NONE', #8091, 70.00000000000002842 ) ;
#37273 = CARTESIAN_POINT ( 'NONE',  ( 60.96635096964421763, 217.5530062829863027, -4.648177544792955347E-16 ) ) ;
#37274 = B_SPLINE_CURVE_WITH_KNOTS ( 'NONE', 3,
 ( #84562, #15101, #31799, #16614 ),
 .UNSPECIFIED., .F., .F.,
 ( 4, 4 ),
 ( 0.03043720490792996627, 0.03951895308350013292 ),
 .UNSPECIFIED. ) ;
#37275 = LINE ( 'NONE', #90026, #46921 ) ;
#37276 = CARTESIAN_POINT ( 'NONE',  ( 184.4054840374143680, 274.4020487136705810, 17.38799575625816374 ) ) ;
#37277 = CARTESIAN_POINT ( 'NONE',  ( 189.9952630391477157, 284.7439679202585694, 16.81314581697001032 ) ) ;
#37278 = CARTESIAN_POINT ( 'NONE',  ( 168.0280942669723458, 278.2301272409342232, 14.33002300203766488 ) ) ;
#37279 = CARTESIAN_POINT ( 'NONE',  ( 192.6706003569902350, 265.2643762149980944, 7.794090319438162773 ) ) ;
#37280 = DIRECTION ( 'NONE',  ( 0.000000000000000000, 0.000000000000000000, 1.000000000000000000 ) ) ;
#37281 = CARTESIAN_POINT ( 'NONE',  ( 76.47316661484272515, 51.61210842333346704, -15.65491330287230376 ) ) ;
#37282 = LINE ( 'NONE', #13510, #19022 ) ;
#37283 = AXIS2_PLACEMENT_3D ( 'NONE', #17708, #26307, #31882 ) ;
#37284 = CARTESIAN_POINT ( 'NONE',  ( 184.7231325909508257, 269.5717479162897803, 15.41860894514769065 ) ) ;
#37285 = CARTESIAN_POINT ( 'NONE',  ( 98.84807947347611901, 234.0024278399160664, -9.188101187500093303 ) ) ;
#37286 = CARTESIAN_POINT ( 'NONE',  ( 5.010160986809694350, 24.93396525600388003, 2.839279412974139660 ) ) ;
#37287 = CARTESIAN_POINT ( 'NONE',  ( 150.7254409736883645, 269.5828735707850683, 14.54962197351449049 ) ) ;
#37288 = LINE ( 'NONE', #13026, #64371 ) ;
#37290 = CARTESIAN_POINT ( 'NONE',  ( 82.10523990517461357, 41.85707133252695655, -5.529865280922476423 ) ) ;
#37289 = CARTESIAN_POINT ( 'NONE',  ( 66.04604627343364598, 68.55213889972618801, 2.102432527703944842 ) ) ;
#37291 = CARTESIAN_POINT ( 'NONE',  ( 201.1561089954156500, 270.4184708626717111, -10.06927476064715066 ) ) ;
#37292 = CARTESIAN_POINT ( 'NONE',  ( 32.06670334149083601, 91.95954910241374591, 59.99999999999999289 ) ) ;
#37293 = CARTESIAN_POINT ( 'NONE',  ( 163.2055398469344993, 284.3816007520933340, -6.092379576987982048 ) ) ;
#37294 = CARTESIAN_POINT ( 'NONE',  ( 193.0065576635309412, 296.3498312632291913, -11.90044991639595295 ) ) ;
#37295 = DIRECTION ( 'NONE',  ( -0.9689225787001356505, 0.2473641778533816060, 0.000000000000000000 ) ) ;
#37296 = ORIENTED_EDGE ( 'NONE', *, *, #68616, .F. ) ;
#37297 = CARTESIAN_POINT ( 'NONE',  ( 22.00287929847174695, 28.10171378149919263, 9.188101187500008038 ) ) ;
#37298 = CARTESIAN_POINT ( 'NONE',  ( 153.2819058590468160, 274.2512448977743134, -12.24885634829186287 ) ) ;
#37299 = CARTESIAN_POINT ( 'NONE',  ( 193.1028332910263998, 296.1830769848763225, -12.04975758233223893 ) ) ;
#37300 = CARTESIAN_POINT ( 'NONE',  ( 196.9431415128477170, 289.5314680279574304, -16.61413060656005669 ) ) ;
#37301 = CARTESIAN_POINT ( 'NONE',  ( 70.36883328969454965, 61.20268388249620273, 14.30258033183015520 ) ) ;
#37302 = CARTESIAN_POINT ( 'NONE',  ( 159.8416255366773839, 253.7931787365127434, 16.77980437810719394 ) ) ;
#37303 = CARTESIAN_POINT ( 'NONE',  ( 73.97068428376778115, 60.66754191651645556, 15.78374986018236292 ) ) ;
#37304 = CARTESIAN_POINT ( 'NONE',  ( 172.6497489972219626, 253.7784896148466771, -8.913986932654800910 ) ) ;
#37305 = CARTESIAN_POINT ( 'NONE',  ( 75.01560251667935120, 53.04709277412393220, -16.49609794243962213 ) ) ;
#37306 = CARTESIAN_POINT ( 'NONE',  ( 127.8330407560429904, 254.6115022471903160, -5.000000000000047962 ) ) ;
#37307 = ORIENTED_EDGE ( 'NONE', *, *, #60113, .F. ) ;
#37308 = CARTESIAN_POINT ( 'NONE',  ( 73.06086572573603632, 69.73927861498383152, 9.650215327041465230 ) ) ;
#37309 = ORIENTED_EDGE ( 'NONE', *, *, #41876, .F. ) ;
#37310 = CARTESIAN_POINT ( 'NONE',  ( 66.30443171339169339, 68.57764064706508123, 4.834780342003228704 ) ) ;
#37311 = B_SPLINE_CURVE_WITH_KNOTS ( 'NONE', 3,
 ( #45229, #6237, #29542, #67534, #90895, #69022, #21445, #98464, #29057, #60414, #76166, #51853, #52331, #91881 ),
 .UNSPECIFIED., .F., .F.,
 ( 4, 2, 2, 2, 2, 2, 4 ),
 ( 0.0007405566181291618581, 0.001026655140925903124, 0.001312753663722644390, 0.001598852186519385439, 0.001884950709316126705, 0.002457147754909603382, 0.003029344800503079409 ),
 .UNSPECIFIED. ) ;
#37312 = CARTESIAN_POINT ( 'NONE',  ( 183.9247570546335737, 291.7700146896927436, -10.70695736048003965 ) ) ;
#37313 = EDGE_LOOP ( 'NONE', ( #35437, #25645, #85730, #64308 ) ) ;
#37314 = CARTESIAN_POINT ( 'NONE',  ( 86.50731970396800818, 47.43598145919347786, -10.90780039058068063 ) ) ;
#37315 = CARTESIAN_POINT ( 'NONE',  ( 206.2281698397254956, 273.4493272160884771, 12.02209638042575612 ) ) ;
#37316 = CARTESIAN_POINT ( 'NONE',  ( 85.04793144752866851, 49.76842598555752772, 13.42690168825988550 ) ) ;
#37317 = CARTESIAN_POINT ( 'NONE',  ( 201.0844796915553161, 282.3584598911111812, -16.59562674965125950 ) ) ;
#37318 = DIRECTION ( 'NONE',  ( -0.8660254037844387076, -0.4999999999999998890, -0.000000000000000000 ) ) ;
#37319 = EDGE_CURVE ( 'NONE', #84261, #42053, #61275, .T. ) ;
#37320 = CARTESIAN_POINT ( 'NONE',  ( 43.36002773778349706, 27.96004757982094446, -5.678558825948275768 ) ) ;
#37321 = CARTESIAN_POINT ( 'NONE',  ( 81.62004238798716926, 55.61031524971931361, -16.33394531952002637 ) ) ;
#37322 = EDGE_CURVE ( 'NONE', #5467, #46146, #72720, .T. ) ;
#37323 = FACE_OUTER_BOUND ( 'NONE', #77447, .T. ) ;
#37324 = CARTESIAN_POINT ( 'NONE',  ( 87.52763816747332726, 45.51472861705721584, 6.966552648612967857 ) ) ;
#37325 = ORIENTED_EDGE ( 'NONE', *, *, #19286, .T. ) ;
#37326 = ORIENTED_EDGE ( 'NONE', *, *, #53502, .T. ) ;
#37327 = CARTESIAN_POINT ( 'NONE',  ( 72.12695820614409570, 72.30325941021428093, -1.374247448237438718 ) ) ;
#37328 = CARTESIAN_POINT ( 'NONE',  ( -13.11024591527734451, 27.99999999999999645, 40.00000000000000000 ) ) ;
#37330 = CARTESIAN_POINT ( 'NONE',  ( 165.9671773636226817, 274.1949923808492713, -15.14753692022039466 ) ) ;
#37329 = DIRECTION ( 'NONE',  ( -0.1266907948509198856, 0.9919422576440839467, 0.000000000000000000 ) ) ;
#37331 = LINE ( 'NONE', #53034, #57837 ) ;
#37332 = CARTESIAN_POINT ( 'NONE',  ( 197.6821651709987577, 273.3821959209279271, -13.39123929363893062 ) ) ;
#37333 = CARTESIAN_POINT ( 'NONE',  ( 75.58192994435955825, 60.58255967155832877, -15.61553270740560961 ) ) ;
#37334 = CARTESIAN_POINT ( 'NONE',  ( 148.1634546024981205, 274.0203641339852538, 9.324875965062235039 ) ) ;
#37336 = EDGE_CURVE ( 'NONE', #39956, #76681, #66579, .T. ) ;
#37335 = CARTESIAN_POINT ( 'NONE',  ( 168.0124741839183855, 287.5020746026971779, -5.006766616574994444 ) ) ;
#37337 = CARTESIAN_POINT ( 'NONE',  ( 165.8108829008523344, 266.0291451123555362, 17.22863011630727925 ) ) ;
#37338 = CARTESIAN_POINT ( 'NONE',  ( 185.3484995286736421, 285.8968933059468895, -15.16821555540626854 ) ) ;
#37339 = CARTESIAN_POINT ( 'NONE',  ( 116.0331843058823296, 246.9869531367911293, 4.594050593750046652 ) ) ;
#37340 = ORIENTED_EDGE ( 'NONE', *, *, #22835, .F. ) ;
#37341 = DIRECTION ( 'NONE',  ( -1.000000000000000000, 0.000000000000000000, 0.000000000000000000 ) ) ;
#37342 = CARTESIAN_POINT ( 'NONE',  ( 40.57792791151964451, 35.37878583063844218, 9.188101187500006262 ) ) ;
#37343 = CARTESIAN_POINT ( 'NONE',  ( 188.7546571689037194, 273.7569421533762011, 15.66845421830230478 ) ) ;
#37344 = ORIENTED_EDGE ( 'NONE', *, *, #47287, .T. ) ;
#37345 = ADVANCED_FACE ( 'NONE', ( #73200 ), #74207, .T. ) ;
#37346 = CARTESIAN_POINT ( 'NONE',  ( 162.9929399913377210, 248.7844230333444102, -9.774158786945124078 ) ) ;
#37347 = CARTESIAN_POINT ( 'NONE',  ( 180.7478016446280549, 294.0847902074218609, -2.561698358318056368 ) ) ;
#37348 = CARTESIAN_POINT ( 'NONE',  ( 147.2612474129807083, 275.5830328251833521, 2.671201371937485636 ) ) ;
#37349 = CARTESIAN_POINT ( 'NONE',  ( 159.7692415128758228, 253.9185515433934768, -16.85856106119654285 ) ) ;
#37350 = CARTESIAN_POINT ( 'NONE',  ( 17.92595094200897776, 22.30066082961421259, -10.00000000000000533 ) ) ;
#37351 = EDGE_CURVE ( 'NONE', #77062, #6177, #3311, .T. ) ;
#37352 = VERTEX_POINT ( 'NONE', #57979 ) ;
#37353 = CARTESIAN_POINT ( 'NONE',  ( 195.4568363890616070, 292.1058240179047516, 16.34518427225309267 ) ) ;
#37354 = VECTOR ( 'NONE', #97899, 1000.000000000000000 ) ;
#37355 = ORIENTED_EDGE ( 'NONE', *, *, #75270, .T. ) ;
#37356 = DIRECTION ( 'NONE',  ( -0.7561390817803280706, 0.6544109481086042290, 0.000000000000000000 ) ) ;
#37357 = ORIENTED_EDGE ( 'NONE', *, *, #19107, .T. ) ;
#37358 = CARTESIAN_POINT ( 'NONE',  ( 164.9103019330012216, 245.0139736909548560, 2.841678961959298810 ) ) ;
#37359 = CARTESIAN_POINT ( 'NONE',  ( 194.9830273982886695, 264.9720653068531533, 4.415740111932965561 ) ) ;
#37360 = CYLINDRICAL_SURFACE ( 'NONE', #18728, 70.00000000000002842 ) ;
#37361 = CARTESIAN_POINT ( 'NONE',  ( 67.57228314452760287, 68.96594721286149365, -4.233564566667188167 ) ) ;
#37363 = DIRECTION ( 'NONE',  ( -0.000000000000000000, -0.000000000000000000, -1.000000000000000000 ) ) ;
#37362 = CARTESIAN_POINT ( 'NONE',  ( 184.3650513960811281, 288.5837029191011993, -14.08819112931042916 ) ) ;
#37364 = CARTESIAN_POINT ( 'NONE',  ( 153.3939648708017387, 264.9608545997728015, -16.49556533540763681 ) ) ;
#37365 = ORIENTED_EDGE ( 'NONE', *, *, #52092, .F. ) ;
#37366 = CARTESIAN_POINT ( 'NONE',  ( 157.1517242151937523, 258.4522244926691883, 18.42395718741238042 ) ) ;
#37367 = DIRECTION ( 'NONE',  ( 0.9909246428798906825, 0.1344185706417126980, 0.000000000000000000 ) ) ;
#37368 = EDGE_CURVE ( 'NONE', #96468, #71854, #58945, .T. ) ;
#37369 = DIRECTION ( 'NONE',  ( 0.000000000000000000, -0.000000000000000000, 1.000000000000000000 ) ) ;
#37370 = CARTESIAN_POINT ( 'NONE',  ( 173.1143141876224263, 251.5640903862351081, -0.2630518927552996100 ) ) ;
#37371 = CARTESIAN_POINT ( 'NONE',  ( 192.3947780338729387, 271.6891214328757087, -14.51840760635450422 ) ) ;
#37372 = CARTESIAN_POINT ( 'NONE',  ( 71.74723311883084875, 72.17470677413867008, 3.272391839458885343 ) ) ;
#37373 = CARTESIAN_POINT ( 'NONE',  ( -19.62009469743497547, 92.92711952563814748, 59.99999999999999289 ) ) ;
#37374 = CARTESIAN_POINT ( 'NONE',  ( 38.49039832772786696, 181.4824982072973683, 3.021315404115420679E-15 ) ) ;
#37375 = EDGE_CURVE ( 'NONE', #5700, #26545, #17463, .T. ) ;
#37376 = CARTESIAN_POINT ( 'NONE',  ( 191.3096096579751304, 282.9911372872209654, -16.77114961036221530 ) ) ;
#37377 = CARTESIAN_POINT ( 'NONE',  ( 82.62542648728522465, 54.14492212412226024, -15.90696914271029883 ) ) ;
#37378 = CARTESIAN_POINT ( 'NONE',  ( 80.33678646758374953, 223.3149278399160949, -9.188101187500095079 ) ) ;
#37379 = DIRECTION ( 'NONE',  ( 0.2588190451025454974, 0.9659258262890615399, 0.000000000000000000 ) ) ;
#37380 = CARTESIAN_POINT ( 'NONE',  ( 77.87494449001893315, 61.77424058857110367, 16.06449337301376090 ) ) ;
#37381 = CARTESIAN_POINT ( 'NONE',  ( 208.3764315856425640, 269.7284287242038658, -1.833640725398759441 ) ) ;
#37382 = EDGE_CURVE ( 'NONE', #73834, #26527, #40631, .T. ) ;
#37383 = CARTESIAN_POINT ( 'NONE',  ( 161.8935665241663457, 250.2391126920490194, -13.69501063978231770 ) ) ;
#37384 = CARTESIAN_POINT ( 'NONE',  ( -22.42236680055709641, 157.8615022471902591, 0.000000000000000000 ) ) ;
#37386 = CARTESIAN_POINT ( 'NONE',  ( -48.36978223816941380, 29.22654356899180428, -10.00000000000000000 ) ) ;
#37385 = CARTESIAN_POINT ( 'NONE',  ( 73.68336374684922419, 69.35704589951700427, -9.943571445751130611 ) ) ;
#37387 = EDGE_CURVE ( 'NONE', #7863, #67877, #42758, .T. ) ;
#37388 = CARTESIAN_POINT ( 'NONE',  ( 120.4921787521148246, 228.8262482093457777, 3.021315404115420679E-15 ) ) ;
#37389 = EDGE_CURVE ( 'NONE', #94453, #13198, #44993, .T. ) ;
#37390 = CARTESIAN_POINT ( 'NONE',  ( 42.07167428219069905, 29.45404122711137163, -8.090169943749478065 ) ) ;
#37391 = CARTESIAN_POINT ( 'NONE',  ( 74.63183655046933040, 58.04581334265427728, -16.40266346922720686 ) ) ;
#37392 = CARTESIAN_POINT ( 'NONE',  ( 82.50768696284946202, 54.20953915494273190, 15.58343736883158037 ) ) ;
#37393 = CARTESIAN_POINT ( 'NONE',  ( 71.99480943628985585, 72.01367526706704325, 2.839808199187065174 ) ) ;
#37394 = CARTESIAN_POINT ( 'NONE',  ( 32.08336737017582152, 180.1423013555409796, -4.594050593750043987 ) ) ;
#37395 = CARTESIAN_POINT ( 'NONE',  ( 41.82599275875796252, 62.29945068332010294, -10.00000000000000000 ) ) ;
#37396 = CARTESIAN_POINT ( 'NONE',  ( 199.4033704071922841, 277.6937026877216681, 15.29448692723246772 ) ) ;
#37397 = CARTESIAN_POINT ( 'NONE',  ( 77.00202394376545101, 51.46254985920837299, -15.55718584050375597 ) ) ;
#37398 = CARTESIAN_POINT ( 'NONE',  ( 71.94004515418134815, 72.62285878051592647, -1.062404765500833070 ) ) ;
#37399 = CARTESIAN_POINT ( 'NONE',  ( 47.96943409690536697, 192.3768266524160140, 9.188101187500096856 ) ) ;
#37400 = CARTESIAN_POINT ( 'NONE',  ( 28.09632999608277615, 19.14754757982091604, -5.678558825948275768 ) ) ;
#37401 = CARTESIAN_POINT ( 'NONE',  ( 170.7779774592389401, 287.5599273070118329, 7.147024354692598891 ) ) ;
#37402 = CARTESIAN_POINT ( 'NONE',  ( 196.9319848161575806, 289.5507919934690335, -17.64330560362266453 ) ) ;
#37403 = CARTESIAN_POINT ( 'NONE',  ( 4.600586583810874153, 20.84336893147753500, -7.433330006724137462 ) ) ;
#37404 = CARTESIAN_POINT ( 'NONE',  ( 64.77737111682259297, 68.52662068827328312, 2.033788753608857291E-15 ) ) ;
#37405 = CARTESIAN_POINT ( 'NONE',  ( 76.65021695619097386, 63.83748121254656382, 14.86493802743865977 ) ) ;
#37406 = LINE ( 'NONE', #92656, #81987 ) ;
#37407 = CARTESIAN_POINT ( 'NONE',  ( 179.4801981787712180, 276.6897665335758347, 16.30276041398731479 ) ) ;
#37408 = CARTESIAN_POINT ( 'NONE',  ( 72.27530749108618124, 60.16728400709956759, 15.12809549573886514 ) ) ;
#37409 = CARTESIAN_POINT ( 'NONE',  ( 153.1524534015446761, 277.1654923934203225, 8.229120888094969999 ) ) ;
#37410 = VECTOR ( 'NONE', #100116, 1000.000000000000000 ) ;
#37411 = CARTESIAN_POINT ( 'NONE',  ( 73.12133584826474930, 57.41764960941905116, -15.88333458976553381 ) ) ;
#37412 = CARTESIAN_POINT ( 'NONE',  ( 88.86189758574322184, 232.1115022471902876, -5.000000000000047962 ) ) ;
#37413 = CARTESIAN_POINT ( 'NONE',  ( 161.2313178023453588, 251.3861611254901618, 13.12937145726518473 ) ) ;
#37414 = CARTESIAN_POINT ( 'NONE',  ( 164.8733870693940844, 270.4814310371710349, -16.86211258855632522 ) ) ;
#37415 = VERTEX_POINT ( 'NONE', #90430 ) ;
#37416 = CARTESIAN_POINT ( 'NONE',  ( 69.24135662524314228, 198.5327760586659451, 1.948934522072303157E-15 ) ) ;
#37417 = ORIENTED_EDGE ( 'NONE', *, *, #68774, .F. ) ;
#37418 = CARTESIAN_POINT ( 'NONE',  ( 166.3291615593880692, 265.1125154004245701, 16.59685441684288421 ) ) ;
#37419 = CARTESIAN_POINT ( 'NONE',  ( 190.9441801652054096, 299.9219738747156043, -4.765040093794296716 ) ) ;
#37420 = LINE ( 'NONE', #76926, #17540 ) ;
#37421 = VERTEX_POINT ( 'NONE', #34190 ) ;
#37422 = CYLINDRICAL_SURFACE ( 'NONE', #45695, 17.82106496071139645 ) ;
#37423 = CARTESIAN_POINT ( 'NONE',  ( 79.15951963630969601, 45.96312243709959944, -13.16404013888753433 ) ) ;
#37424 = CARTESIAN_POINT ( 'NONE',  ( 194.9220242159064185, 293.0321458743159724, -14.92681063007793263 ) ) ;
#37425 = CARTESIAN_POINT ( 'NONE',  ( 72.67905965592419193, 70.26320000030698054, -8.002569769838684621 ) ) ;
#37426 = CARTESIAN_POINT ( 'NONE',  ( 205.0608432903593155, 275.4711961086152883, 13.55071766891341412 ) ) ;
#37427 = ORIENTED_EDGE ( 'NONE', *, *, #49998, .T. ) ;
#37428 = CARTESIAN_POINT ( 'NONE',  ( 18.36860284018464995, 32.64646525600389992, -2.839279412974133887 ) ) ;
#37429 = CARTESIAN_POINT ( 'NONE',  ( 75.11677177402179950, 55.37571795895599536, 16.15001063157648176 ) ) ;
#37430 = CARTESIAN_POINT ( 'NONE',  ( 68.66514842125685902, 69.81561067240546947, -3.556167530028313983 ) ) ;
#37431 = CARTESIAN_POINT ( 'NONE',  ( 75.07659682177997240, 67.19019193167021342, -13.02721601185334244 ) ) ;
#37432 = ORIENTED_EDGE ( 'NONE', *, *, #51816, .F. ) ;
#37433 = CARTESIAN_POINT ( 'NONE',  ( 200.7073644890481319, 268.7613916309068145, -8.767088900587291178 ) ) ;
#37434 = CARTESIAN_POINT ( 'NONE',  ( 159.9894443651313338, 253.5371490153152081, -16.36035038356864391 ) ) ;
#37435 = ORIENTED_EDGE ( 'NONE', *, *, #91802, .F. ) ;
#37436 = ORIENTED_EDGE ( 'NONE', *, *, #45821, .F. ) ;
#37437 = CARTESIAN_POINT ( 'NONE',  ( 78.89069071477848638, 50.23289766025146008, -14.88438564644514805 ) ) ;
#37438 =( BOUNDED_CURVE ( )  B_SPLINE_CURVE ( 2, ( #96432, #26995, #57880, #43159, #49295, #42663, #74100, #10802, #33089 ),
 .UNSPECIFIED., .F., .T. ) 
 B_SPLINE_CURVE_WITH_KNOTS ( ( 3, 2, 2, 2, 3 ),
 ( 0.8346774193548387455, 0.8360215053763441206, 0.8387096774193548709, 0.8413978494623656212, 0.8427419354838709964 ),
 .UNSPECIFIED. ) 
 CURVE ( )  GEOMETRIC_REPRESENTATION_ITEM ( )  RATIONAL_B_SPLINE_CURVE ( ( 0.9330127018922194093, 0.9330127018922194093, 1.000000000000000000, 0.8660254037844387076, 1.000000000000000000, 0.8660254037844387076, 1.000000000000000000, 0.9330127018922194093, 0.9330127018922194093 ) ) 
 REPRESENTATION_ITEM ( '' )  );
#37440 = CARTESIAN_POINT ( 'NONE',  ( 53.62548896571598078, 211.7677522451419350, -5.000000000000047962 ) ) ;
#37439 = CARTESIAN_POINT ( 'NONE',  ( 163.0899802648238790, 283.6324727866974627, -3.105502518930082001 ) ) ;
#37441 = CARTESIAN_POINT ( 'NONE',  ( 208.3863431123642727, 269.7112614563416173, -1.693909372230378851 ) ) ;
#37442 = CARTESIAN_POINT ( 'NONE',  ( 204.1953342137782954, 276.9703018036655067, 13.84727111424505885 ) ) ;
#37443 = CARTESIAN_POINT ( 'NONE',  ( 81.87367770298098435, 58.91494905927235948, -0.4240240480782126453 ) ) ;
#37444 = FACE_OUTER_BOUND ( 'NONE', #22787, .T. ) ;
#37446 = ADVANCED_FACE ( 'NONE', ( #96032 ), #21002, .F. ) ;
#37445 = CARTESIAN_POINT ( 'NONE',  ( 130.8910194135003735, 252.5024278399161233, 9.188101187500095079 ) ) ;
#37447 = CARTESIAN_POINT ( 'NONE',  ( 176.9454523999648359, 269.2643027758560947, 16.09744801016948657 ) ) ;
#37448 = CARTESIAN_POINT ( 'NONE',  ( 180.1735081377211429, 258.0673375898933841, 10.29486082622765686 ) ) ;
#37449 = CARTESIAN_POINT ( 'NONE',  ( 68.48323730116675279, 210.3458772461660544, 9.188101187500095079 ) ) ;
#37450 = ORIENTED_EDGE ( 'NONE', *, *, #19591, .F. ) ;
#37451 = CARTESIAN_POINT ( 'NONE',  ( 173.3416224425137671, 264.9983184062012356, 17.00855018129403007 ) ) ;
#37452 = CARTESIAN_POINT ( 'NONE',  ( 79.15982281496793860, 45.83852568395352023, 13.08051851333009807 ) ) ;
#37453 = ORIENTED_EDGE ( 'NONE', *, *, #32642, .F. ) ;
#37454 = CARTESIAN_POINT ( 'NONE',  ( 160.6598419692975028, 254.0198957426222819, 15.58710629308137108 ) ) ;
#37455 = VERTEX_POINT ( 'NONE', #82824 ) ;
#37456 = ORIENTED_EDGE ( 'NONE', *, *, #6965, .T. ) ;
#37457 = FACE_BOUND ( 'NONE', #99669, .T. ) ;
#37458 = CARTESIAN_POINT ( 'NONE',  ( 79.97565766777488250, 44.45602524408276679, -10.96263857390526120 ) ) ;
#37459 = CARTESIAN_POINT ( 'NONE',  ( 197.9023869102375386, 286.9431481333238594, 16.93429523346308230 ) ) ;
#37460 = ADVANCED_FACE ( 'NONE', ( #35173 ), #73690, .T. ) ;
#37462 = B_SPLINE_SURFACE_WITH_KNOTS ( 'NONE', 3, 1, ( 
 ( #18876, #17876 ),
 ( #32563, #72077 ),
 ( #40138, #8759 ),
 ( #87344, #34077 ),
 ( #57347, #95422 ),
 ( #62954, #47740 ),
 ( #95912, #93905 ),
 ( #48773, #2175 ),
 ( #79706, #41138 ),
 ( #86821, #10269 ),
 ( #3194, #33568 ),
 ( #9267, #39631 ),
 ( #64968, #25978 ),
 ( #9781, #56848 ),
 ( #71078, #49268 ),
 ( #26471, #55340 ),
 ( #80204, #40643 ),
 ( #32042, #78676 ),
 ( #33057, #10772 ),
 ( #88322, #70552 ),
 ( #1168, #86316 ),
 ( #16852, #60693 ),
 ( #73565, #45006 ),
 ( #91651, #11773 ),
 ( #75952, #4658 ),
 ( #4148, #21720 ),
 ( #73078, #42146 ),
 ( #52604, #6528 ),
 ( #36913, #65949 ),
 ( #61207, #76437 ),
 ( #96397, #98748 ),
 ( #67826, #7012 ),
 ( #53115, #35044 ),
 ( #30320, #42636 ) ),
 .UNSPECIFIED., .T., .F., .F.,
 ( 4, 2, 2, 2, 2, 2, 2, 2, 2, 2, 2, 2, 2, 2, 2, 2, 4 ),
 ( 2, 2 ),
 ( 0.000000000000000000, 0.06250000000000000000, 0.1250000000000000000, 0.1875000000000000000, 0.2500000000000000000, 0.3125000000000000000, 0.3750000000000000000, 0.4375000000000000000, 0.5000000000000000000, 0.5625000000000000000, 0.6250000000000000000, 0.6875000000000000000, 0.7500000000000000000, 0.8125000000000000000, 0.8750000000000000000, 0.9375000000000000000, 1.000000000000000000 ),
 ( 0.000000000000000000, 1.000000000000000000 ),
 .UNSPECIFIED. ) ;
#37461 = DIRECTION ( 'NONE',  ( -0.8660254037844378194, -0.5000000000000013323, -0.000000000000000000 ) ) ;
#37463 = CARTESIAN_POINT ( 'NONE',  ( 81.19855876245502202, 56.17955710756607601, 16.10481241976900080 ) ) ;
#37464 = LINE ( 'NONE', #91716, #25675 ) ;
#37465 = B_SPLINE_CURVE_WITH_KNOTS ( 'NONE', 3,
 ( #38343, #67261, #6956, #36860, #37843, #61143 ),
 .UNSPECIFIED., .F., .F.,
 ( 4, 2, 4 ),
 ( 0.001016068118891022640, 0.001335860979828362455, 0.001655653840765702487 ),
 .UNSPECIFIED. ) ;
#37466 = CARTESIAN_POINT ( 'NONE',  ( 72.25937237857473860, 68.78397272217405600, 9.561999692830665865 ) ) ;
#37467 = ADVANCED_FACE ( 'NONE', ( #75685 ), #63438, .F. ) ;
#37468 = VERTEX_POINT ( 'NONE', #70050 ) ;
#37469 = CARTESIAN_POINT ( 'NONE',  ( -42.23460334637721303, 26.80738527414552408, -10.00000000000000000 ) ) ;
#37470 = ORIENTED_EDGE ( 'NONE', *, *, #67208, .T. ) ;
#37471 = CARTESIAN_POINT ( 'NONE',  ( 163.9330008582468849, 260.6526909249793107, -16.22567386398026912 ) ) ;
#37472 = B_SPLINE_CURVE_WITH_KNOTS ( 'NONE', 3,
 ( #81930, #5885, #20601, #97616 ),
 .UNSPECIFIED., .F., .F.,
 ( 4, 4 ),
 ( 0.04352980446333042791, 0.04887066958154935581 ),
 .UNSPECIFIED. ) ;
#37473 = CARTESIAN_POINT ( 'NONE',  ( 183.8084685968938459, 275.4580680932389782, 16.50770767648384663 ) ) ;
#37474 = CARTESIAN_POINT ( 'NONE',  ( -29.43245964505113932, 94.53574275318644027, 44.53316583206422763 ) ) ;
#37475 = CARTESIAN_POINT ( 'NONE',  ( 195.2026777324871318, 279.1963207232482773, 16.32161989445632955 ) ) ;
#37476 = CARTESIAN_POINT ( 'NONE',  ( 147.4771206202524354, 275.6046823160672830, -0.001107820683494442279 ) ) ;
#37477 = CARTESIAN_POINT ( 'NONE',  ( 140.2550926398021147, 251.7833772461660544, -9.188101187500095079 ) ) ;
#37478 = ORIENTED_EDGE ( 'NONE', *, *, #33849, .F. ) ;
#37479 = CARTESIAN_POINT ( 'NONE',  ( 87.90883736606430432, 44.33697863951398688, 4.769790285073534086 ) ) ;
#37480 = CARTESIAN_POINT ( 'NONE',  ( 70.33155363901632029, 67.77084087856721339, -10.11489276010222582 ) ) ;
#37481 = CARTESIAN_POINT ( 'NONE',  ( 80.09120749856197108, 44.41673742825524585, -10.86461196121644157 ) ) ;
#37482 = B_SPLINE_CURVE_WITH_KNOTS ( 'NONE', 3,
 ( #30748, #7951, #82988, #29746 ),
 .UNSPECIFIED., .F., .F.,
 ( 4, 4 ),
 ( 0.000000000000000000, 0.001018976964696252131 ),
 .UNSPECIFIED. ) ;
#37483 = CARTESIAN_POINT ( 'NONE',  ( 72.98735915780690675, 70.85324004147126686, 8.065790162528031715 ) ) ;
#37484 = VECTOR ( 'NONE', #90579, 1000.000000000000114 ) ;
#37485 = CARTESIAN_POINT ( 'NONE',  ( 68.15993400338558672, 67.42531444003920171, -8.116946311972593975 ) ) ;
#37486 = VERTEX_POINT ( 'NONE', #93911 ) ;
#37487 = CARTESIAN_POINT ( 'NONE',  ( 197.0013005625082769, 266.0438005881301819, 4.442356137326111565 ) ) ;
#37488 = EDGE_CURVE ( 'NONE', #2126, #7348, #55832, .T. ) ;
#37489 = CARTESIAN_POINT ( 'NONE',  ( 148.3780186227511138, 276.4204535841791994, -3.878789836482348985 ) ) ;
#37490 = PLANE ( 'NONE',  #49517 ) ;
#37491 = CARTESIAN_POINT ( 'NONE',  ( 80.20727400250618189, 48.45000011746393653, 13.73562201919597214 ) ) ;
#37492 = CARTESIAN_POINT ( 'NONE',  ( 73.69590563849025955, 69.38244366243233685, -9.922201517543204119 ) ) ;
#37493 = CARTESIAN_POINT ( 'NONE',  ( 198.0709943550380387, 266.0030824084365122, 0.8185462138619468142 ) ) ;
#37494 = EDGE_CURVE ( 'NONE', #54703, #31618, #35258, .T. ) ;
#37495 = ORIENTED_EDGE ( 'NONE', *, *, #38725, .T. ) ;
#37496 = DIRECTION ( 'NONE',  ( -0.000000000000000000, 1.000000000000000000, 0.000000000000000000 ) ) ;
#37497 = EDGE_CURVE ( 'NONE', #36578, #33337, #55345, .T. ) ;
#37498 = CARTESIAN_POINT ( 'NONE',  ( 186.6683070189575346, 282.4457408569519430, 16.24588814843900764 ) ) ;
#37499 = CARTESIAN_POINT ( 'NONE',  ( 207.4826643481121664, 271.2764789897469768, 7.783310782367018454 ) ) ;
#37501 = FACE_BOUND ( 'NONE', #71742, .T. ) ;
#37500 = CARTESIAN_POINT ( 'NONE',  ( 177.8084161337914679, 264.6135516876653355, -15.81979285547498826 ) ) ;
#37502 = EDGE_CURVE ( 'NONE', #76229, #18290, #30403, .T. ) ;
#37503 = EDGE_CURVE ( 'NONE', #51698, #61284, #31550, .T. ) ;
#37504 = CARTESIAN_POINT ( 'NONE',  ( 20.07045957425421534, 33.36126292948895866, 6.180339887498949913 ) ) ;
#37505 = FACE_OUTER_BOUND ( 'NONE', #98565, .T. ) ;
#37506 = CARTESIAN_POINT ( 'NONE',  ( 205.4892939765805693, 274.2382912982014886, 10.85387586160992157 ) ) ;
#37507 = CARTESIAN_POINT ( 'NONE',  ( 38.90713653809340400, 79.99999999999998579, 54.99999999999999289 ) ) ;
#37508 = CARTESIAN_POINT ( 'NONE',  ( 198.3150362131025588, 287.1552767044814800, 18.53472937702030521 ) ) ;
#37509 = CARTESIAN_POINT ( 'NONE',  ( 192.7874605187217014, 292.5376213369709149, 15.36506066506490598 ) ) ;
#37510 = CARTESIAN_POINT ( 'NONE',  ( -14.60124842228533915, 168.5024278399160949, 9.188101187500095079 ) ) ;
#37511 = LINE ( 'NONE', #7619, #75774 ) ;
#37512 = ORIENTED_EDGE ( 'NONE', *, *, #33121, .F. ) ;
#37513 = CARTESIAN_POINT ( 'NONE',  ( 178.4399924362400895, 256.1387041246245531, 8.807422250050599644 ) ) ;
#37514 = CARTESIAN_POINT ( 'NONE',  ( 72.86116454657229724, 70.29466190917024448, -8.120416833897904141 ) ) ;
#37515 = CARTESIAN_POINT ( 'NONE',  ( 151.1230807375396807, 268.8941412966845519, -14.26613110909109849 ) ) ;
#37516 = CARTESIAN_POINT ( 'NONE',  ( 10.97399815293012892, 167.9548013555409796, -4.594050593750042211 ) ) ;
#37517 = AXIS2_PLACEMENT_3D ( 'NONE', #98289, #21281, #89245 ) ;
#37518 = CARTESIAN_POINT ( 'NONE',  ( 178.5166367657841135, 273.6876824058858801, -16.98119149330447897 ) ) ;
#37519 = CARTESIAN_POINT ( 'NONE',  ( 30.23324123896446736, 19.58380873178788306, 6.180339887498953466 ) ) ;
#37520 = CARTESIAN_POINT ( 'NONE',  ( 85.32371827457656366, 48.49939495466653483, 12.43282873216696593 ) ) ;
#37521 = CARTESIAN_POINT ( 'NONE',  ( 170.7677701316179935, 271.1495265934172494, -17.63551025999282373 ) ) ;
#37522 = CARTESIAN_POINT ( 'NONE',  ( 71.71105958810139214, 72.07721142573539908, -3.586786881503329472 ) ) ;
#37523 = DIRECTION ( 'NONE',  ( -0.8660254037844387076, -0.4999999999999998890, -0.000000000000000000 ) ) ;
#37524 = CARTESIAN_POINT ( 'NONE',  ( 176.1144182152248447, 252.4374784436402308, -3.440074553853730066 ) ) ;
#37525 = CARTESIAN_POINT ( 'NONE',  ( 150.7471914551857708, 269.5452006317422047, 15.29409085476701691 ) ) ;
#37526 = CARTESIAN_POINT ( 'NONE',  ( 48.59171630976688760, 198.8615022471902591, -10.00000000000009592 ) ) ;
#37527 = CARTESIAN_POINT ( 'NONE',  ( -22.42236680055709641, 157.8615022471902591, 0.000000000000000000 ) ) ;
#37528 = CARTESIAN_POINT ( 'NONE',  ( 147.6207754342248961, 274.9603120256437592, 8.795690793376332195 ) ) ;
#37529 = VECTOR ( 'NONE', #94397, 1000.000000000000000 ) ;
#37530 = CARTESIAN_POINT ( 'NONE',  ( 17.98295739510416524, 187.3149278399160949, -9.188101187500095079 ) ) ;
#37531 = CARTESIAN_POINT ( 'NONE',  ( 72.77745277708220328, 70.81288354178651900, -7.938184674006802943 ) ) ;
#37532 = ADVANCED_FACE ( 'NONE', ( #86827 ), #48067, .F. ) ;
#37533 = CARTESIAN_POINT ( 'NONE',  ( 192.5049767439991513, 297.2185948999652965, 12.57567268027295881 ) ) ;
#37534 = CARTESIAN_POINT ( 'NONE',  ( 40.90268743793880901, 35.56628583063844218, 9.188101187500006262 ) ) ;
#37535 = CARTESIAN_POINT ( 'NONE',  ( 201.1893450866852504, 280.1768276987904756, -16.82388990131531870 ) ) ;
#37536 = DIRECTION ( 'NONE',  ( 0.4999999999999998890, -0.8660254037844385966, 0.000000000000000000 ) ) ;
#37537 = CARTESIAN_POINT ( 'NONE',  ( 185.3440001858262178, 266.5832585216657549, 13.22870378338188324 ) ) ;
#37538 = B_SPLINE_CURVE_WITH_KNOTS ( 'NONE', 3,
 ( #69321, #16617, #94161, #85580, #55106, #31803, #70313, #9021, #94660, #62704 ),
 .UNSPECIFIED., .F., .F.,
 ( 4, 2, 2, 2, 4 ),
 ( 0.000000000000000000, 0.0002622400424273363395, 0.0005244800848546726790, 0.0007867201272820090185, 0.001048960169709345358 ),
 .UNSPECIFIED. ) ;
#37539 = CARTESIAN_POINT ( 'NONE',  ( 153.5289410443318445, 265.1998938147651188, -16.31391090849110981 ) ) ;
#37540 = DIRECTION ( 'NONE',  ( -1.000000000000000000, 0.000000000000000000, 0.000000000000000000 ) ) ;
#37541 = CARTESIAN_POINT ( 'NONE',  ( 12.16147613323643029, 27.99752408145590721, 5.678558825948277544 ) ) ;
#37542 = CARTESIAN_POINT ( 'NONE',  ( 147.7157269441172218, 274.7958511862549926, 8.036290321896261801 ) ) ;
#37543 = CARTESIAN_POINT ( 'NONE',  ( 71.96630278948212833, 59.14415382642645369, 15.37175206046237008 ) ) ;
#37544 = CARTESIAN_POINT ( 'NONE',  ( 155.4917600441137324, 261.3273667757233056, 17.14261720787171939 ) ) ;
#37545 = ORIENTED_EDGE ( 'NONE', *, *, #3970, .F. ) ;
#37546 = CARTESIAN_POINT ( 'NONE',  ( 181.5361471459265204, 289.3569626564614055, 12.72074604773742834 ) ) ;
#37547 = DIRECTION ( 'NONE',  ( -0.9171038997749370036, 0.3986482622784180418, 0.000000000000000000 ) ) ;
#37548 = CARTESIAN_POINT ( 'NONE',  ( 88.23709331947554801, 44.35306696108359148, 2.575362715384265311 ) ) ;
#37549 = VERTEX_POINT ( 'NONE', #3680 ) ;
#37550 = CARTESIAN_POINT ( 'NONE',  ( 15.68640692011977222, 32.55466486950700045, -1.111400068045478839E-16 ) ) ;
#37551 = CARTESIAN_POINT ( 'NONE',  ( 149.0807665407234026, 276.4376266709116408, -5.539133476438467873 ) ) ;
#37552 = CARTESIAN_POINT ( 'NONE',  ( 72.50785297705053267, 57.43012539693897622, 16.30925143403899824 ) ) ;
#37553 = CARTESIAN_POINT ( 'NONE',  ( 155.6048174803203210, 261.1315455520403361, -17.38645169541727498 ) ) ;
#37554 = VERTEX_POINT ( 'NONE', #57352 ) ;
#37555 = EDGE_LOOP ( 'NONE', ( #26140, #22294, #56408 ) ) ;
#37557 = CARTESIAN_POINT ( 'NONE',  ( 204.9427641582406636, 275.6757151647582305, 14.40446820030680897 ) ) ;
#37556 = FACE_OUTER_BOUND ( 'NONE', #59245, .T. ) ;
#37558 = ORIENTED_EDGE ( 'NONE', *, *, #88112, .F. ) ;
#37559 = CARTESIAN_POINT ( 'NONE',  ( 191.4484954869714954, 299.0484741143815199, 8.684991747358081327 ) ) ;
#37560 = CARTESIAN_POINT ( 'NONE',  ( -44.38014153532155603, 70.85927927110010671, -10.00000000000000000 ) ) ;
#37561 = CARTESIAN_POINT ( 'NONE',  ( 80.36956643484273854, 57.45342863445996784, -16.58888403658913901 ) ) ;
#37562 = DIRECTION ( 'NONE',  ( -0.9662637919863231728, -0.2575544297740022248, 0.000000000000000000 ) ) ;
#37563 = ORIENTED_EDGE ( 'NONE', *, *, #29918, .F. ) ;
#37564 = CYLINDRICAL_SURFACE ( 'NONE', #32917, 17.82106496071139645 ) ;
#37565 = EDGE_CURVE ( 'NONE', #75006, #30838, #82241, .T. ) ;
#37566 = CARTESIAN_POINT ( 'NONE',  ( 196.9431415128477170, 289.5314680279574304, -16.61413060656005669 ) ) ;
#37567 = VERTEX_POINT ( 'NONE', #49763 ) ;
#37568 = CARTESIAN_POINT ( 'NONE',  ( 206.4943150373521803, 272.9883502116088039, 11.34100825923693101 ) ) ;
#37569 = CARTESIAN_POINT ( 'NONE',  ( 74.41414138846958792, 62.82147636634939403, 14.66719177346846159 ) ) ;
#37570 = EDGE_LOOP ( 'NONE', ( #54832, #33728, #95801, #62341 ) ) ;
#37571 = CARTESIAN_POINT ( 'NONE',  ( 190.0445576990143195, 301.4801656937889902, 4.140328216824785912 ) ) ;
#37572 = DIRECTION ( 'NONE',  ( -0.5076330711061851630, 0.8615733660689046669, 0.000000000000000000 ) ) ;
#37573 = VERTEX_POINT ( 'NONE', #50745 ) ;
#37574 = EDGE_CURVE ( 'NONE', #34618, #79381, #2094, .T. ) ;
#37575 = CARTESIAN_POINT ( 'NONE',  ( -11.85091256637315205, 72.02634106223788990, 14.52565316431220133 ) ) ;
#37576 = DIRECTION ( 'NONE',  ( 0.000000000000000000, 0.5906904945688705721, 0.8068982213550747185 ) ) ;
#37577 = CARTESIAN_POINT ( 'NONE',  ( 78.41477381122238910, 47.32040575024743134, -14.22103711499937617 ) ) ;
#37578 = CARTESIAN_POINT ( 'NONE',  ( -38.02969130575858259, 25.52022711230254970, -10.00000000000000000 ) ) ;
#37579 = ORIENTED_EDGE ( 'NONE', *, *, #40345, .T. ) ;
#37580 = EDGE_CURVE ( 'NONE', #32094, #34750, #42948, .T. ) ;
#37581 = ORIENTED_EDGE ( 'NONE', *, *, #90907, .T. ) ;
#37582 = CARTESIAN_POINT ( 'NONE',  ( 73.53833585859590016, 69.81206169144661544, 9.302004287366802515 ) ) ;
#37583 = LINE ( 'NONE', #7189, #26993 ) ;
#37584 = CARTESIAN_POINT ( 'NONE',  ( 190.2510882691990730, 301.1224442529128851, -5.480893437181090455 ) ) ;
#37585 = CARTESIAN_POINT ( 'NONE',  ( 148.4049257185216106, 273.6021238924720365, 8.639190357831699529 ) ) ;
#37586 = CARTESIAN_POINT ( 'NONE',  ( 190.4249800432324662, 300.8212548652687133, 3.085047376053959400 ) ) ;
#37587 = CARTESIAN_POINT ( 'NONE',  ( 157.3797482626287092, 258.5641623508735165, -16.86146766721270396 ) ) ;
#37588 = CARTESIAN_POINT ( 'NONE',  ( 147.1630655063547124, 275.7530888758436163, -0.6147864833414894425 ) ) ;
#37589 = CARTESIAN_POINT ( 'NONE',  ( 191.5521510896938935, 298.8689373439769952, -9.847378829740700112 ) ) ;
#37590 = CARTESIAN_POINT ( 'NONE',  ( 149.0323968763055689, 272.5153119669064949, 11.64231532207353403 ) ) ;
#37591 = LINE ( 'NONE', #70499, #10629 ) ;
#37592 = VECTOR ( 'NONE', #97519, 1000.000000000000000 ) ;
#37594 = DIRECTION ( 'NONE',  ( -0.9999580202055560196, -0.009162850352621043637, 0.000000000000000000 ) ) ;
#37593 = CARTESIAN_POINT ( 'NONE',  ( 196.4783028304046013, 290.3365922432724346, -16.37291435488387492 ) ) ;
#37595 = CARTESIAN_POINT ( 'NONE',  ( 67.13624854745103221, 66.75749375781143158, 8.200433981937235828 ) ) ;
#37596 = CARTESIAN_POINT ( 'NONE',  ( 168.2319217786528327, 286.4071002536015840, 3.836160949525527997 ) ) ;
#37597 = CARTESIAN_POINT ( 'NONE',  ( 78.48434347618606921, 47.42827226539994712, 14.25623586707808066 ) ) ;
#37598 = CARTESIAN_POINT ( 'NONE',  ( 102.5829875751790468, 230.0333772461660828, 9.188101187500095079 ) ) ;
#37599 = ORIENTED_EDGE ( 'NONE', *, *, #72286, .T. ) ;
#37600 = CARTESIAN_POINT ( 'NONE',  ( 190.5599134601667117, 300.5875433314996030, -4.781267067655845082 ) ) ;
#37601 = CARTESIAN_POINT ( 'NONE',  ( 72.18576721375995930, 69.97445003978347700, 7.973227091533599875 ) ) ;
#37602 = CARTESIAN_POINT ( 'NONE',  ( 203.0069541289995243, 278.2920787410731691, 14.98668837248997932 ) ) ;
#37603 = CARTESIAN_POINT ( 'NONE',  ( 87.11349487006070547, 46.19076519147612458, 8.411924245371466213 ) ) ;
#37604 = CARTESIAN_POINT ( 'NONE',  ( 180.3507851124660135, 283.5217650176155075, -16.12320021977993534 ) ) ;
#37605 = CARTESIAN_POINT ( 'NONE',  ( 83.66208585045004043, 52.31085355490836264, -15.11568120807085336 ) ) ;
#37606 = CARTESIAN_POINT ( 'NONE',  ( 169.2884693346459244, 285.2280652319857381, -7.815770310637231155 ) ) ;
#37607 = ORIENTED_EDGE ( 'NONE', *, *, #75240, .F. ) ;
#37608 = CARTESIAN_POINT ( 'NONE',  ( 208.3226489551340990, 269.8215829728092103, -1.240262689467544366 ) ) ;
#37609 = CARTESIAN_POINT ( 'NONE',  ( 206.8791291248445532, 272.3218326606039454, -10.16823074922856840 ) ) ;
#37610 = EDGE_CURVE ( 'NONE', #27243, #57163, #64973, .T. ) ;
#37611 = CARTESIAN_POINT ( 'NONE',  ( 79.14312167556931854, 57.64441083166269664, 0.000000000000000000 ) ) ;
#37612 = CARTESIAN_POINT ( 'NONE',  ( 35.43895548624276159, 201.2677522451419350, -5.000000000000047962 ) ) ;
#37613 = CARTESIAN_POINT ( 'NONE',  ( 108.2389556718223673, 242.4869531367911009, 4.594050593750046652 ) ) ;
#37614 = DIRECTION ( 'NONE',  ( -0.000000000000000000, 0.000000000000000000, 1.000000000000000000 ) ) ;
#37615 = VECTOR ( 'NONE', #26427, 1000.000000000000000 ) ;
#37616 = DIRECTION ( 'NONE',  ( -0.8660254037844387076, -0.4999999999999998890, -0.000000000000000000 ) ) ;
#37617 = CARTESIAN_POINT ( 'NONE',  ( 188.8544700204132880, 297.4231428397746413, 9.261439979758030461 ) ) ;
#37618 = CARTESIAN_POINT ( 'NONE',  ( 175.4498787482802982, 253.5586827773643108, -4.041159264954998775 ) ) ;
#37619 = CARTESIAN_POINT ( 'NONE',  ( 35.46636587765004123, 179.0327760586659736, 1.948934522072303157E-15 ) ) ;
#37620 = CARTESIAN_POINT ( 'NONE',  ( -36.52772323645827868, 26.41323893245353105, -10.00000000000000000 ) ) ;
#37621 = ORIENTED_EDGE ( 'NONE', *, *, #57053, .F. ) ;
#37622 = CARTESIAN_POINT ( 'NONE',  ( 181.2305971022323661, 265.9781236237157032, -15.82518789413146010 ) ) ;
#37623 = CARTESIAN_POINT ( 'NONE',  ( 181.9045674196421203, 266.8808357545214562, 15.69428031596684114 ) ) ;
#37624 = EDGE_CURVE ( 'NONE', #9798, #1235, #12272, .T. ) ;
#37625 = CARTESIAN_POINT ( 'NONE',  ( 16.54877636974260824, 190.3615022471903160, 5.000000000000046185 ) ) ;
#37626 = CARTESIAN_POINT ( 'NONE',  ( -78.94662368502557115, 55.85910816071122298, 177.5919119679930134 ) ) ;
#37627 = CARTESIAN_POINT ( 'NONE',  ( 106.1564052266985101, 220.5494855054051584, -2.679491924311248496 ) ) ;
#37628 = DIRECTION ( 'NONE',  ( 0.5000000000000014433, -0.8660254037844378194, 0.000000000000000000 ) ) ;
#37629 = DIRECTION ( 'NONE',  ( 0.000000000000000000, 0.000000000000000000, 1.000000000000000000 ) ) ;
#37630 = CARTESIAN_POINT ( 'NONE',  ( 106.9582200821076299, 245.8927522451419350, 2.944929066748280225E-16 ) ) ;
#37631 = EDGE_LOOP ( 'NONE', ( #86985, #36362, #95544, #48450 ) ) ;
#37632 = CARTESIAN_POINT ( 'NONE',  ( 207.8570869662935365, 270.6279599915536664, -5.669188455878507504 ) ) ;
#37633 = CARTESIAN_POINT ( 'NONE',  ( 155.4352814124438282, 279.7207056978571131, -1.858304131775387003 ) ) ;
#37634 = CARTESIAN_POINT ( 'NONE',  ( 154.3624839403327371, 263.9877490788467185, 16.80989463870938749 ) ) ;
#37635 = ADVANCED_FACE ( 'NONE', ( #4663 ), #64276, .F. ) ;
#37636 = CARTESIAN_POINT ( 'NONE',  ( 8.781437479894508513, 182.0024278399160949, 9.188101187500095079 ) ) ;
#37637 = CARTESIAN_POINT ( 'NONE',  ( 8.420521286406055239, 20.56454794089038884, 10.00000000000000355 ) ) ;
#37638 = CARTESIAN_POINT ( 'NONE',  ( 192.5718708460708797, 272.1165744649917428, 14.18846852481804888 ) ) ;
#37639 = CARTESIAN_POINT ( 'NONE',  ( 71.71174882295490249, 58.93038559433049528, -15.88944412498251602 ) ) ;
#37640 = CARTESIAN_POINT ( 'NONE',  ( 182.3667867738580242, 280.0318728379381241, 17.49684858827472667 ) ) ;
#37642 = CARTESIAN_POINT ( 'NONE',  ( 58.14488549560751807, 210.5024278399160949, 9.188101187500095079 ) ) ;
#37641 = CARTESIAN_POINT ( 'NONE',  ( 194.7293364455423728, 275.0050812418281225, -15.92559422164948479 ) ) ;
#37643 = CARTESIAN_POINT ( 'NONE',  ( 197.4517085639775189, 281.7586087989938051, 17.62726178258972354 ) ) ;
#37644 = CARTESIAN_POINT ( 'NONE',  ( 72.56871628006966546, 57.25199919244864333, 16.34355953453273003 ) ) ;
#37645 = CARTESIAN_POINT ( 'NONE',  ( 71.34022676192449808, 69.59814005368316714, 8.523861822075398109 ) ) ;
#37646 = CARTESIAN_POINT ( 'NONE',  ( 66.24005707684722211, 68.70828816332591771, -4.328508583860865677 ) ) ;
#37647 = EDGE_LOOP ( 'NONE', ( #16986, #48454 ) ) ;
#37648 = B_SPLINE_CURVE_WITH_KNOTS ( 'NONE', 3,
 ( #3210, #64483, #49285, #63972, #72608, #95443, #79230, #80733, #47758, #64985, #62975, #25995, #49776, #56866, #95929, #55846, #87367, #48794, #9803, #87850, #70570, #1188, #93923, #40663, #79725, #2196, #33079, #94915, #25478, #10287, #41159, #96921, #66468, #97884, #65473, #28457, #26982, #65969, #42165, #21368, #58358, #5662, #13286, #90815, #58840, #36550 ),
 .UNSPECIFIED., .F., .F.,
 ( 4, 2, 2, 2, 2, 2, 2, 2, 2, 2, 2, 2, 2, 2, 2, 2, 2, 2, 2, 2, 2, 2, 4 ),
 ( 0.0003494839938075159236, 0.001366047292800560932, 0.001874328942297083652, 0.002001399354671171398, 0.002128469767045259361, 0.002255540179419347323, 0.002382610591793435720, 0.002636751416541610778, 0.002890892241289786703, 0.003399173890786319832, 0.004415737189779446806, 0.005432300488772573779, 0.005940582138269217063, 0.006194722963017495337, 0.006448863787765774479, 0.006512398993952864430, 0.006575934200139955249, 0.006639469406327046068, 0.006703004612514136019, 0.006957145437262477611, 0.007465427086759236254, 0.007973708736255996632, 0.008481990385752756142 ),
 .UNSPECIFIED. ) ;
#37649 = CARTESIAN_POINT ( 'NONE',  ( 165.4619875320036329, 269.3508363939868673, 17.22119345129141266 ) ) ;
#37650 = CARTESIAN_POINT ( 'NONE',  ( 6.156471524329347744, 184.3615022471903160, 5.000000000000046185 ) ) ;
#37651 = CARTESIAN_POINT ( 'NONE',  ( 164.4405316900629259, 245.8276396196081350, -6.144538123479245328 ) ) ;
#37652 = CARTESIAN_POINT ( 'NONE',  ( 133.0017827873424494, 259.8464784336661637, 1.353441290958777327E-15 ) ) ;
#37653 = CARTESIAN_POINT ( 'NONE',  ( 27.11724708220625857, 33.84336893147757763, -7.433330006724137462 ) ) ;
#37654 = CARTESIAN_POINT ( 'NONE',  ( 206.7978835355532112, 272.4625541491475929, -7.782039308735489769 ) ) ;
#37655 = LINE ( 'NONE', #68565, #93755 ) ;
#37656 = CARTESIAN_POINT ( 'NONE',  ( -10.08900441837308470, 61.23661786014601205, -10.00000000000000000 ) ) ;
#37658 = CARTESIAN_POINT ( 'NONE',  ( 175.7882114856885210, 291.4026636951798537, -6.622811550496607857 ) ) ;
#37657 = CARTESIAN_POINT ( 'NONE',  ( 156.9694903541507074, 266.1758412851487492, -17.34135443527054576 ) ) ;
#37659 = CARTESIAN_POINT ( 'NONE',  ( 68.89365374505190687, 64.32635024170694749, 12.51947484636856345 ) ) ;
#37660 = EDGE_LOOP ( 'NONE', ( #96672, #9930, #90382 ) ) ;
#37661 = CARTESIAN_POINT ( 'NONE',  ( 88.19053702688614749, 44.32527345396092500, -2.493626234014364673 ) ) ;
#37662 = CARTESIAN_POINT ( 'NONE',  ( 164.1353833742626591, 246.3561720064182339, 8.180808313729997394 ) ) ;
#37663 = CARTESIAN_POINT ( 'NONE',  ( 151.6586017097065167, 268.5374266604292757, -14.66497191532962141 ) ) ;
#37664 = AXIS2_PLACEMENT_3D ( 'NONE', #42750, #72714, #3303 ) ;
#37665 = CARTESIAN_POINT ( 'NONE',  ( 156.4703069145093650, 280.4439178849370364, -5.466162413456765456 ) ) ;
#37666 = CARTESIAN_POINT ( 'NONE',  ( 197.2297097385163056, 273.4493452446096171, -13.71841916057935507 ) ) ;
#37667 = ORIENTED_EDGE ( 'NONE', *, *, #9039, .F. ) ;
#37668 = FACE_OUTER_BOUND ( 'NONE', #52513, .T. ) ;
#37669 = DIRECTION ( 'NONE',  ( -0.4635919272833941562, 0.8029647720336182681, 0.3746065934159032440 ) ) ;
#37670 = AXIS2_PLACEMENT_3D ( 'NONE', #25706, #55076, #24687 ) ;
#37671 = B_SPLINE_CURVE_WITH_KNOTS ( 'NONE', 3,
 ( #90825, #13770, #28467, #82727, #29472, #90325, #92310, #74610, #98891, #13299, #51788, #66964, #59348, #44157, #14764, #28986, #45646, #75583 ),
 .UNSPECIFIED., .F., .F.,
 ( 4, 2, 2, 2, 2, 2, 2, 2, 4 ),
 ( 7.954564953275306146E-05, 0.0004482884113075860004, 0.0008170311730824190207, 0.001185773934857251933, 0.001554516696632084844, 0.001923259458406917756, 0.002292002220181750885, 0.002660744981956583797, 0.003029487743731416709 ),
 .UNSPECIFIED. ) ;
#37672 = CARTESIAN_POINT ( 'NONE',  ( 148.7588072053147243, 273.7711778218048835, -8.803803025135483296 ) ) ;
#37673 = CARTESIAN_POINT ( 'NONE',  ( 21.74492879244924382, 193.3615022471903160, 5.000000000000046185 ) ) ;
#37674 = DIRECTION ( 'NONE',  ( -0.8116583814955237175, -0.01378320505841506768, -0.5839697723396174434 ) ) ;
#37675 = CARTESIAN_POINT ( 'NONE',  ( 163.3723087697842971, 247.6778559913402091, -10.08585062664141319 ) ) ;
#37676 = CARTESIAN_POINT ( 'NONE',  ( 152.8721808860877616, 265.8646109718731623, -17.65676496037632504 ) ) ;
#37677 = CARTESIAN_POINT ( 'NONE',  ( 190.4940751089258129, 281.5363301538920950, 17.17439451701960706 ) ) ;
#37678 = CARTESIAN_POINT ( 'NONE',  ( 17.82296297622643166, 15.45404122711132544, -8.090169943749478065 ) ) ;
#37679 = CARTESIAN_POINT ( 'NONE',  ( 73.04277380876573034, 70.56196896876862468, 7.835544939490341143 ) ) ;
#37680 = VERTEX_POINT ( 'NONE', #54 ) ;
#37681 = CYLINDRICAL_SURFACE ( 'NONE', #99783, 17.82106496071139645 ) ;
#37682 = CARTESIAN_POINT ( 'NONE',  ( 86.52979389935374854, 47.15173288509246419, -10.60481917042621802 ) ) ;
#37683 = CARTESIAN_POINT ( 'NONE',  ( 79.27712787825650764, 45.82676469203064329, -12.41914995154098911 ) ) ;
#37684 = EDGE_LOOP ( 'NONE', ( #28302, #13730, #36210, #67331 ) ) ;
#37685 = FACE_OUTER_BOUND ( 'NONE', #97545, .T. ) ;
#37686 = CARTESIAN_POINT ( 'NONE',  ( 79.18418104304700478, 60.10533407485777957, -16.47260471942690074 ) ) ;
#37687 = CIRCLE ( 'NONE', #99649, 17.82106496071138224 ) ;
#37688 = AXIS2_PLACEMENT_3D ( 'NONE', #96160, #80470, #65705 ) ;
#37689 = CARTESIAN_POINT ( 'NONE',  ( 204.9432097630379417, 275.6749433546094679, 13.74700047688257776 ) ) ;
#37690 = CARTESIAN_POINT ( 'NONE',  ( 69.47282375568661905, 62.69533200737101453, 13.81976147870238592 ) ) ;
#37691 = ORIENTED_EDGE ( 'NONE', *, *, #44686, .T. ) ;
#37692 = CARTESIAN_POINT ( 'NONE',  ( 94.51795245455393513, 231.5024278399160949, 9.188101187500095079 ) ) ;
#37693 = CARTESIAN_POINT ( 'NONE',  ( 185.2391986358457530, 295.7873944733689768, 8.585680893828113724 ) ) ;
#37694 = CARTESIAN_POINT ( 'NONE',  ( 181.3482518238504611, 271.2696307585432578, -15.99940275358306607 ) ) ;
#37695 = CARTESIAN_POINT ( 'NONE',  ( 81.38072385067304992, 42.55310844818403382, -7.672405682984796194 ) ) ;
#37696 = B_SPLINE_SURFACE_WITH_KNOTS ( 'NONE', 3, 1, ( 
 ( #94565, #31221 ),
 ( #33228, #25123 ),
 ( #24131, #56525 ),
 ( #87513, #62107 ),
 ( #24623, #93055 ),
 ( #64132, #86999 ),
 ( #85998, #93564 ),
 ( #45054, #23609 ),
 ( #70729, #56004 ),
 ( #78853, #16028 ),
 ( #17527, #8435 ),
 ( #48434, #39303 ),
 ( #70220, #827 ),
 ( #79382, #32225 ),
 ( #31706, #86493 ),
 ( #62611, #55018 ),
 ( #9435, #17020 ),
 ( #40310, #71249 ),
 ( #16525, #39797 ),
 ( #47422, #63128 ),
 ( #78347, #63628 ),
 ( #1843, #9945 ),
 ( #40807, #4218 ),
 ( #51303, #49335 ),
 ( #80786, #73151 ),
 ( #20435, #27542 ),
 ( #35116, #74145 ),
 ( #26045, #89387 ),
 ( #87903, #95980 ),
 ( #26542, #11360 ),
 ( #18446, #80275 ) ),
 .UNSPECIFIED., .F., .F., .F.,
 ( 4, 3, 3, 3, 3, 3, 3, 3, 3, 3, 4 ),
 ( 2, 2 ),
 ( 0.000000000000000000, 0.1122669598086934867, 0.2243161639709926047, 0.3396355846219420438, 0.4553962076585420515, 0.5677860799922670454, 0.6749047109689817470, 0.7773884377078588148, 0.8775581155834574210, 0.9782364162378296424, 1.000000000000000000 ),
 ( 0.000000000000000000, 1.000000000000000000 ),
 .UNSPECIFIED. ) ;
#37697 = VERTEX_POINT ( 'NONE', #5648 ) ;
#37698 = ORIENTED_EDGE ( 'NONE', *, *, #4972, .F. ) ;
#37699 = EDGE_CURVE ( 'NONE', #3834, #61894, #69437, .T. ) ;
#37700 = VERTEX_POINT ( 'NONE', #59839 ) ;
#37701 = DIRECTION ( 'NONE',  ( -0.000000000000000000, -0.000000000000000000, -1.000000000000000000 ) ) ;
#37702 = ORIENTED_EDGE ( 'NONE', *, *, #91127, .T. ) ;
#37703 = EDGE_CURVE ( 'NONE', #19444, #56880, #43347, .T. ) ;
#37704 = CARTESIAN_POINT ( 'NONE',  ( 68.73406594905847555, 69.12949821581069898, 5.652800877584020611 ) ) ;
#37705 = ORIENTED_EDGE ( 'NONE', *, *, #67390, .F. ) ;
#37706 = CARTESIAN_POINT ( 'NONE',  ( 163.9910908123517288, 246.6060940548019289, -7.333295033952830444 ) ) ;
#37707 = EDGE_CURVE ( 'NONE', #11091, #72615, #9069, .T. ) ;
#37708 = CARTESIAN_POINT ( 'NONE',  ( 169.8557297738865941, 282.3553244834201337, 11.74113619686330701 ) ) ;
#37709 = EDGE_CURVE ( 'NONE', #14940, #53896, #55220, .T. ) ;
#37710 = CARTESIAN_POINT ( 'NONE',  ( -23.47641611835684117, 99.79318446887796767, 45.19945584158065799 ) ) ;
#37711 = CARTESIAN_POINT ( 'NONE',  ( 82.87668018738534670, 53.58938331343419748, -15.34904665510062571 ) ) ;
#37712 = ORIENTED_EDGE ( 'NONE', *, *, #6598, .F. ) ;
#37713 = CARTESIAN_POINT ( 'NONE',  ( 18.60133699236122595, 19.24335787977762990, -9.188101187500008038 ) ) ;
#37714 = CARTESIAN_POINT ( 'NONE',  ( 198.8280325239424258, 277.6560935625093975, -15.37151893818075266 ) ) ;
#37715 = DIRECTION ( 'NONE',  ( -0.9414334852479518956, -0.3371987438498165734, 0.000000000000000000 ) ) ;
#37717 = VERTEX_POINT ( 'NONE', #31926 ) ;
#37716 = CARTESIAN_POINT ( 'NONE',  ( -12.68721568607400485, 24.67147432707382038, -10.00000000000000000 ) ) ;
#37718 = CARTESIAN_POINT ( 'NONE',  ( 163.2835940097493790, 247.8315144631017404, 11.08416305054517359 ) ) ;
#37719 = CARTESIAN_POINT ( 'NONE',  ( 187.7204020327498313, 260.5175946176191815, 2.856882547745535739 ) ) ;
#37720 = CARTESIAN_POINT ( 'NONE',  ( 79.85280895619634123, 44.70080194145975128, 11.24692901854433735 ) ) ;
#37722 = CARTESIAN_POINT ( 'NONE',  ( -27.42236680055714260, 166.5217562850347406, 1.224646799147364892E-15 ) ) ;
#37721 = B_SPLINE_CURVE_WITH_KNOTS ( 'NONE', 3,
 ( #84264, #45210, #76622, #29038, #21915, #21428, #38091, #91353, #59909, #60397, #13821, #68017, #44701, #75632, #37114, #83762 ),
 .UNSPECIFIED., .F., .F.,
 ( 4, 2, 2, 2, 2, 2, 2, 4 ),
 ( 0.0005218454421851866348, 0.0008352828619746982325, 0.001148720281764209830, 0.001462157701553721319, 0.001775595121343233026, 0.002089032541132744732, 0.002402469960922256221, 0.003029344800501365502 ),
 .UNSPECIFIED. ) ;
#37723 = CARTESIAN_POINT ( 'NONE',  ( 172.0399293152837572, 254.5145317268123790, 11.42224199934888418 ) ) ;
#37724 = CARTESIAN_POINT ( 'NONE',  ( 160.6911010070541863, 282.7964184354547683, 2.101448972218037614 ) ) ;
#37725 =( BOUNDED_CURVE ( )  B_SPLINE_CURVE ( 2, ( #77726, #17402, #79257, #69602, #47295, #23486, #15897, #53709, #23314 ),
 .UNSPECIFIED., .F., .T. ) 
 B_SPLINE_CURVE_WITH_KNOTS ( ( 3, 2, 2, 2, 3 ),
 ( 0.9072580645161290036, 0.9086021505376343788, 0.9112903225806451291, 0.9139784946236558794, 0.9153225806451612545 ),
 .UNSPECIFIED. ) 
 CURVE ( )  GEOMETRIC_REPRESENTATION_ITEM ( )  RATIONAL_B_SPLINE_CURVE ( ( 0.9330127018922194093, 0.9330127018922194093, 1.000000000000000000, 0.8660254037844387076, 1.000000000000000000, 0.8660254037844387076, 1.000000000000000000, 0.9330127018922194093, 0.9330127018922194093 ) ) 
 REPRESENTATION_ITEM ( '' )  );
#37726 = ORIENTED_EDGE ( 'NONE', *, *, #73488, .T. ) ;
#37727 = CARTESIAN_POINT ( 'NONE',  ( 194.6224351033329185, 293.5510494386875848, -14.91730472411656550 ) ) ;
#37728 = CARTESIAN_POINT ( 'NONE',  ( 74.81832046901196520, 67.48663194201290594, -12.71244991431774984 ) ) ;
#37729 = FACE_OUTER_BOUND ( 'NONE', #12095, .T. ) ;
#37730 = CARTESIAN_POINT ( 'NONE',  ( 0.3649266329730349034, 171.0177522451418781, -10.00000000000009592 ) ) ;
#37731 = CARTESIAN_POINT ( 'NONE',  ( 196.1039637098642459, 269.4745711467500087, -10.81934472805613545 ) ) ;
#37732 = B_SPLINE_CURVE_WITH_KNOTS ( 'NONE', 3,
 ( #78032, #87698, #55689, #2540 ),
 .UNSPECIFIED., .F., .F.,
 ( 4, 4 ),
 ( 0.02958148137093116747, 0.03870913465764597161 ),
 .UNSPECIFIED. ) ;
#37733 = CARTESIAN_POINT ( 'NONE',  ( 175.0403197011952159, 281.5117084114038448, -14.13282399009272261 ) ) ;
#37734 = CARTESIAN_POINT ( 'NONE',  ( 163.5122523041594036, 247.4354666796116078, -8.835398473100831040 ) ) ;
#37735 = CARTESIAN_POINT ( 'NONE',  ( 84.47504870052041781, 44.63565290773180294, -8.224897521149806323 ) ) ;
#37736 = CARTESIAN_POINT ( 'NONE',  ( 72.99830029227618411, 70.81959382475521636, 8.127746218293800951 ) ) ;
#37738 = CARTESIAN_POINT ( 'NONE',  ( 27.37565231528585841, 31.50829794293882102, -10.00000000000000355 ) ) ;
#37737 = CARTESIAN_POINT ( 'NONE',  ( -16.46870247313679059, 170.4869531367911293, 4.594050593750046652 ) ) ;
#37739 = CIRCLE ( 'NONE', #11886, 70.00000000000001421 ) ;
#37740 = CARTESIAN_POINT ( 'NONE',  ( 189.0934591145252170, 297.0081427490579813, 8.814819132589450490 ) ) ;
#37741 = ORIENTED_EDGE ( 'NONE', *, *, #51316, .F. ) ;
#37742 = EDGE_LOOP ( 'NONE', ( #78369, #27002, #47571, #26780, #93200 ) ) ;
#37743 = CARTESIAN_POINT ( 'NONE',  ( 45.16679497745494132, 120.1723871950187714, 10.00000000000000000 ) ) ;
#37744 = CARTESIAN_POINT ( 'NONE',  ( 79.14312167556931854, 57.64441083166269664, 0.000000000000000000 ) ) ;
#37745 = VECTOR ( 'NONE', #57226, 1000.000000000000000 ) ;
#37746 =( BOUNDED_CURVE ( )  B_SPLINE_CURVE ( 2, ( #99981, #30564, #32040, #47250, #54847, #79704, #86314, #71076, #24456, #17351, #94395, #80202, #64460 ),
 .UNSPECIFIED., .F., .T. ) 
 B_SPLINE_CURVE_WITH_KNOTS ( ( 3, 2, 2, 2, 2, 2, 3 ),
 ( 0.03750000000000000555, 0.04000000000000000083, 0.04499999999999999833, 0.05000000000000000278, 0.05500000000000000028, 0.05999999999999999778, 0.06250000000000000000 ),
 .UNSPECIFIED. ) 
 CURVE ( )  GEOMETRIC_REPRESENTATION_ITEM ( )  RATIONAL_B_SPLINE_CURVE ( ( 0.9755282581475768211, 0.9755282581475768211, 1.000000000000000000, 0.9510565162951535312, 1.000000000000000000, 0.9510565162951535312, 1.000000000000000000, 0.9510565162951535312, 1.000000000000000000, 0.9510565162951535312, 1.000000000000000000, 0.9755282581475768211, 0.9755282581475768211 ) ) 
 REPRESENTATION_ITEM ( '' )  );
#37747 = FACE_OUTER_BOUND ( 'NONE', #73209, .T. ) ;
#37748 = CARTESIAN_POINT ( 'NONE',  ( 85.38646193529683615, 42.60607428054889567, 1.234017145255211112 ) ) ;
#37749 = CARTESIAN_POINT ( 'NONE',  ( 162.7089540403458159, 248.8268200861687376, -11.78833136687426553 ) ) ;
#37750 = CARTESIAN_POINT ( 'NONE',  ( 84.88791182130400159, 48.20836502411282254, 11.92161542626550208 ) ) ;
#37751 = CARTESIAN_POINT ( 'NONE',  ( 153.6085985088494681, 279.1348322646095994, 3.818864634155017423 ) ) ;
#37752 = CARTESIAN_POINT ( 'NONE',  ( 23.85612603422365297, 175.3923013555409796, 4.594050593750050204 ) ) ;
#37753 = VECTOR ( 'NONE', #25325, 999.9999999999998863 ) ;
#37754 = CARTESIAN_POINT ( 'NONE',  ( 111.5137010038235417, 241.3149278399161233, -9.188101187500095079 ) ) ;
#37755 = CARTESIAN_POINT ( 'NONE',  ( 179.3642964896383205, 292.0887335915682002, -6.148695452510337667 ) ) ;
#37756 = CARTESIAN_POINT ( 'NONE',  ( 168.7310635674097341, 283.4413295356843037, 12.00249716675341638 ) ) ;
#37757 = CARTESIAN_POINT ( 'NONE',  ( 206.6750745834628731, 271.7034134901589368, -6.697661943153482511 ) ) ;
#37758 = AXIS2_PLACEMENT_3D ( 'NONE', #51875, #64712, #87073 ) ;
#37759 = FACE_OUTER_BOUND ( 'NONE', #90884, .T. ) ;
#37760 = EDGE_CURVE ( 'NONE', #15004, #75836, #77976, .T. ) ;
#37761 = CARTESIAN_POINT ( 'NONE',  ( 60.85032556585977659, 217.4860189848785410, -2.679491924311252493 ) ) ;
#37762 = CARTESIAN_POINT ( 'NONE',  ( 195.7291534503633272, 291.6341570319625021, 16.44925029361851543 ) ) ;
#37763 = CYLINDRICAL_SURFACE ( 'NONE', #51779, 10.00000000000010658 ) ;
#37764 = CARTESIAN_POINT ( 'NONE',  ( 161.8882824960653579, 250.2482648971885340, -13.83574485983625557 ) ) ;
#37765 = CARTESIAN_POINT ( 'NONE',  ( 83.24292249771293939, 50.82510919314466236, 14.58399313936658537 ) ) ;
#37766 = CARTESIAN_POINT ( 'NONE',  ( -14.83894680564148238, 24.48641780169620219, 10.00000000000000000 ) ) ;
#37767 = CARTESIAN_POINT ( 'NONE',  ( 196.4319357531070693, 266.2480072935647399, 8.325861693847476985 ) ) ;
#37768 = CARTESIAN_POINT ( 'NONE',  ( 70.09710780656028817, 70.29879786405263076, 4.725240580867070328 ) ) ;
#37769 = DIRECTION ( 'NONE',  ( 0.2433040867433105825, 0.9699500612784163200, 0.000000000000000000 ) ) ;
#37770 = FACE_OUTER_BOUND ( 'NONE', #15618, .T. ) ;
#37771 = ORIENTED_EDGE ( 'NONE', *, *, #29502, .T. ) ;
#37772 = CARTESIAN_POINT ( 'NONE',  ( -22.42236680055709641, 157.8615022471902591, 0.000000000000000000 ) ) ;
#37773 = CARTESIAN_POINT ( 'NONE',  ( 181.5320323368239315, 267.9553237911030692, 15.00661790592713452 ) ) ;
#37774 = EDGE_CURVE ( 'NONE', #18010, #12449, #27175, .T. ) ;
#37775 = CARTESIAN_POINT ( 'NONE',  ( 97.73839765093606502, 236.4244531367911009, -4.594050593750046652 ) ) ;
#37776 = CARTESIAN_POINT ( 'NONE',  ( 161.8153478334749877, 250.3745914384277285, -14.21120979595050215 ) ) ;
#37777 = CARTESIAN_POINT ( 'NONE',  ( 191.3638605175971747, 299.1950661814348678, 7.382965314423603154 ) ) ;
#37778 = DIRECTION ( 'NONE',  ( -0.8660254037844377084, -0.5000000000000014433, -0.000000000000000000 ) ) ;
#37780 = CARTESIAN_POINT ( 'NONE',  ( 194.0373140624720349, 278.4935463477126518, 16.30235809050098794 ) ) ;
#37779 = CARTESIAN_POINT ( 'NONE',  ( 145.0115229932138163, 242.9824982072973683, 3.021315404115420679E-15 ) ) ;
#37781 = CARTESIAN_POINT ( 'NONE',  ( 201.1568026402725877, 270.4843927660949134, -10.02948014338874039 ) ) ;
#37782 = CARTESIAN_POINT ( 'NONE',  ( 198.4782858197754649, 286.8725200914082620, -17.44895083299520522 ) ) ;
#37783 = DIRECTION ( 'NONE',  ( 1.000000000000000000, 0.000000000000000000, 0.000000000000000000 ) ) ;
#37784 = CARTESIAN_POINT ( 'NONE',  ( 37.50955192761952617, 39.84336893147759184, -7.433330006724137462 ) ) ;
#37785 = LINE ( 'NONE', #99619, #27260 ) ;
#37786 = CYLINDRICAL_SURFACE ( 'NONE', #44263, 17.82106496071139645 ) ;
#37787 = VERTEX_POINT ( 'NONE', #78559 ) ;
#37788 = CARTESIAN_POINT ( 'NONE',  ( 26.50621139815081762, 30.70171378149920471, -9.188101187500004485 ) ) ;
#37789 = CARTESIAN_POINT ( 'NONE',  ( 80.74781574657599492, 57.21644485803225422, 16.56566952311892749 ) ) ;
#37790 = CARTESIAN_POINT ( 'NONE',  ( 147.5118896528469179, 275.1489077312122049, -3.975523961781759930 ) ) ;
#37791 = CARTESIAN_POINT ( 'NONE',  ( 196.8435556370661459, 289.7039558245273838, -16.43899056939217118 ) ) ;
#37792 = VERTEX_POINT ( 'NONE', #9146 ) ;
#37793 = CARTESIAN_POINT ( 'NONE',  ( 70.89420290055875284, 60.93121495745884175, 14.54576430277729315 ) ) ;
#37794 = CARTESIAN_POINT ( 'NONE',  ( 198.4264492142971221, 286.9623037257889564, 17.00126466006521397 ) ) ;
#37795 = CARTESIAN_POINT ( 'NONE',  ( 180.3364889203162988, 263.1152589884272857, -12.84555436964710218 ) ) ;
#37796 = CARTESIAN_POINT ( 'NONE',  ( 169.4616969408077978, 252.2111926658335221, -8.760020798663340713 ) ) ;
#37797 = CARTESIAN_POINT ( 'NONE',  ( 152.8107382695299918, 265.9710327055011589, 16.32045346488711246 ) ) ;
#37798 = ORIENTED_EDGE ( 'NONE', *, *, #65619, .T. ) ;
#37799 = CARTESIAN_POINT ( 'NONE',  ( 73.03023235113748513, 69.68176590430279305, 9.698330045464274463 ) ) ;
#37800 = CARTESIAN_POINT ( 'NONE',  ( 35.22902474502244274, 28.84335787977765619, 9.188101187500006262 ) ) ;
#37801 = ORIENTED_EDGE ( 'NONE', *, *, #64611, .T. ) ;
#37802 = CARTESIAN_POINT ( 'NONE',  ( 164.7636693376427388, 247.7456902508657492, 7.156984819320836522 ) ) ;
#37803 = CARTESIAN_POINT ( 'NONE',  ( 184.9534712104859011, 293.2739629945884872, -10.43194920464371300 ) ) ;
#37804 = ORIENTED_EDGE ( 'NONE', *, *, #26693, .T. ) ;
#37805 = CARTESIAN_POINT ( 'NONE',  ( 86.40784109447328376, 47.52432272822921533, -11.05097720836334396 ) ) ;
#37806 = CARTESIAN_POINT ( 'NONE',  ( 158.9588665712855118, 256.6514483001959661, 16.71440725461184940 ) ) ;
#37807 = CARTESIAN_POINT ( 'NONE',  ( 190.5140674548521531, 278.6669388570777528, -16.50821822264429173 ) ) ;
#37808 = CARTESIAN_POINT ( 'NONE',  ( 153.8198515416281964, 264.2231972476349711, -16.55097973663693978 ) ) ;
#37809 = CARTESIAN_POINT ( 'NONE',  ( 200.7134601498536028, 283.0010845879393742, -16.98649239173277792 ) ) ;
#37810 = VECTOR ( 'NONE', #82599, 1000.000000000000114 ) ;
#37811 = CARTESIAN_POINT ( 'NONE',  ( 34.24030602833327208, 37.95586893147758900, 7.433330006724141015 ) ) ;
#37812 = CARTESIAN_POINT ( 'NONE',  ( 193.0126352936363503, 264.4189281174865869, 8.906082567666748773 ) ) ;
#37813 = EDGE_CURVE ( 'NONE', #66505, #79746, #53038, .T. ) ;
#37814 = CYLINDRICAL_SURFACE ( 'NONE', #87139, 14.99999999999967493 ) ;
#37815 = ORIENTED_EDGE ( 'NONE', *, *, #84417, .T. ) ;
#37816 = CARTESIAN_POINT ( 'NONE',  ( 45.37789370152431445, 208.5530062829863027, -4.648177544792955347E-16 ) ) ;
#37817 = VERTEX_POINT ( 'NONE', #17232 ) ;
#37818 = CIRCLE ( 'NONE', #73428, 70.00000000000001421 ) ;
#37819 = ORIENTED_EDGE ( 'NONE', *, *, #60128, .T. ) ;
#37820 = CARTESIAN_POINT ( 'NONE',  ( 198.1516807435644409, 286.9647030927445144, 16.94921385266723490 ) ) ;
#37821 = CARTESIAN_POINT ( 'NONE',  ( 87.11842579636694950, 45.87328929624024454, -8.641498891285833039 ) ) ;
#37823 = CARTESIAN_POINT ( 'NONE',  ( 190.1235086622576773, 300.2499232672161043, -3.363423802915200156 ) ) ;
#37822 = CARTESIAN_POINT ( 'NONE',  ( 174.3740210016665628, 256.9530918469817493, -12.27374415811068076 ) ) ;
#37824 = DIRECTION ( 'NONE',  ( -0.8660254037844387076, -0.4999999999999998890, -0.000000000000000000 ) ) ;
#37825 = CARTESIAN_POINT ( 'NONE',  ( 197.8058269970693743, 272.4609363502503356, -13.32996429882288147 ) ) ;
#37826 = CIRCLE ( 'NONE', #32991, 7.273499999999997634 ) ;
#37827 = CARTESIAN_POINT ( 'NONE',  ( 203.4776550330608416, 276.3243839139203715, 14.43342264677212405 ) ) ;
#37828 = CARTESIAN_POINT ( 'NONE',  ( 82.08231906242987463, 40.78080646243900276, 1.383867760887848020 ) ) ;
#37829 = CARTESIAN_POINT ( 'NONE',  ( 168.2008345946905479, 248.1884056956802453, -5.064766917302788052 ) ) ;
#37830 = ADVANCED_FACE ( 'NONE', ( #70960 ), #1561, .T. ) ;
#37831 = CARTESIAN_POINT ( 'NONE',  ( 77.30991866800115986, 63.26798366544798569, -15.19874235486285663 ) ) ;
#37832 = CONICAL_SURFACE ( 'NONE', #58867, 11.91750000000000043, 0.7853981633974482790 ) ;
#37833 = CARTESIAN_POINT ( 'NONE',  ( 186.8266632922035910, 287.0577513604794149, -15.74549898466382203 ) ) ;
#37834 = CARTESIAN_POINT ( 'NONE',  ( 106.3175485811169239, 238.3149278399160949, -9.188101187500095079 ) ) ;
#37835 = ORIENTED_EDGE ( 'NONE', *, *, #97583, .F. ) ;
#37836 = DIRECTION ( 'NONE',  ( -0.000000000000000000, -0.000000000000000000, -1.000000000000000000 ) ) ;
#37837 = CARTESIAN_POINT ( 'NONE',  ( 36.57375671714491006, 36.51421378149921537, -9.188101187500004485 ) ) ;
#37838 = CARTESIAN_POINT ( 'NONE',  ( 188.2014231658550898, 273.5110677970230313, 15.67131877287846287 ) ) ;
#37839 = VERTEX_POINT ( 'NONE', #79084 ) ;
#37840 = CARTESIAN_POINT ( 'NONE',  ( 74.07678436671264421, 68.35284689741969544, -11.67875583378132198 ) ) ;
#37841 = LINE ( 'NONE', #54031, #75489 ) ;
#37842 = CARTESIAN_POINT ( 'NONE',  ( 198.2505066714982149, 285.2670451491296149, 0.000000000000000000 ) ) ;
#37843 = CARTESIAN_POINT ( 'NONE',  ( 190.4495984692767649, 300.3985526752458668, -0.4774468551831849705 ) ) ;
#37844 = CARTESIAN_POINT ( 'NONE',  ( 193.8698296682186992, 271.7227521665574841, -15.05645239061159479 ) ) ;
#37845 = VERTEX_POINT ( 'NONE', #25337 ) ;
#37846 = CARTESIAN_POINT ( 'NONE',  ( 195.4428138874578167, 292.1301117031320587, 15.46566957515385710 ) ) ;
#37847 = ORIENTED_EDGE ( 'NONE', *, *, #95033, .T. ) ;
#37848 = CARTESIAN_POINT ( 'NONE',  ( -19.65312891409030271, 93.06504152958497400, 59.99999999999999289 ) ) ;
#37849 = ORIENTED_EDGE ( 'NONE', *, *, #96152, .F. ) ;
#37850 = CARTESIAN_POINT ( 'NONE',  ( 190.8936203498974464, 267.5824989483721197, -12.06459381115725904 ) ) ;
#37851 = CARTESIAN_POINT ( 'NONE',  ( 192.3722320044300034, 262.8214543474982179, 4.572296880953776288 ) ) ;
#37852 = DIRECTION ( 'NONE',  ( -0.8435938723211519052, -0.5369817302126803638, 0.000000000000000000 ) ) ;
#37853 = CARTESIAN_POINT ( 'NONE',  ( 6.406750531224583156, 186.0530062829863027, -4.648177544792955347E-16 ) ) ;
#37855 = CARTESIAN_POINT ( 'NONE',  ( 160.5389806683030827, 281.4356532093604528, 5.616753171805936695 ) ) ;
#37854 = CARTESIAN_POINT ( 'NONE',  ( 184.2746014452833379, 288.7589902912345678, -13.23859099789902594 ) ) ;
#37856 = CARTESIAN_POINT ( 'NONE',  ( 197.4075646047015482, 273.1427705089788560, -14.69744958829762815 ) ) ;
#37857 = VERTEX_POINT ( 'NONE', #30938 ) ;
#37858 = CARTESIAN_POINT ( 'NONE',  ( 147.1249913145849177, 275.8190353104462815, 3.637773609013635223 ) ) ;
#37859 = CARTESIAN_POINT ( 'NONE',  ( 73.55941717774605593, 69.21675373535786946, 9.988905871803112291 ) ) ;
#37860 = CARTESIAN_POINT ( 'NONE',  ( 190.5337456798271205, 263.9425320260396575, -9.625448268029721532 ) ) ;
#37861 = CARTESIAN_POINT ( 'NONE',  ( 173.5418303646803793, 251.2005048794018194, -1.013737780652142151 ) ) ;
#37862 = CARTESIAN_POINT ( 'NONE',  ( 163.2308556539849178, 280.6958281187306170, -11.57967609262591502 ) ) ;
#37863 = CARTESIAN_POINT ( 'NONE',  ( 72.13517842779845068, 72.31474564102330760, 3.615969315562336472 ) ) ;
#37864 = CARTESIAN_POINT ( 'NONE',  ( 31.23047667836735641, 41.52903772873361277, -1.583844403245329602 ) ) ;
#37865 = DIRECTION ( 'NONE',  ( -1.000000000000000000, 0.000000000000000000, 0.000000000000000000 ) ) ;
#37866 = CARTESIAN_POINT ( 'NONE',  ( 194.4165969972361552, 293.9075714965812267, 14.23342188338008718 ) ) ;
#37867 = CARTESIAN_POINT ( 'NONE',  ( 191.4282566499900895, 282.7875431929116417, -17.14954741723730436 ) ) ;
#37868 = CARTESIAN_POINT ( 'NONE',  ( 82.75828967192548191, 53.74568045750391576, -15.77735475420663569 ) ) ;
#37869 = CARTESIAN_POINT ( 'NONE',  ( 81.47361835793333285, 217.8458772461660544, 9.188101187500095079 ) ) ;
#37870 = FACE_OUTER_BOUND ( 'NONE', #40047, .T. ) ;
#37871 = CARTESIAN_POINT ( 'NONE',  ( 147.5381343315788172, 275.1034506142203782, -4.056595942992749393 ) ) ;
#37872 = FACE_OUTER_BOUND ( 'NONE', #12178, .T. ) ;
#37873 = ADVANCED_FACE ( 'NONE', ( #85182 ), #15729, .T. ) ;
#37874 = CARTESIAN_POINT ( 'NONE',  ( 161.1232569692349443, 251.5733279787459367, -14.02750397520710557 ) ) ;
#37875 = CARTESIAN_POINT ( 'NONE',  ( -19.65312891409030271, 93.06504152958497400, 177.5919119679930134 ) ) ;
#37877 = CARTESIAN_POINT ( 'NONE',  ( 76.46903462498934800, 51.53433314985417013, 15.63818393615307478 ) ) ;
#37876 = CARTESIAN_POINT ( 'NONE',  ( 73.32220977704777454, 69.17604616796300832, -9.911163241522066514 ) ) ;
#37878 = CARTESIAN_POINT ( 'NONE',  ( 193.8626392119275010, 262.2145712166342264, 1.470488869930418607 ) ) ;
#37879 = FACE_OUTER_BOUND ( 'NONE', #13093, .T. ) ;
#37880 = CARTESIAN_POINT ( 'NONE',  ( 157.3305006125302441, 282.1378183958786963, 1.589776369934247979 ) ) ;
#37881 = CARTESIAN_POINT ( 'NONE',  ( 157.5520850189458884, 257.7587792392113215, 16.71892742266126319 ) ) ;
#37882 = CARTESIAN_POINT ( 'NONE',  ( 72.21694820471849141, 72.08926726930118889, 3.059610661676269050 ) ) ;
#37883 = VECTOR ( 'NONE', #62166, 1000.000000000000000 ) ;
#37884 = CARTESIAN_POINT ( 'NONE',  ( 31.13589176296283156, 188.7833772461660544, -9.188101187500095079 ) ) ;
#37885 = EDGE_CURVE ( 'NONE', #80464, #65643, #4017, .T. ) ;
#37886 = CARTESIAN_POINT ( 'NONE',  ( 56.57573509489573382, 191.2202760586659736, -5.415160957724236172E-17 ) ) ;
#37887 = CARTESIAN_POINT ( 'NONE',  ( 196.4677102463732012, 290.3549391369982686, 16.45225250689336249 ) ) ;
#37889 = CARTESIAN_POINT ( 'NONE',  ( 81.35748880148537410, 42.22347387491733173, -7.155507324468848296 ) ) ;
#37888 = VECTOR ( 'NONE', #710, 1000.000000000000114 ) ;
#37890 = CARTESIAN_POINT ( 'NONE',  ( 78.83097366254324356, 50.94081823793872132, -15.13050861895527177 ) ) ;
#37891 = CARTESIAN_POINT ( 'NONE',  ( -11.23620533500811725, 170.9865022471903444, -10.00000000000009415 ) ) ;
#37892 = CARTESIAN_POINT ( 'NONE',  ( 57.73936995728981714, 194.9548013555410080, -4.594050593750042211 ) ) ;
#37893 = CARTESIAN_POINT ( 'NONE',  ( 23.58217936225004863, 25.56628583063841376, 9.188101187500006262 ) ) ;
#37894 = CARTESIAN_POINT ( 'NONE',  ( 150.6626254231123880, 269.6916732958875969, -15.32062296289003811 ) ) ;
#37895 = CARTESIAN_POINT ( 'NONE',  ( 196.8435556370661459, 289.7039558245273838, -16.43899056939217118 ) ) ;
#37896 = CARTESIAN_POINT ( 'NONE',  ( 8.675723883004062387, 25.98502408145591147, -5.678558825948271327 ) ) ;
#37897 = LINE ( 'NONE', #12268, #50486 ) ;
#37898 = CARTESIAN_POINT ( 'NONE',  ( 76.88601853014658616, 63.69663891124154276, 15.33692311465240543 ) ) ;
#37899 = CARTESIAN_POINT ( 'NONE',  ( 175.6477625036710606, 291.0204324385146037, 2.451421089737829906 ) ) ;
#37900 = CARTESIAN_POINT ( 'NONE',  ( 159.4889735931715222, 254.4039898200529706, 16.88104032092801887 ) ) ;
#37901 = LINE ( 'NONE', #14129, #50568 ) ;
#37902 = CARTESIAN_POINT ( 'NONE',  ( 201.3272413420560554, 281.9379843783140700, 16.84531592925761601 ) ) ;
#37903 = EDGE_CURVE ( 'NONE', #93443, #57499, #44223, .T. ) ;
#37904 = DIRECTION ( 'NONE',  ( 0.5000000000000048850, -0.8660254037844358210, 0.000000000000000000 ) ) ;
#37905 = CARTESIAN_POINT ( 'NONE',  ( 109.6465072765697641, 244.1115022471903160, -5.000000000000047962 ) ) ;
#37906 = CARTESIAN_POINT ( 'NONE',  ( 161.8289209813647176, 250.3510820566641257, 13.28523796267037937 ) ) ;
#37907 = CARTESIAN_POINT ( 'NONE',  ( 194.0058304551163531, 285.1060772508486707, -16.99837373451835631 ) ) ;
#37908 = EDGE_LOOP ( 'NONE', ( #24816, #47423, #2860 ) ) ;
#37909 = CARTESIAN_POINT ( 'NONE',  ( 77.19879077027466963, 49.27944484189550423, 15.37723906343501490 ) ) ;
#37910 = ORIENTED_EDGE ( 'NONE', *, *, #32301, .T. ) ;
#37911 = CARTESIAN_POINT ( 'NONE',  ( 46.54103524584390783, 115.8319611975524595, 10.00000000000000000 ) ) ;
#37912 = CARTESIAN_POINT ( 'NONE',  ( 194.1883405663843689, 293.5167174303800834, 14.56505799480749452 ) ) ;
#37913 = DIRECTION ( 'NONE',  ( -0.8660254037844387076, -0.4999999999999998890, -0.000000000000000000 ) ) ;
#37914 = EDGE_LOOP ( 'NONE', ( #80643, #82750, #71399, #1204 ) ) ;
#37915 = CARTESIAN_POINT ( 'NONE',  ( 157.4068442735347446, 281.9945091197541274, 2.874377194828706905 ) ) ;
#37916 = CARTESIAN_POINT ( 'NONE',  ( 207.6727254509676186, 270.9472835030587703, 7.315149605389819953 ) ) ;
#37917 = CARTESIAN_POINT ( 'NONE',  ( 148.1004780136491377, 274.1294427855589788, -7.811560775291159331 ) ) ;
#37918 = CARTESIAN_POINT ( 'NONE',  ( 85.22469180575973269, 42.26411194152829154, 2.911061958177603604 ) ) ;
#37919 = VERTEX_POINT ( 'NONE', #49151 ) ;
#37920 = CARTESIAN_POINT ( 'NONE',  ( 18.54180792094154029, 32.74646525600390135, 2.839279412974139660 ) ) ;
#37921 = CARTESIAN_POINT ( 'NONE',  ( 67.55733782939270782, 69.42818843681499175, -2.263445650850663515 ) ) ;
#37922 = CARTESIAN_POINT ( 'NONE',  ( 48.91560817564824504, 80.00000000000000000, 59.99999999999999289 ) ) ;
#37923 = EDGE_CURVE ( 'NONE', #18075, #54901, #67649, .T. ) ;
#37924 = EDGE_CURVE ( 'NONE', #70463, #56261, #19757, .T. ) ;
#37925 = ORIENTED_EDGE ( 'NONE', *, *, #32798, .F. ) ;
#37926 = FACE_OUTER_BOUND ( 'NONE', #72010, .T. ) ;
#37927 = CARTESIAN_POINT ( 'NONE',  ( 159.2122473525774069, 254.8832937285494609, -16.22689353966294590 ) ) ;
#37928 = ORIENTED_EDGE ( 'NONE', *, *, #60227, .T. ) ;
#37929 = EDGE_CURVE ( 'NONE', #20151, #734, #97366, .T. ) ;
#37930 = CARTESIAN_POINT ( 'NONE',  ( 174.6916540630883503, 286.2244833470182925, 10.52363204570947275 ) ) ;
#37932 = CARTESIAN_POINT ( 'NONE',  ( 67.83594148062915963, 65.58978118587256745, -10.89425741029403305 ) ) ;
#37931 = CARTESIAN_POINT ( 'NONE',  ( 162.5729093422976916, 283.3574902375370925, -3.116333471781629783 ) ) ;
#37933 = CARTESIAN_POINT ( 'NONE',  ( 207.8136982414359579, 270.7031114674828700, -0.9536989003868096004 ) ) ;
#37934 = CARTESIAN_POINT ( 'NONE',  ( 164.4936379324916516, 245.7356569095223051, 6.719479797016231437 ) ) ;
#37935 = FACE_OUTER_BOUND ( 'NONE', #83125, .T. ) ;
#37936 = CARTESIAN_POINT ( 'NONE',  ( 179.2728639618759985, 293.8282488962061620, 5.658163206248635113 ) ) ;
#37937 = CARTESIAN_POINT ( 'NONE',  ( 133.7599021114188247, 248.0333772461660544, 9.188101187500095079 ) ) ;
#37938 = ADVANCED_FACE ( 'NONE', ( #43527 ), #73454, .F. ) ;
#37939 = CARTESIAN_POINT ( 'NONE',  ( 177.2759083163978744, 269.2989204424369518, 16.08029799372871338 ) ) ;
#37940 = CARTESIAN_POINT ( 'NONE',  ( 181.9605180691946771, 260.3799461757151334, 9.466307468308277961 ) ) ;
#37941 = CARTESIAN_POINT ( 'NONE',  ( 75.92590343676303632, 205.4548013555409796, -4.594050593750042211 ) ) ;
#37942 = VERTEX_POINT ( 'NONE', #27347 ) ;
#37943 = CARTESIAN_POINT ( 'NONE',  ( 171.2741013746033332, 249.3936815359432728, 2.927055546763141169 ) ) ;
#37944 = FACE_OUTER_BOUND ( 'NONE', #70121, .T. ) ;
#37945 = CARTESIAN_POINT ( 'NONE',  ( 189.4199209167946663, 300.3895034224956930, 3.306026617473488027 ) ) ;
#37946 = ORIENTED_EDGE ( 'NONE', *, *, #57621, .T. ) ;
#37947 = CARTESIAN_POINT ( 'NONE',  ( 161.3383531994606699, 252.8394435820131605, 14.78188028638097506 ) ) ;
#37948 = ORIENTED_EDGE ( 'NONE', *, *, #34302, .T. ) ;
#37949 = ORIENTED_EDGE ( 'NONE', *, *, #60812, .F. ) ;
#37950 = EDGE_CURVE ( 'NONE', #97599, #21181, #89209, .T. ) ;
#37951 = FACE_BOUND ( 'NONE', #55299, .T. ) ;
#37952 = CARTESIAN_POINT ( 'NONE',  ( 67.15620270673211678, 67.72793565538280802, 6.583466307750684976 ) ) ;
#37953 = EDGE_CURVE ( 'NONE', #12155, #83087, #33965, .T. ) ;
#37954 = CARTESIAN_POINT ( 'NONE',  ( 194.1604701155857526, 284.7193346175499187, 17.50795125310741795 ) ) ;
#37955 = CARTESIAN_POINT ( 'NONE',  ( -32.90453922033355383, 95.26561800654556578, 10.83411691445564351 ) ) ;
#37956 = CARTESIAN_POINT ( 'NONE',  ( 68.10741622413405594, 65.45592947349832968, 10.45487064772517982 ) ) ;
#37957 = CARTESIAN_POINT ( 'NONE',  ( 194.4263876777154394, 293.8906135405502482, 15.23185943445137802 ) ) ;
#37958 = PLANE ( 'NONE',  #81982 ) ;
#37959 = CARTESIAN_POINT ( 'NONE',  ( 87.45543461181301836, 45.01664465679171201, 6.930016242323786990 ) ) ;
#37960 = EDGE_LOOP ( 'NONE', ( #35112, #5786, #59039, #35360 ) ) ;
#37961 = VECTOR ( 'NONE', #6602, 1000.000000000000227 ) ;
#37962 = B_SPLINE_SURFACE_WITH_KNOTS ( 'NONE', 3, 1, ( 
 ( #38164, #21504 ),
 ( #5796, #69084 ),
 ( #76217, #30594 ),
 ( #83333, #37675 ),
 ( #99509, #99012 ),
 ( #52886, #100009 ),
 ( #83836, #14402 ),
 ( #6794, #68586 ),
 ( #51394, #36185 ),
 ( #60975, #67090 ),
 ( #91939, #77185 ),
 ( #93428, #22977 ),
 ( #53866, #84827 ),
 ( #46789, #190 ),
 ( #1708, #23981 ),
 ( #46264, #1195 ),
 ( #15366, #39160 ),
 ( #47278, #62462 ),
 ( #54878, #32589 ),
 ( #79241, #8294 ),
 ( #31075, #94425 ),
 ( #40674, #2207 ),
 ( #31570, #92429 ),
 ( #70073, #69582 ),
 ( #61963, #688 ),
 ( #16881, #7792 ),
 ( #61480, #85859 ),
 ( #38678, #16385 ),
 ( #63487, #24979 ),
 ( #78201, #92916 ),
 ( #23469, #86348 ),
 ( #54360, #8788 ),
 ( #32073, #15876 ),
 ( #62986, #93930 ) ),
 .UNSPECIFIED., .T., .F., .F.,
 ( 4, 2, 2, 2, 2, 2, 2, 2, 2, 2, 2, 2, 2, 2, 2, 2, 4 ),
 ( 2, 2 ),
 ( 0.000000000000000000, 0.06250000000000000000, 0.1250000000000000000, 0.1875000000000000000, 0.2500000000000000000, 0.3125000000000000000, 0.3750000000000000000, 0.4375000000000000000, 0.5000000000000000000, 0.5625000000000000000, 0.6250000000000000000, 0.6875000000000000000, 0.7500000000000000000, 0.8125000000000000000, 0.8750000000000000000, 0.9375000000000000000, 1.000000000000000000 ),
 ( 0.000000000000000000, 1.000000000000000000 ),
 .UNSPECIFIED. ) ;
#37963 = DIRECTION ( 'NONE',  ( 0.2091919045418403900, 0.9778746070300412541, 0.000000000000000000 ) ) ;
#37964 = ORIENTED_EDGE ( 'NONE', *, *, #13412, .T. ) ;
#37965 = CARTESIAN_POINT ( 'NONE',  ( 76.18264033726677553, 51.55645319538977134, -15.67776776688645235 ) ) ;
#37966 = VECTOR ( 'NONE', #71520, 1000.000000000000227 ) ;
#37967 = FACE_OUTER_BOUND ( 'NONE', #61146, .T. ) ;
#37968 = CARTESIAN_POINT ( 'NONE',  ( 194.9160431658341395, 279.6352213503219559, 17.41133371011275699 ) ) ;
#37969 = CARTESIAN_POINT ( 'NONE',  ( 162.9383048163760463, 261.5404076612216500, 17.29887017337560096 ) ) ;
#37970 = CARTESIAN_POINT ( 'NONE',  ( 133.7599021114188247, 248.0333772461660544, 9.188101187500095079 ) ) ;
#37971 = ORIENTED_EDGE ( 'NONE', *, *, #38134, .T. ) ;
#37972 = CARTESIAN_POINT ( 'NONE',  ( -23.47208873469913115, 24.42380372261332155, -10.00000000000000000 ) ) ;
#37973 = CARTESIAN_POINT ( 'NONE',  ( 17.55280445478281237, 33.77154675864930056, 177.5919119679930134 ) ) ;
#37974 = CARTESIAN_POINT ( 'NONE',  ( 87.95576658732893804, 44.05533438356886222, -1.735394378949605576 ) ) ;
#37975 = CARTESIAN_POINT ( 'NONE',  ( 152.8328714238065515, 265.9326969577624027, -16.29536156676786263 ) ) ;
#37976 = LINE ( 'NONE', #45098, #75686 ) ;
#37977 = CARTESIAN_POINT ( 'NONE',  ( 67.94548261240784370, 67.41770141102237801, -7.935486469137003951 ) ) ;
#37978 = EDGE_LOOP ( 'NONE', ( #47533, #53072, #16677, #28726 ) ) ;
#37979 = CARTESIAN_POINT ( 'NONE',  ( 199.4197156453936373, 266.8589959824688549, 4.580656179805971284 ) ) ;
#37980 = CARTESIAN_POINT ( 'NONE',  ( 76.67083364154854053, 226.6199935810941213, 2.679491924311251605 ) ) ;
#37981 = FACE_OUTER_BOUND ( 'NONE', #54008, .T. ) ;
#37982 = CARTESIAN_POINT ( 'NONE',  ( 80.24293753902323090, 48.56639400389035899, 13.78793733260431331 ) ) ;
#37983 = CARTESIAN_POINT ( 'NONE',  ( 83.82185059330514321, 51.95230014857058620, 14.93193377595572002 ) ) ;
#37984 = CARTESIAN_POINT ( 'NONE',  ( 196.5499765897077964, 265.0522732887451411, 0.8242394764280709385 ) ) ;
#37985 = VERTEX_POINT ( 'NONE', #64851 ) ;
#37986 = DIRECTION ( 'NONE',  ( -0.3473291852295006810, 0.6015917957689992379, 0.7193398003386451967 ) ) ;
#37987 = CARTESIAN_POINT ( 'NONE',  ( 183.0648203791300546, 280.6896956899441875, 16.60862611305853775 ) ) ;
#37989 = EDGE_CURVE ( 'NONE', #60097, #100252, #12148, .T. ) ;
#37988 = CIRCLE ( 'NONE', #26746, 70.00000000000001421 ) ;
#37990 = CARTESIAN_POINT ( 'NONE',  ( 206.9676408587583296, 272.1685258403992975, 7.544050792475608169 ) ) ;
#37992 = CARTESIAN_POINT ( 'NONE',  ( 196.8989084261116886, 269.7173827915191850, 12.31991664540137954 ) ) ;
#37991 = LINE ( 'NONE', #24316, #79124 ) ;
#37993 = EDGE_CURVE ( 'NONE', #39719, #54166, #26129, .T. ) ;
#37994 = CARTESIAN_POINT ( 'NONE',  ( 24.75116620650193866, 19.45404122711133965, -8.090169943749478065 ) ) ;
#37995 = CARTESIAN_POINT ( 'NONE',  ( 28.09809348231459936, 175.4824982072973967, 3.021315404115420679E-15 ) ) ;
#37996 = CARTESIAN_POINT ( 'NONE',  ( 164.8705138155180521, 286.2009910768602481, -3.373684704351256780 ) ) ;
#37997 = CARTESIAN_POINT ( 'NONE',  ( 48.81784752633560487, 86.82484054835779830, -10.00000000000000000 ) ) ;
#37998 = DIRECTION ( 'NONE',  ( 0.8660254037844385966, 0.5000000000000003331, -0.000000000000000000 ) ) ;
#37999 = CARTESIAN_POINT ( 'NONE',  ( -12.86919761471646773, 169.5024278399161233, -9.188101187500093303 ) ) ;
#38000 = CARTESIAN_POINT ( 'NONE',  ( 75.63696797857046761, 221.1427522451419065, -10.00000000000009592 ) ) ;
#38001 = ORIENTED_EDGE ( 'NONE', *, *, #31161, .T. ) ;
#38002 = EDGE_CURVE ( 'NONE', #68704, #73023, #46546, .T. ) ;
#38003 = CARTESIAN_POINT ( 'NONE',  ( 66.89604841441746430, 67.64130223492367122, -6.456890807137734889 ) ) ;
#38004 = CARTESIAN_POINT ( 'NONE',  ( 73.02740203026323229, 70.73066625390264051, -7.556326162255497358 ) ) ;
#38005 = CARTESIAN_POINT ( 'NONE',  ( -19.65312891409030271, 93.06504152958497400, 10.00000000000000888 ) ) ;
#38006 = CARTESIAN_POINT ( 'NONE',  ( 16.17015057563676450, 170.9548013555409796, -4.594050593750042211 ) ) ;
#38007 = CARTESIAN_POINT ( 'NONE',  ( 29.08982151148960682, 17.76426979415090912, 3.090169943749476733 ) ) ;
#38008 = CARTESIAN_POINT ( 'NONE',  ( 83.48029009741895834, 41.89032089958049454, -3.321841928985223902 ) ) ;
#38009 = CARTESIAN_POINT ( 'NONE',  ( 171.6054817282545741, 271.5228642886609123, -16.51620184496720611 ) ) ;
#38010 = CARTESIAN_POINT ( 'NONE',  ( 150.1413706805870731, 276.5095333114461482, 3.755964711348897200 ) ) ;
#38011 = CARTESIAN_POINT ( 'NONE',  ( 179.3677837486497992, 255.1410135168996192, -4.004816050580029874 ) ) ;
#38012 = ADVANCED_FACE ( 'NONE', ( #30329 ), #29341, .T. ) ;
#38013 = CARTESIAN_POINT ( 'NONE',  ( 189.4592384298869376, 261.1887071297708758, -0.7541892224000766864 ) ) ;
#38014 = EDGE_CURVE ( 'NONE', #1578, #82522, #60206, .T. ) ;
#38015 = VECTOR ( 'NONE', #8806, 1000.000000000000000 ) ;
#38016 = CARTESIAN_POINT ( 'NONE',  ( 183.0125666146673780, 295.6744899775687827, 1.024979532612127819 ) ) ;
#38017 = CARTESIAN_POINT ( 'NONE',  ( 52.48883062679684741, 201.1115022471902591, 10.00000000000009592 ) ) ;
#38018 = FACE_OUTER_BOUND ( 'NONE', #231, .T. ) ;
#38019 = CARTESIAN_POINT ( 'NONE',  ( 190.4281805785508084, 300.8157113754859893, -1.233909217199055774 ) ) ;
#38020 = CARTESIAN_POINT ( 'NONE',  ( 13.65283037618196893, 184.8149278399160664, 9.188101187500093303 ) ) ;
#38021 = CARTESIAN_POINT ( 'NONE',  ( 72.45751905151223582, 70.67373443742413031, -7.865264308201658672 ) ) ;
#38022 = LINE ( 'NONE', #31930, #79232 ) ;
#38023 = CARTESIAN_POINT ( 'NONE',  ( 44.29582294825809896, 31.28920272979930672, -7.433330006724141015 ) ) ;
#38024 = CARTESIAN_POINT ( 'NONE',  ( 202.1252189466871130, 279.3787218446790348, -15.92426048611617340 ) ) ;
#38025 = AXIS2_PLACEMENT_3D ( 'NONE', #15475, #54985, #1303 ) ;
#38026 = CARTESIAN_POINT ( 'NONE',  ( 165.0509870607838252, 244.7702999017660375, -2.356357909806504392 ) ) ;
#38027 = CARTESIAN_POINT ( 'NONE',  ( 188.6625213059338932, 268.1393303463237885, 13.54573900311840084 ) ) ;
#38028 = DIRECTION ( 'NONE',  ( 0.000000000000000000, -0.000000000000000000, -1.000000000000000000 ) ) ;
#38029 = CARTESIAN_POINT ( 'NONE',  ( 179.7179132322487192, 263.0089460524625906, -13.84971012364866638 ) ) ;
#38030 = APPLICATION_PROTOCOL_DEFINITION ( 'draft international standard', 'automotive_design', 1998, #5180 ) ;
#38031 = CARTESIAN_POINT ( 'NONE',  ( 15.62557774837418023, 29.99752408145591076, 5.678558825948277544 ) ) ;
#38032 = CARTESIAN_POINT ( 'NONE',  ( 189.8136646974935786, 301.8800841035353528, -0.6430783927310335102 ) ) ;
#38033 = CARTESIAN_POINT ( 'NONE',  ( 71.62614020371384527, 59.05562564738432485, 15.84271347433855937 ) ) ;
#38034 = CARTESIAN_POINT ( 'NONE',  ( 155.4216552449402684, 261.4487918497463284, 18.51722274565528892 ) ) ;
#38035 = VERTEX_POINT ( 'NONE', #44009 ) ;
#38036 = LINE ( 'NONE', #20894, #35046 ) ;
#38037 = DIRECTION ( 'NONE',  ( 0.000000000000000000, 0.000000000000000000, -1.000000000000000000 ) ) ;
#38038 = CARTESIAN_POINT ( 'NONE',  ( 75.30812353949326621, 53.54509013300328490, -16.04758382930608462 ) ) ;
#38039 = CYLINDRICAL_SURFACE ( 'NONE', #54930, 12.49999999999999645 ) ;
#38040 = EDGE_CURVE ( 'NONE', #65090, #42238, #92531, .T. ) ;
#38041 = ORIENTED_EDGE ( 'NONE', *, *, #91233, .F. ) ;
#38042 = CYLINDRICAL_SURFACE ( 'NONE', #68409, 16.60714546451156792 ) ;
#38043 = CARTESIAN_POINT ( 'NONE',  ( 70.87177484439632735, 71.18736215039216120, -3.328809516792729628 ) ) ;
#38044 = CARTESIAN_POINT ( 'NONE',  ( 76.54127139839069116, 63.71106849112843662, 14.88784118061668060 ) ) ;
#38045 = CARTESIAN_POINT ( 'NONE',  ( 86.37830602736983110, 44.06976214698578076, 6.283005621740559654 ) ) ;
#38046 = VERTEX_POINT ( 'NONE', #61672 ) ;
#38047 = VERTEX_POINT ( 'NONE', #7998 ) ;
#38048 = EDGE_CURVE ( 'NONE', #26850, #40206, #47805, .T. ) ;
#38050 = CARTESIAN_POINT ( 'NONE',  ( 87.75883572471174432, 43.84347704570461701, 0.1997593521038640851 ) ) ;
#38049 = CARTESIAN_POINT ( 'NONE',  ( -22.42236680055709641, 157.8615022471902591, 0.000000000000000000 ) ) ;
#38051 = ORIENTED_EDGE ( 'NONE', *, *, #59259, .T. ) ;
#38052 = CARTESIAN_POINT ( 'NONE',  ( 201.1388841337167435, 282.2642286331299601, -18.17233400608081340 ) ) ;
#38053 = CARTESIAN_POINT ( 'NONE',  ( 72.29580736936866003, 70.47844812545214666, 8.033860781394157158 ) ) ;
#38054 = CARTESIAN_POINT ( 'NONE',  ( 80.17048798456011127, 57.79824262504149601, 16.60278798193533589 ) ) ;
#38055 = CARTESIAN_POINT ( 'NONE',  ( 163.8003088823192286, 260.8948240748503054, -17.39314492925268141 ) ) ;
#38056 = VERTEX_POINT ( 'NONE', #13602 ) ;
#38057 = CARTESIAN_POINT ( 'NONE',  ( 147.6857584380539095, 274.8477581613835810, 8.112022437684441201 ) ) ;
#38058 = EDGE_CURVE ( 'NONE', #89714, #24132, #3180, .T. ) ;
#38059 = ORIENTED_EDGE ( 'NONE', *, *, #45133, .T. ) ;
#38060 = CARTESIAN_POINT ( 'NONE',  ( 157.1837449796689725, 258.3967629017010381, 16.97243084443542216 ) ) ;
#38061 = EDGE_CURVE ( 'NONE', #17145, #58533, #99203, .T. ) ;
#38062 = CARTESIAN_POINT ( 'NONE',  ( 158.1203932377468107, 265.1298614022592801, 17.32494200193550071 ) ) ;
#38063 = EDGE_LOOP ( 'NONE', ( #22249, #20002, #94834, #72260 ) ) ;
#38064 = LINE ( 'NONE', #68978, #5042 ) ;
#38065 = CARTESIAN_POINT ( 'NONE',  ( 78.22211991000880005, 47.46001686969969313, -14.34986434894588037 ) ) ;
#38066 = ORIENTED_EDGE ( 'NONE', *, *, #92641, .T. ) ;
#38067 = CARTESIAN_POINT ( 'NONE',  ( -5.322652039529478962, 75.81237378679655592, 14.51925131820462944 ) ) ;
#38068 = CARTESIAN_POINT ( 'NONE',  ( 159.5199931099367063, 254.7822369541973728, 15.51695619349162669 ) ) ;
#38069 = DIRECTION ( 'NONE',  ( -1.000000000000000000, 0.000000000000000000, 0.000000000000000000 ) ) ;
#38070 = VECTOR ( 'NONE', #77227, 1000.000000000000000 ) ;
#38071 = CARTESIAN_POINT ( 'NONE',  ( 83.73227335166906471, 52.23299626358674175, 14.68463506771709071 ) ) ;
#38072 = ORIENTED_EDGE ( 'NONE', *, *, #38842, .F. ) ;
#38073 = EDGE_LOOP ( 'NONE', ( #3792, #94784, #30616, #97817 ) ) ;
#38074 = CARTESIAN_POINT ( 'NONE',  ( 86.91531864373632743, 46.48574869114507635, 8.998937368789745150 ) ) ;
#38075 = CARTESIAN_POINT ( 'NONE',  ( 3.330649899756923382, 26.67094063374350554, 10.00000000000000000 ) ) ;
#38076 = CARTESIAN_POINT ( 'NONE',  ( 148.1672759425158290, 274.0137453789218398, 7.847779094015780110 ) ) ;
#38077 = CARTESIAN_POINT ( 'NONE',  ( 190.8138402884741254, 300.1477291634665789, 4.037153726988762514 ) ) ;
#38078 = CARTESIAN_POINT ( 'NONE',  ( 170.6169145365665827, 275.3029056381844271, -16.38693344838593191 ) ) ;
#38079 = CARTESIAN_POINT ( 'NONE',  ( 191.6193632569555803, 298.7525224553929206, 9.793282278935404150 ) ) ;
#38080 = CARTESIAN_POINT ( 'NONE',  ( 191.8210230231139803, 298.4032374945642232, -8.800268167321144475 ) ) ;
#38081 = CARTESIAN_POINT ( 'NONE',  ( 162.8769348986911609, 257.5139437324259006, 15.59328385742420231 ) ) ;
#38082 = CYLINDRICAL_SURFACE ( 'NONE', #67234, 17.82106496071139645 ) ;
#38084 = FACE_OUTER_BOUND ( 'NONE', #71846, .T. ) ;
#38083 = CARTESIAN_POINT ( 'NONE',  ( 149.1939152435731728, 272.2355539484436235, -11.44223522189843933 ) ) ;
#38085 = CARTESIAN_POINT ( 'NONE',  ( 67.13662373189187349, 66.66751012937585585, 8.328433812688242455 ) ) ;
#38086 = CARTESIAN_POINT ( 'NONE',  ( 168.3980180112511391, 286.3881167737972646, 4.061716199848717679 ) ) ;
#38087 = ORIENTED_EDGE ( 'NONE', *, *, #94717, .F. ) ;
#38088 = AXIS2_PLACEMENT_3D ( 'NONE', #78843, #94064, #9426 ) ;
#38089 = CARTESIAN_POINT ( 'NONE',  ( 190.8340530982597727, 300.1127195499541926, -4.121419783134655290 ) ) ;
#38090 = CARTESIAN_POINT ( 'NONE',  ( 71.10715990604394676, 67.46059230156090791, 10.27172394241540587 ) ) ;
#38091 = CARTESIAN_POINT ( 'NONE',  ( 148.8084825648000731, 273.2965378644469183, 9.141718298254820851 ) ) ;
#38092 = CARTESIAN_POINT ( 'NONE',  ( 79.59581904190152102, 45.85957369269166861, 12.92145696107577280 ) ) ;
#38093 = CIRCLE ( 'NONE', #88381, 70.00000000000001421 ) ;
#38094 = CARTESIAN_POINT ( 'NONE',  ( 191.7051687561719575, 297.9732336099989425, -9.478784037103174853 ) ) ;
#38095 = CARTESIAN_POINT ( 'NONE',  ( 80.36388009702766055, 54.35699232560062910, -16.24410003110130418 ) ) ;
#38096 = CARTESIAN_POINT ( 'NONE',  ( 169.0953906076103692, 285.0085978602089654, -7.951903769486427187 ) ) ;
#38097 = VERTEX_POINT ( 'NONE', #6982 ) ;
#38098 = CARTESIAN_POINT ( 'NONE',  ( 207.6163508138795635, 271.0449272387537576, -1.385071889578343152 ) ) ;
#38099 = CARTESIAN_POINT ( 'NONE',  ( 159.5050723400634638, 254.3761059724978679, -15.34938048045353298 ) ) ;
#38100 = CARTESIAN_POINT ( 'NONE',  ( 72.27036641034979425, 71.53639658761527187, 5.041488442294285832 ) ) ;
#38101 = CARTESIAN_POINT ( 'NONE',  ( 50.59440005247052596, 190.0177522451418213, 5.000000000000051514 ) ) ;
#38102 = CARTESIAN_POINT ( 'NONE',  ( 123.3136442261515526, 235.8768266524159856, 9.188101187500096856 ) ) ;
#38103 = CARTESIAN_POINT ( 'NONE',  ( 180.2882253864519839, 294.9333264195223592, -3.538453439748629137 ) ) ;
#38104 = CARTESIAN_POINT ( 'NONE',  ( 66.71384051412610461, 67.45816284232765270, -6.613419748436212053 ) ) ;
#38105 = CARTESIAN_POINT ( 'NONE',  ( 157.8092552871339365, 257.3133472685137235, 17.04082256169242626 ) ) ;
#38106 = CARTESIAN_POINT ( 'NONE',  ( 175.1838294155237463, 253.3695104272607352, -3.877482245682918105 ) ) ;
#38107 = CARTESIAN_POINT ( 'NONE',  ( 43.80151329331025067, 196.0958772461660544, -9.188101187500095079 ) ) ;
#38108 = CARTESIAN_POINT ( 'NONE',  ( 82.31861562935819165, 40.66747216598101033, 3.229644762565942795 ) ) ;
#38109 = CARTESIAN_POINT ( 'NONE',  ( 50.06890205215324130, 99.29708757740752390, 177.5919119679930134 ) ) ;
#38110 = ORIENTED_EDGE ( 'NONE', *, *, #47652, .T. ) ;
#38111 = CARTESIAN_POINT ( 'NONE',  ( 196.4030970371012472, 264.3490001850324234, -4.693669024083267693 ) ) ;
#38112 = CARTESIAN_POINT ( 'NONE',  ( 179.2088379982556035, 266.5293678400578301, 15.13748914936972589 ) ) ;
#38113 = CARTESIAN_POINT ( 'NONE',  ( 30.34687108590969373, 93.06504152958497400, 60.00000000000000000 ) ) ;
#38114 = CARTESIAN_POINT ( 'NONE',  ( 147.5177358149801421, 275.1387818813681179, 4.867883209065928085 ) ) ;
#38115 = DIRECTION ( 'NONE',  ( 0.3975764696564279554, -0.6886226453387660484, -0.6064089404866747079 ) ) ;
#38116 = PLANE ( 'NONE',  #4203 ) ;
#38117 = CARTESIAN_POINT ( 'NONE',  ( 181.0193311394079103, 261.5502185760933003, 13.24438261311760812 ) ) ;
#38118 = CARTESIAN_POINT ( 'NONE',  ( 119.8042635715769251, 226.6427522451417644, 1.119607411625061291E-15 ) ) ;
#38119 = DIRECTION ( 'NONE',  ( -0.8660254037844359321, -0.5000000000000051070, -0.000000000000000000 ) ) ;
#38120 = ORIENTED_EDGE ( 'NONE', *, *, #51194, .T. ) ;
#38121 = EDGE_CURVE ( 'NONE', #39829, #45578, #3448, .T. ) ;
#38122 = CARTESIAN_POINT ( 'NONE',  ( 158.7770781770005044, 282.1650295664360897, -1.628693105680839359 ) ) ;
#38123 = CARTESIAN_POINT ( 'NONE',  ( 82.45677405825341566, 47.10285889642413792, -12.64402151228549620 ) ) ;
#38124 = VECTOR ( 'NONE', #42477, 1000.000000000000000 ) ;
#38125 = CARTESIAN_POINT ( 'NONE',  ( 35.79112540406921283, 179.2202760586659736, -5.415160957724236172E-17 ) ) ;
#38126 = CARTESIAN_POINT ( 'NONE',  ( 3.886609837484615859, 24.01751292744054211, 6.180339887498949913 ) ) ;
#38127 = CARTESIAN_POINT ( 'NONE',  ( 192.1384501294028553, 272.2803415673531049, 15.07942017704054471 ) ) ;
#38128 = CARTESIAN_POINT ( 'NONE',  ( 71.85869513609317494, 58.67586711399007982, -15.48493562761568576 ) ) ;
#38129 = CARTESIAN_POINT ( 'NONE',  ( 73.04738217724886340, 69.71546789186045601, 9.669594540409617522 ) ) ;
#38131 = CARTESIAN_POINT ( 'NONE',  ( 66.48072710279772934, 203.0643266524160424, 9.188101187500095079 ) ) ;
#38130 = CARTESIAN_POINT ( 'NONE',  ( 195.7949008739993531, 275.8773930737895057, -15.42861398852914512 ) ) ;
#38132 = CARTESIAN_POINT ( 'NONE',  ( 200.1662314894802819, 283.9489124310637180, 17.19420058542677054 ) ) ;
#38133 = CARTESIAN_POINT ( 'NONE',  ( 72.68285417969771345, 57.18103607157792823, 15.88118435539451490 ) ) ;
#38134 = EDGE_CURVE ( 'NONE', #42320, #93829, #15143, .T. ) ;
#38135 = PLANE ( 'NONE',  #24605 ) ;
#38136 = ORIENTED_EDGE ( 'NONE', *, *, #8614, .F. ) ;
#38137 = VECTOR ( 'NONE', #60284, 1000.000000000000114 ) ;
#38138 = ADVANCED_FACE ( 'NONE', ( #93618 ), #87565, .F. ) ;
#38139 = CARTESIAN_POINT ( 'NONE',  ( 161.9943004083856408, 267.2312384411657149, 16.48735601444852961 ) ) ;
#38140 = CARTESIAN_POINT ( 'NONE',  ( 16.11576366785047654, 170.1115022471901739, -5.000000000000041744 ) ) ;
#38141 = CARTESIAN_POINT ( 'NONE',  ( 207.8060684685902686, 270.7163266217015689, 2.015725026008670540 ) ) ;
#38142 = CARTESIAN_POINT ( 'NONE',  ( 137.8192226437758450, 256.5024278399160949, -9.188101187500093303 ) ) ;
#38143 = CARTESIAN_POINT ( 'NONE',  ( 34.67812306484450602, 22.94754757982092030, 5.678558825948272215 ) ) ;
#38144 = CARTESIAN_POINT ( 'NONE',  ( 164.0729100755626746, 260.4632643121815363, -16.14824515792620829 ) ) ;
#38145 = CARTESIAN_POINT ( 'NONE',  ( 185.7793147125802875, 260.5841321348162865, 6.335720874329757279 ) ) ;
#38146 = CARTESIAN_POINT ( 'NONE',  ( 74.95826842568676796, 53.11571732367104204, -16.02841466325640951 ) ) ;
#38148 = DIRECTION ( 'NONE',  ( 0.000000000000000000, 0.000000000000000000, 1.000000000000000000 ) ) ;
#38147 = CARTESIAN_POINT ( 'NONE',  ( 88.47356364199694667, 43.97712956045979382, 1.870819122003384516 ) ) ;
#38149 = CARTESIAN_POINT ( 'NONE',  ( 68.82743466988767977, 64.08478545733547094, 12.03889531702951565 ) ) ;
#38150 = ORIENTED_EDGE ( 'NONE', *, *, #64625, .T. ) ;
#38151 = CARTESIAN_POINT ( 'NONE',  ( 80.90513341749731069, 49.79037932115560494, 14.73721116675313603 ) ) ;
#38152 =( NAMED_UNIT ( * ) PLANE_ANGLE_UNIT ( ) SI_UNIT ( $, .RADIAN. ) );
#38153 = CARTESIAN_POINT ( 'NONE',  ( 179.5572819769699606, 286.1165802574137160, 13.07273523577711138 ) ) ;
#38154 = CARTESIAN_POINT ( 'NONE',  ( 156.6893878665337638, 280.2375996934318323, -5.371908398693758357 ) ) ;
#38155 = CARTESIAN_POINT ( 'NONE',  ( 5.010160986809694350, 24.93396525600388003, 2.839279412974139660 ) ) ;
#38156 = VERTEX_POINT ( 'NONE', #79433 ) ;
#38157 = LINE ( 'NONE', #53377, #32765 ) ;
#38158 = DIRECTION ( 'NONE',  ( 0.4330127018922138582, 0.2500000000000087153, 0.8660254037844388186 ) ) ;
#38159 = AXIS2_PLACEMENT_3D ( 'NONE', #12094, #43963, #34873 ) ;
#38160 = CARTESIAN_POINT ( 'NONE',  ( 49.04287251715432205, 95.72274150194785136, -10.00000000000000000 ) ) ;
#38161 = CARTESIAN_POINT ( 'NONE',  ( 200.5812521528945638, 281.4385583276488205, -17.14082239954941755 ) ) ;
#38162 = CARTESIAN_POINT ( 'NONE',  ( 74.81832046901195099, 67.48663194201290594, -12.71244991431774984 ) ) ;
#38163 = AXIS2_PLACEMENT_3D ( 'NONE', #12373, #51344, #27577 ) ;
#38164 = CARTESIAN_POINT ( 'NONE',  ( 208.3764315856425640, 269.7284287242038658, -1.833640725398759441 ) ) ;
#38165 = DIRECTION ( 'NONE',  ( -3.755686162884236985E-16, 8.056116744242159655E-32, 1.000000000000000000 ) ) ;
#38166 = VERTEX_POINT ( 'NONE', #1895 ) ;
#38167 = ADVANCED_FACE ( 'NONE', ( #55069 ), #55560, .T. ) ;
#38168 = CARTESIAN_POINT ( 'NONE',  ( 190.9259979929221913, 280.9477547779517863, 16.64741033664369141 ) ) ;
#38169 = CARTESIAN_POINT ( 'NONE',  ( 167.0957737472305666, 246.8272050136007749, 1.963998143010642128 ) ) ;
#38170 = EDGE_LOOP ( 'NONE', ( #78769, #82303, #9697, #71269 ) ) ;
#38171 = CARTESIAN_POINT ( 'NONE',  ( 149.0761751337341821, 272.4394858007734683, 11.56094486755886130 ) ) ;
#38172 = CARTESIAN_POINT ( 'NONE',  ( 6.406750531224583156, 186.0530062829863027, -4.648177544792955347E-16 ) ) ;
#38173 = CARTESIAN_POINT ( 'NONE',  ( 81.71554479561422113, 45.45142740597917452, -10.99315133951941093 ) ) ;
#38174 = ORIENTED_EDGE ( 'NONE', *, *, #86110, .T. ) ;
#38175 = CARTESIAN_POINT ( 'NONE',  ( 162.7435819479956933, 250.7668427907593411, -13.06080741167749082 ) ) ;
#38176 = CARTESIAN_POINT ( 'NONE',  ( 79.31967116076748425, 59.78699023733838658, -16.51284638439523533 ) ) ;
#38177 = B_SPLINE_CURVE_WITH_KNOTS ( 'NONE', 3,
 ( #57117, #57619, #96674, #3934 ),
 .UNSPECIFIED., .F., .F.,
 ( 4, 4 ),
 ( 0.03227822889357200020, 0.04124890145165294175 ),
 .UNSPECIFIED. ) ;
#38178 = CARTESIAN_POINT ( 'NONE',  ( 8.736352098677466316, 26.81751292744054638, -6.180339887498951690 ) ) ;
#38179 = CARTESIAN_POINT ( 'NONE',  ( 66.29454943693275482, 69.24199052626691753, -2.144636311159408226 ) ) ;
#38180 = CARTESIAN_POINT ( 'NONE',  ( 69.48618880206072390, 62.61793869292603176, 13.29615132219218765 ) ) ;
#38181 = VERTEX_POINT ( 'NONE', #48992 ) ;
#38182 = CARTESIAN_POINT ( 'NONE',  ( 102.3121810886139116, 236.0024278399160949, 9.188101187500095079 ) ) ;
#38183 = CARTESIAN_POINT ( 'NONE',  ( 200.2690241097007799, 283.7708703901988656, 16.96680019208369927 ) ) ;
#38184 = CARTESIAN_POINT ( 'NONE',  ( 73.38460905275829305, 69.71371501254900238, -9.902851190597802500 ) ) ;
#38185 = CARTESIAN_POINT ( 'NONE',  ( 181.2482315834775477, 271.4898918969783495, -16.12830051190350034 ) ) ;
#38186 = CARTESIAN_POINT ( 'NONE',  ( 81.45028675782795347, 42.16027941493478437, -7.981823387058465613 ) ) ;
#38187 = ORIENTED_EDGE ( 'NONE', *, *, #4394, .F. ) ;
#38188 = EDGE_CURVE ( 'NONE', #33639, #8542, #74407, .T. ) ;
#38189 = VERTEX_POINT ( 'NONE', #89538 ) ;
#38190 = EDGE_LOOP ( 'NONE', ( #75328, #58654, #12349 ) ) ;
#38191 = CARTESIAN_POINT ( 'NONE',  ( 80.61656135465395323, 47.24360202468593428, 12.89152188940151333 ) ) ;
#38192 = ORIENTED_EDGE ( 'NONE', *, *, #74763, .T. ) ;
#38193 = CARTESIAN_POINT ( 'NONE',  ( 69.15891061406161100, 69.66865021447996753, 4.956695084876229451 ) ) ;
#38194 = ORIENTED_EDGE ( 'NONE', *, *, #46570, .F. ) ;
#38195 = CARTESIAN_POINT ( 'NONE',  ( 208.3135187673106543, 269.8373969220020285, 2.829653198597726682 ) ) ;
#38196 = CARTESIAN_POINT ( 'NONE',  ( 190.8429499865819707, 278.0757709512191695, -17.64141544901220371 ) ) ;
#38197 = CARTESIAN_POINT ( 'NONE',  ( 171.0593044012981068, 283.5750802371461532, 12.19867815159854807 ) ) ;
#38198 = CARTESIAN_POINT ( 'NONE',  ( 194.2223991963907963, 294.2439319543634610, -14.97294938100067441 ) ) ;
#38199 = CARTESIAN_POINT ( 'NONE',  ( 68.90154995574886243, 68.41372695714582619, -7.258461826296537467 ) ) ;
#38200 = CARTESIAN_POINT ( 'NONE',  ( 200.0411626275569574, 270.6720010161316736, -11.59284015024147152 ) ) ;
#38201 = CARTESIAN_POINT ( 'NONE',  ( 16.48196734934595753, 24.91421378149918198, 9.188101187500008038 ) ) ;
#38202 = VECTOR ( 'NONE', #87171, 1000.000000000000114 ) ;
#38203 = CARTESIAN_POINT ( 'NONE',  ( 163.4923624983613024, 282.7451307114477572, 8.800724806903520658 ) ) ;
#38204 = CARTESIAN_POINT ( 'NONE',  ( 80.05322980421331636, 57.68292478952278657, 16.60179730502024142 ) ) ;
#38206 = EDGE_LOOP ( 'NONE', ( #52265, #74891, #78582, #35079 ) ) ;
#38205 = CARTESIAN_POINT ( 'NONE',  ( -41.47773752187638507, 44.74077244691897448, 59.99999999999999289 ) ) ;
#38207 = CIRCLE ( 'NONE', #83613, 49.99999999999999289 ) ;
#38208 = CARTESIAN_POINT ( 'NONE',  ( 202.9972156839127990, 279.0455039708822937, 16.77197898838388213 ) ) ;
#38209 = FACE_OUTER_BOUND ( 'NONE', #53522, .T. ) ;
#38210 = CARTESIAN_POINT ( 'NONE',  ( 77.47822618113920612, 49.74927637487309084, -15.48360864196420295 ) ) ;
#38211 = VECTOR ( 'NONE', #42442, 1000.000000000000114 ) ;
#38212 = CARTESIAN_POINT ( 'NONE',  ( 180.3515574791316283, 255.6186696229350446, 6.159525720347461153 ) ) ;
#38213 = ADVANCED_FACE ( 'NONE', ( #74314 ), #49986, .F. ) ;
#38214 = DIRECTION ( 'NONE',  ( 0.3473291852294957405, -0.6015917957689906892, 0.7193398003386545225 ) ) ;
#38215 = CARTESIAN_POINT ( 'NONE',  ( 194.7902205010250043, 263.3917080119609295, -0.7864463132427590430 ) ) ;
#38216 = ORIENTED_EDGE ( 'NONE', *, *, #2178, .F. ) ;
#38217 = CARTESIAN_POINT ( 'NONE',  ( 194.0373855506731502, 294.5643849888401746, -14.18241207909759538 ) ) ;
#38218 = CARTESIAN_POINT ( 'NONE',  ( 75.36609510305467552, 62.13380695430679168, -15.15412763540104102 ) ) ;
#38220 = EDGE_CURVE ( 'NONE', #55654, #83576, #88544, .T. ) ;
#38219 = LINE ( 'NONE', #46840, #62937 ) ;
#38221 = CARTESIAN_POINT ( 'NONE',  ( 5.561079055679667427, 174.0177522451418781, -10.00000000000009592 ) ) ;
#38222 = CARTESIAN_POINT ( 'NONE',  ( 82.85511220885132389, 53.72155160612705060, -15.38925759434244434 ) ) ;
#38223 = CARTESIAN_POINT ( 'NONE',  ( 174.5125536636238621, 282.4638039902177979, -14.82547868367492327 ) ) ;
#38224 = CARTESIAN_POINT ( 'NONE',  ( 203.6765436393997675, 277.8688734369772533, -15.81082241283986178 ) ) ;
#38225 = CARTESIAN_POINT ( 'NONE',  ( 72.01470311467906527, 72.29437185155289569, 0.6840695740065164676 ) ) ;
#38226 = CARTESIAN_POINT ( 'NONE',  ( 178.6423073663378602, 290.9544255387157818, 10.03153667033594765 ) ) ;
#38228 = CARTESIAN_POINT ( 'NONE',  ( 24.30227344809185652, 37.52903772873359856, -1.583844403245329602 ) ) ;
#38227 = CARTESIAN_POINT ( 'NONE',  ( -7.212535326543083158, 157.4548013555409796, -4.594050593750042211 ) ) ;
#38229 = CARTESIAN_POINT ( 'NONE',  ( 185.2391986358457530, 295.7873944733689768, 8.585680893828113724 ) ) ;
#38230 = ORIENTED_EDGE ( 'NONE', *, *, #98832, .T. ) ;
#38231 = VECTOR ( 'NONE', #37093, 1000.000000000000000 ) ;
#38232 = VERTEX_POINT ( 'NONE', #11510 ) ;
#38233 = CARTESIAN_POINT ( 'NONE',  ( 151.9857020112045802, 279.0317921242573789, 1.822192154687843457 ) ) ;
#38234 = DIRECTION ( 'NONE',  ( 0.5000000000000013323, -0.8660254037844378194, 0.000000000000000000 ) ) ;
#38235 = CARTESIAN_POINT ( 'NONE',  ( 79.14312167556931854, 57.64441083166269664, 0.000000000000000000 ) ) ;
#38236 = AXIS2_PLACEMENT_3D ( 'NONE', #33298, #72833, #89551 ) ;
#38237 = LINE ( 'NONE', #30669, #25890 ) ;
#38238 = CARTESIAN_POINT ( 'NONE',  ( 162.6464992788258144, 248.9349949062956284, -10.29443606917336496 ) ) ;
#38239 = CARTESIAN_POINT ( 'NONE',  ( 71.46708483896914288, 71.41611121499917658, 5.261356510684446874 ) ) ;
#38240 = CARTESIAN_POINT ( 'NONE',  ( 150.1971333718279880, 276.5536166081793112, 3.687813122935997168 ) ) ;
#38241 = CARTESIAN_POINT ( 'NONE',  ( 25.93973934025619599, 185.7833772461660544, -9.188101187500095079 ) ) ;
#38242 = CARTESIAN_POINT ( 'NONE',  ( 116.0331843058823296, 246.9869531367911293, 4.594050593750046652 ) ) ;
#38243 = CARTESIAN_POINT ( 'NONE',  ( 181.2440676231241241, 294.5520841294345473, -6.623935519155441654 ) ) ;
#38244 = CARTESIAN_POINT ( 'NONE',  ( 196.0931812089658592, 275.1780562578900913, 15.95755391823183444 ) ) ;
#38245 = CYLINDRICAL_SURFACE ( 'NONE', #2823, 17.82106496071139645 ) ;
#38246 = B_SPLINE_CURVE_WITH_KNOTS ( 'NONE', 3,
 ( #51204, #3160, #34045, #64935 ),
 .UNSPECIFIED., .F., .F.,
 ( 4, 4 ),
 ( 0.005339423476618587738, 0.01094292413399224062 ),
 .UNSPECIFIED. ) ;
#38247 = FACE_OUTER_BOUND ( 'NONE', #81888, .T. ) ;
#38248 = CARTESIAN_POINT ( 'NONE',  ( 76.94717320005119632, 54.64271564352422672, -16.08472187958355448 ) ) ;
#38249 = CARTESIAN_POINT ( 'NONE',  ( -19.65312891409030271, 93.06504152958497400, 10.00000000000000888 ) ) ;
#38250 = CARTESIAN_POINT ( 'NONE',  ( 68.74472142891936244, 63.88220321458977224, -12.16134622803817500 ) ) ;
#38251 = DIRECTION ( 'NONE',  ( -0.8660254037844387076, -0.4999999999999998890, -0.000000000000000000 ) ) ;
#38252 = CARTESIAN_POINT ( 'NONE',  ( 82.13428468617439648, 46.48939983997102132, 12.30969175005605898 ) ) ;
#38253 = CARTESIAN_POINT ( 'NONE',  ( 49.54000814145098275, 103.6626726051169669, 177.5919119679930134 ) ) ;
#38254 = CARTESIAN_POINT ( 'NONE',  ( 71.89619214677514947, 64.26066769777372656, 13.73780722179543901 ) ) ;
#38255 = CARTESIAN_POINT ( 'NONE',  ( 171.3829901640632443, 279.8345946159657274, 13.89615929642840619 ) ) ;
#38256 = CARTESIAN_POINT ( 'NONE',  ( 19.94070920123167312, 188.9865022471903160, -10.00000000000009592 ) ) ;
#38257 = EDGE_CURVE ( 'NONE', #47538, #87383, #54679, .T. ) ;
#38258 = CARTESIAN_POINT ( 'NONE',  ( 69.70445039019863032, 69.81249935811580087, 5.371585936356678914 ) ) ;
#38259 = CARTESIAN_POINT ( 'NONE',  ( 207.3343352015242829, 271.1099079521872000, 2.793079588467688001 ) ) ;
#38260 = CARTESIAN_POINT ( 'NONE',  ( 180.8886733632373591, 266.5746820064321128, -14.68068468162151596 ) ) ;
#38261 = ORIENTED_EDGE ( 'NONE', *, *, #83999, .T. ) ;
#38262 = CARTESIAN_POINT ( 'NONE',  ( 75.28801175639888754, 63.39411007085420380, 15.10357975279682741 ) ) ;
#38263 = EDGE_CURVE ( 'NONE', #1077, #9692, #57958, .T. ) ;
#38264 = B_SPLINE_CURVE_WITH_KNOTS ( 'NONE', 3,
 ( #71719, #9395, #10402, #2310 ),
 .UNSPECIFIED., .F., .F.,
 ( 4, 4 ),
 ( 0.0001948154735252194804, 0.0003149152481875766942 ),
 .UNSPECIFIED. ) ;
#38266 = EDGE_CURVE ( 'NONE', #8436, #41607, #26683, .T. ) ;
#38265 = CARTESIAN_POINT ( 'NONE',  ( 184.4241326561383403, 269.4503056644531966, 15.31856924807197196 ) ) ;
#38267 = ADVANCED_FACE ( 'NONE', ( #73790 ), #98092, .T. ) ;
#38268 = CARTESIAN_POINT ( 'NONE',  ( 87.34609280552280097, 230.4244531367911009, -4.594050593750046652 ) ) ;
#38269 = CARTESIAN_POINT ( 'NONE',  ( 7.926391159377050855, 27.68290643055185285, 3.479690158560446702E-15 ) ) ;
#38270 = CARTESIAN_POINT ( 'NONE',  ( -7.266922234329370234, 156.6115022471902023, -5.000000000000041744 ) ) ;
#38271 = CARTESIAN_POINT ( 'NONE',  ( 66.10780414051450293, 68.63670250712272036, 1.777645618418523865 ) ) ;
#38273 = CARTESIAN_POINT ( 'NONE',  ( 195.6708441445795756, 278.3169109478037626, 17.04649191961062726 ) ) ;
#38272 = CARTESIAN_POINT ( 'NONE',  ( 157.4177733328310467, 257.9914139036126812, 18.29188238796808363 ) ) ;
#38274 = CARTESIAN_POINT ( 'NONE',  ( 201.4550628388361417, 270.3106342360672443, -10.24027999735716854 ) ) ;
#38275 = CARTESIAN_POINT ( 'NONE',  ( 181.5558742819051474, 255.2544784655372894, -2.503599602330015994 ) ) ;
#38276 = FACE_OUTER_BOUND ( 'NONE', #25124, .T. ) ;
#38277 = AXIS2_PLACEMENT_3D ( 'NONE', #25705, #10003, #40867 ) ;
#38278 = CARTESIAN_POINT ( 'NONE',  ( 33.90715327291019321, 42.68290643055190259, 3.479690158560446702E-15 ) ) ;
#38279 = CARTESIAN_POINT ( 'NONE',  ( 43.54162044069033755, 26.10801979619932567, 3.090169943749476733 ) ) ;
#38280 = CARTESIAN_POINT ( 'NONE',  ( 7.313483791488072150, 163.4824982072973683, 3.021315404115420679E-15 ) ) ;
#38281 = VERTEX_POINT ( 'NONE', #3409 ) ;
#38282 = CARTESIAN_POINT ( 'NONE',  ( 27.91230638117223606, 28.06628583063842797, -9.188101187500006262 ) ) ;
#38283 = CARTESIAN_POINT ( 'NONE',  ( 178.5040461245142183, 280.6592112227464213, 16.58436230249095189 ) ) ;
#38284 = AXIS2_PLACEMENT_3D ( 'NONE', #34951, #71981, #10179 ) ;
#38285 = CARTESIAN_POINT ( 'NONE',  ( 196.6512732745314906, 267.5067273676284003, 9.687024394805378691 ) ) ;
#38286 = CARTESIAN_POINT ( 'NONE',  ( 65.93257831369518840, 197.3262482093457777, 3.021315404115420679E-15 ) ) ;
#38287 = VERTEX_POINT ( 'NONE', #73297 ) ;
#38288 = B_SPLINE_SURFACE_WITH_KNOTS ( 'NONE', 3, 1, ( 
 ( #74521, #35980 ),
 ( #74010, #34493 ),
 ( #50194, #65395 ),
 ( #42574, #26904 ),
 ( #96839, #57783 ),
 ( #19812, #81146 ),
 ( #50680, #28899 ),
 ( #82652, #13211 ),
 ( #66884, #4595 ),
 ( #19332, #81635 ),
 ( #28383, #58771 ),
 ( #35489, #75009 ),
 ( #89742, #20306 ),
 ( #4091, #5589 ),
 ( #65886, #52176 ),
 ( #51179, #100214 ),
 ( #77402, #85547 ),
 ( #86551, #38375 ),
 ( #1902, #54069 ),
 ( #8008, #16587 ),
 ( #394, #61679 ),
 ( #23670, #23178 ),
 ( #32781, #38880 ),
 ( #47483, #15569 ),
 ( #54562, #92629 ),
 ( #47973, #17083 ),
 ( #8989, #55075 ),
 ( #78918, #70794 ),
 ( #31282, #63691 ),
 ( #69289, #78408 ),
 ( #85025, #76884 ),
 ( #9505, #16088 ),
 ( #46994, #46473 ),
 ( #69784, #77908 ) ),
 .UNSPECIFIED., .T., .F., .F.,
 ( 4, 2, 2, 2, 2, 2, 2, 2, 2, 2, 2, 2, 2, 2, 2, 2, 4 ),
 ( 2, 2 ),
 ( 0.000000000000000000, 0.06250000000000000000, 0.1250000000000000000, 0.1875000000000000000, 0.2500000000000000000, 0.3125000000000000000, 0.3750000000000000000, 0.4375000000000000000, 0.5000000000000000000, 0.5625000000000000000, 0.6250000000000000000, 0.6875000000000000000, 0.7500000000000000000, 0.8125000000000000000, 0.8750000000000000000, 0.9375000000000000000, 1.000000000000000000 ),
 ( 0.000000000000000000, 1.000000000000000000 ),
 .UNSPECIFIED. ) ;
#38289 = AXIS2_PLACEMENT_3D ( 'NONE', #56912, #34137, #71147 ) ;
#38290 = CARTESIAN_POINT ( 'NONE',  ( 84.76146393123151768, 50.45989236026047564, -13.93701821937661833 ) ) ;
#38291 = CARTESIAN_POINT ( 'NONE',  ( 198.2819808855875863, 287.2125302111982705, 18.53535247371401695 ) ) ;
#38292 = CARTESIAN_POINT ( 'NONE',  ( 183.6672295643515440, 264.5222299264054868, -13.41344130462387518 ) ) ;
#38293 = CARTESIAN_POINT ( 'NONE',  ( 169.4327616935881053, 251.8687907473509711, -8.483257748728734171 ) ) ;
#38294 = CARTESIAN_POINT ( 'NONE',  ( 151.2157266582228772, 248.1115022471902023, -5.000000000000041744 ) ) ;
#38295 = ORIENTED_EDGE ( 'NONE', *, *, #31070, .F. ) ;
#38296 = EDGE_CURVE ( 'NONE', #4844, #7878, #55764, .T. ) ;
#38297 = CARTESIAN_POINT ( 'NONE',  ( 187.5143746346354021, 278.9518094448188776, 17.63296374067274286 ) ) ;
#38298 = CARTESIAN_POINT ( 'NONE',  ( 28.52453836335597614, 34.65586893147758474, -7.433330006724137462 ) ) ;
#38299 = ORIENTED_EDGE ( 'NONE', *, *, #92568, .T. ) ;
#38300 = B_SPLINE_CURVE_WITH_KNOTS ( 'NONE', 3,
 ( #50365, #20484, #3785, #4785, #36152, #88953, #34667, #20992, #28556, #81319, #59437, #34180, #18999, #88439, #66074, #43750 ),
 .UNSPECIFIED., .F., .F.,
 ( 4, 1, 2, 2, 2, 1, 2, 2, 4 ),
 ( 0.000000000000000000, 0.1249999999999949207, 0.1874999999999934219, 0.2499999999999919509, 0.4999999999999922284, 0.6249999999999923395, 0.6874999999999938938, 0.7499999999999954481, 1.000000000000000000 ),
 .UNSPECIFIED. ) ;
#38301 = DIRECTION ( 'NONE',  ( 0.4999999999999992784, -0.8660254037844390407, 0.000000000000000000 ) ) ;
#38302 = CARTESIAN_POINT ( 'NONE',  ( 183.4092525909616711, 291.5038694251641687, -10.73000149755480948 ) ) ;
#38303 = ORIENTED_EDGE ( 'NONE', *, *, #33431, .T. ) ;
#38304 = PLANE ( 'NONE',  #55465 ) ;
#38305 = CARTESIAN_POINT ( 'NONE',  ( 206.2884309622781984, 273.3449518901063584, 11.80432421640126250 ) ) ;
#38306 = CARTESIAN_POINT ( 'NONE',  ( 84.68103419341217375, 50.25510846593720515, 13.84703097836258934 ) ) ;
#38307 = CARTESIAN_POINT ( 'NONE',  ( 153.3658703804616152, 265.0095156844545272, -16.92037735142076826 ) ) ;
#38308 = B_SPLINE_CURVE_WITH_KNOTS ( 'NONE', 3,
 ( #23069, #62061, #99107, #76310 ),
 .UNSPECIFIED., .F., .F.,
 ( 4, 4 ),
 ( 0.001669260644153817410, 0.003387224320680204057 ),
 .UNSPECIFIED. ) ;
#38309 = CARTESIAN_POINT ( 'NONE',  ( 187.4167187180463259, 296.4074041626601002, 9.525756846988903348 ) ) ;
#38310 = CARTESIAN_POINT ( 'NONE',  ( 182.7847760313759409, 280.0284915794045446, -17.53211380394024843 ) ) ;
#38311 = AXIS2_PLACEMENT_3D ( 'NONE', #72011, #25916, #2615 ) ;
#38312 = CARTESIAN_POINT ( 'NONE',  ( 79.95417701789796183, 44.68756451846406463, 11.18129038331146141 ) ) ;
#38313 = CARTESIAN_POINT ( 'NONE',  ( 81.42054145595460568, 55.42004525696071937, -16.32184955832448026 ) ) ;
#38314 = CARTESIAN_POINT ( 'NONE',  ( 76.89034932008942747, 61.82808869569446841, -15.91935783100940860 ) ) ;
#38315 = VERTEX_POINT ( 'NONE', #35780 ) ;
#38316 = CARTESIAN_POINT ( 'NONE',  ( 162.8640727416213281, 249.5241558410263849, 11.11676342424593855 ) ) ;
#38317 = VECTOR ( 'NONE', #42467, 1000.000000000000000 ) ;
#38318 = VERTEX_POINT ( 'NONE', #66673 ) ;
#38319 = VERTEX_POINT ( 'NONE', #97131 ) ;
#38320 = CARTESIAN_POINT ( 'NONE',  ( 87.19297534993042120, 45.95771221245824734, -8.700079422534972906 ) ) ;
#38321 =( BOUNDED_CURVE ( )  B_SPLINE_CURVE ( 2, ( #24615, #55497, #8919, #18916, #78841, #32716, #17010, #63617, #3708 ),
 .UNSPECIFIED., .F., .F. ) 
 B_SPLINE_CURVE_WITH_KNOTS ( ( 3, 2, 2, 2, 3 ),
 ( 0.4879032258064516236, 0.4892473118279569988, 0.4919354838709677491, 0.4946236559139784994, 0.4959677419354838745 ),
 .UNSPECIFIED. ) 
 CURVE ( )  GEOMETRIC_REPRESENTATION_ITEM ( )  RATIONAL_B_SPLINE_CURVE ( ( 0.9330127018922194093, 0.9330127018922194093, 1.000000000000000000, 0.8660254037844387076, 1.000000000000000000, 0.8660254037844387076, 1.000000000000000000, 0.9330127018922194093, 0.9330127018922194093 ) ) 
 REPRESENTATION_ITEM ( '' )  );
#38323 = CARTESIAN_POINT ( 'NONE',  ( 190.5526305594705434, 299.9695577504274979, -4.324655322867677398 ) ) ;
#38322 = CARTESIAN_POINT ( 'NONE',  ( 170.8944053752079810, 255.0871438150282700, -11.36895391432762636 ) ) ;
#38324 = CARTESIAN_POINT ( 'NONE',  ( 164.9402323277223275, 244.9621327266073081, -1.073314903116530106 ) ) ;
#38325 = CARTESIAN_POINT ( 'NONE',  ( 197.4166373598459074, 273.1534249293282528, -13.33078627074450395 ) ) ;
#38326 = CARTESIAN_POINT ( 'NONE',  ( 72.02158190405090465, 61.69589088016835632, -14.52859831159107884 ) ) ;
#38327 = CARTESIAN_POINT ( 'NONE',  ( 82.80357023854472232, 40.61453041052752155, 0.9744293009809118500 ) ) ;
#38328 = CARTESIAN_POINT ( 'NONE',  ( 168.0467845603413366, 249.4717662844409176, -5.469034782820844320 ) ) ;
#38329 = CARTESIAN_POINT ( 'NONE',  ( 77.03509876804180578, 63.43842436480252900, -15.45738776637924516 ) ) ;
#38330 = CARTESIAN_POINT ( 'NONE',  ( 178.1815451042072596, 255.1982646830548447, 5.740691749723041859 ) ) ;
#38331 = CARTESIAN_POINT ( 'NONE',  ( 120.0931990297694085, 230.9548013555409796, -4.594050593750042211 ) ) ;
#38332 = CARTESIAN_POINT ( 'NONE',  ( 187.0608580662972713, 262.1253545432567762, -10.24587999176721276 ) ) ;
#38333 = CARTESIAN_POINT ( 'NONE',  ( 35.31444455405989657, 43.49540643055190969, 3.479690158560446702E-15 ) ) ;
#38334 = CARTESIAN_POINT ( 'NONE',  ( 188.1875818435630663, 273.5226728761291497, 15.67860454874873355 ) ) ;
#38335 = EDGE_CURVE ( 'NONE', #69980, #4020, #96627, .T. ) ;
#38336 = ORIENTED_EDGE ( 'NONE', *, *, #82629, .F. ) ;
#38337 = B_SPLINE_CURVE_WITH_KNOTS ( 'NONE', 3,
 ( #12553, #51534, #74860, #35834, #97180, #52035, #98154, #89591, #5932, #36325, #43426, #20156, #51024, #96682 ),
 .UNSPECIFIED., .F., .F.,
 ( 4, 2, 2, 2, 2, 2, 4 ),
 ( 0.002301009298598415652, 0.002438001431547676037, 0.002574993564496935988, 0.002711985697446196372, 0.002848977830395456323, 0.003396946362192322221, 0.004492883425785989399 ),
 .UNSPECIFIED. ) ;
#38338 = ORIENTED_EDGE ( 'NONE', *, *, #38058, .F. ) ;
#38339 = CARTESIAN_POINT ( 'NONE',  ( 74.02866129013209218, 68.91877476116354728, -11.13505360475025263 ) ) ;
#38340 = CARTESIAN_POINT ( 'NONE',  ( 117.2783561438722586, 238.5177522451418497, -10.00000000000009592 ) ) ;
#38341 = FACE_OUTER_BOUND ( 'NONE', #29521, .T. ) ;
#38342 = CARTESIAN_POINT ( 'NONE',  ( 192.6336181944592454, 296.9957813718090165, 11.10275837363962737 ) ) ;
#38343 = CARTESIAN_POINT ( 'NONE',  ( 190.2204363742943656, 300.4646209966566062, -1.328626404316530739E-11 ) ) ;
#38344 = LINE ( 'NONE', #53549, #15601 ) ;
#38345 = ORIENTED_EDGE ( 'NONE', *, *, #76421, .F. ) ;
#38346 = ORIENTED_EDGE ( 'NONE', *, *, #88883, .F. ) ;
#38347 = CARTESIAN_POINT ( 'NONE',  ( 78.87748066101475786, 48.05297491638317808, 14.45999959637729049 ) ) ;
#38348 = LINE ( 'NONE', #92601, #68944 ) ;
#38349 = VERTEX_POINT ( 'NONE', #28176 ) ;
#38350 = CARTESIAN_POINT ( 'NONE',  ( 80.87517248313827167, 58.64441083166272506, 0.000000000000000000 ) ) ;
#38351 = CARTESIAN_POINT ( 'NONE',  ( 192.5930808083610088, 262.6107660501119199, 4.653369615412138671 ) ) ;
#38352 = CARTESIAN_POINT ( 'NONE',  ( 158.0314954405573644, 263.1485498153232356, 17.26347671721901023 ) ) ;
#38353 = AXIS2_PLACEMENT_3D ( 'NONE', #18230, #86677, #40992 ) ;
#38354 = LINE ( 'NONE', #39838, #25737 ) ;
#38356 = CARTESIAN_POINT ( 'NONE',  ( 160.7022581417230356, 281.5213664053168827, 5.619168078228955920 ) ) ;
#38355 = CARTESIAN_POINT ( 'NONE',  ( 197.8980529691977779, 285.8775128688180871, 17.80711829255526979 ) ) ;
#38357 = CARTESIAN_POINT ( 'NONE',  ( 201.2139346379346705, 282.1342373466909521, -16.65315141107179286 ) ) ;
#38358 = ORIENTED_EDGE ( 'NONE', *, *, #74016, .F. ) ;
#38360 = CARTESIAN_POINT ( 'NONE',  ( 147.5634954182374372, 275.0595239235922236, 4.682022975662822439 ) ) ;
#38359 = AXIS2_PLACEMENT_3D ( 'NONE', #64730, #78951, #4802 ) ;
#38361 = CARTESIAN_POINT ( 'NONE',  ( 73.32924055991662726, 68.54209549527047329, 10.53624946344089786 ) ) ;
#38362 = CARTESIAN_POINT ( 'NONE',  ( 188.2563532189512898, 263.5935347285679313, -9.073490670746114262 ) ) ;
#38363 = CARTESIAN_POINT ( 'NONE',  ( 149.1870424807857489, 245.3932355074535678, -2.679491924311248496 ) ) ;
#38364 = CARTESIAN_POINT ( 'NONE',  ( 192.7286328587738922, 271.7632531150862860, -14.68684183385635933 ) ) ;
#38365 = CARTESIAN_POINT ( 'NONE',  ( 12.56145106960391011, 171.3927522451417929, 10.00000000000009948 ) ) ;
#38366 = CARTESIAN_POINT ( 'NONE',  ( 82.10990542498430500, 41.84899041517284957, 5.504228460268151046 ) ) ;
#38367 = CARTESIAN_POINT ( 'NONE',  ( 38.37437292394342592, 181.4155109091896065, 2.679491924311254714 ) ) ;
#38368 = VECTOR ( 'NONE', #40835, 1000.000000000000000 ) ;
#38369 = CARTESIAN_POINT ( 'NONE',  ( 191.4422718808379500, 282.7623406846040552, -17.33968414145821058 ) ) ;
#38370 = DIRECTION ( 'NONE',  ( 0.8575671445351807920, -0.5143720371616018472, 0.000000000000000000 ) ) ;
#38371 = CARTESIAN_POINT ( 'NONE',  ( 78.87554214658000262, 216.3458772461660544, 9.188101187500095079 ) ) ;
#38372 = CARTESIAN_POINT ( 'NONE',  ( -45.75347490765857117, 28.11296735934751112, -10.00000000000000000 ) ) ;
#38373 = CARTESIAN_POINT ( 'NONE',  ( 192.6679047218190135, 296.9363953644068488, -13.34486378385621386 ) ) ;
#38374 = PLANE ( 'NONE',  #85151 ) ;
#38375 = CARTESIAN_POINT ( 'NONE',  ( 154.9792334219179679, 262.2150889255981951, -17.21325849938693153 ) ) ;
#38376 = CARTESIAN_POINT ( 'NONE',  ( 207.8232941427535536, 270.6864908788566026, -6.505149060073906142 ) ) ;
#38377 = DIRECTION ( 'NONE',  ( -0.000000000000000000, -0.000000000000000000, -1.000000000000000000 ) ) ;
#38378 = CIRCLE ( 'NONE', #7656, 45.00000000000000000 ) ;
#38379 = CARTESIAN_POINT ( 'NONE',  ( 46.33644181719702715, 190.8927522451418213, 10.00000000000009948 ) ) ;
#38381 = CARTESIAN_POINT ( 'NONE',  ( 76.03486699543272209, 51.37517956710286171, 15.65877648513449394 ) ) ;
#38380 = DIRECTION ( 'NONE',  ( -0.8660254037844387076, -0.4999999999999998890, -0.000000000000000000 ) ) ;
#38382 = DIRECTION ( 'NONE',  ( -0.5000000000000006661, 0.8660254037844382635, -1.877843081442121204E-16 ) ) ;
#38383 = CARTESIAN_POINT ( 'NONE',  ( -19.65312891409030271, 93.06504152958497400, 40.00000000000000000 ) ) ;
#38384 = CARTESIAN_POINT ( 'NONE',  ( 204.8200301798767384, 275.8882966510998926, -12.76918925326218179 ) ) ;
#38385 = EDGE_CURVE ( 'NONE', #84992, #6168, #27193, .T. ) ;
#38386 = CARTESIAN_POINT ( 'NONE',  ( 157.7233946900069839, 257.4620621851055375, 16.86796251324260254 ) ) ;
#38387 = LINE ( 'NONE', #56077, #23638 ) ;
#38388 = EDGE_CURVE ( 'NONE', #92570, #47543, #80528, .T. ) ;
#38389 = CARTESIAN_POINT ( 'NONE',  ( 25.93973934025619599, 185.7833772461660544, -9.188101187500095079 ) ) ;
#38390 = VECTOR ( 'NONE', #58718, 1000.000000000000114 ) ;
#38391 = EDGE_CURVE ( 'NONE', #93052, #69710, #90019, .T. ) ;
#38392 = CARTESIAN_POINT ( 'NONE',  ( 49.48463145776311478, 205.5024278399160949, -9.188101187500093303 ) ) ;
#38393 = DIRECTION ( 'NONE',  ( -0.7713975076906469663, 0.000000000000000000, -0.6363535849892403284 ) ) ;
#38394 = CARTESIAN_POINT ( 'NONE',  ( 87.97191574057694652, 43.96735841855976901, 0.5176211603016172003 ) ) ;
#38395 = CARTESIAN_POINT ( 'NONE',  ( 165.7191908502203717, 249.0136070854895820, -9.415553735363799248 ) ) ;
#38396 = CARTESIAN_POINT ( 'NONE',  ( -16.43235775771474749, 167.9865022471903160, -10.00000000000009415 ) ) ;
#38397 = CARTESIAN_POINT ( 'NONE',  ( 66.87519508149094349, 69.72765056100607239, -0.6245140038366959745 ) ) ;
#38398 = LINE ( 'NONE', #16113, #71993 ) ;
#38399 = CARTESIAN_POINT ( 'NONE',  ( 15.95033727479334651, 30.18502408145591787, 5.678558825948276656 ) ) ;
#38400 = FACE_OUTER_BOUND ( 'NONE', #42300, .T. ) ;
#38401 = CARTESIAN_POINT ( 'NONE',  ( 149.4908848037268001, 271.7211875819559737, -12.92288068979413573 ) ) ;
#38402 = CARTESIAN_POINT ( 'NONE',  ( 18.07869151248302941, 12.29860640527291338, -2.839279412974138328 ) ) ;
#38403 = CARTESIAN_POINT ( 'NONE',  ( 59.93088934303040105, 217.6589784336661353, -6.496448406907676862E-16 ) ) ;
#38404 = CARTESIAN_POINT ( 'NONE',  ( 76.85308935164593436, 63.86692010595712787, 14.89649355574711542 ) ) ;
#38405 = CARTESIAN_POINT ( 'NONE',  ( 175.2603759342789829, 291.6537898291654187, 1.882018043770492977 ) ) ;
#38406 = CARTESIAN_POINT ( 'NONE',  ( 159.8655504377736918, 253.7517395922482706, 15.51368179719542262 ) ) ;
#38407 = CARTESIAN_POINT ( 'NONE',  ( 191.2557879401978198, 261.3776189723048446, -4.694998167070893125 ) ) ;
#38408 = CARTESIAN_POINT ( 'NONE',  ( 150.0366313281010093, 275.4335823404518351, 7.372954474402361846 ) ) ;
#38409 = CARTESIAN_POINT ( 'NONE',  ( 80.85015884162737620, 54.78783238080045948, -15.87653912250667076 ) ) ;
#38410 = CARTESIAN_POINT ( 'NONE',  ( 105.6772241758911264, 238.4865022471903444, -10.00000000000009415 ) ) ;
#38411 = CARTESIAN_POINT ( 'NONE',  ( 161.1884843536000744, 251.4603508349806873, 13.21272898143761942 ) ) ;
#38412 = CARTESIAN_POINT ( 'NONE',  ( 164.2600772519394923, 246.1401958748887182, -2.110785484364219311 ) ) ;
#38413 = ORIENTED_EDGE ( 'NONE', *, *, #30771, .T. ) ;
#38414 = CARTESIAN_POINT ( 'NONE',  ( 76.96233170383452205, 49.64203404956955978, 15.03896742044604373 ) ) ;
#38415 = CARTESIAN_POINT ( 'NONE',  ( 82.59507288524608271, 53.86809943430368008, 15.83774089001704155 ) ) ;
#38416 = VERTEX_POINT ( 'NONE', #96129 ) ;
#38417 = CARTESIAN_POINT ( 'NONE',  ( 159.7692415128758228, 253.9185515433934768, -16.85856106119654285 ) ) ;
#38418 = CARTESIAN_POINT ( 'NONE',  ( 186.8942146390193955, 276.6477083451915178, -17.00271009909913289 ) ) ;
#38419 = CARTESIAN_POINT ( 'NONE',  ( 115.5259514080638468, 249.0530062829863311, -4.648177544792955347E-16 ) ) ;
#38420 = VERTEX_POINT ( 'NONE', #67169 ) ;
#38421 = ORIENTED_EDGE ( 'NONE', *, *, #3975, .T. ) ;
#38422 = CARTESIAN_POINT ( 'NONE',  ( 79.15520340520409093, 45.87709371214184273, -12.50344660193819557 ) ) ;
#38423 = CARTESIAN_POINT ( 'NONE',  ( 148.4042165687623083, 273.6033521758856750, -8.709765892313745539 ) ) ;
#38424 = LINE ( 'NONE', #14146, #15910 ) ;
#38425 = VECTOR ( 'NONE', #37986, 1000.000000000000000 ) ;
#38426 = ORIENTED_EDGE ( 'NONE', *, *, #56421, .F. ) ;
#38427 = AXIS2_PLACEMENT_3D ( 'NONE', #44632, #13278, #44140 ) ;
#38428 = CARTESIAN_POINT ( 'NONE',  ( 23.18645373101242413, 19.10170272979927120, -7.433330006724141015 ) ) ;
#38429 = CARTESIAN_POINT ( 'NONE',  ( 74.93856232934675177, 54.57110059908732325, 16.13587931614057425 ) ) ;
#38430 = CARTESIAN_POINT ( 'NONE',  ( 7.026152882275393807, 27.55466486950697913, -1.111400068045478839E-16 ) ) ;
#38431 = FACE_OUTER_BOUND ( 'NONE', #13575, .T. ) ;
#38432 = ORIENTED_EDGE ( 'NONE', *, *, #57118, .T. ) ;
#38433 = FACE_OUTER_BOUND ( 'NONE', #17003, .T. ) ;
#38434 = CARTESIAN_POINT ( 'NONE',  ( 159.9470087484377814, 253.6106496594791508, -16.54933891566789939 ) ) ;
#38435 = VERTEX_POINT ( 'NONE', #57571 ) ;
#38436 = CARTESIAN_POINT ( 'NONE',  ( 171.1617965414632749, 285.2369355936916691, 11.22781892977234719 ) ) ;
#38437 = AXIS2_PLACEMENT_3D ( 'NONE', #53815, #54825, #98963 ) ;
#38439 = CARTESIAN_POINT ( 'NONE',  ( 67.74061933540588143, 65.90611994544174479, -10.51275149194319347 ) ) ;
#38438 = CARTESIAN_POINT ( 'NONE',  ( 162.9873704432093291, 283.5760391986459013, -3.109501405526100992 ) ) ;
#38440 = CARTESIAN_POINT ( 'NONE',  ( 68.93202468094986557, 70.80071090747883034, -1.952293371299729907 ) ) ;
#38441 = CARTESIAN_POINT ( 'NONE',  ( 163.8670932201372352, 246.8208641845333773, 5.912697114930636211 ) ) ;
#38442 = CARTESIAN_POINT ( 'NONE',  ( 198.5558597050348908, 286.7381581807989051, 17.16554469393394200 ) ) ;
#38443 = CARTESIAN_POINT ( 'NONE',  ( 157.2777284163744582, 258.2339788142568864, -16.82360006463426316 ) ) ;
#38444 = CARTESIAN_POINT ( 'NONE',  ( 131.9464011004214115, 256.1744531367911009, 4.594050593750047540 ) ) ;
#38445 = CARTESIAN_POINT ( 'NONE',  ( 203.1999414577625203, 267.8405105413980891, 2.559446679431893301 ) ) ;
#38446 = VECTOR ( 'NONE', #77057, 1000.000000000000000 ) ;
#38447 = CARTESIAN_POINT ( 'NONE',  ( 195.4450401646303987, 290.4134588786556037, -16.67804988919992581 ) ) ;
#38448 = CARTESIAN_POINT ( 'NONE',  ( 70.81050702595493362, 217.8149278399160664, 9.188101187500093303 ) ) ;
#38449 = ORIENTED_EDGE ( 'NONE', *, *, #37040, .T. ) ;
#38450 = CARTESIAN_POINT ( 'NONE',  ( 172.8011810764148208, 265.0538244599177347, 15.94685020396837238 ) ) ;
#38451 = CARTESIAN_POINT ( 'NONE',  ( 204.0604753336787667, 271.4817813032398703, 9.862283393711939183 ) ) ;
#38452 = EDGE_CURVE ( 'NONE', #47670, #48810, #7848, .T. ) ;
#38453 = EDGE_LOOP ( 'NONE', ( #83632, #97555, #78227, #73825 ) ) ;
#38454 = CARTESIAN_POINT ( 'NONE',  ( 195.4711919121670860, 292.0809595225171620, -15.84858701701355521 ) ) ;
#38455 = EDGE_LOOP ( 'NONE', ( #79879, #32077, #15657 ) ) ;
#38456 = DIRECTION ( 'NONE',  ( -0.5000000000000002220, 0.8660254037844384856, 0.000000000000000000 ) ) ;
#38457 = CARTESIAN_POINT ( 'NONE',  ( 66.72329116482525535, 67.50330200424541260, 6.535431412545530172 ) ) ;
#38458 = CARTESIAN_POINT ( 'NONE',  ( 197.6796757083432681, 286.6912785265818115, 16.92400811840941799 ) ) ;
#38459 = CARTESIAN_POINT ( 'NONE',  ( 147.0660117096331874, 275.9211909828330249, -0.7354350123930680772 ) ) ;
#38460 = DIRECTION ( 'NONE',  ( -0.8660254037844380415, -0.5000000000000011102, 0.000000000000000000 ) ) ;
#38461 = CARTESIAN_POINT ( 'NONE',  ( 154.8596847415876994, 262.4221533139083817, 17.65401077761399762 ) ) ;
#38462 = CARTESIAN_POINT ( 'NONE',  ( -71.07364842061382149, 47.42355933771584375, -10.00000000000000000 ) ) ;
#38463 = CARTESIAN_POINT ( 'NONE',  ( 77.90126356732251622, 215.7833772461660544, -9.188101187500095079 ) ) ;
#38464 = ORIENTED_EDGE ( 'NONE', *, *, #48508, .T. ) ;
#38465 = ADVANCED_FACE ( 'NONE', ( #57069 ), #18598, .T. ) ;
#38466 = PRESENTATION_LAYER_ASSIGNMENT (  '', '', ( #44901 ) ) ;
#38467 = VERTEX_POINT ( 'NONE', #53453 ) ;
#38468 = DIRECTION ( 'NONE',  ( -0.000000000000000000, -0.000000000000000000, -1.000000000000000000 ) ) ;
#38469 = CARTESIAN_POINT ( 'NONE',  ( -44.74834796241764678, 29.05375577536863929, 10.00000000000000000 ) ) ;
#38470 = VERTEX_POINT ( 'NONE', #67673 ) ;
#38471 = EDGE_CURVE ( 'NONE', #79855, #61965, #16420, .T. ) ;
#38472 = DIRECTION ( 'NONE',  ( -0.7352104281592295454, 0.6778389383370672094, 0.000000000000000000 ) ) ;
#38473 = CARTESIAN_POINT ( 'NONE',  ( 184.3174667830732574, 275.3152583799672470, 16.37424376149754934 ) ) ;
#38474 = CARTESIAN_POINT ( 'NONE',  ( 165.0020474182383339, 244.8550658491588479, 1.825383354618924425 ) ) ;
#38475 = CARTESIAN_POINT ( 'NONE',  ( 165.4191378457005897, 285.2699752501742978, 0.5081224057291762186 ) ) ;
#38476 = DIRECTION ( 'NONE',  ( -1.000000000000000000, 0.000000000000000000, 0.000000000000000000 ) ) ;
#38477 = DIRECTION ( 'NONE',  ( 0.5000000000000048850, -0.8660254037844358210, 0.000000000000000000 ) ) ;
#38478 = ORIENTED_EDGE ( 'NONE', *, *, #97551, .T. ) ;
#38479 = CARTESIAN_POINT ( 'NONE',  ( 188.6582881733277191, 295.0323815393699647, 11.70685045119338774 ) ) ;
#38480 = CARTESIAN_POINT ( 'NONE',  ( 37.84453522905105416, 33.80066082961425167, 10.00000000000000533 ) ) ;
#38481 = CARTESIAN_POINT ( 'NONE',  ( 37.92328063009087202, 22.86426979415092475, -3.090169943749474069 ) ) ;
#38482 = CARTESIAN_POINT ( 'NONE',  ( 200.8665851640556070, 282.7358642834317948, -16.69422397739980823 ) ) ;
#38483 = CARTESIAN_POINT ( 'NONE',  ( 72.69644901625827060, 70.79839986596044810, 7.145041847480314345 ) ) ;
#38484 = CARTESIAN_POINT ( 'NONE',  ( 70.19981261826917773, 67.37186692534301358, -9.767772922657160350 ) ) ;
#38485 = ORIENTED_EDGE ( 'NONE', *, *, #38605, .F. ) ;
#38486 = CARTESIAN_POINT ( 'NONE',  ( 196.0436306077152722, 265.5675073304090574, 4.427515145396084151 ) ) ;
#38487 = CARTESIAN_POINT ( 'NONE',  ( 148.3216606269014619, 276.4951605611222476, -3.899572877788914482 ) ) ;
#38488 = CARTESIAN_POINT ( 'NONE',  ( 22.53878541258498558, 190.4865022471903160, -10.00000000000009592 ) ) ;
#38489 = VECTOR ( 'NONE', #65956, 999.9999999999998863 ) ;
#38490 = CARTESIAN_POINT ( 'NONE',  ( 80.05248732009229684, 47.95723979042521279, 13.50885685003757786 ) ) ;
#38491 = DIRECTION ( 'NONE',  ( 0.4999999999999998890, -0.8660254037844385966, 0.000000000000000000 ) ) ;
#38492 = CARTESIAN_POINT ( 'NONE',  ( 153.3323979404929958, 270.2931725392325575, 13.99377495420697137 ) ) ;
#38493 = VERTEX_POINT ( 'NONE', #68162 ) ;
#38494 = CARTESIAN_POINT ( 'NONE',  ( 147.3023124603499809, 275.5119060767245287, 5.196938859334171212 ) ) ;
#38495 = CARTESIAN_POINT ( 'NONE',  ( 162.9466247808429102, 248.4151622881552441, 11.25765811906727443 ) ) ;
#38496 = VECTOR ( 'NONE', #90893, 1000.000000000000114 ) ;
#38497 = AXIS2_PLACEMENT_3D ( 'NONE', #84241, #89847, #54263 ) ;
#38498 = CARTESIAN_POINT ( 'NONE',  ( 206.9026071836525205, 272.2811674698855313, 7.240992997279449561 ) ) ;
#38500 = CARTESIAN_POINT ( 'NONE',  ( 73.73151203714552082, 55.28494777167826157, 16.11827203802588571 ) ) ;
#38499 = CARTESIAN_POINT ( 'NONE',  ( 193.9495889092963807, 294.7164532324382549, 15.46986001312306058 ) ) ;
#38501 = CARTESIAN_POINT ( 'NONE',  ( 26.48321701407081363, 20.45404122711134320, -8.090169943749478065 ) ) ;
#38502 = DIRECTION ( 'NONE',  ( 1.000000000000000000, 0.000000000000000000, 0.000000000000000000 ) ) ;
#38503 = CARTESIAN_POINT ( 'NONE',  ( 163.3311208880642766, 283.7460365591649065, -3.269890911538303246 ) ) ;
#38504 = LINE ( 'NONE', #85681, #79313 ) ;
#38505 = FACE_OUTER_BOUND ( 'NONE', #23608, .T. ) ;
#38506 = CIRCLE ( 'NONE', #93595, 6.749999999999992006 ) ;
#38507 = CARTESIAN_POINT ( 'NONE',  ( 153.5792543191700474, 246.1427522451417644, 1.119607411625061291E-15 ) ) ;
#38508 = FACE_OUTER_BOUND ( 'NONE', #15432, .T. ) ;
#38509 = ORIENTED_EDGE ( 'NONE', *, *, #28633, .T. ) ;
#38510 = EDGE_CURVE ( 'NONE', #30892, #38287, #14353, .T. ) ;
#38511 = VECTOR ( 'NONE', #25545, 1000.000000000000000 ) ;
#38512 = CARTESIAN_POINT ( 'NONE',  ( 66.71010751141994888, 68.10836325903318311, -6.508687729400615574 ) ) ;
#38513 = CARTESIAN_POINT ( 'NONE',  ( 72.84354978475251130, 71.10232518220605868, -7.524857974791618886 ) ) ;
#38514 = LINE ( 'NONE', #46104, #64003 ) ;
#38515 = CARTESIAN_POINT ( 'NONE',  ( 81.82619482746289918, 41.23108798929906982, 5.814899641828136012 ) ) ;
#38516 = CARTESIAN_POINT ( 'NONE',  ( 10.56744132731740393, 189.1589784336661637, -6.496448406907676862E-16 ) ) ;
#38517 = CARTESIAN_POINT ( 'NONE',  ( 176.1996253725332053, 265.6108028435369306, -16.12497321327553834 ) ) ;
#38518 = CARTESIAN_POINT ( 'NONE',  ( 181.7343043149082291, 275.5595704463788138, -16.43090409027867693 ) ) ;
#38519 = CARTESIAN_POINT ( 'NONE',  ( 27.47308016966368882, 31.56454794089043148, 10.00000000000000355 ) ) ;
#38520 = CARTESIAN_POINT ( 'NONE',  ( 84.36224227157138955, 42.17653682963820216, -2.312994364957334348 ) ) ;
#38521 = CARTESIAN_POINT ( 'NONE',  ( 205.0520875136525376, 275.4863615587311756, -14.16385635411862509 ) ) ;
#38522 = FACE_OUTER_BOUND ( 'NONE', #23009, .T. ) ;
#38523 = B_SPLINE_SURFACE_WITH_KNOTS ( 'NONE', 3, 1, ( 
 ( #57108, #80472 ),
 ( #72855, #37301 ),
 ( #75837, #66709 ),
 ( #83450, #53004 ),
 ( #35815, #28211 ),
 ( #99128, #98641 ),
 ( #43903, #14017 ),
 ( #97645, #58597 ),
 ( #83955, #59086 ),
 ( #36805, #21621 ),
 ( #67717, #98134 ),
 ( #75333, #68201 ),
 ( #74349, #90060 ),
 ( #29711, #52501 ),
 ( #90570, #60587 ),
 ( #97162, #20629 ),
 ( #29224, #91543 ),
 ( #45401, #44897 ),
 ( #6424, #82957 ),
 ( #22111, #60092 ),
 ( #5916, #51006 ),
 ( #51512, #14519 ),
 ( #76331, #37793 ),
 ( #6904, #27727 ),
 ( #13531, #59593 ),
 ( #89572, #20132 ),
 ( #21138, #28719 ),
 ( #81957, #12532 ),
 ( #43404, #4937 ),
 ( #82478, #13042 ),
 ( #91056, #74843 ) ),
 .UNSPECIFIED., .F., .F., .F.,
 ( 4, 3, 3, 3, 3, 3, 3, 3, 3, 3, 4 ),
 ( 2, 2 ),
 ( 0.000000000000000000, 0.1122669598086702414, 0.2243161639709582988, 0.3396355846219021313, 0.4553962076585123531, 0.5677860799922337387, 0.6749047109689639834, 0.7773884377078371655, 0.8775581155834336622, 0.9782364162377958916, 1.000000000000000000 ),
 ( 0.000000000000000000, 1.000000000000000000 ),
 .UNSPECIFIED. ) ;
#38524 = CARTESIAN_POINT ( 'NONE',  ( 41.64315915125185086, 206.3967562850347122, -4.648177544792955347E-16 ) ) ;
#38525 = DIRECTION ( 'NONE',  ( 0.05364311403569549386, 0.9985601716053735810, 0.000000000000000000 ) ) ;
#38526 = B_SPLINE_CURVE_WITH_KNOTS ( 'NONE', 3,
 ( #56654, #64770, #80001, #12067 ),
 .UNSPECIFIED., .F., .F.,
 ( 4, 4 ),
 ( 0.02779447496634188455, 0.03699400560506550112 ),
 .UNSPECIFIED. ) ;
#38527 = CARTESIAN_POINT ( 'NONE',  ( 182.8490516821578922, 296.1971294003607227, 1.821377340828691516 ) ) ;
#38528 = CARTESIAN_POINT ( 'NONE',  ( 78.03658003843786162, 205.8615022471901739, 5.000000000000051514 ) ) ;
#38529 = CYLINDRICAL_SURFACE ( 'NONE', #70068, 10.00000000000010658 ) ;
#38530 = AXIS2_PLACEMENT_3D ( 'NONE', #29354, #52135, #46016 ) ;
#38531 = CARTESIAN_POINT ( 'NONE',  ( 147.6220714307702622, 274.9580672937808572, 8.392894244419288441 ) ) ;
#38532 = CARTESIAN_POINT ( 'NONE',  ( 26.15589859543730000, 198.1589784336661637, -6.496448406907675876E-16 ) ) ;
#38533 = CARTESIAN_POINT ( 'NONE',  ( 69.18180081457823860, 70.09578702365529068, -5.264143515239704918 ) ) ;
#38534 = CARTESIAN_POINT ( 'NONE',  ( 202.9990333130177191, 270.0056268523717335, -6.342944502012394459 ) ) ;
#38535 = CARTESIAN_POINT ( 'NONE',  ( 150.8247211172754589, 269.4109153179094278, -14.37608026040300402 ) ) ;
#38536 = CARTESIAN_POINT ( 'NONE',  ( 207.5338226493333025, 271.1878702128032614, 6.432541580693135863 ) ) ;
#38537 = CARTESIAN_POINT ( 'NONE',  ( 155.2098048002210930, 261.8157275836062468, 16.98811268941991059 ) ) ;
#38538 = CARTESIAN_POINT ( 'NONE',  ( -17.42236680055705023, 149.2012482093457777, 0.000000000000000000 ) ) ;
#38539 = CARTESIAN_POINT ( 'NONE',  ( 202.8700503780948736, 278.3479282389285459, -15.15511564031462832 ) ) ;
#38540 = CARTESIAN_POINT ( 'NONE',  ( 161.0050726372687393, 280.1669587882555561, 9.054279574223530247 ) ) ;
#38541 = CONTEXT_DEPENDENT_SHAPE_REPRESENTATION ( #65544, #42683 ) ;
#38542 = CARTESIAN_POINT ( 'NONE',  ( 22.22900788544320605, 15.76004757982089544, 5.678558825948272215 ) ) ;
#38543 = CARTESIAN_POINT ( 'NONE',  ( 198.2505066714982149, 285.2670451491296149, 0.000000000000000000 ) ) ;
#38544 = CARTESIAN_POINT ( 'NONE',  ( 71.46833469722506038, 59.16469923302185663, 15.28718056364334821 ) ) ;
#38545 = CARTESIAN_POINT ( 'NONE',  ( 186.8465721486132907, 268.7342973959014216, -14.16766902808887174 ) ) ;
#38546 = ORIENTED_EDGE ( 'NONE', *, *, #85833, .T. ) ;
#38547 = CARTESIAN_POINT ( 'NONE',  ( 81.65498813923811383, 45.89998691845250534, -12.05192607633446578 ) ) ;
#38548 = CARTESIAN_POINT ( 'NONE',  ( 73.44882731304140577, 59.76980209779112130, -15.46587551932410065 ) ) ;
#38549 = CARTESIAN_POINT ( 'NONE',  ( 81.68014092384574099, 42.03450286479537112, 7.559063547066712907 ) ) ;
#38550 = ORIENTED_EDGE ( 'NONE', *, *, #87066, .F. ) ;
#38551 = CARTESIAN_POINT ( 'NONE',  ( -110.0000000000000142, -8.000000000000000000, 9.212605237762145904 ) ) ;
#38552 = CARTESIAN_POINT ( 'NONE',  ( 72.61665845909378447, 71.49531248604364464, -5.610398693002283110 ) ) ;
#38553 = CARTESIAN_POINT ( 'NONE',  ( 73.14850971396091950, 57.24856527839357767, 16.39375171836413614 ) ) ;
#38554 = DIRECTION ( 'NONE',  ( -0.2877784213863818774, 0.9576970189910596343, 0.000000000000000000 ) ) ;
#38555 = ORIENTED_EDGE ( 'NONE', *, *, #22731, .F. ) ;
#38556 = ORIENTED_EDGE ( 'NONE', *, *, #94207, .F. ) ;
#38558 = LINE ( 'NONE', #63373, #32989 ) ;
#38557 = DIRECTION ( 'NONE',  ( -0.8660254037844387076, -0.4999999999999998890, -0.000000000000000000 ) ) ;
#38559 = ORIENTED_EDGE ( 'NONE', *, *, #57745, .F. ) ;
#38560 = CARTESIAN_POINT ( 'NONE',  ( 201.2535035105529744, 282.0657020489176716, -18.08976065250591958 ) ) ;
#38561 = VECTOR ( 'NONE', #37144, 1000.000000000000000 ) ;
#38562 = CARTESIAN_POINT ( 'NONE',  ( 70.40337949093891723, 65.94787112513976979, 11.92354459682091417 ) ) ;
#38563 = CARTESIAN_POINT ( 'NONE',  ( 196.4030970371012472, 264.3490001850324234, -4.693669024083267693 ) ) ;
#38564 = CARTESIAN_POINT ( 'NONE',  ( -105.0000000000000000, 10.00000000000000000, 14.21260523776214235 ) ) ;
#38566 = ORIENTED_EDGE ( 'NONE', *, *, #80199, .T. ) ;
#38565 = B_SPLINE_CURVE_WITH_KNOTS ( 'NONE', 3,
 ( #55207, #71444, #71942, #86188 ),
 .UNSPECIFIED., .F., .F.,
 ( 4, 4 ),
 ( 1.003144254802035469E-16, 0.005446537507594250913 ),
 .UNSPECIFIED. ) ;
#38567 = CARTESIAN_POINT ( 'NONE',  ( 147.7978300115112233, 274.6536445020713018, 7.902890709649431855 ) ) ;
#38568 = VECTOR ( 'NONE', #84785, 1000.000000000000114 ) ;
#38569 = VECTOR ( 'NONE', #74998, 1000.000000000000000 ) ;
#38570 = EDGE_CURVE ( 'NONE', #53329, #38470, #57509, .T. ) ;
#38571 = ORIENTED_EDGE ( 'NONE', *, *, #80453, .F. ) ;
#38572 = CARTESIAN_POINT ( 'NONE',  ( 195.9920715006079490, 291.1787696107118677, 15.99608784761372071 ) ) ;
#38573 = VECTOR ( 'NONE', #68099, 1000.000000000000000 ) ;
#38574 = CARTESIAN_POINT ( 'NONE',  ( 158.9922026222019156, 265.5549985037428087, 16.88018579597198610 ) ) ;
#38575 = ORIENTED_EDGE ( 'NONE', *, *, #76180, .T. ) ;
#38576 = CARTESIAN_POINT ( 'NONE',  ( 81.55541168055334822, 59.46620198043990513, -0.3345653031794336152 ) ) ;
#38577 = CARTESIAN_POINT ( 'NONE',  ( 78.19896130658693778, 47.52697404029742501, -14.39010834518865423 ) ) ;
#38578 = EDGE_CURVE ( 'NONE', #98895, #70875, #37263, .T. ) ;
#38579 = ORIENTED_EDGE ( 'NONE', *, *, #29834, .T. ) ;
#38580 = CARTESIAN_POINT ( 'NONE',  ( -17.24452398764597305, 75.38583958956024844, 13.39357157112610608 ) ) ;
#38581 = CARTESIAN_POINT ( 'NONE',  ( 160.5772802285540024, 254.1801457531887536, 15.69096569341868452 ) ) ;
#38582 = CARTESIAN_POINT ( 'NONE',  ( 78.28343461854488794, 47.82939899132422568, -14.51444300807813548 ) ) ;
#38583 = DIRECTION ( 'NONE',  ( -0.9957145386939475484, -0.09248003802712848054, 0.000000000000000000 ) ) ;
#38584 = ORIENTED_EDGE ( 'NONE', *, *, #79610, .T. ) ;
#38585 = ORIENTED_EDGE ( 'NONE', *, *, #23850, .T. ) ;
#38586 = VECTOR ( 'NONE', #84818, 1000.000000000000000 ) ;
#38587 = CARTESIAN_POINT ( 'NONE',  ( 189.9686529740312153, 299.6116365339944423, 6.575253125843024016 ) ) ;
#38588 = CARTESIAN_POINT ( 'NONE',  ( 70.44081555586384980, 218.1427522451419065, -10.00000000000009592 ) ) ;
#38589 = CARTESIAN_POINT ( 'NONE',  ( 190.6084209867335915, 300.5035258309363826, -0.5505750481748228342 ) ) ;
#38590 = CARTESIAN_POINT ( 'NONE',  ( 190.6661865267473104, 300.4034729807058852, 4.523489664447863490 ) ) ;
#38591 = CARTESIAN_POINT ( 'NONE',  ( 136.9263074957796675, 249.8615022471902591, -10.00000000000009592 ) ) ;
#38592 = EDGE_CURVE ( 'NONE', #63287, #21764, #20033, .T. ) ;
#38593 = CARTESIAN_POINT ( 'NONE',  ( 191.1517988646461674, 299.5623677386828376, 8.533933079859274073 ) ) ;
#38594 = CARTESIAN_POINT ( 'NONE',  ( 147.0456760057551833, 275.9564134551570760, -3.678503029046952033 ) ) ;
#38595 = CARTESIAN_POINT ( 'NONE',  ( 163.1374594064594987, 257.6710164228418876, 15.57553777135039219 ) ) ;
#38596 = CARTESIAN_POINT ( 'NONE',  ( 70.83774435152801630, 69.32499766432513866, 7.689863540467408498 ) ) ;
#38597 = AXIS2_PLACEMENT_3D ( 'NONE', #59852, #13760, #61719 ) ;
#38598 = CARTESIAN_POINT ( 'NONE',  ( 71.41016749218992743, 59.45273978182970609, 15.19346469599747174 ) ) ;
#38599 = CARTESIAN_POINT ( 'NONE',  ( 80.01849117754963459, 40.12822637883668619, 1.972556413651486167E-15 ) ) ;
#38600 = CARTESIAN_POINT ( 'NONE',  ( 71.59027552632591096, 65.27526798289987653, -12.38681006073837665 ) ) ;
#38601 = CARTESIAN_POINT ( 'NONE',  ( 77.94133778169836546, 48.01103128161624056, 14.15575917907049863 ) ) ;
#38602 = VERTEX_POINT ( 'NONE', #91504 ) ;
#38603 = CARTESIAN_POINT ( 'NONE',  ( 190.4637805006824749, 300.7540505016085035, -3.224520439125855287 ) ) ;
#38604 = CARTESIAN_POINT ( 'NONE',  ( -66.21217304253430314, 40.79406095866393400, 177.5919119679930134 ) ) ;
#38605 = EDGE_CURVE ( 'NONE', #45423, #78211, #59823, .T. ) ;
#38606 = CARTESIAN_POINT ( 'NONE',  ( 79.09530520295683687, 46.04380001988058524, 13.24189403536401954 ) ) ;
#38607 = EDGE_CURVE ( 'NONE', #42933, #65992, #55932, .T. ) ;
#38608 = CARTESIAN_POINT ( 'NONE',  ( 179.5645164103034119, 282.8161413207554915, -15.65081265547478928 ) ) ;
#38609 = CARTESIAN_POINT ( 'NONE',  ( 148.0336604448368405, 274.2451742095802842, -9.068513419098270134 ) ) ;
#38610 = CARTESIAN_POINT ( 'NONE',  ( 169.2175156373457128, 285.3665543728620264, -7.678154704465813829 ) ) ;
#38611 = VERTEX_POINT ( 'NONE', #94004 ) ;
#38612 = CARTESIAN_POINT ( 'NONE',  ( 208.3586375946586315, 269.7592488206576604, -1.970210487958146128 ) ) ;
#38613 = CARTESIAN_POINT ( 'NONE',  ( 72.59688737879588416, 71.44559626476468850, 5.687857618654109437 ) ) ;
#38614 = CARTESIAN_POINT ( 'NONE',  ( 43.23318412030275226, 195.7677522451418781, 10.00000000000009592 ) ) ;
#38615 = CARTESIAN_POINT ( 'NONE',  ( 151.4376533647338476, 268.3492855237141725, -15.16853828792834236 ) ) ;
#38616 = CARTESIAN_POINT ( 'NONE',  ( 67.00896575216198414, 67.70770252604407347, -6.454429227916835821 ) ) ;
#38617 = CARTESIAN_POINT ( 'NONE',  ( 196.2048238403250764, 290.8102717488927169, 17.53926796892840656 ) ) ;
#38618 = CARTESIAN_POINT ( 'NONE',  ( 175.4671943841053690, 253.5411772790661757, -4.255739755355884668 ) ) ;
#38619 = CARTESIAN_POINT ( 'NONE',  ( 50.02589733512838421, 205.8149278399161233, 9.188101187500093303 ) ) ;
#38620 = CARTESIAN_POINT ( 'NONE',  ( 178.6804572816645589, 292.0409386983645277, -5.741727636564030846 ) ) ;
#38621 = FACE_OUTER_BOUND ( 'NONE', #34813, .T. ) ;
#38622 = VERTEX_POINT ( 'NONE', #78779 ) ;
#38623 = CARTESIAN_POINT ( 'NONE',  ( 71.79693945464293847, 65.84970020821658920, 12.07886075470384135 ) ) ;
#38624 = CARTESIAN_POINT ( 'NONE',  ( 88.03940145429997699, 44.60316185140228384, -4.090138835865407607 ) ) ;
#38625 = ADVANCED_FACE ( 'NONE', ( #70143 ), #71688, .F. ) ;
#38626 = CARTESIAN_POINT ( 'NONE',  ( 26.84540973961100008, 174.7592609112379876, 2.679491924311254714 ) ) ;
#38627 = CARTESIAN_POINT ( 'NONE',  ( 147.4368675721658519, 275.2788497866417288, 5.050119523016719292 ) ) ;
#38628 = LINE ( 'NONE', #15317, #3013 ) ;
#38629 = DIRECTION ( 'NONE',  ( 0.5000000000000048850, -0.8660254037844358210, 0.000000000000000000 ) ) ;
#38630 = CARTESIAN_POINT ( 'NONE',  ( 180.9275591696145966, 262.4355116931648126, 12.34148954679617560 ) ) ;
#38631 = ADVANCED_FACE ( 'NONE', ( #62035 ), #17330, .T. ) ;
#38632 = CARTESIAN_POINT ( 'NONE',  ( 118.1443815476567352, 229.0177522451417929, 5.000000000000051514 ) ) ;
#38633 = AXIS2_PLACEMENT_3D ( 'NONE', #14930, #8347, #45820 ) ;
#38634 = CARTESIAN_POINT ( 'NONE',  ( -19.65312891409030271, 93.06504152958497400, -10.00000000000000888 ) ) ;
#38635 = VERTEX_POINT ( 'NONE', #35153 ) ;
#38636 = ADVANCED_FACE ( 'NONE', ( #65063 ), #57955, .F. ) ;
#38637 = CIRCLE ( 'NONE', #16016, 9.000000000000007105 ) ;
#38638 = ADVANCED_FACE ( 'NONE', ( #81309 ), #11880, .F. ) ;
#38639 = CARTESIAN_POINT ( 'NONE',  ( 147.6300909839706321, 274.9441770201837585, 8.328755691084779755 ) ) ;
#38640 = CARTESIAN_POINT ( 'NONE',  ( 207.8446715390582540, 270.6494641423232679, -2.429516028743652800 ) ) ;
#38641 = VECTOR ( 'NONE', #88047, 1000.000000000000000 ) ;
#38642 = ADVANCED_FACE ( 'NONE', ( #58925 ), #58447, .T. ) ;
#38643 = CARTESIAN_POINT ( 'NONE',  ( 26.10194555558328133, 192.0024278399160949, -9.188101187500093303 ) ) ;
#38644 = AXIS2_PLACEMENT_3D ( 'NONE', #11858, #89400, #98453 ) ;
#38645 = CARTESIAN_POINT ( 'NONE',  ( 15.32787473065566530, 20.80066082961420904, 10.00000000000000533 ) ) ;
#38646 = CARTESIAN_POINT ( 'NONE',  ( -16.78138373794034877, 105.4614945587019577, 44.35755392706056455 ) ) ;
#38647 = CARTESIAN_POINT ( 'NONE',  ( 193.6523268064705974, 293.2313262976975352, 15.26490498002906193 ) ) ;
#38648 = CARTESIAN_POINT ( 'NONE',  ( 73.02433024948126672, 69.66517378990663190, 9.714162469163342806 ) ) ;
#38649 = EDGE_CURVE ( 'NONE', #45893, #31631, #93401, .T. ) ;
#38651 = CARTESIAN_POINT ( 'NONE',  ( 75.14098114064213974, 208.0643266524159571, -9.188101187500093303 ) ) ;
#38650 = CARTESIAN_POINT ( 'NONE',  ( 174.2270345836575132, 287.1587744952294088, 10.32173088169526842 ) ) ;
#38652 = DIRECTION ( 'NONE',  ( -0.8660254037844387076, -0.4999999999999998890, -0.000000000000000000 ) ) ;
#38653 = CARTESIAN_POINT ( 'NONE',  ( 72.71802232570068725, 57.16443033622703496, 15.88657016229421615 ) ) ;
#38654 = CARTESIAN_POINT ( 'NONE',  ( -32.60591808846487538, 96.18968631316256790, 44.15639294459641917 ) ) ;
#38655 = CARTESIAN_POINT ( 'NONE',  ( 66.51857804634171600, 68.84334513988093818, -4.410274944405629505 ) ) ;
#38656 = VERTEX_POINT ( 'NONE', #56950 ) ;
#38657 = AXIS2_PLACEMENT_3D ( 'NONE', #1203, #47777, #62995 ) ;
#38658 = CARTESIAN_POINT ( 'NONE',  ( 165.3960647433960673, 269.3279595906375334, 17.30649301441624743 ) ) ;
#38659 = CARTESIAN_POINT ( 'NONE',  ( 35.52916646935165090, 177.9865022471901170, 1.119607411625061291E-15 ) ) ;
#38660 = CARTESIAN_POINT ( 'NONE',  ( 208.0287371622045782, 270.3306531311065442, 3.558879245883286746 ) ) ;
#38661 = CARTESIAN_POINT ( 'NONE',  ( -9.107486540969064848, 174.7369531367911293, -4.594050593750048428 ) ) ;
#38662 = CARTESIAN_POINT ( 'NONE',  ( 31.70236382085744609, 33.70171378149921537, -9.188101187500004485 ) ) ;
#38663 = CARTESIAN_POINT ( 'NONE',  ( 167.7933980256991333, 262.5155890272394004, -16.76255740563084018 ) ) ;
#38664 = CARTESIAN_POINT ( 'NONE',  ( 185.2721877113579012, 260.3715536164725677, 6.614250018501683037 ) ) ;
#38665 = CARTESIAN_POINT ( 'NONE',  ( 164.5348324038273518, 245.6643059921780718, 1.473102934610569958 ) ) ;
#38666 = DIRECTION ( 'NONE',  ( -0.09274582908234026146, -0.9956898167541081701, 0.000000000000000000 ) ) ;
#38667 = CARTESIAN_POINT ( 'NONE',  ( 65.81547766408900202, 68.95580224303030548, 2.207512132855569131 ) ) ;
#38668 = EDGE_LOOP ( 'NONE', ( #58665, #3347, #38585, #86756 ) ) ;
#38669 = CARTESIAN_POINT ( 'NONE',  ( 81.81187772080372156, 54.45965212650729370, 16.10770018195577435 ) ) ;
#38670 = CARTESIAN_POINT ( 'NONE',  ( -19.65312891409030271, 93.06504152958497400, -10.00000000000000888 ) ) ;
#38671 = CARTESIAN_POINT ( 'NONE',  ( -110.0000000000000000, 4.999999999999999112, 59.99999999999999289 ) ) ;
#38672 = CARTESIAN_POINT ( 'NONE',  ( 7.926391159377050855, 27.68290643055185996, 3.479690158560446702E-15 ) ) ;
#38673 = ORIENTED_EDGE ( 'NONE', *, *, #66813, .T. ) ;
#38674 = CARTESIAN_POINT ( 'NONE',  ( 165.7158856635367670, 245.9455260183406153, -1.115825035939094878 ) ) ;
#38675 = CARTESIAN_POINT ( 'NONE',  ( 200.8924071879331166, 282.0774472293816189, -16.63419059431211977 ) ) ;
#38676 = CARTESIAN_POINT ( 'NONE',  ( 87.63502826371535548, 214.7365022471901739, -10.00000000000009237 ) ) ;
#38677 = CARTESIAN_POINT ( 'NONE',  ( 98.24615118885414233, 215.9824982072973683, 3.021315404115420679E-15 ) ) ;
#38678 = CARTESIAN_POINT ( 'NONE',  ( 208.1612901671020381, 270.1010645919285480, -2.401583477149568768 ) ) ;
#38679 = CARTESIAN_POINT ( 'NONE',  ( 157.8501323257721083, 280.8042112442767007, -7.123878780571343050 ) ) ;
#38680 = EDGE_LOOP ( 'NONE', ( #73249, #45755, #14195, #47063 ) ) ;
#38681 = VERTEX_POINT ( 'NONE', #81799 ) ;
#38682 = CARTESIAN_POINT ( 'NONE',  ( 190.4722783054066326, 281.5708337987511527, 17.36680661303515549 ) ) ;
#38683 = CARTESIAN_POINT ( 'NONE',  ( 72.99387774792295147, 70.80171071775477287, 7.420862911638799631 ) ) ;
#38684 = VERTEX_POINT ( 'NONE', #20473 ) ;
#38685 = CARTESIAN_POINT ( 'NONE',  ( 149.6896757981861583, 271.3768714794653647, 12.49809796062302603 ) ) ;
#38686 = CARTESIAN_POINT ( 'NONE',  ( 17.57657260583443559, 33.08080186712592763, -3.090169943749475845 ) ) ;
#38687 = CARTESIAN_POINT ( 'NONE',  ( 82.94646378975579637, 45.29401946974905968, -10.14977777037833562 ) ) ;
#38688 = B_SPLINE_CURVE_WITH_KNOTS ( 'NONE', 3,
 ( #15708, #39493, #46610, #77540, #39005, #15204, #30921 ),
 .UNSPECIFIED., .F., .F.,
 ( 4, 3, 4 ),
 ( 0.000000000000000000, 0.001498044977029682010, 0.003457732078973784796 ),
 .UNSPECIFIED. ) ;
#38689 = ORIENTED_EDGE ( 'NONE', *, *, #85914, .T. ) ;
#38690 = CARTESIAN_POINT ( 'NONE',  ( 191.0933613939813540, 299.6635844069401173, -8.689828987424775164 ) ) ;
#38691 = CARTESIAN_POINT ( 'NONE',  ( 79.52258874318322057, 59.35007886418325285, -16.21401609639227104 ) ) ;
#38692 = B_SPLINE_CURVE_WITH_KNOTS ( 'NONE', 3,
 ( #17318, #32530, #79671, #33020, #78642, #9225, #25417, #55791, #49234, #86784, #56309, #94857, #48739, #63424, #95876, #10233, #41102, #48223, #40104, #87305, #94363, #72038, #2641, #33529, #63918, #80168, #79170, #25941, #56816, #24917, #71044, #80673, #18837, #40609, #10735, #96362, #87799, #9750, #18340, #72553, #3157, #71543, #88283, #34042, #64932, #26435, #1646, #57313, #11249, #3639 ),
 .UNSPECIFIED., .F., .F.,
 ( 4, 2, 2, 2, 2, 2, 2, 2, 2, 2, 2, 2, 2, 2, 2, 2, 2, 2, 2, 2, 2, 2, 2, 2, 4 ),
 ( 0.0008287262012033482601, 0.001030356982722712084, 0.001131172373482456717, 0.001231987764242201133, 0.001332803155001945766, 0.001433618545761690399, 0.001635249327281108325, 0.002038510890320054114, 0.002441772453359000554, 0.003248295579436893434, 0.004054818705514786313, 0.004861341831592680060, 0.005264603394631663796, 0.005466234176151118368, 0.005567049566910887287, 0.005617457262290818584, 0.005667864957670749881, 0.005718272653050681179, 0.005768680348430612476, 0.005869495739190313741, 0.006071126520709579227, 0.006474388083748255050, 0.006877649646786930873, 0.007079280428306236259, 0.007280911209825541644 ),
 .UNSPECIFIED. ) ;
#38693 = CARTESIAN_POINT ( 'NONE',  ( 196.9728329903666122, 289.4800408803428695, -17.53478045286815856 ) ) ;
#38694 = CARTESIAN_POINT ( 'NONE',  ( 70.01663930090745680, 62.76214446738973152, 13.38958553957018083 ) ) ;
#38695 = ORIENTED_EDGE ( 'NONE', *, *, #2021, .F. ) ;
#38696 = CARTESIAN_POINT ( 'NONE',  ( 161.1027382213887336, 251.6088674925233022, 13.55451100897754557 ) ) ;
#38697 = CARTESIAN_POINT ( 'NONE',  ( 191.4922467593309250, 298.9726946877590876, 7.604184559945784017 ) ) ;
#38698 = CARTESIAN_POINT ( 'NONE',  ( 168.6888362159111523, 279.3388723634037660, -14.98891133512231377 ) ) ;
#38699 = ORIENTED_EDGE ( 'NONE', *, *, #15402, .F. ) ;
#38700 = ORIENTED_EDGE ( 'NONE', *, *, #87678, .T. ) ;
#38701 = ORIENTED_EDGE ( 'NONE', *, *, #61502, .T. ) ;
#38702 = CARTESIAN_POINT ( 'NONE',  ( 80.20053959639768948, 46.07477633858642463, 12.22461583764979132 ) ) ;
#38703 = VERTEX_POINT ( 'NONE', #12375 ) ;
#38704 = CARTESIAN_POINT ( 'NONE',  ( 70.56998135810292183, 71.19273197352897853, 2.578484167683574579 ) ) ;
#38705 = VERTEX_POINT ( 'NONE', #74183 ) ;
#38706 = CARTESIAN_POINT ( 'NONE',  ( -63.08903959183645327, 39.77784189046417396, -10.00000000000000000 ) ) ;
#38707 = CARTESIAN_POINT ( 'NONE',  ( 82.17853646903301978, 46.01985525210849914, 11.26429781250972084 ) ) ;
#38708 = CARTESIAN_POINT ( 'NONE',  ( 167.6203508625312963, 281.1962390192910561, 11.49557606910398633 ) ) ;
#38709 = CARTESIAN_POINT ( 'NONE',  ( 194.7576540903134799, 293.3168432830895540, -14.62421624641040196 ) ) ;
#38710 = EDGE_CURVE ( 'NONE', #16392, #45778, #68261, .T. ) ;
#38712 = CARTESIAN_POINT ( 'NONE',  ( 70.34489617550165974, 68.43624669578447595, -8.554681912399528798 ) ) ;
#38711 = AXIS2_PLACEMENT_3D ( 'NONE', #64122, #10939, #79869 ) ;
#38713 = CARTESIAN_POINT ( 'NONE',  ( 203.9777429970372395, 272.3976805576900801, -11.01560090989651997 ) ) ;
#38714 = CARTESIAN_POINT ( 'NONE',  ( 12.93608109523609073, 25.65586893147755276, -7.433330006724137462 ) ) ;
#38715 = CARTESIAN_POINT ( 'NONE',  ( 163.6954058318546004, 282.3930307436989438, 8.504173745411177876 ) ) ;
#38716 = CARTESIAN_POINT ( 'NONE',  ( 80.22399782384964340, 57.81478883376428968, 16.60249858296847947 ) ) ;
#38717 = CIRCLE ( 'NONE', #53328, 70.00000000000001421 ) ;
#38719 = ORIENTED_EDGE ( 'NONE', *, *, #29628, .F. ) ;
#38718 = DIRECTION ( 'NONE',  ( 1.000000000000000000, 0.000000000000000000, 0.000000000000000000 ) ) ;
#38720 = CARTESIAN_POINT ( 'NONE',  ( 171.1028772385554078, 259.1587979975018357, -13.89206456122039235 ) ) ;
#38721 = CARTESIAN_POINT ( 'NONE',  ( 206.8775514429320026, 272.3245652858344670, -9.838455694836268250 ) ) ;
#38722 = EDGE_CURVE ( 'NONE', #64867, #58503, #76175, .T. ) ;
#38723 = CARTESIAN_POINT ( 'NONE',  ( 165.5968251294584661, 246.8041483929534081, -2.409699260217772476 ) ) ;
#38724 = CARTESIAN_POINT ( 'NONE',  ( 67.67928228426634973, 65.72340518148261879, -10.66721164749792550 ) ) ;
#38725 = EDGE_CURVE ( 'NONE', #12312, #55017, #99463, .T. ) ;
#38726 = CARTESIAN_POINT ( 'NONE',  ( 161.1089126327036354, 251.5981730984191529, 13.95161017039218976 ) ) ;
#38727 = CARTESIAN_POINT ( 'NONE',  ( 161.2907445571653398, 283.4895778383536822, 2.139433395802937454 ) ) ;
#38728 = VECTOR ( 'NONE', #34944, 1000.000000000000000 ) ;
#38729 = ORIENTED_EDGE ( 'NONE', *, *, #84418, .T. ) ;
#38730 = CARTESIAN_POINT ( 'NONE',  ( 155.7875766807000559, 260.8149973314318686, -17.66409480421729583 ) ) ;
#38731 = CARTESIAN_POINT ( 'NONE',  ( 74.79265276366315618, 66.79451150088598865, -13.18326711696947839 ) ) ;
#38732 = FACE_OUTER_BOUND ( 'NONE', #7948, .T. ) ;
#38733 = CARTESIAN_POINT ( 'NONE',  ( 0.4370954166217684844, 164.3927522451417929, -10.00000000000009059 ) ) ;
#38734 = CARTESIAN_POINT ( 'NONE',  ( 79.66011734693590540, 225.9869531367911293, 4.594050593750046652 ) ) ;
#38735 = CARTESIAN_POINT ( 'NONE',  ( 195.3483670750180465, 269.0306795110596454, -10.80387254427798993 ) ) ;
#38736 = CARTESIAN_POINT ( 'NONE',  ( 204.2446710276013846, 276.8848479354406322, -15.25810902262900193 ) ) ;
#38737 = CARTESIAN_POINT ( 'NONE',  ( 173.4037495197947294, 288.6795182003594391, 9.022545291891718833 ) ) ;
#38739 = CARTESIAN_POINT ( 'NONE',  ( 4.715407580134756138, 161.9824982072973683, 3.021315404115420679E-15 ) ) ;
#38738 = CARTESIAN_POINT ( 'NONE',  ( 9.485603764116877556, 164.0327760586659451, 1.948934522072303157E-15 ) ) ;
#38740 = VECTOR ( 'NONE', #58117, 1000.000000000000000 ) ;
#38741 = CARTESIAN_POINT ( 'NONE',  ( 161.8662906133268393, 250.2863559554455719, 14.03735902266321744 ) ) ;
#38742 = ORIENTED_EDGE ( 'NONE', *, *, #51565, .F. ) ;
#38743 = ORIENTED_EDGE ( 'NONE', *, *, #36677, .F. ) ;
#38744 = CARTESIAN_POINT ( 'NONE',  ( 154.0986224399686648, 280.1916420498395155, 2.233781007141098396 ) ) ;
#38745 = CARTESIAN_POINT ( 'NONE',  ( -27.06652637371191616, 106.1054225863516081, 45.19937630303414267 ) ) ;
#38746 = CARTESIAN_POINT ( 'NONE',  ( 82.76604230628169034, 46.51291437311898846, -11.43955186660948620 ) ) ;
#38747 = CARTESIAN_POINT ( 'NONE',  ( 157.8811243250769110, 257.1888664433053009, -17.39256699147873064 ) ) ;
#38748 = CARTESIAN_POINT ( 'NONE',  ( 162.6452507235760265, 248.9371574674245551, -11.74121925143418999 ) ) ;
#38749 = CARTESIAN_POINT ( 'NONE',  ( 85.81045474425822306, 231.8967562850347122, -4.648177544792955347E-16 ) ) ;
#38750 = CARTESIAN_POINT ( 'NONE',  ( 149.6148422561466305, 277.4437614652936190, 3.137689077364430368 ) ) ;
#38751 = EDGE_CURVE ( 'NONE', #22997, #7931, #77419, .T. ) ;
#38752 = CARTESIAN_POINT ( 'NONE',  ( 15.03297158952216961, 188.6744531367911293, 4.594050593750047540 ) ) ;
#38753 = CARTESIAN_POINT ( 'NONE',  ( 126.3990332750161087, 231.5327760586659736, 1.948934522072303157E-15 ) ) ;
#38754 = CARTESIAN_POINT ( 'NONE',  ( 24.48993338297023570, 63.68956773670547733, 59.99999999999999289 ) ) ;
#38755 = EDGE_LOOP ( 'NONE', ( #81046, #33801, #22266, #22749 ) ) ;
#38756 = CARTESIAN_POINT ( 'NONE',  ( 153.4539715540829548, 274.2402401102759768, -12.15832997750954725 ) ) ;
#38757 = EDGE_CURVE ( 'NONE', #16411, #51013, #98968, .T. ) ;
#38758 = CARTESIAN_POINT ( 'NONE',  ( 38.90713653809340400, 79.99999999999998579, -54.99999999999999289 ) ) ;
#38759 = FACE_OUTER_BOUND ( 'NONE', #32503, .T. ) ;
#38760 = CARTESIAN_POINT ( 'NONE',  ( 80.65563100889036718, 57.39222741419450813, -16.23563745603325259 ) ) ;
#38761 = CARTESIAN_POINT ( 'NONE',  ( 48.58805178314242568, 84.67719436603331928, 10.00000000000000000 ) ) ;
#38762 = CARTESIAN_POINT ( 'NONE',  ( 207.1007598919583472, 271.9379569114424271, -6.086525981869248092 ) ) ;
#38763 = CARTESIAN_POINT ( 'NONE',  ( 147.6095889327917803, 274.9796876144846465, -8.460961150142429332 ) ) ;
#38764 = EDGE_CURVE ( 'NONE', #63766, #12823, #68539, .T. ) ;
#38765 = CARTESIAN_POINT ( 'NONE',  ( 189.3809998303445070, 262.9338621993890683, 7.973474124051453948 ) ) ;
#38766 = CARTESIAN_POINT ( 'NONE',  ( 167.7277483666692035, 278.2164418835184279, 14.55005577363578695 ) ) ;
#38767 = CARTESIAN_POINT ( 'NONE',  ( 192.5461644579549159, 265.2488509464530466, 7.905308701533972915 ) ) ;
#38768 = CARTESIAN_POINT ( 'NONE',  ( 70.25824951304763033, 70.48770578870288261, 4.457343381985276132 ) ) ;
#38769 = CARTESIAN_POINT ( 'NONE',  ( 147.6947327179224487, 274.8322142526899370, 9.090449717876689206 ) ) ;
#38770 = DIRECTION ( 'NONE',  ( 0.3613624741150662234, 0.7937185950816985081, 0.4893137583626408493 ) ) ;
#38771 = EDGE_LOOP ( 'NONE', ( #61725, #92801, #85686, #44763 ) ) ;
#38772 = CARTESIAN_POINT ( 'NONE',  ( 152.7033526488152972, 266.7879839391151222, -15.74280670727761233 ) ) ;
#38773 = CARTESIAN_POINT ( 'NONE',  ( 184.0878125373319847, 268.7792329301184964, 16.25146861396065390 ) ) ;
#38774 = CARTESIAN_POINT ( 'NONE',  ( 100.2557178503908517, 222.5643266524160140, 9.188101187500095079 ) ) ;
#38775 = CARTESIAN_POINT ( 'NONE',  ( 20.82171660429349203, 14.94754757982089366, 5.678558825948272215 ) ) ;
#38776 = CARTESIAN_POINT ( 'NONE',  ( -8.493791556357338735, 159.2365022471901455, -10.00000000000009237 ) ) ;
#38777 = AXIS2_PLACEMENT_3D ( 'NONE', #42093, #96339, #3139 ) ;
#38778 = FACE_OUTER_BOUND ( 'NONE', #62436, .T. ) ;
#38779 = CARTESIAN_POINT ( 'NONE',  ( 195.3033857398789621, 278.9466194944354811, 16.29485747049683297 ) ) ;
#38780 = CARTESIAN_POINT ( 'NONE',  ( 196.4543326713419162, 290.3781097766342327, 17.78932051653062274 ) ) ;
#38781 = CARTESIAN_POINT ( 'NONE',  ( 186.8613019359277985, 289.0675096450263482, -15.39881596941752839 ) ) ;
#38782 = CARTESIAN_POINT ( 'NONE',  ( -22.42236680055709641, 157.8615022471902591, 0.000000000000000000 ) ) ;
#38783 = PLANE ( 'NONE',  #83073 ) ;
#38784 = CARTESIAN_POINT ( 'NONE',  ( 204.1793336335251468, 276.6190018376958051, 13.41972674969341206 ) ) ;
#38785 = DIRECTION ( 'NONE',  ( -0.8660254037844387076, -0.4999999999999998890, -0.000000000000000000 ) ) ;
#38786 = ORIENTED_EDGE ( 'NONE', *, *, #65428, .F. ) ;
#38787 = CARTESIAN_POINT ( 'NONE',  ( 192.9292740511494912, 266.8656835997284702, 11.45998025205365423 ) ) ;
#38788 = CARTESIAN_POINT ( 'NONE',  ( 25.62156559687931434, 36.83396525600391413, -2.839279412974133887 ) ) ;
#38789 = CARTESIAN_POINT ( 'NONE',  ( 74.97344113721968029, 63.30522816103469097, -15.06658365657160381 ) ) ;
#38790 = CARTESIAN_POINT ( 'NONE',  ( 82.01068334961553319, 51.50464542205782692, 15.17394240593265664 ) ) ;
#38791 = CARTESIAN_POINT ( 'NONE',  ( 196.7823306783968746, 289.8100005636337073, -17.85370042640856170 ) ) ;
#38792 = VERTEX_POINT ( 'NONE', #7235 ) ;
#38793 = DIRECTION ( 'NONE',  ( -0.000000000000000000, 0.000000000000000000, -1.000000000000000000 ) ) ;
#38794 = CARTESIAN_POINT ( 'NONE',  ( 83.58892928146231327, 42.23796536282910097, 5.791887481487747458 ) ) ;
#38795 = CARTESIAN_POINT ( 'NONE',  ( 183.3038736369663582, 264.5073148912692886, -13.20120179016996254 ) ) ;
#38796 = DIRECTION ( 'NONE',  ( -0.000000000000000000, -0.000000000000000000, -1.000000000000000000 ) ) ;
#38797 = VECTOR ( 'NONE', #5381, 1000.000000000000227 ) ;
#38798 = CARTESIAN_POINT ( 'NONE',  ( 192.1859061758433143, 297.7712413352111298, 11.15082371775444336 ) ) ;
#38799 = CARTESIAN_POINT ( 'NONE',  ( 189.4188400755406292, 280.0569678547571471, 16.65366941511145527 ) ) ;
#38800 = CARTESIAN_POINT ( 'NONE',  ( 36.24780089259745353, 32.87878583063844218, -9.188101187500006262 ) ) ;
#38801 = ORIENTED_EDGE ( 'NONE', *, *, #35795, .F. ) ;
#38802 = CARTESIAN_POINT ( 'NONE',  ( 169.2713223461767313, 284.8094741354592543, 10.92384103809050444 ) ) ;
#38803 = EDGE_CURVE ( 'NONE', #85413, #45858, #42766, .T. ) ;
#38804 = CARTESIAN_POINT ( 'NONE',  ( -22.42236680055709641, 157.8615022471902591, 0.000000000000000000 ) ) ;
#38805 = VERTEX_POINT ( 'NONE', #6246 ) ;
#38806 = CARTESIAN_POINT ( 'NONE',  ( 86.36251143053004853, 47.01529372492075254, -10.02184405881504325 ) ) ;
#38807 = CARTESIAN_POINT ( 'NONE',  ( 159.0779171328172481, 255.1159604941658472, 17.23506282224926522 ) ) ;
#38808 = CARTESIAN_POINT ( 'NONE',  ( 84.45465033531688448, 50.16481452220934756, 13.87013043972112847 ) ) ;
#38809 = CARTESIAN_POINT ( 'NONE',  ( 192.6084828143412437, 297.0393171272406221, -13.31966769178241705 ) ) ;
#38810 = CARTESIAN_POINT ( 'NONE',  ( 81.36927088231499283, 44.63534392387484218, -11.07837440946456553 ) ) ;
#38811 = AXIS2_PLACEMENT_3D ( 'NONE', #98612, #61060, #22576 ) ;
#38812 = CARTESIAN_POINT ( 'NONE',  ( 38.99862784774133928, 37.91421378149922816, 9.188101187500008038 ) ) ;
#38813 = CARTESIAN_POINT ( 'NONE',  ( 80.28413171908289314, 44.31094758583755322, 11.35608167334395446 ) ) ;
#38814 = CARTESIAN_POINT ( 'NONE',  ( 175.7824178399792174, 285.8628427244275372, -13.39878279634721103 ) ) ;
#38815 = ORIENTED_EDGE ( 'NONE', *, *, #88805, .F. ) ;
#38816 = CARTESIAN_POINT ( 'NONE',  ( -63.08903959183645327, 39.77784189046417396, 10.00000000000000000 ) ) ;
#38817 = EDGE_LOOP ( 'NONE', ( #18431, #39801, #77467, #46040 ) ) ;
#38818 = CARTESIAN_POINT ( 'NONE',  ( 81.20643963274024202, 55.68550677472633481, 16.38154045842715334 ) ) ;
#38819 = ORIENTED_EDGE ( 'NONE', *, *, #57166, .F. ) ;
#38820 = CARTESIAN_POINT ( 'NONE',  ( 86.83317331226271563, 45.77437086576020420, -8.734311406240857778 ) ) ;
#38821 = ORIENTED_EDGE ( 'NONE', *, *, #11483, .T. ) ;
#38822 = CARTESIAN_POINT ( 'NONE',  ( 190.6473439991314933, 300.0390052271857826, -3.781200630501462268 ) ) ;
#38823 = CARTESIAN_POINT ( 'NONE',  ( 164.2901811315512077, 246.0880544258967575, -1.801919852217561235 ) ) ;
#38824 = CARTESIAN_POINT ( 'NONE',  ( 199.2409351612726027, 274.1797303067421012, -13.51492913604719703 ) ) ;
#38825 = DIRECTION ( 'NONE',  ( 0.5000000000000002220, -0.8660254037844384856, 0.000000000000000000 ) ) ;
#38826 = CARTESIAN_POINT ( 'NONE',  ( 78.88438918712202508, 46.31898556578845216, 12.90870092474543540 ) ) ;
#38827 = CARTESIAN_POINT ( 'NONE',  ( 171.2101627772172492, 250.9235556046914155, -5.579768846723117015 ) ) ;
#38828 = DIRECTION ( 'NONE',  ( -0.6363689690731114679, -0.7713848165480219343, 0.000000000000000000 ) ) ;
#38829 = EDGE_CURVE ( 'NONE', #4704, #96078, #1721, .T. ) ;
#38830 = CARTESIAN_POINT ( 'NONE',  ( 183.4135727292207605, 284.6015171189660578, -15.04630399923350659 ) ) ;
#38831 = CARTESIAN_POINT ( 'NONE',  ( 113.4351080945290278, 245.4869531367911009, 4.594050593750046652 ) ) ;
#38832 = CARTESIAN_POINT ( 'NONE',  ( 186.6240524511718206, 262.8751839256129301, -9.355389698624779982 ) ) ;
#38833 = CARTESIAN_POINT ( 'NONE',  ( 42.23901261427005949, 30.10170272979930672, -7.433330006724141015 ) ) ;
#38834 = CARTESIAN_POINT ( 'NONE',  ( 177.0439216176413879, 289.2672441982131204, -10.54826698963404041 ) ) ;
#38835 = ORIENTED_EDGE ( 'NONE', *, *, #38972, .T. ) ;
#38836 = EDGE_LOOP ( 'NONE', ( #40555, #51922, #7620, #32089, #29017 ) ) ;
#38837 = CARTESIAN_POINT ( 'NONE',  ( -11.40312891409031693, 78.77562236714182120, 59.99999999999999289 ) ) ;
#38838 = CARTESIAN_POINT ( 'NONE',  ( 76.84140186645967674, 62.34076209027359994, -15.36631987037957181 ) ) ;
#38839 = CARTESIAN_POINT ( 'NONE',  ( 171.1102460733511066, 287.7606437450009480, -4.678464158645172510 ) ) ;
#38840 = CARTESIAN_POINT ( 'NONE',  ( 196.2048238403250764, 290.8102717488927169, 17.53926796892840656 ) ) ;
#38841 = CARTESIAN_POINT ( 'NONE',  ( 72.15377119973463493, 62.27101953176124738, 14.31680684859204078 ) ) ;
#38842 = EDGE_CURVE ( 'NONE', #2203, #9334, #15320, .T. ) ;
#38843 = DIRECTION ( 'NONE',  ( 0.4999999999999992784, -0.8660254037844390407, 0.000000000000000000 ) ) ;
#38844 = CARTESIAN_POINT ( 'NONE',  ( 77.71695824120645568, 49.45779813244274692, 15.33409790704233977 ) ) ;
#38845 = ORIENTED_EDGE ( 'NONE', *, *, #80179, .F. ) ;
#38846 = CARTESIAN_POINT ( 'NONE',  ( 153.5824857651062416, 266.9593715351384731, 16.60156113108486764 ) ) ;
#38847 = EDGE_CURVE ( 'NONE', #55003, #91593, #59024, .T. ) ;
#38848 = CARTESIAN_POINT ( 'NONE',  ( 75.69598090375797028, 54.45081556845784121, -16.58729045400416879 ) ) ;
#38849 = ORIENTED_EDGE ( 'NONE', *, *, #49315, .F. ) ;
#38850 = CARTESIAN_POINT ( 'NONE',  ( 148.3253847707240141, 273.7398928553401447, -9.074433450356286457 ) ) ;
#38851 = CARTESIAN_POINT ( 'NONE',  ( 3.808674319871268921, 184.5530062829863027, -4.648177544792955347E-16 ) ) ;
#38852 = ORIENTED_EDGE ( 'NONE', *, *, #16471, .T. ) ;
#38853 = CARTESIAN_POINT ( 'NONE',  ( 188.1446237001680970, 265.8515323599089584, -11.63103201079399440 ) ) ;
#38854 = AXIS2_PLACEMENT_3D ( 'NONE', #15011, #54001, #55499 ) ;
#38855 = CARTESIAN_POINT ( 'NONE',  ( 190.6739029791876305, 284.0814300001334800, -17.04622756081775492 ) ) ;
#38856 = CARTESIAN_POINT ( 'NONE',  ( 192.3824498117414237, 262.8597123339034738, 4.564481591547765227 ) ) ;
#38857 = LINE ( 'NONE', #76392, #20325 ) ;
#38858 = CARTESIAN_POINT ( 'NONE',  ( 204.6497552248077341, 273.0205207247614680, -10.58234289185253196 ) ) ;
#38860 = CARTESIAN_POINT ( 'NONE',  ( 156.8342227191775464, 280.4122116305982217, 5.959992801529873319 ) ) ;
#38859 = CARTESIAN_POINT ( 'NONE',  ( 153.2402432998383972, 270.1751345723797044, 14.03626019444179818 ) ) ;
#38861 = CARTESIAN_POINT ( 'NONE',  ( 201.0844796915553161, 282.3584598911111812, -16.59562674965125950 ) ) ;
#38862 = ORIENTED_EDGE ( 'NONE', *, *, #84985, .T. ) ;
#38863 = CARTESIAN_POINT ( 'NONE',  ( 147.2443490232117256, 275.6123016948292275, 5.226063659459642352 ) ) ;
#38864 = CARTESIAN_POINT ( 'NONE',  ( 72.28688483481026594, 65.33959170025640617, 12.64045241524083885 ) ) ;
#38865 = CARTESIAN_POINT ( 'NONE',  ( 73.68985795168487130, 65.52845945377288217, 13.58442946136029228 ) ) ;
#38866 = CARTESIAN_POINT ( 'NONE',  ( -19.65312891409030271, 93.06504152958497400, 10.00000000000000888 ) ) ;
#38867 = CARTESIAN_POINT ( 'NONE',  ( 26.27351996285747049, 192.6427522451419634, -10.00000000000009592 ) ) ;
#38868 = CARTESIAN_POINT ( 'NONE',  ( 188.5899576770683836, 298.6136929722685522, -4.164154921440024637 ) ) ;
#38869 = CARTESIAN_POINT ( 'NONE',  ( 72.48280754011685190, 70.60311863597817705, 7.264376673680498442 ) ) ;
#38870 = CARTESIAN_POINT ( 'NONE',  ( 170.7312474266366564, 253.4461053635303358, 11.28381232434868764 ) ) ;
#38871 = VECTOR ( 'NONE', #99815, 1000.000000000000341 ) ;
#38872 = CARTESIAN_POINT ( 'NONE',  ( -13.03246669095222998, 174.8297689869269220, -2.679491924311245832 ) ) ;
#38873 = CARTESIAN_POINT ( 'NONE',  ( 191.5677310693528170, 283.6434865987201874, -16.60331218763614558 ) ) ;
#38874 = EDGE_CURVE ( 'NONE', #39182, #31533, #19841, .T. ) ;
#38875 = CARTESIAN_POINT ( 'NONE',  ( 82.44970526080962259, 53.47733151612504088, -15.75145310647261709 ) ) ;
#38876 = CARTESIAN_POINT ( 'NONE',  ( 74.97842782955004282, 214.0958772461660544, -9.188101187500095079 ) ) ;
#38877 = CARTESIAN_POINT ( 'NONE',  ( 67.85970132199700799, 69.63639107943987483, 4.385596732954796018 ) ) ;
#38878 = CARTESIAN_POINT ( 'NONE',  ( 72.10617024684209753, 72.18421392457030095, 4.031754617348218162 ) ) ;
#38879 = CARTESIAN_POINT ( 'NONE',  ( 180.2008674086625888, 256.3788900776044102, -7.862092545524210330 ) ) ;
#38880 = CARTESIAN_POINT ( 'NONE',  ( 154.8545429534089237, 262.4310591522755089, -17.81746354318405778 ) ) ;
#38881 = B_SPLINE_CURVE_WITH_KNOTS ( 'NONE', 3,
 ( #93874, #94862, #2144, #62923, #32014, #39601, #24431, #25422, #47221, #33025, #31511, #41109, #17845, #78143, #86288, #56821, #62406, #15818, #70016, #93362, #8729, #79175, #25947, #95393, #78647, #54817, #85797, #63924, #71548, #70521, #23919, #32535, #55306, #39102, #48745, #1136, #9754, #24923, #16822, #46722 ),
 .UNSPECIFIED., .F., .F.,
 ( 4, 2, 2, 2, 2, 2, 2, 2, 2, 2, 2, 2, 2, 2, 2, 2, 2, 2, 2, 4 ),
 ( 0.0009045477389935737030, 0.0009985104552911751828, 0.001092473171588776446, 0.001280398604183980490, 0.001656249469374568989, 0.002407951199755620220, 0.003911354660517611659, 0.004663056390898655951, 0.005038907256089211056, 0.005226832688684499018, 0.005320795404982177693, 0.005414758121279858102, 0.005461739479428661878, 0.005508720837577467389, 0.005602683553875100961, 0.005790608986470392391, 0.005978534419065682087, 0.006166459851660971783, 0.006542310716851552910, 0.006918161582042132302 ),
 .UNSPECIFIED. ) ;
#38882 = CARTESIAN_POINT ( 'NONE',  ( 78.53484019558472085, 58.14436697958397104, 16.22033106392862578 ) ) ;
#38883 = CARTESIAN_POINT ( 'NONE',  ( 84.69192290788414823, 50.49093492985745257, -13.55378674288394336 ) ) ;
#38884 = FACE_OUTER_BOUND ( 'NONE', #15903, .T. ) ;
#38886 = CARTESIAN_POINT ( 'NONE',  ( 76.09822188795720876, 51.18568606329870363, 16.10049749365522942 ) ) ;
#38885 = CARTESIAN_POINT ( 'NONE',  ( 73.69504701792554613, 69.38216658601243125, -9.921919506181135162 ) ) ;
#38887 = LINE ( 'NONE', #69790, #88664 ) ;
#38888 = CARTESIAN_POINT ( 'NONE',  ( 169.2950589356292710, 252.1013886194228348, -9.631404982488993127 ) ) ;
#38889 = CARTESIAN_POINT ( 'NONE',  ( 204.9769638368455844, 275.6164795838122927, -13.69608158933077746 ) ) ;
#38890 = CARTESIAN_POINT ( 'NONE',  ( 168.3110316854768485, 273.6977835318167536, 17.00254241999702387 ) ) ;
#38891 = CARTESIAN_POINT ( 'NONE',  ( 157.7861133721078772, 257.3534302411229646, 18.03837896619386783 ) ) ;
#38892 = CARTESIAN_POINT ( 'NONE',  ( -19.65312891409030271, 93.06504152958497400, 10.00000000000000888 ) ) ;
#38893 = CARTESIAN_POINT ( 'NONE',  ( 45.07374842694240868, 187.6423013555410080, -4.594050593750043987 ) ) ;
#38894 = CARTESIAN_POINT ( 'NONE',  ( 64.36996372895568186, 195.7202760586659167, -5.415160957724236172E-17 ) ) ;
#38895 = DIRECTION ( 'NONE',  ( -0.7005979833698863235, -0.7135562106085605594, 0.000000000000000000 ) ) ;
#38896 = CARTESIAN_POINT ( 'NONE',  ( 88.35650425256305596, 44.18871754174234212, 0.2633948951645489478 ) ) ;
#38897 = CARTESIAN_POINT ( 'NONE',  ( 7.727700963378506316, 20.16454794089039382, -10.00000000000000355 ) ) ;
#38898 = CARTESIAN_POINT ( 'NONE',  ( 139.4158702080621879, 260.4869531367911009, 4.594050593750046652 ) ) ;
#38899 = EDGE_CURVE ( 'NONE', #78035, #60981, #35618, .T. ) ;
#38900 = CARTESIAN_POINT ( 'NONE',  ( 197.1913910522388846, 270.0342516794337371, -10.84445706988983460 ) ) ;
#38901 = CARTESIAN_POINT ( 'NONE',  ( 23.73493010604062192, 29.10171378149919974, 9.188101187500008038 ) ) ;
#38902 = CARTESIAN_POINT ( 'NONE',  ( 137.3333197629383449, 238.5494855054051868, -2.679491924311248496 ) ) ;
#38903 = CARTESIAN_POINT ( 'NONE',  ( 148.9831146496684084, 272.6006712873522133, -12.63706091291043343 ) ) ;
#38904 = CARTESIAN_POINT ( 'NONE',  ( 15.97197434310064601, 12.14754757982088940, -5.678558825948276656 ) ) ;
#38905 = CARTESIAN_POINT ( 'NONE',  ( 61.82584055745639517, 200.3768266524159856, -9.188101187500093303 ) ) ;
#38906 = CARTESIAN_POINT ( 'NONE',  ( 159.0704364050992297, 255.7598713771850782, -16.06560598622004576 ) ) ;
#38907 = CARTESIAN_POINT ( 'NONE',  ( 82.80988375738442642, 53.83802849848978411, -15.42793928106117818 ) ) ;
#38908 = CARTESIAN_POINT ( 'NONE',  ( 159.2303255284352304, 254.8519814094557603, 16.39103317446447150 ) ) ;
#38909 = CARTESIAN_POINT ( 'NONE',  ( 73.99071832934600934, 66.66873186589971567, 12.45603791228730550 ) ) ;
#38910 = CARTESIAN_POINT ( 'NONE',  ( 153.3733417098790426, 276.7809054075530639, 7.651122506530271927 ) ) ;
#38911 = CARTESIAN_POINT ( 'NONE',  ( 87.64404534381598921, 45.17643606527867917, -6.176835110407645324 ) ) ;
#38913 =( BOUNDED_CURVE ( )  B_SPLINE_CURVE ( 2, ( #68760, #59658, #99685, #69263, #21193, #92607, #30268, #52071, #75902 ),
 .UNSPECIFIED., .F., .T. ) 
 B_SPLINE_CURVE_WITH_KNOTS ( ( 3, 2, 2, 2, 3 ),
 ( 0.02822580645161290591, 0.02956989247311828106, 0.03225806451612903136, 0.03494623655913978166, 0.03629032258064516375 ),
 .UNSPECIFIED. ) 
 CURVE ( )  GEOMETRIC_REPRESENTATION_ITEM ( )  RATIONAL_B_SPLINE_CURVE ( ( 0.9330127018922192983, 0.9330127018922194093, 1.000000000000000000, 0.8660254037844387076, 1.000000000000000000, 0.8660254037844387076, 1.000000000000000000, 0.9330127018922191873, 0.9330127018922194093 ) ) 
 REPRESENTATION_ITEM ( '' )  );
#38912 = CARTESIAN_POINT ( 'NONE',  ( 102.2852913444020686, 239.8615022471903160, 5.000000000000046185 ) ) ;
#38914 = CARTESIAN_POINT ( 'NONE',  ( 161.6707029936031574, 250.6251236501384483, 14.45053103226186231 ) ) ;
#38915 = CARTESIAN_POINT ( 'NONE',  ( 207.4285356523023154, 271.3702326410368642, 7.833982582429932506 ) ) ;
#38916 = ORIENTED_EDGE ( 'NONE', *, *, #19780, .T. ) ;
#38917 = DIRECTION ( 'NONE',  ( 0.000000000000000000, -0.000000000000000000, 1.000000000000000000 ) ) ;
#38918 = CARTESIAN_POINT ( 'NONE',  ( 82.52272021305054750, 54.20245997282780337, 15.57906378977955164 ) ) ;
#38919 = ORIENTED_EDGE ( 'NONE', *, *, #83623, .T. ) ;
#38920 = CARTESIAN_POINT ( 'NONE',  ( 206.7923762329701276, 272.4720930770340033, -9.496103119940368487 ) ) ;
#38921 = CARTESIAN_POINT ( 'NONE',  ( 186.8221477911302770, 276.5908659110200460, -17.12696914844746843 ) ) ;
#38922 = CARTESIAN_POINT ( 'NONE',  ( 71.50240432004942193, 72.40933122983058468, 5.654570818603106787E-06 ) ) ;
#38923 = ORIENTED_EDGE ( 'NONE', *, *, #48838, .T. ) ;
#38924 = CARTESIAN_POINT ( 'NONE',  ( 173.6959472565854981, 251.9178171641904953, -0.2492449988941567163 ) ) ;
#38925 = EDGE_LOOP ( 'NONE', ( #41359, #74224, #78391, #39166 ) ) ;
#38926 = LINE ( 'NONE', #70331, #26359 ) ;
#38927 = CARTESIAN_POINT ( 'NONE',  ( 194.6356465353167948, 293.5281665672507643, -16.13180903283129197 ) ) ;
#38928 = DIRECTION ( 'NONE',  ( -0.8660254037844387076, -0.4999999999999998890, -0.000000000000000000 ) ) ;
#38929 = VERTEX_POINT ( 'NONE', #73546 ) ;
#38930 = CARTESIAN_POINT ( 'NONE',  ( 31.98500480842837490, 19.26216523072496400, -2.296566073217252530E-15 ) ) ;
#38931 = CARTESIAN_POINT ( 'NONE',  ( 79.98829826360795892, 44.59498145176360140, 11.76229304004083964 ) ) ;
#38932 = CARTESIAN_POINT ( 'NONE',  ( 152.3360070569975449, 270.2436951681156643, -14.78697292633622951 ) ) ;
#38933 = CARTESIAN_POINT ( 'NONE',  ( 75.06695094285402092, 67.05599132900849213, -12.66018568268391853 ) ) ;
#38934 = EDGE_LOOP ( 'NONE', ( #33112, #66126, #72772, #35647 ) ) ;
#38935 = DIRECTION ( 'NONE',  ( -0.8660254037844379305, -0.5000000000000014433, -0.000000000000000000 ) ) ;
#38936 = PLANE ( 'NONE',  #36701 ) ;
#38937 = ORIENTED_EDGE ( 'NONE', *, *, #64057, .T. ) ;
#38938 = AXIS2_PLACEMENT_3D ( 'NONE', #36567, #23356, #22371 ) ;
#38939 = CARTESIAN_POINT ( 'NONE',  ( -2.474071885612758148, 64.61506735976895754, -10.00000000000000000 ) ) ;
#38941 = CARTESIAN_POINT ( 'NONE',  ( 67.92368367061898482, 65.30421490620477698, -10.50538595028323918 ) ) ;
#38940 = CARTESIAN_POINT ( 'NONE',  ( 163.2758796796684067, 283.7716228465783956, -2.991217566210298884 ) ) ;
#38942 = CARTESIAN_POINT ( 'NONE',  ( 207.5886452961740076, 271.0929146030698007, -1.661373005306138184 ) ) ;
#38943 = CARTESIAN_POINT ( 'NONE',  ( 164.1259971043086239, 246.3724295028720519, 5.761669507629934905 ) ) ;
#38944 = CARTESIAN_POINT ( 'NONE',  ( 71.64405606982037966, 72.29848632667865616, -2.396508723004914909 ) ) ;
#38945 = CARTESIAN_POINT ( 'NONE',  ( 157.6668627405778409, 257.5599783937680058, -16.78811156090270629 ) ) ;
#38947 = CARTESIAN_POINT ( 'NONE',  ( 144.4230134433972523, 248.0643266524160140, 9.188101187500095079 ) ) ;
#38946 = B_SPLINE_CURVE_WITH_KNOTS ( 'NONE', 3,
 ( #33821, #40876, #3905, #96642, #26209, #12011, #25716, #41893, #71821, #11023, #35292, #87583, #64709, #27208, #95660, #57086 ),
 .UNSPECIFIED., .F., .F.,
 ( 4, 1, 2, 2, 2, 1, 2, 2, 4 ),
 ( 0.000000000000000000, 0.1250000000000001388, 0.1874999999999999167, 0.2499999999999997224, 0.4999999999999936717, 0.6249999999999927836, 0.6874999999999924505, 0.7499999999999920064, 1.000000000000000000 ),
 .UNSPECIFIED. ) ;
#38948 = CARTESIAN_POINT ( 'NONE',  ( 206.4992971559627506, 270.5621682591477111, 2.903359756976243933 ) ) ;
#38949 = CARTESIAN_POINT ( 'NONE',  ( 178.8741573099551943, 257.7081751745919291, 10.05521247607878088 ) ) ;
#38950 = CARTESIAN_POINT ( 'NONE',  ( 77.57650404090335883, 215.5958772461660544, -9.188101187500095079 ) ) ;
#38951 = ORIENTED_EDGE ( 'NONE', *, *, #77903, .F. ) ;
#38952 = CARTESIAN_POINT ( 'NONE',  ( 191.3375250863502970, 299.2406804863936145, 8.828791580707859410 ) ) ;
#38953 = DIRECTION ( 'NONE',  ( -0.7713848165480284846, 0.6363689690731033632, 0.000000000000000000 ) ) ;
#38954 = ORIENTED_EDGE ( 'NONE', *, *, #73971, .F. ) ;
#38955 = CARTESIAN_POINT ( 'NONE',  ( 177.6444986370304946, 293.6980009803469329, 2.770296639708824227 ) ) ;
#38956 = ORIENTED_EDGE ( 'NONE', *, *, #63360, .F. ) ;
#38957 = B_SPLINE_CURVE_WITH_KNOTS ( 'NONE', 3,
 ( #7849, #92969, #46318, #76270 ),
 .UNSPECIFIED., .F., .F.,
 ( 4, 4 ),
 ( 0.002878795719159728261, 0.006003557113845784873 ),
 .UNSPECIFIED. ) ;
#38958 = CARTESIAN_POINT ( 'NONE',  ( 66.75636626838043242, 67.88323880877007355, 6.998558940700871034 ) ) ;
#38959 = CARTESIAN_POINT ( 'NONE',  ( 191.5521510896938935, 298.8689373439769952, -9.847378829740700112 ) ) ;
#38960 = CARTESIAN_POINT ( 'NONE',  ( 81.23909821190164848, 55.73431417435049440, 16.38583623711208404 ) ) ;
#38961 = CARTESIAN_POINT ( 'NONE',  ( 78.19967833365834053, 48.92268198308481431, -14.50970423465381209 ) ) ;
#38962 = EDGE_CURVE ( 'NONE', #46531, #81472, #48902, .T. ) ;
#38963 = CYLINDRICAL_SURFACE ( 'NONE', #36580, 49.99999999999999289 ) ;
#38964 = CARTESIAN_POINT ( 'NONE',  ( 76.33141897508073725, 221.0024278399160949, 9.188101187500095079 ) ) ;
#38965 = ORIENTED_EDGE ( 'NONE', *, *, #30619, .F. ) ;
#38966 = ADVANCED_FACE ( 'NONE', ( #10750 ), #48757, .F. ) ;
#38967 = ORIENTED_EDGE ( 'NONE', *, *, #9846, .F. ) ;
#38969 = EDGE_CURVE ( 'NONE', #346, #87238, #88794, .T. ) ;
#38968 = CARTESIAN_POINT ( 'NONE',  ( 201.0785059933280650, 282.3688066399498098, -17.20790163225820280 ) ) ;
#38970 = ORIENTED_EDGE ( 'NONE', *, *, #96554, .T. ) ;
#38971 = CARTESIAN_POINT ( 'NONE',  ( 76.41687528450239597, 51.62467577766678772, -15.66419350453952752 ) ) ;
#38972 = EDGE_CURVE ( 'NONE', #10682, #1290, #72054, .T. ) ;
#38973 = CARTESIAN_POINT ( 'NONE',  ( 75.99750771566300500, 65.44421971917600445, -13.95497799904429570 ) ) ;
#38974 = CARTESIAN_POINT ( 'NONE',  ( 196.4287751515431921, 269.1031666285815618, -12.09581130873691279 ) ) ;
#38975 = DIRECTION ( 'NONE',  ( -0.8660254037844387076, -0.4999999999999998890, -0.000000000000000000 ) ) ;
#38976 = CARTESIAN_POINT ( 'NONE',  ( 162.8777320348721673, 261.4784687625029278, 17.43788665286368911 ) ) ;
#38977 = VERTEX_POINT ( 'NONE', #85554 ) ;
#38978 = CARTESIAN_POINT ( 'NONE',  ( 84.01082902402941954, 43.69534178878007680, -7.113612602852647626 ) ) ;
#38979 = CARTESIAN_POINT ( 'NONE',  ( -14.81556294067986457, 35.32291336244301760, 59.99999999999999289 ) ) ;
#38980 = CARTESIAN_POINT ( 'NONE',  ( 155.8995516477446301, 262.1116139477605884, -16.97658656424888335 ) ) ;
#38981 = CARTESIAN_POINT ( 'NONE',  ( 153.1961624462112752, 265.3034584490234806, -16.19494717845262954 ) ) ;
#38982 = B_SPLINE_CURVE_WITH_KNOTS ( 'NONE', 3,
 ( #22177, #15058, #6485, #22683, #76395, #100195, #38860, #31262, #62149, #69266, #45949, #67780, #44966, #53070, #23157, #77382, #68268, #93095, #29289, #99191, #91605, #45462, #6971, #7984, #36874, #37855, #68764, #38356, #61161, #92610, #30780, #69766, #77890, #24174, #70261, #48479, #79421, #1883, #25687, #95122, #40847, #1386, #869, #40353, #62653, #17572, #39346, #86040, #56567, #71793 ),
 .UNSPECIFIED., .F., .F.,
 ( 4, 2, 2, 2, 2, 2, 2, 2, 2, 2, 2, 2, 2, 2, 2, 2, 2, 2, 2, 2, 2, 2, 2, 2, 4 ),
 ( 0.0005289711837892736640, 0.0009717741654603732774, 0.001193175656295859116, 0.001303876401713549397, 0.001414577147131239462, 0.001525277892548929960, 0.001635978637966619808, 0.001857380128802034198, 0.002300183110472862544, 0.003185789073814480638, 0.004071395037156097865, 0.004957001000497714659, 0.005399803982168523489, 0.005621205473003964767, 0.005731906218421648977, 0.005787256591130453785, 0.005842606963839258594, 0.005897957336548063402, 0.005953307709256868210, 0.006064008454674477827, 0.006285409945509695326, 0.006728212927180128589, 0.007171015908850563586, 0.007392417399685759401, 0.007613818890520955215 ),
 .UNSPECIFIED. ) ;
#38983 = CARTESIAN_POINT ( 'NONE',  ( 72.49859375374551007, 70.63268695749106030, 7.230702372335866990 ) ) ;
#38984 = CARTESIAN_POINT ( 'NONE',  ( 67.66477494612622934, 65.93994996590180335, 10.43000742999573482 ) ) ;
#38985 = EDGE_LOOP ( 'NONE', ( #43813, #43929, #59653, #31136 ) ) ;
#38986 = CARTESIAN_POINT ( 'NONE',  ( 199.8133446373031177, 266.7051771727681739, 4.672154848026198515 ) ) ;
#38987 = CARTESIAN_POINT ( 'NONE',  ( 148.2604030792711853, 276.0951355443942248, -3.828504021689099979 ) ) ;
#38988 = DIRECTION ( 'NONE',  ( -0.9957145386939485476, -0.09248003802711830812, 0.000000000000000000 ) ) ;
#38989 = CARTESIAN_POINT ( 'NONE',  ( 187.8793669350804123, 266.2890599608011826, -12.74918944048514469 ) ) ;
#38990 = CARTESIAN_POINT ( 'NONE',  ( 198.6619468263075419, 265.9559996360017635, 1.504078954549255220 ) ) ;
#38991 = CARTESIAN_POINT ( 'NONE',  ( 156.6340579379407245, 272.3087899941822343, 14.25056221956334923 ) ) ;
#38992 = ORIENTED_EDGE ( 'NONE', *, *, #5397, .F. ) ;
#38993 = FACE_OUTER_BOUND ( 'NONE', #56763, .T. ) ;
#38994 = CARTESIAN_POINT ( 'NONE',  ( 202.3425522658138505, 280.1794142728863903, 15.86053073629060961 ) ) ;
#38995 = CARTESIAN_POINT ( 'NONE',  ( 156.6084421796713002, 261.3932165810376205, -17.82046942966612590 ) ) ;
#38997 = CARTESIAN_POINT ( 'NONE',  ( 74.09532166844117285, 55.24532013836130773, 16.12365093312453368 ) ) ;
#38996 = CARTESIAN_POINT ( 'NONE',  ( 194.4904290197884507, 293.7796906822950973, 14.50206953321744940 ) ) ;
#38998 = CARTESIAN_POINT ( 'NONE',  ( 178.3271064952729716, 287.7206632098644263, -13.02025800059123561 ) ) ;
#38999 = CARTESIAN_POINT ( 'NONE',  ( 22.94593010929795085, 36.18080186712593616, 3.090169943749475401 ) ) ;
#39000 = CARTESIAN_POINT ( 'NONE',  ( 168.6260063310307373, 273.1609051843404927, 15.95833444951868429 ) ) ;
#39001 = CARTESIAN_POINT ( 'NONE',  ( 75.43017357788674815, 188.3759306620403891, 30.52142883766498827 ) ) ;
#39002 = CARTESIAN_POINT ( 'NONE',  ( 180.0662822340164269, 262.4007578510376675, -14.24330825748563534 ) ) ;
#39003 = CARTESIAN_POINT ( 'NONE',  ( 188.2447773146031409, 260.7966381918191701, 3.249388362550839293 ) ) ;
#39004 = CARTESIAN_POINT ( 'NONE',  ( -6.536213301660246167, 167.0333772461660828, 9.188101187500095079 ) ) ;
#39005 = CARTESIAN_POINT ( 'NONE',  ( 189.6561516143011659, 295.9170104107913062, -11.61052802970076314 ) ) ;
#39006 = VERTEX_POINT ( 'NONE', #5624 ) ;
#39007 = CARTESIAN_POINT ( 'NONE',  ( 175.3074307085254020, 254.5436327766159650, 9.407465564047683415 ) ) ;
#39008 = CARTESIAN_POINT ( 'NONE',  ( 72.85870443091526738, 70.94102631263370995, -7.807649534274232472 ) ) ;
#39009 = CARTESIAN_POINT ( 'NONE',  ( 81.58528556317443758, 41.69952858397179796, 5.867569315483937231 ) ) ;
#39010 = CARTESIAN_POINT ( 'NONE',  ( 20.93329029645117245, 173.7048013555409796, 4.594050593750051981 ) ) ;
#39011 = EDGE_CURVE ( 'NONE', #75363, #33639, #70593, .T. ) ;
#39012 = CARTESIAN_POINT ( 'NONE',  ( 181.9693517213364089, 275.7599053639374915, -16.43459007604911548 ) ) ;
#39013 = CARTESIAN_POINT ( 'NONE',  ( 31.08397696812772182, 23.11029122506295863, -8.090169943749478065 ) ) ;
#39014 = CARTESIAN_POINT ( 'NONE',  ( 147.2229325088103735, 275.6493961858936927, -0.4918294119671829390 ) ) ;
#39015 = CARTESIAN_POINT ( 'NONE',  ( 81.32995746972275697, 56.15987802315089539, 16.09091581593350639 ) ) ;
#39016 = CARTESIAN_POINT ( 'NONE',  ( 87.18641337702047167, 46.17289800388120113, -8.348801549285765233 ) ) ;
#39017 = CARTESIAN_POINT ( 'NONE',  ( 187.7221740047435219, 259.7727845006203893, -0.7698188447816332047 ) ) ;
#39018 = CARTESIAN_POINT ( 'NONE',  ( 71.97440221194672461, 212.3615022471902591, -10.00000000000009592 ) ) ;
#39019 = CARTESIAN_POINT ( 'NONE',  ( 71.26875018709939980, 66.61859495416860000, -11.15484612302055289 ) ) ;
#39020 = DIRECTION ( 'NONE',  ( 0.4999999999999998890, -0.8660254037844385966, 0.000000000000000000 ) ) ;
#39021 = CARTESIAN_POINT ( 'NONE',  ( 28.21305602519035460, 187.0958772461660544, -9.188101187500095079 ) ) ;
#39022 = CARTESIAN_POINT ( 'NONE',  ( 72.69592421641890212, 70.74456683587561656, -7.971905174712502706 ) ) ;
#39023 = EDGE_CURVE ( 'NONE', #8043, #33367, #94865, .T. ) ;
#39024 = DIRECTION ( 'NONE',  ( 0.000000000000000000, 1.000000000000000000, -0.000000000000000000 ) ) ;
#39025 = CARTESIAN_POINT ( 'NONE',  ( 202.9963324477415654, 270.0117979724515749, -6.355055958317759490 ) ) ;
#39026 = CARTESIAN_POINT ( 'NONE',  ( 198.9590707264871412, 286.0397762054715827, -17.05306195936250191 ) ) ;
#39027 = DIRECTION ( 'NONE',  ( -0.09573633691163400961, -0.9954067278227237692, 0.000000000000000000 ) ) ;
#39028 = DIRECTION ( 'NONE',  ( 0.8660254037844399289, 0.4999999999999977240, -0.000000000000000000 ) ) ;
#39029 = CARTESIAN_POINT ( 'NONE',  ( 159.8940227261901157, 278.4197979795083597, -10.01923854142061998 ) ) ;
#39030 = CARTESIAN_POINT ( 'NONE',  ( -16.26211276271276418, 167.1916292661124714, 6.123233995736853057E-16 ) ) ;
#39031 = CARTESIAN_POINT ( 'NONE',  ( 23.96105869301208813, 16.76004757982090254, 5.678558825948272215 ) ) ;
#39032 = CARTESIAN_POINT ( 'NONE',  ( 8.232026531027987204, 23.49103043416547365, -8.090169943749479842 ) ) ;
#39033 = CARTESIAN_POINT ( 'NONE',  ( 71.91139111156488184, 59.09947579900738646, 15.87520130762167625 ) ) ;
#39034 = CYLINDRICAL_SURFACE ( 'NONE', #54854, 70.00000000000002842 ) ;
#39035 = VERTEX_POINT ( 'NONE', #6633 ) ;
#39036 = CARTESIAN_POINT ( 'NONE',  ( 9.941082954516852865, 14.24335787977761214, -9.188101187500008038 ) ) ;
#39037 = CARTESIAN_POINT ( 'NONE',  ( 74.59194231731085267, 59.40658604406281995, -15.72090067485143550 ) ) ;
#39038 = CARTESIAN_POINT ( 'NONE',  ( 81.89930626884697062, 42.21375885363389813, 7.647715624881986862 ) ) ;
#39039 = CARTESIAN_POINT ( 'NONE',  ( 44.42076818640806835, 30.81029122506298634, 8.090169943749479842 ) ) ;
#39040 = ORIENTED_EDGE ( 'NONE', *, *, #5839, .T. ) ;
#39041 = CARTESIAN_POINT ( 'NONE',  ( 72.33760062768145360, 71.68797599686796218, -5.790821312261726916 ) ) ;
#39042 = DIRECTION ( 'NONE',  ( -0.4999999999999997224, 0.8660254037844387076, 0.000000000000000000 ) ) ;
#39043 = CARTESIAN_POINT ( 'NONE',  ( 83.06993023455761715, 40.79143924675896926, 1.309702138887457679 ) ) ;
#39044 = VERTEX_POINT ( 'NONE', #82685 ) ;
#39045 = EDGE_LOOP ( 'NONE', ( #37132, #67012, #77015, #72028 ) ) ;
#39047 = CARTESIAN_POINT ( 'NONE',  ( 87.35151617023949200, 43.63067449739911297, -0.4462371624748913690 ) ) ;
#39046 = CARTESIAN_POINT ( 'NONE',  ( 189.6119997129436854, 274.5211355351512452, -16.98768979124082534 ) ) ;
#39048 = ORIENTED_EDGE ( 'NONE', *, *, #38570, .T. ) ;
#39049 = CARTESIAN_POINT ( 'NONE',  ( 191.1489696025915919, 299.5672681643093256, 8.892130899335590755 ) ) ;
#39050 = CARTESIAN_POINT ( 'NONE',  ( 69.61585729181811644, 63.78595448314586491, 13.21249610887674208 ) ) ;
#39051 = CARTESIAN_POINT ( 'NONE',  ( 72.88508378922313113, 56.80021903471959632, -15.95571064693559293 ) ) ;
#39052 = CARTESIAN_POINT ( 'NONE',  ( 77.30463285345523161, 63.36080703450485174, 15.53535672671000079 ) ) ;
#39053 = CARTESIAN_POINT ( 'NONE',  ( 147.6430623265936219, 274.9217099957185155, 8.258152514891218487 ) ) ;
#39054 = CARTESIAN_POINT ( 'NONE',  ( -19.65312891409030271, 93.06504152958497400, -54.99999999999999289 ) ) ;
#39055 = ORIENTED_EDGE ( 'NONE', *, *, #33619, .F. ) ;
#39056 = CARTESIAN_POINT ( 'NONE',  ( 195.7617614321055157, 291.5776783508526364, 16.33009124109666033 ) ) ;
#39057 = CARTESIAN_POINT ( 'NONE',  ( 178.2682848727497742, 278.5227009152765163, -17.33614543379448136 ) ) ;
#39058 = VERTEX_POINT ( 'NONE', #68416 ) ;
#39059 = CARTESIAN_POINT ( 'NONE',  ( 26.01788259378743717, 35.99752408145593563, 5.678558825948277544 ) ) ;
#39060 = ADVANCED_FACE ( 'NONE', ( #400 ), #1983, .F. ) ;
#39061 = CARTESIAN_POINT ( 'NONE',  ( 190.6023073677431512, 300.5141149296460981, 3.174888932019753973 ) ) ;
#39062 = CARTESIAN_POINT ( 'NONE',  ( 71.63103492117565452, 72.07843208848032646, 3.395715836721224790 ) ) ;
#39063 = ORIENTED_EDGE ( 'NONE', *, *, #14341, .F. ) ;
#39064 = CARTESIAN_POINT ( 'NONE',  ( 207.1610391518539984, 269.8335501706607715, 0.000000000000000000 ) ) ;
#39065 = CARTESIAN_POINT ( 'NONE',  ( 184.1240780222136095, 289.0015729834078684, -14.54488561116068901 ) ) ;
#39066 = CARTESIAN_POINT ( 'NONE',  ( 185.4867332780130766, 297.4061142773095412, 5.671143563000668131 ) ) ;
#39067 = CARTESIAN_POINT ( 'NONE',  ( 83.56942396399851702, 52.37055672471088741, 14.78365564216985639 ) ) ;
#39068 = ORIENTED_EDGE ( 'NONE', *, *, #49491, .F. ) ;
#39069 = VECTOR ( 'NONE', #35700, 1000.000000000000114 ) ;
#39070 = EDGE_LOOP ( 'NONE', ( #7160, #23406, #78255, #39729 ) ) ;
#39071 = CARTESIAN_POINT ( 'NONE',  ( 87.78081971166569986, 44.10618430004836910, 2.676874261813567468 ) ) ;
#39072 = CARTESIAN_POINT ( 'NONE',  ( 199.9502294570856407, 265.6703872523112295, 6.360370400932541246E-13 ) ) ;
#39073 = CARTESIAN_POINT ( 'NONE',  ( 147.6857584380539095, 274.8477581613835810, 8.112022437684441201 ) ) ;
#39074 = ORIENTED_EDGE ( 'NONE', *, *, #45604, .F. ) ;
#39075 = CARTESIAN_POINT ( 'NONE',  ( 190.0896302098338424, 301.4020978150248311, 3.433521196325825642 ) ) ;
#39076 = CARTESIAN_POINT ( 'NONE',  ( 132.4598011448335058, 258.8297689869269220, -2.679491924311252493 ) ) ;
#39077 = CARTESIAN_POINT ( 'NONE',  ( 161.1061647010182583, 251.6029326557136585, -13.56144933775657613 ) ) ;
#39078 = EDGE_CURVE ( 'NONE', #15116, #3513, #58571, .T. ) ;
#39079 = CARTESIAN_POINT ( 'NONE',  ( 146.7842303614460207, 276.4092505945183689, -4.491116827832889236 ) ) ;
#39080 = CARTESIAN_POINT ( 'NONE',  ( 159.9162261860523699, 255.4583558200632751, 16.33510284766913045 ) ) ;
#39081 = CARTESIAN_POINT ( 'NONE',  ( 69.01174091589227544, 65.49457112254064839, 10.95257573316000688 ) ) ;
#39082 = CARTESIAN_POINT ( 'NONE',  ( 85.92648014804265699, 231.9637435831425023, 2.679491924311251605 ) ) ;
#39083 = CARTESIAN_POINT ( 'NONE',  ( 67.41087925495308752, 66.60807491237166289, 8.627370698444245534 ) ) ;
#39084 = CARTESIAN_POINT ( 'NONE',  ( 70.51113942130736234, 65.45616864928850021, -11.75070865024357403 ) ) ;
#39085 = CARTESIAN_POINT ( 'NONE',  ( 78.30366600412818912, 47.44550441188034995, 14.31860126704143532 ) ) ;
#39086 = CARTESIAN_POINT ( 'NONE',  ( 121.0403275412173656, 234.5643266524160140, 9.188101187500095079 ) ) ;
#39087 = ORIENTED_EDGE ( 'NONE', *, *, #41816, .F. ) ;
#39088 = CARTESIAN_POINT ( 'NONE',  ( 149.0702641876670214, 272.4497238596823649, -12.82991616757612974 ) ) ;
#39089 = CARTESIAN_POINT ( 'NONE',  ( 70.14510041679191943, 64.94605215490624062, 11.99719282233523288 ) ) ;
#39090 = CARTESIAN_POINT ( 'NONE',  ( 176.5752601597114335, 288.5842064133888130, 11.38490813771325350 ) ) ;
#39091 = CARTESIAN_POINT ( 'NONE',  ( 155.6048174803203210, 261.1315455520403361, -17.38645169541727498 ) ) ;
#39092 = B_SPLINE_CURVE_WITH_KNOTS ( 'NONE', 3,
 ( #28293, #98221, #92153, #22197 ),
 .UNSPECIFIED., .F., .F.,
 ( 4, 4 ),
 ( 1.001342737176739535E-16, 0.002470176110450654407 ),
 .UNSPECIFIED. ) ;
#39093 = CARTESIAN_POINT ( 'NONE',  ( 183.2867325885053731, 284.6525227658081008, -14.98979207437814942 ) ) ;
#39094 = CARTESIAN_POINT ( 'NONE',  ( 83.53129465503697304, 51.49339246050250551, -14.42226391936362973 ) ) ;
#39095 = CARTESIAN_POINT ( 'NONE',  ( 169.3011938600986355, 285.2037582914177847, -7.848347211270669810 ) ) ;
#39096 = ORIENTED_EDGE ( 'NONE', *, *, #90618, .F. ) ;
#39097 = CARTESIAN_POINT ( 'NONE',  ( 80.25077290097513583, 58.18867766503439043, -16.60702595570231566 ) ) ;
#39098 = CARTESIAN_POINT ( 'NONE',  ( 72.01291228344958029, 71.60916324447191528, 5.531298035833725812 ) ) ;
#39099 = CARTESIAN_POINT ( 'NONE',  ( 74.62401959271109320, 66.89443057110611335, 13.05059976691391377 ) ) ;
#39100 = CARTESIAN_POINT ( 'NONE',  ( 128.5097966488581562, 238.8768266524159856, 9.188101187500096856 ) ) ;
#39101 = CARTESIAN_POINT ( 'NONE',  ( 150.9115585710837877, 269.2605084359132093, -15.80434701481532578 ) ) ;
#39102 = CARTESIAN_POINT ( 'NONE',  ( 185.6974139818678395, 297.0515939156086915, 4.189404417500578681 ) ) ;
#39103 = CARTESIAN_POINT ( 'NONE',  ( 187.8012813670164007, 281.6076117757134512, -17.61501541281564442 ) ) ;
#39104 = DIRECTION ( 'NONE',  ( -0.000000000000000000, -0.000000000000000000, 1.000000000000000000 ) ) ;
#39105 = CARTESIAN_POINT ( 'NONE',  ( 40.25596147474394826, 203.2369531367911293, -4.594050593750048428 ) ) ;
#39106 = DIRECTION ( 'NONE',  ( 0.000000000000000000, -0.000000000000000000, 1.000000000000000000 ) ) ;
#39107 = VERTEX_POINT ( 'NONE', #53684 ) ;
#39108 = CARTESIAN_POINT ( 'NONE',  ( 70.74303910967452680, 62.45564769402658101, 13.80964952784702504 ) ) ;
#39109 = CARTESIAN_POINT ( 'NONE',  ( 187.7806315037265108, 258.7815634600612498, -2.095649164382547003 ) ) ;
#39110 = B_SPLINE_SURFACE_WITH_KNOTS ( 'NONE', 3, 1, ( 
 ( #30631, #61516 ),
 ( #91462, #75252 ),
 ( #92463, #15404 ),
 ( #67625, #6333 ),
 ( #46297, #30124 ),
 ( #224, #22527 ),
 ( #29632, #76253 ),
 ( #77224, #60505 ),
 ( #7830, #61007 ),
 ( #22023, #31108 ),
 ( #53417, #37711 ),
 ( #92948, #54393 ),
 ( #44812, #6825 ),
 ( #52923, #83369 ),
 ( #85369, #83874 ),
 ( #44320, #98559 ),
 ( #29144, #60015 ),
 ( #90979, #63020 ),
 ( #24518, #94963 ),
 ( #16417, #86885 ),
 ( #85893, #8327 ),
 ( #16913, #32110 ),
 ( #17941, #40708 ),
 ( #2746, #71144 ),
 ( #55891, #25528 ),
 ( #54914, #47312 ),
 ( #47802, #8819 ),
 ( #48840, #39687 ),
 ( #62494, #56416 ),
 ( #31603, #32622 ),
 ( #79275, #17418 ) ),
 .UNSPECIFIED., .F., .F., .F.,
 ( 4, 3, 3, 3, 3, 3, 3, 3, 3, 3, 4 ),
 ( 2, 2 ),
 ( 0.000000000000000000, 0.1333490885032429241, 0.3007194338854423110, 0.4699862290245206409, 0.5844252810809303922, 0.6686540514502636867, 0.7354980260655383795, 0.8028463152565493699, 0.8633854507757111607, 0.9437142632667171460, 1.000000000000000000 ),
 ( 0.000000000000000000, 1.000000000000000000 ),
 .UNSPECIFIED. ) ;
#39111 = FACE_OUTER_BOUND ( 'NONE', #91120, .T. ) ;
#39112 = B_SPLINE_CURVE_WITH_KNOTS ( 'NONE', 3,
 ( #48410, #93544, #94047, #32200 ),
 .UNSPECIFIED., .F., .F.,
 ( 4, 4 ),
 ( 0.007058328506315592749, 0.01518834970152095967 ),
 .UNSPECIFIED. ) ;
#39113 = CARTESIAN_POINT ( 'NONE',  ( 35.24274519906763459, 113.7842027444719406, 59.99999999999999289 ) ) ;
#39114 = CARTESIAN_POINT ( 'NONE',  ( 81.90827648927033522, 41.78436240737912755, -5.623587741670904805 ) ) ;
#39115 = CARTESIAN_POINT ( 'NONE',  ( 203.5258219653775313, 278.1299310341851765, -16.21052911601769608 ) ) ;
#39116 = CARTESIAN_POINT ( 'NONE',  ( 178.3765882103122635, 261.1946448298811561, 12.30242364351752471 ) ) ;
#39117 = CARTESIAN_POINT ( 'NONE',  ( 109.5562962934610738, 227.3927522451417929, -10.00000000000009059 ) ) ;
#39118 = CARTESIAN_POINT ( 'NONE',  ( 193.9796946036068164, 292.6643086402947915, -15.64068455845557537 ) ) ;
#39119 = ORIENTED_EDGE ( 'NONE', *, *, #73954, .F. ) ;
#39120 = CARTESIAN_POINT ( 'NONE',  ( 147.7157269441172218, 274.7958511862549926, 8.036290321896261801 ) ) ;
#39121 = CARTESIAN_POINT ( 'NONE',  ( 88.03377929273251823, 44.78256942470972035, 4.638045985396566095 ) ) ;
#39122 = EDGE_CURVE ( 'NONE', #56639, #1578, #96840, .T. ) ;
#39123 = CARTESIAN_POINT ( 'NONE',  ( 29.05227845693028854, 178.3923013555409796, 4.594050593750050204 ) ) ;
#39124 = CARTESIAN_POINT ( 'NONE',  ( 7.905500100003217234, 28.65659080271449000, -1.878358725466461243E-16 ) ) ;
#39125 = CARTESIAN_POINT ( 'NONE',  ( 39.77289032284285497, 58.49985355908045648, -10.00000000000000000 ) ) ;
#39126 = CYLINDRICAL_SURFACE ( 'NONE', #98308, 1.449999999999993072 ) ;
#39127 = CARTESIAN_POINT ( 'NONE',  ( 72.06779285608921271, 72.04837681130726423, 2.871792874092435000 ) ) ;
#39129 = CARTESIAN_POINT ( 'NONE',  ( 69.56611615166231388, 198.7202760586659736, -5.415160957724236172E-17 ) ) ;
#39128 = CARTESIAN_POINT ( 'NONE',  ( 176.7336046869569088, 287.5723076295245733, 10.59130312256274564 ) ) ;
#39130 = EDGE_CURVE ( 'NONE', #26521, #7348, #54176, .T. ) ;
#39131 = CARTESIAN_POINT ( 'NONE',  ( 208.3132655666949233, 269.8378354783333180, 2.688523655043302707 ) ) ;
#39132 = CARTESIAN_POINT ( 'NONE',  ( 73.60933432321982650, 55.64367109616565443, 16.10230547196763595 ) ) ;
#39133 = CARTESIAN_POINT ( 'NONE',  ( -30.69451156873374487, 96.82744408686065185, 44.54218732323495544 ) ) ;
#39134 = CARTESIAN_POINT ( 'NONE',  ( 17.89217828605986327, 10.73415679381820986, 1.333680081654574804E-15 ) ) ;
#39135 = VERTEX_POINT ( 'NONE', #91740 ) ;
#39136 = CARTESIAN_POINT ( 'NONE',  ( 29.10614472461704949, 177.6115022471902023, -5.000000000000041744 ) ) ;
#39137 = DIRECTION ( 'NONE',  ( 0.8660254037844395958, 0.4999999999999985567, 0.000000000000000000 ) ) ;
#39138 = CARTESIAN_POINT ( 'NONE',  ( -7.645548028435306342, 157.2048013555409796, 4.594050593750051981 ) ) ;
#39139 = CARTESIAN_POINT ( 'NONE',  ( 31.65185205300530313, 23.98920272979928114, 7.433330006724137462 ) ) ;
#39142 = ADVANCED_FACE ( 'NONE', ( #60283 ), #8113, .T. ) ;
#39141 = CARTESIAN_POINT ( 'NONE',  ( 200.2855905910826664, 282.2403571352788276, 17.19125751069146801 ) ) ;
#39140 = CARTESIAN_POINT ( 'NONE',  ( 164.2175316724671177, 260.1791609587825178, -16.14942496352231416 ) ) ;
#39143 = CARTESIAN_POINT ( 'NONE',  ( 185.5939859232946674, 260.4830921086240210, 6.337058001680582642 ) ) ;
#39144 = CARTESIAN_POINT ( 'NONE',  ( 164.8849641302980444, 245.0578600525887794, 2.884140591399200648 ) ) ;
#39145 = CARTESIAN_POINT ( 'NONE',  ( 88.35595341439740480, 43.98873182231152867, 2.401576318819967693 ) ) ;
#39146 = CARTESIAN_POINT ( 'NONE',  ( 66.08603031403475825, 68.56143032305313056, 2.184140419465945726 ) ) ;
#39147 = ORIENTED_EDGE ( 'NONE', *, *, #74300, .F. ) ;
#39148 = CARTESIAN_POINT ( 'NONE',  ( 181.7987620307110603, 287.9999103646144363, 13.73581616295024688 ) ) ;
#39149 = CARTESIAN_POINT ( 'NONE',  ( 196.6975304897132162, 289.5045102203591796, 16.45742868403355530 ) ) ;
#39150 = CARTESIAN_POINT ( 'NONE',  ( 4.836955906052805787, 24.83396525600387861, -2.839279412974133887 ) ) ;
#39151 = ORIENTED_EDGE ( 'NONE', *, *, #29961, .F. ) ;
#39152 = CARTESIAN_POINT ( 'NONE',  ( 206.4829433911860406, 273.0080464805345173, 8.621361281597655690 ) ) ;
#39153 = CARTESIAN_POINT ( 'NONE',  ( 157.1002372043759010, 258.5414026113353430, -17.73553732786789539 ) ) ;
#39154 = CARTESIAN_POINT ( 'NONE',  ( 71.78057061738425659, 72.16630549687447171, 0.5834590807434386628 ) ) ;
#39155 = EDGE_CURVE ( 'NONE', #85624, #4197, #24659, .T. ) ;
#39156 = CARTESIAN_POINT ( 'NONE',  ( 192.6470966816805230, 296.9724359471326807, 11.11268290051284424 ) ) ;
#39157 = LINE ( 'NONE', #7282, #59486 ) ;
#39159 = CARTESIAN_POINT ( 'NONE',  ( 149.8083888948594335, 271.5779462620446338, 11.70101749353969645 ) ) ;
#39158 = B_SPLINE_CURVE_WITH_KNOTS ( 'NONE', 3,
 ( #24259, #55137, #86122, #86616 ),
 .UNSPECIFIED., .F., .F.,
 ( 4, 4 ),
 ( 0.008993077315648693310, 0.01492662969474104623 ),
 .UNSPECIFIED. ) ;
#39160 = CARTESIAN_POINT ( 'NONE',  ( 162.6262389125959373, 248.9700868899859074, -10.50380342094597808 ) ) ;
#39161 = CARTESIAN_POINT ( 'NONE',  ( 201.3505934466285510, 281.8975373467312693, -16.83770227898004279 ) ) ;
#39162 = VERTEX_POINT ( 'NONE', #504 ) ;
#39163 = ORIENTED_EDGE ( 'NONE', *, *, #2985, .T. ) ;
#39164 = CARTESIAN_POINT ( 'NONE',  ( 42.45923888023187232, 122.5484010731363043, -10.00000000000000000 ) ) ;
#39165 = CARTESIAN_POINT ( 'NONE',  ( 72.72687233632774451, 70.81140904708308881, 7.152679309755922255 ) ) ;
#39166 = ORIENTED_EDGE ( 'NONE', *, *, #75659, .F. ) ;
#39167 = CARTESIAN_POINT ( 'NONE',  ( 198.4097421844162170, 265.0824675037606539, -3.039349057205883664 ) ) ;
#39168 = CARTESIAN_POINT ( 'NONE',  ( -86.81108781737714253, 0.000000000000000000, 0.000000000000000000 ) ) ;
#39169 = ORIENTED_EDGE ( 'NONE', *, *, #21839, .T. ) ;
#39170 = CARTESIAN_POINT ( 'NONE',  ( 109.9999999999999716, 10.00000000000004086, -14.21260523776213347 ) ) ;
#39171 = CARTESIAN_POINT ( 'NONE',  ( 79.13855990483197900, 59.10183223203091529, -16.21630931228972372 ) ) ;
#39172 = CARTESIAN_POINT ( 'NONE',  ( 196.5114383562724072, 290.2791998289336561, -17.87308875047256862 ) ) ;
#39174 = VECTOR ( 'NONE', #10672, 1000.000000000000114 ) ;
#39173 = CARTESIAN_POINT ( 'NONE',  ( 70.02188392290977959, 62.77544136721036239, 13.38372670034021894 ) ) ;
#39175 = EDGE_LOOP ( 'NONE', ( #42597, #18688, #82131 ) ) ;
#39176 = CARTESIAN_POINT ( 'NONE',  ( 200.5810378487751393, 283.2304467414622877, 18.38516374632547112 ) ) ;
#39177 = CARTESIAN_POINT ( 'NONE',  ( 151.2648146047323507, 268.6486510375538614, 15.71323890031163550 ) ) ;
#39178 = CARTESIAN_POINT ( 'NONE',  ( 179.4722142099873565, 269.7276464518548096, -17.35046799866735157 ) ) ;
#39179 = ORIENTED_EDGE ( 'NONE', *, *, #20552, .F. ) ;
#39180 = EDGE_CURVE ( 'NONE', #13801, #16332, #60886, .T. ) ;
#39181 = ORIENTED_EDGE ( 'NONE', *, *, #27802, .F. ) ;
#39182 = VERTEX_POINT ( 'NONE', #78016 ) ;
#39183 = CARTESIAN_POINT ( 'NONE',  ( 74.12068342383874153, 64.67028550015082544, 13.75713335287279193 ) ) ;
#39184 = VERTEX_POINT ( 'NONE', #52691 ) ;
#39185 = CARTESIAN_POINT ( 'NONE',  ( 160.5099781893591455, 258.1706592185460067, -17.21824937912870013 ) ) ;
#39186 = ORIENTED_EDGE ( 'NONE', *, *, #93127, .T. ) ;
#39187 = EDGE_CURVE ( 'NONE', #20674, #44016, #31393, .T. ) ;
#39188 = CARTESIAN_POINT ( 'NONE',  ( 208.1876422586379647, 270.0554214305024630, 3.377638779759113863 ) ) ;
#39189 = CARTESIAN_POINT ( 'NONE',  ( 83.09975762653809284, 48.63870101769774124, 12.90973747663798576 ) ) ;
#39190 = CARTESIAN_POINT ( 'NONE',  ( 167.7205243766922536, 281.0751846570960879, 11.60013190390802151 ) ) ;
#39191 = CARTESIAN_POINT ( 'NONE',  ( 147.7467138384290308, 274.7421803109381813, -9.190172068879620682 ) ) ;
#39192 = EDGE_CURVE ( 'NONE', #70394, #77615, #36982, .T. ) ;
#39193 = DIRECTION ( 'NONE',  ( -0.000000000000000000, -0.000000000000000000, -1.000000000000000000 ) ) ;
#39194 = EDGE_CURVE ( 'NONE', #74996, #20915, #90151, .T. ) ;
#39195 = CARTESIAN_POINT ( 'NONE',  ( 190.3443929803903814, 298.9608357525441420, -8.219721500574586059 ) ) ;
#39196 = AXIS2_PLACEMENT_3D ( 'NONE', #64542, #33135, #2255 ) ;
#39197 = CARTESIAN_POINT ( 'NONE',  ( 164.5259176133158689, 246.1953198488120051, 1.882264443804981813 ) ) ;
#39198 = CARTESIAN_POINT ( 'NONE',  ( 9.881553883097156543, 27.74646525600388713, 2.839279412974139660 ) ) ;
#39199 = CARTESIAN_POINT ( 'NONE',  ( 198.3993091967326166, 277.2393576875207373, -15.29194110241194160 ) ) ;
#39200 = CARTESIAN_POINT ( 'NONE',  ( 80.19730562280793151, 57.80653512312768783, 16.60264294324888468 ) ) ;
#39202 = VERTEX_POINT ( 'NONE', #46082 ) ;
#39201 = CARTESIAN_POINT ( 'NONE',  ( 198.1230806404959139, 287.4877535090322453, 17.00698319228197164 ) ) ;
#39203 = EDGE_CURVE ( 'NONE', #83781, #26122, #93642, .T. ) ;
#39204 = CARTESIAN_POINT ( 'NONE',  ( 110.0000000000000142, 10.00000000000004086, 59.99999999999999289 ) ) ;
#39205 = CARTESIAN_POINT ( 'NONE',  ( -64.94778771796556782, 41.33875607593970614, 10.00000000000000000 ) ) ;
#39206 = EDGE_CURVE ( 'NONE', #62642, #82127, #44021, .T. ) ;
#39207 = CARTESIAN_POINT ( 'NONE',  ( 159.8597520197352537, 253.7617827468940277, -16.74905990210778839 ) ) ;
#39208 = PLANE ( 'NONE',  #39196 ) ;
#39209 =( BOUNDED_CURVE ( )  B_SPLINE_CURVE ( 2, ( #17070, #71800, #94615, #9993, #48486, #87046, #25172, #32771, #56053 ),
 .UNSPECIFIED., .F., .T. ) 
 B_SPLINE_CURVE_WITH_KNOTS ( ( 3, 2, 2, 2, 3 ),
 ( 0.5685483870967742437, 0.5698924731182796188, 0.5725806451612903691, 0.5752688172043011194, 0.5766129032258064946 ),
 .UNSPECIFIED. ) 
 CURVE ( )  GEOMETRIC_REPRESENTATION_ITEM ( )  RATIONAL_B_SPLINE_CURVE ( ( 0.9330127018922194093, 0.9330127018922194093, 1.000000000000000000, 0.8660254037844387076, 1.000000000000000000, 0.8660254037844387076, 1.000000000000000000, 0.9330127018922194093, 0.9330127018922194093 ) ) 
 REPRESENTATION_ITEM ( '' )  );
#39210 = CARTESIAN_POINT ( 'NONE',  ( 81.11448992224303822, 46.11779734161436295, -11.84940212323523667 ) ) ;
#39211 = DIRECTION ( 'NONE',  ( -0.000000000000000000, 0.000000000000000000, -1.000000000000000000 ) ) ;
#39212 = CARTESIAN_POINT ( 'NONE',  ( -24.40473831032599605, 23.22649767201584581, 177.5919119679930134 ) ) ;
#39213 = VERTEX_POINT ( 'NONE', #29414 ) ;
#39215 = CARTESIAN_POINT ( 'NONE',  ( 193.8198143686853712, 294.9412293303058732, -14.86391783401530553 ) ) ;
#39214 = B_SPLINE_CURVE_WITH_KNOTS ( 'NONE', 3,
 ( #44742, #15844, #45738, #23440, #29081, #68552, #45253, #37641, #21466, #159, #69048, #46753, #99978, #77154, #30562, #76188, #53353, #60945, #38130, #52354, #69554, #85301, #77680, #13863, #92886, #6262, #61446, #37158, #68057, #53834, #84794, #7756, #71574, #86817, #94890, #39627, #93393, #62950, #40134, #47736, #87340, #2171, #85825, #41642, #49263, #17872, #48769, #8755 ),
 .UNSPECIFIED., .F., .F.,
 ( 4, 2, 2, 2, 2, 2, 2, 2, 2, 2, 2, 2, 2, 2, 2, 2, 2, 2, 2, 2, 2, 2, 2, 4 ),
 ( 0.002781645625483006659, 0.003194136222294276066, 0.003297258871497089731, 0.003400381520699903397, 0.003503504169902717062, 0.003606626819105530728, 0.003812872117511218774, 0.004019117415916907687, 0.004431608012728316739, 0.005256589206351068057, 0.006081570399973819374, 0.006906551593596570691, 0.007731532787219322009, 0.007834655436422123531, 0.007886216761023559854, 0.007937778085624996177, 0.007989339410226430765, 0.008040900734827867088, 0.008144023384030739734, 0.008556513980842487058, 0.008762759279248379801, 0.008969004577654274279, 0.009175249876060167023, 0.009381495174466059767 ),
 .UNSPECIFIED. ) ;
#39216 = CARTESIAN_POINT ( 'NONE',  ( 137.2172943591538967, 238.4824982072973967, 3.021315404115420679E-15 ) ) ;
#39217 = CARTESIAN_POINT ( 'NONE',  ( -22.42236680055709641, 157.8615022471902591, 0.000000000000000000 ) ) ;
#39218 = CARTESIAN_POINT ( 'NONE',  ( 9.458193372709645885, 176.2677522451418497, 10.00000000000009592 ) ) ;
#39219 = CARTESIAN_POINT ( 'NONE',  ( 87.02133327910362937, 230.2369531367911009, -4.594050593750048428 ) ) ;
#39220 = CARTESIAN_POINT ( 'NONE',  ( 33.92732256784238132, 47.61654385008751689, -10.00000000000000000 ) ) ;
#39221 = FACE_OUTER_BOUND ( 'NONE', #81467, .T. ) ;
#39222 = CARTESIAN_POINT ( 'NONE',  ( 168.4958712465444819, 279.2003023517014526, -13.40781613193690802 ) ) ;
#39223 = CARTESIAN_POINT ( 'NONE',  ( 4.424420716760506522, 173.3615022471902591, -10.00000000000009592 ) ) ;
#39225 = CARTESIAN_POINT ( 'NONE',  ( 75.57301432718394096, 65.50289043567833858, 13.81433800577013926 ) ) ;
#39224 = CARTESIAN_POINT ( 'NONE',  ( 5.371288904610766579, 186.1589784336661637, -6.496448406907675876E-16 ) ) ;
#39226 = CARTESIAN_POINT ( 'NONE',  ( 161.0952649348064938, 251.6218116045831437, 13.81854265722852482 ) ) ;
#39227 = ORIENTED_EDGE ( 'NONE', *, *, #50081, .F. ) ;
#39229 = ORIENTED_EDGE ( 'NONE', *, *, #59202, .T. ) ;
#39228 = PRODUCT_DEFINITION_CONTEXT ( 'detailed design', #33745, 'design' ) ;
#39230 = CARTESIAN_POINT ( 'NONE',  ( 6.396987757676594555, 15.64441083166260427, 0.000000000000000000 ) ) ;
#39231 = CARTESIAN_POINT ( 'NONE',  ( 189.0804396436501236, 261.2380845551991229, -6.138920082207003581 ) ) ;
#39232 = CARTESIAN_POINT ( 'NONE',  ( 86.04723689193814096, 45.96568028731314115, -8.941333467903920251 ) ) ;
#39233 = CARTESIAN_POINT ( 'NONE',  ( 202.1579274701688291, 280.4991937992804765, -15.90174466444106649 ) ) ;
#39234 = CARTESIAN_POINT ( 'NONE',  ( 74.27850899688687036, 68.48602583890969697, -11.15250335310150298 ) ) ;
#39235 = CARTESIAN_POINT ( 'NONE',  ( 37.36027580478098287, 198.5024278399160664, 9.188101187500095079 ) ) ;
#39236 = CARTESIAN_POINT ( 'NONE',  ( 196.7621536703766196, 275.9285207744129025, 15.30025596421527467 ) ) ;
#39237 = ORIENTED_EDGE ( 'NONE', *, *, #39446, .T. ) ;
#39238 = LINE ( 'NONE', #24063, #65836 ) ;
#39239 = CARTESIAN_POINT ( 'NONE',  ( 182.3105792408025820, 260.2671590519555025, -11.01268989705850743 ) ) ;
#39240 = VECTOR ( 'NONE', #55961, 1000.000000000000000 ) ;
#39241 = ADVANCED_FACE ( 'NONE', ( #2520 ), #86970, .F. ) ;
#39242 = CARTESIAN_POINT ( 'NONE',  ( 164.8705138155180521, 286.2009910768602481, -3.373684704351256780 ) ) ;
#39243 = CARTESIAN_POINT ( 'NONE',  ( 80.64966744098836671, 57.49487408124664967, -16.23886060901187989 ) ) ;
#39244 = CARTESIAN_POINT ( 'NONE',  ( 155.4186054393023255, 261.4540742680644598, 17.05753227160644769 ) ) ;
#39245 = CARTESIAN_POINT ( 'NONE',  ( 57.23161641937173982, 215.3967562850347122, -4.648177544792955347E-16 ) ) ;
#39246 = DIRECTION ( 'NONE',  ( -0.8660254037844387076, -0.4999999999999998890, -0.000000000000000000 ) ) ;
#39247 = CARTESIAN_POINT ( 'NONE',  ( 147.7112127936102866, 274.8036699242858276, -9.124700685424272706 ) ) ;
#39248 = AXIS2_PLACEMENT_3D ( 'NONE', #76100, #6169, #53744 ) ;
#39249 = CARTESIAN_POINT ( 'NONE',  ( 190.9986981037068290, 264.2499144972765066, 7.795840479274263046 ) ) ;
#39250 = CARTESIAN_POINT ( 'NONE',  ( 11.23059542939759936, 30.24628978557580794, -10.00000000000000000 ) ) ;
#39251 = CARTESIAN_POINT ( 'NONE',  ( 176.4011637054438495, 256.6761881497252489, -11.13936515825015228 ) ) ;
#39252 = CARTESIAN_POINT ( 'NONE',  ( 191.1000148935602567, 299.6520602076213891, -9.462302242170249400 ) ) ;
#39253 = CARTESIAN_POINT ( 'NONE',  ( 190.4750160083620472, 300.7345900314585947, -1.159659205620361400 ) ) ;
#39254 = DIRECTION ( 'NONE',  ( -0.000000000000000000, -0.000000000000000000, 1.000000000000000000 ) ) ;
#39255 = ORIENTED_EDGE ( 'NONE', *, *, #32602, .T. ) ;
#39256 = CARTESIAN_POINT ( 'NONE',  ( 149.9060791885465846, 273.0020498124315509, -11.57482514211843849 ) ) ;
#39257 = CARTESIAN_POINT ( 'NONE',  ( 163.7183543885751078, 247.0784873978576854, -6.786164904910574336 ) ) ;
#39258 = CARTESIAN_POINT ( 'NONE',  ( 183.5291393727272009, 269.0254755003825267, 15.13985252155338834 ) ) ;
#39259 = CARTESIAN_POINT ( 'NONE',  ( 101.4461556848294492, 235.5024278399160949, -9.188101187500093303 ) ) ;
#39260 = CARTESIAN_POINT ( 'NONE',  ( 17.90548643172614263, 12.19860640527291373, 2.839279412974134775 ) ) ;
#39262 = EDGE_CURVE ( 'NONE', #6127, #71267, #71883, .T. ) ;
#39261 = CARTESIAN_POINT ( 'NONE',  ( -6.697530200413229551, 155.3932355074535963, -2.679491924311250717 ) ) ;
#39263 = CARTESIAN_POINT ( 'NONE',  ( 72.29638194752672575, 59.45177225770978424, -15.84340229133642985 ) ) ;
#39264 = VECTOR ( 'NONE', #81458, 1000.000000000000000 ) ;
#39266 = CARTESIAN_POINT ( 'NONE',  ( 191.5813027864163587, 276.8931351878708256, 16.99066381371337187 ) ) ;
#39265 = CARTESIAN_POINT ( 'NONE',  ( 136.7639277290220718, 259.7677522451419350, -5.000000000000047962 ) ) ;
#39267 = CARTESIAN_POINT ( 'NONE',  ( 204.6600721283745372, 272.9583799553993231, -9.753926932682416506 ) ) ;
#39268 = CARTESIAN_POINT ( 'NONE',  ( -70.89022602266993545, 47.22876919346843749, 10.00000000000000000 ) ) ;
#39269 = CARTESIAN_POINT ( 'NONE',  ( 149.9431819415206348, 271.6515743903611906, -11.68441791719118328 ) ) ;
#39270 = CARTESIAN_POINT ( 'NONE',  ( 105.1336465626505969, 243.0530062829863027, -4.648177544792955347E-16 ) ) ;
#39271 = DIRECTION ( 'NONE',  ( 0.000000000000000000, 1.000000000000000000, 0.000000000000000000 ) ) ;
#39272 = CARTESIAN_POINT ( 'NONE',  ( 86.47393795017364937, 47.46484117499104372, 10.41372632371118101 ) ) ;
#39273 = ORIENTED_EDGE ( 'NONE', *, *, #37387, .T. ) ;
#39274 = CARTESIAN_POINT ( 'NONE',  ( 163.2954787364450340, 255.9746288828553702, -14.88763456503479787 ) ) ;
#39275 = CARTESIAN_POINT ( 'NONE',  ( 178.1322669947267343, 280.4903793975759640, 16.69614814349041509 ) ) ;
#39276 = CARTESIAN_POINT ( 'NONE',  ( 197.3934918644919776, 268.5675634807000733, 9.323123344629930642 ) ) ;
#39278 = ORIENTED_EDGE ( 'NONE', *, *, #43091, .F. ) ;
#39277 = EDGE_CURVE ( 'NONE', #32845, #469, #79067, .T. ) ;
#39279 = EDGE_CURVE ( 'NONE', #1341, #29582, #80339, .T. ) ;
#39280 = CARTESIAN_POINT ( 'NONE',  ( 75.81625539762656274, 65.12695345013474935, -14.47344923651660054 ) ) ;
#39281 = CARTESIAN_POINT ( 'NONE',  ( 179.9888841032236257, 262.5618594283533298, -12.69062350693043761 ) ) ;
#39282 = CARTESIAN_POINT ( 'NONE',  ( 74.14312167556930433, 66.30466486950707861, 1.224646799147354045E-15 ) ) ;
#39283 = CARTESIAN_POINT ( 'NONE',  ( 88.49445028879968334, 43.86712364161932243, -9.307608808691473302E-08 ) ) ;
#39284 = VERTEX_POINT ( 'NONE', #50100 ) ;
#39285 = CARTESIAN_POINT ( 'NONE',  ( 73.63798764345266079, 69.67310094948797428, 10.11710443556177275 ) ) ;
#39286 = CARTESIAN_POINT ( 'NONE',  ( 43.36002773778349706, 27.96004757982094446, -5.678558825948276656 ) ) ;
#39287 = EDGE_LOOP ( 'NONE', ( #7529, #58993, #97795, #18652 ) ) ;
#39288 = CARTESIAN_POINT ( 'NONE',  ( 167.3868433433993630, 249.7561290667149194, 6.957693806426012983 ) ) ;
#39289 = CARTESIAN_POINT ( 'NONE',  ( 194.3442947553755005, 294.0328026529847421, -15.97648891113594871 ) ) ;
#39290 = CARTESIAN_POINT ( 'NONE',  ( 157.0150015346687553, 258.6890351218854676, 16.85538724311808068 ) ) ;
#39291 = ORIENTED_EDGE ( 'NONE', *, *, #73450, .F. ) ;
#39292 = CARTESIAN_POINT ( 'NONE',  ( 79.59476633789469702, 59.27799801817308634, 16.56459525109986330 ) ) ;
#39293 = DIRECTION ( 'NONE',  ( 0.3887219701523905169, 0.9213551052231946370, 0.000000000000000000 ) ) ;
#39294 = CARTESIAN_POINT ( 'NONE',  ( 154.0741575860427304, 263.7827262580370871, -16.96155047328870680 ) ) ;
#39295 = CARTESIAN_POINT ( 'NONE',  ( -19.65312891409030271, 93.06504152958497400, 10.00000000000000888 ) ) ;
#39296 = CARTESIAN_POINT ( 'NONE',  ( 120.7424577590100654, 230.5177522451417929, 5.000000000000051514 ) ) ;
#39297 = CARTESIAN_POINT ( 'NONE',  ( 81.59199138121388728, 55.54565483415311888, -16.32615847003737386 ) ) ;
#39298 = ORIENTED_EDGE ( 'NONE', *, *, #84109, .F. ) ;
#39299 = ORIENTED_EDGE ( 'NONE', *, *, #5774, .T. ) ;
#39300 = CARTESIAN_POINT ( 'NONE',  ( 162.6627524694667954, 249.2999192911965167, 10.54795694096488745 ) ) ;
#39301 = B_SPLINE_CURVE_WITH_KNOTS ( 'NONE', 3,
 ( #62539, #16949, #9363, #62034 ),
 .UNSPECIFIED., .F., .F.,
 ( 4, 4 ),
 ( 0.000000000000000000, 0.007566978283060982885 ),
 .UNSPECIFIED. ) ;
#39302 = ORIENTED_EDGE ( 'NONE', *, *, #43944, .F. ) ;
#39303 = CARTESIAN_POINT ( 'NONE',  ( 77.12749119013076893, 49.43705909587082914, -14.93372123758744152 ) ) ;
#39304 = ORIENTED_EDGE ( 'NONE', *, *, #48621, .T. ) ;
#39305 = CARTESIAN_POINT ( 'NONE',  ( 170.2702171900916710, 269.5895188327120877, 16.72394520728834522 ) ) ;
#39306 = CARTESIAN_POINT ( 'NONE',  ( 78.86981778719953695, 51.57386105711080404, 15.33895568566510015 ) ) ;
#39307 = EDGE_LOOP ( 'NONE', ( #40645, #46901 ) ) ;
#39308 = ADVANCED_FACE ( 'NONE', ( #21206 ), #39693, .T. ) ;
#39309 = CARTESIAN_POINT ( 'NONE',  ( 190.6193642582544499, 300.0591430953767258, -3.705976999785533632 ) ) ;
#39310 = CARTESIAN_POINT ( 'NONE',  ( 36.30495719079549843, 21.36477965099642873, 1.583844403245364907 ) ) ;
#39311 = CARTESIAN_POINT ( 'NONE',  ( 190.0646458372534937, 301.4453720177293121, 2.091788150666768153 ) ) ;
#39312 = CARTESIAN_POINT ( 'NONE',  ( 206.6389649419900536, 271.5030152196637800, -6.665702415263554670 ) ) ;
#39313 = CARTESIAN_POINT ( 'NONE',  ( 82.27383947616280579, 40.86467265836121499, 1.031166341950346954 ) ) ;
#39314 = CARTESIAN_POINT ( 'NONE',  ( 168.7460418684975139, 249.8756972425479148, -5.467426467192338713 ) ) ;
#39315 = CARTESIAN_POINT ( 'NONE',  ( 76.92814081923833669, 62.93039039429913828, -15.23958875853725203 ) ) ;
#39316 = EDGE_CURVE ( 'NONE', #73949, #82380, #35320, .T. ) ;
#39317 = CARTESIAN_POINT ( 'NONE',  ( 183.5877099323311370, 284.2622598002585050, -15.59430947663861566 ) ) ;
#39318 = ADVANCED_FACE ( 'NONE', ( #47318 ), #3257, .F. ) ;
#39319 = CARTESIAN_POINT ( 'NONE',  ( 128.5097966488581562, 238.8768266524159856, 9.188101187500098632 ) ) ;
#39320 = CARTESIAN_POINT ( 'NONE',  ( 186.6224779119422408, 262.8828560441721720, -9.606717503673682046 ) ) ;
#39321 = CARTESIAN_POINT ( 'NONE',  ( 38.69312636016019269, 30.84335787977765619, 9.188101187500006262 ) ) ;
#39322 = CARTESIAN_POINT ( 'NONE',  ( 179.3876637460693928, 290.2313054047237983, -9.427853318526828730 ) ) ;
#39323 = ORIENTED_EDGE ( 'NONE', *, *, #44251, .T. ) ;
#39324 = EDGE_CURVE ( 'NONE', #55385, #15274, #70622, .T. ) ;
#39325 = CARTESIAN_POINT ( 'NONE',  ( 203.3725562006430039, 276.0788499616656395, 13.32272411125720701 ) ) ;
#39326 = CARTESIAN_POINT ( 'NONE',  ( 180.7648415157122486, 256.2425494826519525, 1.247752698343054467 ) ) ;
#39327 = AXIS2_PLACEMENT_3D ( 'NONE', #6029, #92182, #60205 ) ;
#39328 = EDGE_CURVE ( 'NONE', #90496, #81863, #97200, .T. ) ;
#39329 = CARTESIAN_POINT ( 'NONE',  ( 174.0430117795368972, 289.9400120375415213, -4.743096007750332355 ) ) ;
#39330 = DIRECTION ( 'NONE',  ( 0.5000000000000048850, -0.8660254037844358210, 0.000000000000000000 ) ) ;
#39331 = CARTESIAN_POINT ( 'NONE',  ( -22.42236680055709641, 157.8615022471902591, 0.000000000000000000 ) ) ;
#39332 = CARTESIAN_POINT ( 'NONE',  ( 66.30954113569532637, 68.28728378170326607, 3.992301261007330737 ) ) ;
#39333 = CARTESIAN_POINT ( 'NONE',  ( 180.2260403442535051, 295.0423342771414923, -3.480517403894910711 ) ) ;
#39334 = CARTESIAN_POINT ( 'NONE',  ( 148.5730530464635706, 273.3109188183360061, 10.25868201370624888 ) ) ;
#39335 = CARTESIAN_POINT ( 'NONE',  ( 165.0169426809697768, 246.6514736266339298, 5.598232276327055779 ) ) ;
#39336 = ORIENTED_EDGE ( 'NONE', *, *, #36119, .F. ) ;
#39337 = CARTESIAN_POINT ( 'NONE',  ( 194.8598199529639317, 293.1398868181796615, -15.91766051364927570 ) ) ;
#39338 = CARTESIAN_POINT ( 'NONE',  ( 66.03861470602267048, 68.70284247729489380, -0.4429836963394074290 ) ) ;
#39339 = VERTEX_POINT ( 'NONE', #40204 ) ;
#39340 = DIRECTION ( 'NONE',  ( -0.8660254037844379305, -0.5000000000000014433, -0.000000000000000000 ) ) ;
#39341 = CARTESIAN_POINT ( 'NONE',  ( 191.0217486410549839, 283.4676459628224165, -16.57262105235832905 ) ) ;
#39342 = CARTESIAN_POINT ( 'NONE',  ( 178.2544296081904918, 259.9720107254665322, -13.27066457805568866 ) ) ;
#39343 = LINE ( 'NONE', #93603, #13870 ) ;
#39344 = CARTESIAN_POINT ( 'NONE',  ( 204.6823371430232896, 272.9704135290961062, -9.754921121218281144 ) ) ;
#39346 = CARTESIAN_POINT ( 'NONE',  ( 160.5163443890054964, 282.2647654489487081, 6.663140935368019768 ) ) ;
#39345 = CARTESIAN_POINT ( 'NONE',  ( 164.7124473124548558, 284.1078844219010193, -6.876237286123044967 ) ) ;
#39347 = FACE_OUTER_BOUND ( 'NONE', #88210, .T. ) ;
#39348 = ORIENTED_EDGE ( 'NONE', *, *, #53826, .T. ) ;
#39349 = LINE ( 'NONE', #9485, #22238 ) ;
#39351 = CARTESIAN_POINT ( 'NONE',  ( 72.68994967886170855, 66.60535542942379550, 11.89643324170776850 ) ) ;
#39350 = B_SPLINE_SURFACE_WITH_KNOTS ( 'NONE', 3, 1, ( 
 ( #84486, #75372 ),
 ( #61129, #15029 ),
 ( #90607, #29750 ),
 ( #45920, #69237 ),
 ( #21174, #76839 ),
 ( #91577, #29260 ),
 ( #7436, #60622 ),
 ( #100166, #5953 ),
 ( #52054, #43938 ),
 ( #6940, #37831 ),
 ( #13569, #60129 ),
 ( #14559, #91091 ),
 ( #82992, #36847 ),
 ( #44934, #68239 ),
 ( #67755, #98680 ),
 ( #38329, #21656 ),
 ( #5460, #75880 ),
 ( #30752, #52538 ),
 ( #83489, #14055 ),
 ( #45434, #92105 ),
 ( #90096, #82516 ),
 ( #51553, #6458 ),
 ( #22149, #53040 ),
 ( #20665, #99661 ),
 ( #13077, #74877 ),
 ( #36344, #67246 ),
 ( #98176, #23620 ),
 ( #86504, #94083 ),
 ( #85492, #16536 ),
 ( #61629, #39315 ),
 ( #32736, #1352 ) ),
 .UNSPECIFIED., .F., .F., .F.,
 ( 4, 3, 3, 3, 3, 3, 3, 3, 3, 3, 4 ),
 ( 2, 2 ),
 ( 0.000000000000000000, 0.1333490885032290463, 0.3007194338854137228, 0.4699862290245038765, 0.5844252810809251741, 0.6686540514502686827, 0.7354980260655517021, 0.8028463152565618044, 0.8633854507757415808, 0.9437142632667480102, 1.000000000000000000 ),
 ( 0.000000000000000000, 1.000000000000000000 ),
 .UNSPECIFIED. ) ;
#39352 = CARTESIAN_POINT ( 'NONE',  ( 164.2681401592249699, 247.4123488826276969, -7.457225004184277140 ) ) ;
#39353 = CARTESIAN_POINT ( 'NONE',  ( 156.6812872898450735, 261.2670451491295012, 0.000000000000000000 ) ) ;
#39354 = CARTESIAN_POINT ( 'NONE',  ( 173.7407999030873498, 250.8548675950284519, -1.041279177761091912 ) ) ;
#39355 = CARTESIAN_POINT ( 'NONE',  ( 185.8592955827088531, 297.1117474649988708, -4.290889079375690862 ) ) ;
#39356 = CARTESIAN_POINT ( 'NONE',  ( 204.3095277081791892, 275.7254174276451977, 13.16468475777854863 ) ) ;
#39357 = CARTESIAN_POINT ( 'NONE',  ( 193.6455285480667783, 269.4045135959429444, 13.67829860818159027 ) ) ;
#39358 = CARTESIAN_POINT ( 'NONE',  ( 74.29686697005888618, 68.54486718330414874, 11.12163720784228893 ) ) ;
#39359 = CARTESIAN_POINT ( 'NONE',  ( 70.87618550449425925, 71.40954602149369634, -2.428563748625821805 ) ) ;
#39360 = CARTESIAN_POINT ( 'NONE',  ( -7.320788502016136512, 157.3923013555410080, 4.594050593750050204 ) ) ;
#39361 = CARTESIAN_POINT ( 'NONE',  ( 87.45434598099585344, 230.4869531367911293, 4.594050593750046652 ) ) ;
#39362 = CARTESIAN_POINT ( 'NONE',  ( 67.65687428590848640, 66.76031625959198834, 8.613883631066450164 ) ) ;
#39363 = CARTESIAN_POINT ( 'NONE',  ( 193.1977289678065404, 296.0187128512746995, -12.37159405312863925 ) ) ;
#39364 = CARTESIAN_POINT ( 'NONE',  ( 50.32263495959776378, 94.90690751109829648, 10.00000000000000000 ) ) ;
#39365 = ADVANCED_FACE ( 'NONE', ( #86387 ), #40779, .F. ) ;
#39366 = FACE_OUTER_BOUND ( 'NONE', #69124, .T. ) ;
#39367 = FACE_OUTER_BOUND ( 'NONE', #52383, .T. ) ;
#39368 = CARTESIAN_POINT ( 'NONE',  ( 84.60735463175657856, 50.53152741511170376, -13.60229262012000184 ) ) ;
#39369 = CARTESIAN_POINT ( 'NONE',  ( 37.58366506746438773, 204.0530062829863027, 1.101618078115930403E-13 ) ) ;
#39371 = CARTESIAN_POINT ( 'NONE',  ( 76.31637673998004345, 51.11355729699548078, 16.05611523598242840 ) ) ;
#39370 = CARTESIAN_POINT ( 'NONE',  ( 73.05863210132505969, 69.60576123971952711, -9.808587366596247747 ) ) ;
#39372 = CARTESIAN_POINT ( 'NONE',  ( 72.28884795246587203, 71.97623822831552332, -3.689212715915426877 ) ) ;
#39373 = CARTESIAN_POINT ( 'NONE',  ( 169.4383027745296602, 251.8538218511134232, -9.888297047301421117 ) ) ;
#39374 = CARTESIAN_POINT ( 'NONE',  ( 164.7584947292794766, 245.2769114807558140, -5.139043669254925284 ) ) ;
#39375 = CARTESIAN_POINT ( 'NONE',  ( 196.4390255720217908, 290.4046224503736653, 16.34739044515864848 ) ) ;
#39376 = CARTESIAN_POINT ( 'NONE',  ( -58.01722807680246774, 56.46252223527211811, 59.99999999999999289 ) ) ;
#39377 = DIRECTION ( 'NONE',  ( 0.3473291852294957405, -0.6015917957689906892, 0.7193398003386545225 ) ) ;
#39378 = CARTESIAN_POINT ( 'NONE',  ( 44.64073572505018461, 187.3923013555410080, 4.594050593750050204 ) ) ;
#39379 = CARTESIAN_POINT ( 'NONE',  ( 69.15955932604958889, 219.9244531367911293, -4.594050593750046652 ) ) ;
#39380 = FACE_OUTER_BOUND ( 'NONE', #15880, .T. ) ;
#39382 = ADVANCED_FACE ( 'NONE', ( #4738 ), #49829, .F. ) ;
#39381 = CARTESIAN_POINT ( 'NONE',  ( 88.37416949021037738, 43.79857776338975839, 0.1607882160166528573 ) ) ;
#39383 = CARTESIAN_POINT ( 'NONE',  ( 167.2628569450862699, 259.7336296457672233, 16.26364047457860096 ) ) ;
#39384 = CARTESIAN_POINT ( 'NONE',  ( -6.040052912301403509, 153.9865022471901455, 1.119607411625061291E-15 ) ) ;
#39386 = CARTESIAN_POINT ( 'NONE',  ( 69.77735531064696772, 70.84206482737464228, -4.035796813025271490 ) ) ;
#39385 = CARTESIAN_POINT ( 'NONE',  ( 72.17322115918098291, 71.85944340353097459, -3.889528917610050041 ) ) ;
#39387 = FACE_OUTER_BOUND ( 'NONE', #41719, .T. ) ;
#39388 = CARTESIAN_POINT ( 'NONE',  ( 25.46698091360950045, 30.10171378149919974, 9.188101187500008038 ) ) ;
#39389 = CARTESIAN_POINT ( 'NONE',  ( 150.8247211172754589, 269.4109153179094278, -14.37608026040300402 ) ) ;
#39390 = CARTESIAN_POINT ( 'NONE',  ( 83.29758183770785251, 47.02354989389091600, -11.60801483937473044 ) ) ;
#39391 = CARTESIAN_POINT ( 'NONE',  ( 11.30507296547734697, 15.03085787977761179, 9.188101187500006262 ) ) ;
#39392 = CARTESIAN_POINT ( 'NONE',  ( 61.98804677278346986, 206.5958772461660828, -9.188101187500095079 ) ) ;
#39393 = CARTESIAN_POINT ( 'NONE',  ( 76.96934732445689065, 63.82118396924765591, 14.93646943666589344 ) ) ;
#39394 = CYLINDRICAL_SURFACE ( 'NONE', #26781, 10.00000000000000355 ) ;
#39395 = CARTESIAN_POINT ( 'NONE',  ( 159.2077906806335932, 254.8910129107889588, 16.14624949541834553 ) ) ;
#39396 = DIRECTION ( 'NONE',  ( -0.9979398670145497308, -0.06415622980648827411, 0.000000000000000000 ) ) ;
#39397 = CARTESIAN_POINT ( 'NONE',  ( 201.3152185631758186, 281.9588084421832264, 17.09304993608981604 ) ) ;
#39398 = EDGE_CURVE ( 'NONE', #91230, #6477, #67010, .T. ) ;
#39399 = EDGE_CURVE ( 'NONE', #43843, #75021, #74146, .T. ) ;
#39400=STYLED_ITEM('',(#100310),#42857);
#39401 = CARTESIAN_POINT ( 'NONE',  ( 78.24789397509293565, 55.76986583530001695, -16.13979192025500353 ) ) ;
#39402 = CARTESIAN_POINT ( 'NONE',  ( 112.2445834879231796, 225.6115022471901739, -5.000000000000041744 ) ) ;
#39403 = CARTESIAN_POINT ( 'NONE',  ( -17.26249501324477720, 59.91680024587567033, -10.00000000000000000 ) ) ;
#39404 = CARTESIAN_POINT ( 'NONE',  ( 206.9408877595175511, 272.2148635675444552, 6.707071080545934372 ) ) ;
#39405 = VERTEX_POINT ( 'NONE', #51829 ) ;
#39406 = CARTESIAN_POINT ( 'NONE',  ( 77.21588584563488666, 49.49447693446913377, 14.93476029654182646 ) ) ;
#39407 = CARTESIAN_POINT ( 'NONE',  ( 184.7589102698180454, 271.2641373520414163, 16.13988341988741482 ) ) ;
#39408 = ORIENTED_EDGE ( 'NONE', *, *, #1153, .T. ) ;
#39409 = CARTESIAN_POINT ( 'NONE',  ( 206.7680519836501958, 272.5142239127119979, -10.57935479673322021 ) ) ;
#39410 = CARTESIAN_POINT ( 'NONE',  ( 187.3045064622214682, 276.9103046244464394, -16.79128408433122033 ) ) ;
#39411 = CARTESIAN_POINT ( 'NONE',  ( 67.61525443866294438, 68.60254357949423820, -5.272938102954969786 ) ) ;
#39412 = ORIENTED_EDGE ( 'NONE', *, *, #90160, .F. ) ;
#39413 = CARTESIAN_POINT ( 'NONE',  ( 173.5969002525141605, 251.1178000409413187, 0.5105381496963667942 ) ) ;
#39414 = ORIENTED_EDGE ( 'NONE', *, *, #68098, .T. ) ;
#39415 = CARTESIAN_POINT ( 'NONE',  ( 49.32130651720206771, 81.12656353050643077, 177.5919119679930134 ) ) ;
#39416 = CARTESIAN_POINT ( 'NONE',  ( 148.3025927079438304, 273.7793698660844939, -8.046026357031887954 ) ) ;
#39417 = CARTESIAN_POINT ( 'NONE',  ( 155.8152618860606538, 260.7670451491295012, 0.000000000000000000 ) ) ;
#39418 = VERTEX_POINT ( 'NONE', #96975 ) ;
#39419 = CARTESIAN_POINT ( 'NONE',  ( 27.58754685475307156, 27.87878583063842797, -9.188101187500006262 ) ) ;
#39420 = CARTESIAN_POINT ( 'NONE',  ( 49.87168060777529632, 103.2007005253944385, -10.00000000000000000 ) ) ;
#39421 = CARTESIAN_POINT ( 'NONE',  ( 75.04128323750522611, 66.36387088788158906, -13.13100288533564886 ) ) ;
#39422 = ORIENTED_EDGE ( 'NONE', *, *, #84676, .F. ) ;
#39423 = LINE ( 'NONE', #6560, #49824 ) ;
#39424 = DIRECTION ( 'NONE',  ( -0.8660254037844387076, -0.4999999999999998890, -0.000000000000000000 ) ) ;
#39425 = ORIENTED_EDGE ( 'NONE', *, *, #8433, .F. ) ;
#39426 = CARTESIAN_POINT ( 'NONE',  ( -19.65312891409030271, 93.06504152958497400, 10.00000000000000888 ) ) ;
#39427 = EDGE_CURVE ( 'NONE', #68209, #10682, #73152, .T. ) ;
#39429 = CARTESIAN_POINT ( 'NONE',  ( 67.78518765966735771, 65.95975373770653505, -10.48313618456564988 ) ) ;
#39428 = CARTESIAN_POINT ( 'NONE',  ( 67.79325343485642463, 65.52334347001540493, 10.20133969316753131 ) ) ;
#39430 = CARTESIAN_POINT ( 'NONE',  ( -38.94059804707394079, 66.00003524665416421, -10.00000000000000000 ) ) ;
#39431 = CARTESIAN_POINT ( 'NONE',  ( 182.8258399896172648, 294.6916754291505072, 8.116841955439214829 ) ) ;
#39432 = CARTESIAN_POINT ( 'NONE',  ( 185.3862244519964406, 292.5652162196358859, -10.75470610306963515 ) ) ;
#39433 = CARTESIAN_POINT ( 'NONE',  ( 205.3465787480556344, 274.9762877783610406, -13.79319041940166279 ) ) ;
#39434 = CARTESIAN_POINT ( 'NONE',  ( 139.7406297344813311, 260.6744531367911009, 4.594050593750047540 ) ) ;
#39435 = CARTESIAN_POINT ( 'NONE',  ( 203.5602143330212641, 268.7753616305579385, 2.467715433455414331 ) ) ;
#39436 = CARTESIAN_POINT ( 'NONE',  ( 179.0261547916831546, 258.3138165185279149, 9.736748159590288054 ) ) ;
#39437 = CARTESIAN_POINT ( 'NONE',  ( 88.13101510164371177, 227.8149278399160949, -9.188101187500095079 ) ) ;
#39438 = ORIENTED_EDGE ( 'NONE', *, *, #7007, .T. ) ;
#39439 = CARTESIAN_POINT ( 'NONE',  ( 151.4025156491502742, 268.4101458323662541, 14.71049357081981235 ) ) ;
#39440 = PLANE ( 'NONE',  #49646 ) ;
#39441 = VERTEX_POINT ( 'NONE', #57921 ) ;
#39442 = CARTESIAN_POINT ( 'NONE',  ( 156.9377365471174812, 258.8228620059706486, -16.89686783298308015 ) ) ;
#39443 = VERTEX_POINT ( 'NONE', #13336 ) ;
#39444 = ORIENTED_EDGE ( 'NONE', *, *, #92424, .T. ) ;
#39445 = CARTESIAN_POINT ( 'NONE',  ( 80.00158170572299809, 44.44258412922052770, -10.93648124919405795 ) ) ;
#39446 = EDGE_CURVE ( 'NONE', #78211, #86358, #34363, .T. ) ;
#39447 = CARTESIAN_POINT ( 'NONE',  ( 147.0276296945837373, 275.9876705829954062, 0.7617065417431535534 ) ) ;
#39448 = CARTESIAN_POINT ( 'NONE',  ( 81.32396741884589630, 55.80035763937271298, 16.38826086546822580 ) ) ;
#39449 = CARTESIAN_POINT ( 'NONE',  ( 46.32860941106299890, 116.4404604047837779, 10.00000000000000000 ) ) ;
#39450 = CARTESIAN_POINT ( 'NONE',  ( 163.0682440866927720, 248.2045114712421423, 11.63988583931958942 ) ) ;
#39451 = CARTESIAN_POINT ( 'NONE',  ( 82.93520977470207356, 212.5643266524159856, -9.188101187500093303 ) ) ;
#39452 = ORIENTED_EDGE ( 'NONE', *, *, #54062, .F. ) ;
#39453 = ORIENTED_EDGE ( 'NONE', *, *, #7066, .F. ) ;
#39454 = CARTESIAN_POINT ( 'NONE',  ( 208.3790849386676598, 269.7238329819538762, -1.525282248498321946 ) ) ;
#39455 = ORIENTED_EDGE ( 'NONE', *, *, #45322, .T. ) ;
#39456 = CARTESIAN_POINT ( 'NONE',  ( 19.65800174957785629, 23.30066082961421969, -10.00000000000000533 ) ) ;
#39457 = CARTESIAN_POINT ( 'NONE',  ( 76.03323602888910671, 65.53324422044475739, -14.33394004605309036 ) ) ;
#39458 = EDGE_CURVE ( 'NONE', #17175, #49794, #19463, .T. ) ;
#39459 = CARTESIAN_POINT ( 'NONE',  ( 207.0644055248061761, 269.7777976096807038, -0.04004023774084553011 ) ) ;
#39460 = DIRECTION ( 'NONE',  ( -0.000000000000000000, -0.000000000000000000, -1.000000000000000000 ) ) ;
#39461 = CARTESIAN_POINT ( 'NONE',  ( 87.74187345177139719, 44.20045605528624577, 4.652363546664123106 ) ) ;
#39462 = ORIENTED_EDGE ( 'NONE', *, *, #49000, .T. ) ;
#39463 = CARTESIAN_POINT ( 'NONE',  ( 188.8759260044885764, 294.9136311979676748, 11.52016544153279654 ) ) ;
#39464 = CARTESIAN_POINT ( 'NONE',  ( 43.27754793094329244, 25.39040679176986970, -6.890680421881970419E-14 ) ) ;
#39465 = LINE ( 'NONE', #70390, #2838 ) ;
#39466 = CARTESIAN_POINT ( 'NONE',  ( 153.0308080659177392, 265.5898606369461277, -17.74682723936668438 ) ) ;
#39467 = B_SPLINE_CURVE_WITH_KNOTS ( 'NONE', 3,
 ( #79699, #63947, #9260, #62947, #70545, #78165, #72068, #54841, #71571, #8260, #2167, #32555, #86813, #48766, #24451, #33048 ),
 .UNSPECIFIED., .F., .F.,
 ( 4, 1, 2, 2, 2, 1, 2, 2, 4 ),
 ( 0.000000000000000000, 0.1249999999999967804, 0.1874999999999955591, 0.2499999999999943379, 0.4999999999999986677, 0.6250000000000023315, 0.6875000000000021094, 0.7500000000000019984, 1.000000000000000000 ),
 .UNSPECIFIED. ) ;
#39468 = EDGE_CURVE ( 'NONE', #36836, #36314, #60391, .T. ) ;
#39469 = DIRECTION ( 'NONE',  ( 1.000000000000000000, 0.000000000000000000, 0.000000000000000000 ) ) ;
#39470 = EDGE_LOOP ( 'NONE', ( #37450, #9040, #37771, #58396 ) ) ;
#39471 = CARTESIAN_POINT ( 'NONE',  ( 195.8540013720623278, 265.4683100572506191, 4.431129527759733122 ) ) ;
#39472 = CARTESIAN_POINT ( 'NONE',  ( 86.96746701141694302, 211.0177522451417929, 5.000000000000051514 ) ) ;
#39473 = DIRECTION ( 'NONE',  ( 0.7905172007421643610, 0.000000000000000000, 0.6124398381316914497 ) ) ;
#39474 = CARTESIAN_POINT ( 'NONE',  ( 171.1784097330638872, 251.6294428635012537, 7.086366496291955919 ) ) ;
#39475 = CARTESIAN_POINT ( 'NONE',  ( 83.82827945288542537, 51.88092520783234818, 14.50189114860043027 ) ) ;
#39476 = EDGE_CURVE ( 'NONE', #8628, #28346, #53785, .T. ) ;
#39477 = DIRECTION ( 'NONE',  ( 0.4999999999999998890, -0.8660254037844385966, 0.000000000000000000 ) ) ;
#39478 = ORIENTED_EDGE ( 'NONE', *, *, #38220, .T. ) ;
#39479 = VECTOR ( 'NONE', #52898, 1000.000000000000000 ) ;
#39480 = CARTESIAN_POINT ( 'NONE',  ( 165.8866640751390094, 265.8956478032751534, 17.81115609982314751 ) ) ;
#39481 = CARTESIAN_POINT ( 'NONE',  ( -15.86348812680012799, 102.2296172668195737, 44.51064192688916421 ) ) ;
#39482 = LINE ( 'NONE', #31401, #32442 ) ;
#39484 = CYLINDRICAL_SURFACE ( 'NONE', #68973, 16.60714546451156792 ) ;
#39483 = CARTESIAN_POINT ( 'NONE',  ( 194.2199708651012600, 294.2481379475345875, 15.50834247347371253 ) ) ;
#39485 = CARTESIAN_POINT ( 'NONE',  ( 69.69198297313906210, 62.71137935599142565, -13.30837126644457236 ) ) ;
#39486 = CARTESIAN_POINT ( 'NONE',  ( 32.90709467669684329, 21.12755873383627758, -6.180339887498949025 ) ) ;
#39487 = CARTESIAN_POINT ( 'NONE',  ( -19.65312891409030271, 93.06504152958497400, 177.5919119679930134 ) ) ;
#39488 = CARTESIAN_POINT ( 'NONE',  ( 174.5508403973756515, 260.3590064504865040, -14.93617697178709314 ) ) ;
#39489 = CARTESIAN_POINT ( 'NONE',  ( -0.01211276271276175848, 139.0458036431182620, -21.50000000000002487 ) ) ;
#39490 = CARTESIAN_POINT ( 'NONE',  ( 161.7767236248226084, 250.4414905302161287, -13.15904643207033153 ) ) ;
#39491 =( BOUNDED_CURVE ( )  B_SPLINE_CURVE ( 2, ( #22546, #5363, #91479, #28647, #6841, #67646, #29650, #21558, #53432 ),
 .UNSPECIFIED., .F., .T. ) 
 B_SPLINE_CURVE_WITH_KNOTS ( ( 3, 2, 2, 2, 3 ),
 ( 0.6895161290322581182, 0.6908602150537634934, 0.6935483870967742437, 0.6962365591397849940, 0.6975806451612903691 ),
 .UNSPECIFIED. ) 
 CURVE ( )  GEOMETRIC_REPRESENTATION_ITEM ( )  RATIONAL_B_SPLINE_CURVE ( ( 0.9330127018922194093, 0.9330127018922194093, 1.000000000000000000, 0.8660254037844387076, 1.000000000000000000, 0.8660254037844387076, 1.000000000000000000, 0.9330127018922194093, 0.9330127018922194093 ) ) 
 REPRESENTATION_ITEM ( '' )  );
#39492 = CARTESIAN_POINT ( 'NONE',  ( -6.807019788225388446, 173.0024278399160949, 9.188101187500095079 ) ) ;
#39493 = CARTESIAN_POINT ( 'NONE',  ( 191.1597575862519705, 296.5656282560291288, -11.82805995379970021 ) ) ;
#39494 = ORIENTED_EDGE ( 'NONE', *, *, #88410, .F. ) ;
#39496 = CARTESIAN_POINT ( 'NONE',  ( 177.3028647534693789, 256.5043743002872816, 8.298765593072630509 ) ) ;
#39495 = B_SPLINE_CURVE_WITH_KNOTS ( 'NONE', 3,
 ( #80058, #10626, #1360, #33775, #95100, #47439, #9459, #40329, #78873, #10969, #71268, #63647, #25140, #64661, #64148, #25664 ),
 .UNSPECIFIED., .F., .F.,
 ( 4, 1, 2, 2, 2, 1, 2, 2, 4 ),
 ( 0.000000000000000000, 0.1249999999999990841, 0.1875000000000001665, 0.2500000000000012768, 0.5000000000000003331, 0.6249999999999998890, 0.6874999999999983347, 0.7499999999999966693, 1.000000000000000000 ),
 .UNSPECIFIED. ) ;
#39497 = DIRECTION ( 'NONE',  ( -0.000000000000000000, -0.000000000000000000, -1.000000000000000000 ) ) ;
#39498 = DIRECTION ( 'NONE',  ( 0.000000000000000000, 0.000000000000000000, 1.000000000000000000 ) ) ;
#39499 = CARTESIAN_POINT ( 'NONE',  ( 28.05084980986327281, 180.8768266524160424, -9.188101187500093303 ) ) ;
#39500 = CARTESIAN_POINT ( 'NONE',  ( 22.93916872074224855, 35.01751292744057054, 6.180339887498949913 ) ) ;
#39501 = CARTESIAN_POINT ( 'NONE',  ( 34.02846334099481140, 24.81029122506296503, 8.090169943749479842 ) ) ;
#39502 = CARTESIAN_POINT ( 'NONE',  ( 76.77731254116882553, 64.09355814141257213, -15.16545583891343263 ) ) ;
#39503 = CARTESIAN_POINT ( 'NONE',  ( 173.3031365584441232, 273.4220882896894409, -17.43855797201185354 ) ) ;
#39504 = CARTESIAN_POINT ( 'NONE',  ( 133.7124848875370731, 259.5530062829863596, -4.648177544792955347E-16 ) ) ;
#39505 = CARTESIAN_POINT ( 'NONE',  ( 186.9795881944451423, 295.9919572693598866, -7.697386768984371130 ) ) ;
#39506 = CARTESIAN_POINT ( 'NONE',  ( 189.1827640625472782, 261.0025008612562942, -0.7550638320438417539 ) ) ;
#39507 = EDGE_CURVE ( 'NONE', #3834, #66626, #62863, .T. ) ;
#39508 = ADVANCED_FACE ( 'NONE', ( #7705 ), #54281, .T. ) ;
#39509 = CARTESIAN_POINT ( 'NONE',  ( 193.0616670940060828, 295.8427809175656762, -12.31989297540982697 ) ) ;
#39510 = CARTESIAN_POINT ( 'NONE',  ( 78.46959274033007148, 206.1115022471901739, -5.000000000000041744 ) ) ;
#39511 = CARTESIAN_POINT ( 'NONE',  ( 72.62602488434787062, 66.38659855042941160, -12.03580873979266208 ) ) ;
#39512 = DIRECTION ( 'NONE',  ( 1.000000000000000000, 0.000000000000000000, 0.000000000000000000 ) ) ;
#39513 = EDGE_CURVE ( 'NONE', #13677, #58122, #51208, .T. ) ;
#39514 = CARTESIAN_POINT ( 'NONE',  ( 34.70824655357364463, 190.8458772461660544, 9.188101187500095079 ) ) ;
#39515 = CARTESIAN_POINT ( 'NONE',  ( 50.27371054362190961, 89.86549102125590593, 10.00000000000000000 ) ) ;
#39516 = EDGE_CURVE ( 'NONE', #3474, #82113, #92350, .T. ) ;
#39517 = SURFACE_SIDE_STYLE ('',( #61333 ) ) ;
#39518 = CARTESIAN_POINT ( 'NONE',  ( 206.6389649419900536, 271.5030152196637800, -6.665702415263554670 ) ) ;
#39519 = CARTESIAN_POINT ( 'NONE',  ( 151.3124059063077311, 268.5662204852269497, -14.45542936000225609 ) ) ;
#39520 = DIRECTION ( 'NONE',  ( -1.000000000000000000, 0.000000000000000000, 0.000000000000000000 ) ) ;
#39521 = CARTESIAN_POINT ( 'NONE',  ( 0.5273063997305368344, 171.1115022471902591, 10.00000000000009592 ) ) ;
#39522 = CARTESIAN_POINT ( 'NONE',  ( 73.62250635243425734, 69.55784274833358438, 10.23584637956793308 ) ) ;
#39523 = DIRECTION ( 'NONE',  ( -1.000000000000000000, 0.000000000000000000, 0.000000000000000000 ) ) ;
#39524 = CARTESIAN_POINT ( 'NONE',  ( 26.41418602390824333, 17.11110640527292759, -2.839279412974138328 ) ) ;
#39525 = CARTESIAN_POINT ( 'NONE',  ( 162.6937333994314656, 248.8531830095558632, 10.02305144031113926 ) ) ;
#39526 = CARTESIAN_POINT ( 'NONE',  ( 105.5870131927823508, 231.7677522451418497, 10.00000000000009592 ) ) ;
#39527 = CARTESIAN_POINT ( 'NONE',  ( 175.0279472884096776, 256.8441564353742592, 11.93536191757501363 ) ) ;
#39528 = ORIENTED_EDGE ( 'NONE', *, *, #36119, .T. ) ;
#39529 = B_SPLINE_CURVE_WITH_KNOTS ( 'NONE', 3,
 ( #65922, #72565, #3169, #63933 ),
 .UNSPECIFIED., .F., .F.,
 ( 4, 4 ),
 ( 0.04541327962301634075, 0.04887120950165262795 ),
 .UNSPECIFIED. ) ;
#39530 = CARTESIAN_POINT ( 'NONE',  ( 10.98031343905818069, 14.84335787977761179, 9.188101187500006262 ) ) ;
#39531 = CARTESIAN_POINT ( 'NONE',  ( 88.22000632671873177, 44.27423112938744509, 4.003506518527978564 ) ) ;
#39532 = CARTESIAN_POINT ( 'NONE',  ( 75.79749919803089142, 58.99206122708265809, -15.93881189237040097 ) ) ;
#39533 = CARTESIAN_POINT ( 'NONE',  ( 71.75124654091098364, 72.49002453570855664, -1.344699539992842752 ) ) ;
#39534 = VERTEX_POINT ( 'NONE', #38598 ) ;
#39535 = LINE ( 'NONE', #31450, #65177 ) ;
#39536 = CARTESIAN_POINT ( 'NONE',  ( 72.29604205201167133, 71.64671137691723857, -5.830803549263603891 ) ) ;
#39537 = CARTESIAN_POINT ( 'NONE',  ( 190.7851751463332164, 300.1973786460605425, 8.237717828100052486 ) ) ;
#39538 = CARTESIAN_POINT ( 'NONE',  ( 181.2136957205551084, 257.4508974852847700, -7.654872872151471164 ) ) ;
#39539 = AXIS2_PLACEMENT_3D ( 'NONE', #73518, #60271, #59270 ) ;
#39540 = VERTEX_POINT ( 'NONE', #69502 ) ;
#39541 = EDGE_LOOP ( 'NONE', ( #97706, #67975 ) ) ;
#39543 = CARTESIAN_POINT ( 'NONE',  ( 84.44461922012131083, 42.65730447493894673, -4.171913819451575911 ) ) ;
#39542 = CARTESIAN_POINT ( 'NONE',  ( 66.57026871561890857, 68.76443072695623471, 4.738950751700697239 ) ) ;
#39544 = ORIENTED_EDGE ( 'NONE', *, *, #53947, .F. ) ;
#39545 = CARTESIAN_POINT ( 'NONE',  ( 201.4214977800931763, 281.7747274386935601, -17.04225209925078133 ) ) ;
#39546 = CARTESIAN_POINT ( 'NONE',  ( 71.82992063434448937, 72.13096581328876766, -3.644439638307356955 ) ) ;
#39547 = CARTESIAN_POINT ( 'NONE',  ( 79.83401254395657531, 57.87045807247319118, 16.26439772172798115 ) ) ;
#39548 = CARTESIAN_POINT ( 'NONE',  ( 147.9748066657072627, 274.3471119452502762, 9.387104374042873900 ) ) ;
#39549 = AXIS2_PLACEMENT_3D ( 'NONE', #48322, #17932, #41706 ) ;
#39550 = B_SPLINE_CURVE_WITH_KNOTS ( 'NONE', 3,
 ( #26652, #49947, #11477, #10455 ),
 .UNSPECIFIED., .F., .F.,
 ( 4, 4 ),
 ( 0.000000000000000000, 0.007447265025110824666 ),
 .UNSPECIFIED. ) ;
#39551 = CARTESIAN_POINT ( 'NONE',  ( 181.3700392331832631, 287.2969061643829036, -13.32859413632180434 ) ) ;
#39552 = ORIENTED_EDGE ( 'NONE', *, *, #97538, .F. ) ;
#39553 = CARTESIAN_POINT ( 'NONE',  ( 67.00187114335926708, 67.08813303282481399, 8.529924657355548945 ) ) ;
#39554 = CARTESIAN_POINT ( 'NONE',  ( 160.2389756875691944, 266.2308171109146429, 16.63061643655940713 ) ) ;
#39555 = EDGE_LOOP ( 'NONE', ( #29395, #92833, #11665, #74989 ) ) ;
#39556 = CARTESIAN_POINT ( 'NONE',  ( 22.00590953607929023, 34.74646525600390845, 2.839279412974139660 ) ) ;
#39557 = DIRECTION ( 'NONE',  ( 0.6600842437418872333, -0.7511915808658273797, 0.000000000000000000 ) ) ;
#39558 = CARTESIAN_POINT ( 'NONE',  ( 78.36279588851795097, 47.41043415324341481, -13.73196331463247155 ) ) ;
#39559 = CARTESIAN_POINT ( 'NONE',  ( 64.36996372895569607, 195.7202760586659736, -5.415160957724236172E-17 ) ) ;
#39560 = ORIENTED_EDGE ( 'NONE', *, *, #75925, .F. ) ;
#39561 = CARTESIAN_POINT ( 'NONE',  ( 193.7609008727193043, 262.8443104439116951, 4.759103018491034121 ) ) ;
#39562 = CARTESIAN_POINT ( 'NONE',  ( 159.8276996530030090, 255.3946308028359624, 16.30222759331605786 ) ) ;
#39563 = CARTESIAN_POINT ( 'NONE',  ( 89.49337443912149581, 229.1427522451419065, 10.00000000000009415 ) ) ;
#39564 = CARTESIAN_POINT ( 'NONE',  ( 172.7335680787827528, 271.6338345647230312, 16.60374280657107349 ) ) ;
#39565 = VERTEX_POINT ( 'NONE', #76141 ) ;
#39566 = CARTESIAN_POINT ( 'NONE',  ( 189.9548861516039722, 299.9966941760355326, 5.043691249193295256 ) ) ;
#39567 = CARTESIAN_POINT ( 'NONE',  ( 84.25080109756747504, 42.92892633554705384, -5.211464095953071585 ) ) ;
#39568 = CARTESIAN_POINT ( 'NONE',  ( 73.11106055086588640, 213.0177522451418497, -10.00000000000009592 ) ) ;
#39569 = CARTESIAN_POINT ( 'NONE',  ( 190.5674408456512765, 300.5745055173924811, -0.9151048603553563199 ) ) ;
#39570 = VERTEX_POINT ( 'NONE', #84257 ) ;
#39571 = CARTESIAN_POINT ( 'NONE',  ( 174.9895866936052471, 261.2018727689135176, -14.15269007960848313 ) ) ;
#39572 = LINE ( 'NONE', #85770, #37199 ) ;
#39573 = CARTESIAN_POINT ( 'NONE',  ( 191.0536258616249370, 299.7324083678473130, 8.935283001608469888 ) ) ;
#39574 = CARTESIAN_POINT ( 'NONE',  ( 192.6789561813392595, 296.9172536750198219, -11.84591848451790952 ) ) ;
#39575 = CARTESIAN_POINT ( 'NONE',  ( 163.3485124243574091, 257.7923317456250629, 15.56224772009493229 ) ) ;
#39576 = ADVANCED_FACE ( 'NONE', ( #85251 ), #59902, .F. ) ;
#39577 = CARTESIAN_POINT ( 'NONE',  ( 69.25351710553235307, 66.05396458075408361, 10.55744696599895427 ) ) ;
#39578 = VECTOR ( 'NONE', #84333, 1000.000000000000114 ) ;
#39579 = CARTESIAN_POINT ( 'NONE',  ( 206.1932826529868805, 273.5097535960530877, 11.72208607728249241 ) ) ;
#39580 = CARTESIAN_POINT ( 'NONE',  ( 0.005075371086064872639, 27.18819441265828019, -10.00000000000000000 ) ) ;
#39581 = CARTESIAN_POINT ( 'NONE',  ( 75.62235313057280450, 64.20969772940269138, -14.41545499348065285 ) ) ;
#39582 = CARTESIAN_POINT ( 'NONE',  ( 78.48653837275075773, 47.85077451888660960, 13.91762572861853187 ) ) ;
#39583 = B_SPLINE_CURVE_WITH_KNOTS ( 'NONE', 3,
 ( #37188, #30593, #21990, #91427, #61479, #8293, #92428, #99508, #22976, #39159 ),
 .UNSPECIFIED., .F., .F.,
 ( 4, 2, 2, 2, 4 ),
 ( 0.000000000000000000, 0.0004172351265548456087, 0.0008344702531096912174, 0.001251705379664536880, 0.001668940506219382435 ),
 .UNSPECIFIED. ) ;
#39584 = CARTESIAN_POINT ( 'NONE',  ( 107.7791399978856930, 233.0333772461660828, 9.188101187500095079 ) ) ;
#39585 = ORIENTED_EDGE ( 'NONE', *, *, #28118, .F. ) ;
#39586 = CARTESIAN_POINT ( 'NONE',  ( 190.2594329105515101, 301.1079909101196108, -4.731131889240534960 ) ) ;
#39587 = DIRECTION ( 'NONE',  ( 0.3940053768033583426, -0.6824373310787393843, 0.6156614753256619554 ) ) ;
#39588 = CARTESIAN_POINT ( 'NONE',  ( 193.7609008727193043, 262.8443104439116951, 4.759103018491034121 ) ) ;
#39589 = CARTESIAN_POINT ( 'NONE',  ( 154.9792334219179679, 262.2150889255981951, -17.21325849938693153 ) ) ;
#39590 = B_SPLINE_CURVE_WITH_KNOTS ( 'NONE', 3,
 ( #68951, #61352, #35200, #30460, #34698, #58488, #20518, #12420, #66105, #27622, #97529, #4819, #74731, #92307 ),
 .UNSPECIFIED., .F., .F.,
 ( 4, 2, 2, 2, 2, 2, 4 ),
 ( 0.0009458495952914972114, 0.001465415157218448623, 0.001725197938181909692, 0.001984980719145370762, 0.002244763500108832265, 0.002504546281072293334, 0.003024111842999374633 ),
 .UNSPECIFIED. ) ;
#39591 = CARTESIAN_POINT ( 'NONE',  ( 163.7136804588959649, 247.0865828815331042, 6.783386239354816105 ) ) ;
#39592 = CARTESIAN_POINT ( 'NONE',  ( 83.58592293191674116, 51.62412561587523641, -14.84978998814507989 ) ) ;
#39593 = CARTESIAN_POINT ( 'NONE',  ( 165.4298696296856690, 283.8953809392911580, -8.443581878439131216 ) ) ;
#39594 = ORIENTED_EDGE ( 'NONE', *, *, #59547, .F. ) ;
#39595 = CARTESIAN_POINT ( 'NONE',  ( 162.7459776558209228, 248.7626933030860812, -9.895605163646791880 ) ) ;
#39597 = EDGE_CURVE ( 'NONE', #28763, #84992, #27976, .T. ) ;
#39596 = CARTESIAN_POINT ( 'NONE',  ( 181.9913924001663759, 260.5072070915913400, 9.621015379077912044 ) ) ;
#39598 = CARTESIAN_POINT ( 'NONE',  ( 74.61783790005046058, 67.04252370310037179, 12.50665000838213814 ) ) ;
#39599 = CARTESIAN_POINT ( 'NONE',  ( 132.6505673846437503, 238.2048013555409796, 4.594050593750051981 ) ) ;
#39600 = CARTESIAN_POINT ( 'NONE',  ( 198.4782858197754649, 286.8725200914082620, -17.44895083299520522 ) ) ;
#39601 = CARTESIAN_POINT ( 'NONE',  ( 189.1685910125652299, 299.5261110243415033, 4.889329439728404836 ) ) ;
#39602 = CARTESIAN_POINT ( 'NONE',  ( 187.3694706215540862, 281.3094075288585714, -17.25064062178364566 ) ) ;
#39603 = DIRECTION ( 'NONE',  ( 0.000000000000000000, -0.000000000000000000, 1.000000000000000000 ) ) ;
#39604 = CARTESIAN_POINT ( 'NONE',  ( 47.42782112377506820, 204.3149278399160664, 9.188101187500093303 ) ) ;
#39605 = CARTESIAN_POINT ( 'NONE',  ( 85.41379983563213329, 48.29620419992356517, -11.76667240678645321 ) ) ;
#39606 = VERTEX_POINT ( 'NONE', #77628 ) ;
#39607 = DIRECTION ( 'NONE',  ( -0.4999999999999999445, 0.8660254037844385966, 0.000000000000000000 ) ) ;
#39608 = LINE ( 'NONE', #9238, #22130 ) ;
#39609 = CARTESIAN_POINT ( 'NONE',  ( 72.04273812837081437, 59.28583566120335746, 15.34548535902080246 ) ) ;
#39610 = CARTESIAN_POINT ( 'NONE',  ( 174.5571948831425857, 262.1308976863569455, 14.30389198049646282 ) ) ;
#39611 = CARTESIAN_POINT ( 'NONE',  ( 82.00121032730237403, 41.82734585847611442, -5.599361062352755880 ) ) ;
#39612 = CARTESIAN_POINT ( 'NONE',  ( 203.4696564630250464, 278.2272125378923988, -16.38980782817167636 ) ) ;
#39613 = CARTESIAN_POINT ( 'NONE',  ( 179.2813879323843196, 261.6109213834521938, 12.22300016988861415 ) ) ;
#39614 = CARTESIAN_POINT ( 'NONE',  ( 124.2065593741477301, 252.5177522451419350, 5.000000000000046185 ) ) ;
#39615 = B_SPLINE_SURFACE_WITH_KNOTS ( 'NONE', 3, 1, ( 
 ( #88735, #90211 ),
 ( #69332, #76924 ),
 ( #71350, #48023 ),
 ( #9034, #92668 ),
 ( #16133, #61721 ),
 ( #16628, #84575 ),
 ( #31325, #30835 ),
 ( #86592, #1450 ),
 ( #38920, #40416 ),
 ( #938, #23221 ),
 ( #24237, #8537 ),
 ( #39906, #85067 ),
 ( #69825, #54110 ),
 ( #62715, #31814 ),
 ( #62212, #85592 ),
 ( #15615, #78452 ),
 ( #32330, #24725 ),
 ( #70324, #22740 ),
 ( #436, #17127 ),
 ( #47031, #55608 ),
 ( #63231, #46513 ),
 ( #61223, #47524 ),
 ( #77948, #93673 ),
 ( #78967, #77451 ),
 ( #100253, #70839 ),
 ( #9554, #55115 ),
 ( #30333, #94173 ),
 ( #23714, #53619 ),
 ( #8047, #38417 ),
 ( #92187, #93164 ),
 ( #15113, #7525 ),
 ( #46007, #54609 ),
 ( #39409, #86102 ),
 ( #72362, #25751 ) ),
 .UNSPECIFIED., .T., .F., .F.,
 ( 4, 2, 2, 2, 2, 2, 2, 2, 2, 2, 2, 2, 2, 2, 2, 2, 4 ),
 ( 2, 2 ),
 ( 0.000000000000000000, 0.06250000000000000000, 0.1250000000000000000, 0.1875000000000000000, 0.2500000000000000000, 0.3125000000000000000, 0.3750000000000000000, 0.4375000000000000000, 0.5000000000000000000, 0.5625000000000000000, 0.6250000000000000000, 0.6875000000000000000, 0.7500000000000000000, 0.8125000000000000000, 0.8750000000000000000, 0.9375000000000000000, 1.000000000000000000 ),
 ( 0.000000000000000000, 1.000000000000000000 ),
 .UNSPECIFIED. ) ;
#39616 = CARTESIAN_POINT ( 'NONE',  ( 147.8791740781505837, 276.5127524457575987, 2.771564245682613947 ) ) ;
#39617 = ORIENTED_EDGE ( 'NONE', *, *, #79934, .T. ) ;
#39618 = VECTOR ( 'NONE', #4934, 1000.000000000000000 ) ;
#39619 = CARTESIAN_POINT ( 'NONE',  ( 202.9685995779611858, 279.0950685203052899, 16.84977534244423580 ) ) ;
#39620 = CARTESIAN_POINT ( 'NONE',  ( 87.68052222859077460, 44.70628762572462733, 5.023047487083897700 ) ) ;
#39621 = CARTESIAN_POINT ( 'NONE',  ( 25.42527643493543366, 194.6744531367911293, 4.594050593750047540 ) ) ;
#39622 = CARTESIAN_POINT ( 'NONE',  ( 13.61667370911268193, 23.56454794089040661, 10.00000000000000355 ) ) ;
#39623 = LINE ( 'NONE', #39125, #59754 ) ;
#39624 = CARTESIAN_POINT ( 'NONE',  ( 38.27158024800235125, 186.2365022471901739, -10.00000000000009237 ) ) ;
#39625 = B_SPLINE_CURVE_WITH_KNOTS ( 'NONE', 3,
 ( #4585, #98299, #13200, #74000, #43054, #81622, #35479, #28888, #27394, #44058, #42564, #52166, #59765, #12195, #58762, #26896, #65875, #57774, #81138, #96831, #89732, #51692, #88748, #6078 ),
 .UNSPECIFIED., .F., .F.,
 ( 4, 2, 2, 2, 2, 2, 2, 2, 2, 2, 2, 4 ),
 ( 0.000000000000000000, 0.1250000000000211220, 0.2500000000000422440, 0.3750000000000633937, 0.4375000000000662248, 0.5000000000000690559, 0.5625000000000719425, 0.6250000000000748290, 0.6875000000000777156, 0.7500000000000806022, 0.8750000000000404121, 1.000000000000000000 ),
 .UNSPECIFIED. ) ;
#39626 = CARTESIAN_POINT ( 'NONE',  ( 44.10470679282202866, 121.9603419428074602, 10.00000000000000000 ) ) ;
#39628 = CARTESIAN_POINT ( 'NONE',  ( 63.88265089144443465, 201.5643266524160424, 9.188101187500095079 ) ) ;
#39627 = CARTESIAN_POINT ( 'NONE',  ( 198.2339335403562472, 277.5049642442517097, -15.43335200160522902 ) ) ;
#39629 = CARTESIAN_POINT ( 'NONE',  ( 174.0414442612575954, 288.4808356476244739, 7.602831793599980514 ) ) ;
#39630 = CARTESIAN_POINT ( 'NONE',  ( 183.6498318386265396, 256.3252116762061519, 1.424693195823348635 ) ) ;
#39631 = CARTESIAN_POINT ( 'NONE',  ( 157.4805323096970255, 257.8827121670497036, -16.70238855805511591 ) ) ;
#39632 = CARTESIAN_POINT ( 'NONE',  ( 18.10888558598233544, 12.58380873178785997, 6.180339887498953466 ) ) ;
#39633 = ORIENTED_EDGE ( 'NONE', *, *, #62082, .T. ) ;
#39634 = CARTESIAN_POINT ( 'NONE',  ( 23.90999230191033575, 194.6115022471903160, -5.000000000000047962 ) ) ;
#39635 = CARTESIAN_POINT ( 'NONE',  ( 185.0112656319525115, 294.4118031042779080, 9.900635645151082187 ) ) ;
#39636 = CARTESIAN_POINT ( 'NONE',  ( 25.98835327777827686, 41.64452202306098627, 10.00000000000000000 ) ) ;
#39637 = CARTESIAN_POINT ( 'NONE',  ( -10.21716836350912949, 177.1589784336661637, -6.496448406907675876E-16 ) ) ;
#39638 = CARTESIAN_POINT ( 'NONE',  ( 26.97895004263468266, 38.68290643055188127, 3.479690158560446702E-15 ) ) ;
#39640 = CARTESIAN_POINT ( 'NONE',  ( 170.5783285705315961, 263.4208030108840717, 15.80046225904663260 ) ) ;
#39639 = CARTESIAN_POINT ( 'NONE',  ( 164.1930575273928810, 260.6154384242434503, -16.15766538543017816 ) ) ;
#39641 = EDGE_CURVE ( 'NONE', #74638, #49426, #99924, .T. ) ;
#39642 = CARTESIAN_POINT ( 'NONE',  ( 188.9382125046037117, 261.1427886392369828, 6.789719310133031982 ) ) ;
#39643 = CARTESIAN_POINT ( 'NONE',  ( -42.72532191160158987, 28.29708160126036987, 10.00000000000000000 ) ) ;
#39644 = CARTESIAN_POINT ( 'NONE',  ( 187.0838235210196672, 259.2678003084403144, -2.401093518989122266 ) ) ;
#39645 = CARTESIAN_POINT ( 'NONE',  ( 66.31377247145708509, 69.19807880125443944, 2.483205996023140294 ) ) ;
#39646 = ORIENTED_EDGE ( 'NONE', *, *, #53934, .F. ) ;
#39647 = CARTESIAN_POINT ( 'NONE',  ( 136.0602820919951341, 259.3615022471902876, 5.000000000000046185 ) ) ;
#39648 = CARTESIAN_POINT ( 'NONE',  ( 144.2948532952960932, 258.0163529461947292, -10.00000000000009592 ) ) ;
#39649 = CARTESIAN_POINT ( 'NONE',  ( 155.3647120480568162, 278.9503195987401796, -5.223984518467562843 ) ) ;
#39650 = CARTESIAN_POINT ( 'NONE',  ( 10.91775413003093931, 21.70171378149917985, -9.188101187500004485 ) ) ;
#39651 = CARTESIAN_POINT ( 'NONE',  ( 206.9483995484939101, 272.2018527673814106, 9.530154192725417417 ) ) ;
#39652 = AXIS2_PLACEMENT_3D ( 'NONE', #18580, #80414, #48971 ) ;
#39653 = CARTESIAN_POINT ( 'NONE',  ( 159.3237119419271437, 254.6902313965507858, -15.56765445935501191 ) ) ;
#39654 = DIRECTION ( 'NONE',  ( 0.4999999999999992784, -0.8660254037844390407, 0.000000000000000000 ) ) ;
#39655 = CARTESIAN_POINT ( 'NONE',  ( 88.86189758574333553, 212.1115022471902023, -5.000000000000041744 ) ) ;
#39656 = CARTESIAN_POINT ( 'NONE',  ( 191.4149729938089592, 298.5499520618976135, 8.351909744838231120 ) ) ;
#39657 = DIRECTION ( 'NONE',  ( 0.000000000000000000, 0.000000000000000000, -1.000000000000000000 ) ) ;
#39658 = CARTESIAN_POINT ( 'NONE',  ( 67.41069134358542669, 70.04696837240071261, -4.305487806446024446E-08 ) ) ;
#39659 = ORIENTED_EDGE ( 'NONE', *, *, #65240, .T. ) ;
#39660 = EDGE_LOOP ( 'NONE', ( #77356, #78518, #31986, #21072 ) ) ;
#39661 = CARTESIAN_POINT ( 'NONE',  ( 156.2183318835597561, 276.9731782824784432, -10.13063037517403231 ) ) ;
#39662 = CARTESIAN_POINT ( 'NONE',  ( 49.80235952159635104, 79.38263285747564169, -10.00000000000000000 ) ) ;
#39663 = ORIENTED_EDGE ( 'NONE', *, *, #76116, .F. ) ;
#39664 = FACE_OUTER_BOUND ( 'NONE', #91679, .T. ) ;
#39665 = CARTESIAN_POINT ( 'NONE',  ( 188.7627825353981166, 297.5844699726765725, 7.724845922223074979 ) ) ;
#39666 = VERTEX_POINT ( 'NONE', #83246 ) ;
#39667 = PLANE ( 'NONE',  #63664 ) ;
#39668 = CARTESIAN_POINT ( 'NONE',  ( 79.23201746742373075, 59.47846325219751407, -16.53522573291432352 ) ) ;
#39669 = CARTESIAN_POINT ( 'NONE',  ( 196.6800254274587019, 289.9871984561398222, -17.90749311895638129 ) ) ;
#39670 = CARTESIAN_POINT ( 'NONE',  ( 80.82248141129124974, 43.03714829935063335, 9.686067628345497837 ) ) ;
#39671 = EDGE_LOOP ( 'NONE', ( #12340, #84380, #66277, #26868 ) ) ;
#39672 = CARTESIAN_POINT ( 'NONE',  ( 203.2795549558504433, 278.5564780069144035, 16.55170960561796889 ) ) ;
#39673 = LINE ( 'NONE', #92934, #10078 ) ;
#39674 = CARTESIAN_POINT ( 'NONE',  ( 175.4606724842758751, 268.3091254637062661, -17.51855393743042910 ) ) ;
#39675 = ORIENTED_EDGE ( 'NONE', *, *, #74606, .F. ) ;
#39676 = VERTEX_POINT ( 'NONE', #75624 ) ;
#39677 = VERTEX_POINT ( 'NONE', #13812 ) ;
#39678 = CARTESIAN_POINT ( 'NONE',  ( 73.67041371685652962, 62.60474759977234527, 14.58206332630679292 ) ) ;
#39679 = VECTOR ( 'NONE', #48554, 1000.000000000000114 ) ;
#39680 = VERTEX_POINT ( 'NONE', #6211 ) ;
#39681 = CARTESIAN_POINT ( 'NONE',  ( 161.1429874292947488, 271.1544374080688726, 16.26257973483764729 ) ) ;
#39682 = ORIENTED_EDGE ( 'NONE', *, *, #17833, .F. ) ;
#39683 = CARTESIAN_POINT ( 'NONE',  ( 88.05624235485146301, 44.55787864911079765, -5.145732200269208967 ) ) ;
#39684 = LINE ( 'NONE', #16909, #70799 ) ;
#39685 = CARTESIAN_POINT ( 'NONE',  ( 177.9925615710933755, 254.8251403409008731, -7.350624415798725053 ) ) ;
#39686 = CARTESIAN_POINT ( 'NONE',  ( 194.9636675848471441, 292.9600174435121289, -15.57898232594655319 ) ) ;
#39687 = CARTESIAN_POINT ( 'NONE',  ( 82.53534059687447666, 53.28184184896795017, -15.31749960034531099 ) ) ;
#39688 = DIRECTION ( 'NONE',  ( 0.5000000000000048850, -0.8660254037844358210, 0.000000000000000000 ) ) ;
#39689 = DIRECTION ( 'NONE',  ( 1.000000000000000000, 1.156482317317871331E-15, 0.000000000000000000 ) ) ;
#39690 = CARTESIAN_POINT ( 'NONE',  ( 17.99393647837114329, 33.49540643055186706, 3.479690158560446702E-15 ) ) ;
#39691 = EDGE_CURVE ( 'NONE', #97801, #49707, #53303, .T. ) ;
#39692 = CARTESIAN_POINT ( 'NONE',  ( 198.6255909461775104, 276.8423615036599585, -15.32991266925497342 ) ) ;
#39693 = CYLINDRICAL_SURFACE ( 'NONE', #46667, 17.82106496071139645 ) ;
#39695 = ORIENTED_EDGE ( 'NONE', *, *, #49987, .F. ) ;
#39694 = FACE_OUTER_BOUND ( 'NONE', #74493, .T. ) ;
#39696 = CARTESIAN_POINT ( 'NONE',  ( 147.4105755286778106, 275.3243889417975083, -3.778870683123901397 ) ) ;
#39697 = CARTESIAN_POINT ( 'NONE',  ( 191.2557879401978198, 261.3776189723048446, -4.694998167070893125 ) ) ;
#39698 = CARTESIAN_POINT ( 'NONE',  ( 206.7923762329701276, 272.4720930770340033, -9.496103119940368487 ) ) ;
#39699 = CARTESIAN_POINT ( 'NONE',  ( -14.83262083840144996, 124.7156766241961208, 37.49999999999998579 ) ) ;
#39700 = CARTESIAN_POINT ( 'NONE',  ( 85.03726002374489212, 45.61754386869292688, -9.156370252284901312 ) ) ;
#39701 = EDGE_CURVE ( 'NONE', #75907, #46284, #68505, .T. ) ;
#39702 = CARTESIAN_POINT ( 'NONE',  ( 161.8873598795597388, 250.2498629158519350, 13.90822209621415873 ) ) ;
#39703 = CARTESIAN_POINT ( 'NONE',  ( 106.5432495796755603, 238.9865022471903160, 10.00000000000009415 ) ) ;
#39704 = ORIENTED_EDGE ( 'NONE', *, *, #46818, .T. ) ;
#39705 = CARTESIAN_POINT ( 'NONE',  ( -58.00277386063315532, 34.50477571329874138, 10.00000000000000000 ) ) ;
#39706 = B_SPLINE_CURVE_WITH_KNOTS ( 'NONE', 3,
 ( #91634, #51608, #22202, #6995 ),
 .UNSPECIFIED., .F., .F.,
 ( 4, 4 ),
 ( 0.01573702636073541841, 0.02454403038988591315 ),
 .UNSPECIFIED. ) ;
#39707 = DIRECTION ( 'NONE',  ( 0.000000000000000000, 0.000000000000000000, 1.000000000000000000 ) ) ;
#39709 = EDGE_CURVE ( 'NONE', #68725, #33752, #60888, .T. ) ;
#39708 = DIRECTION ( 'NONE',  ( -0.6056412518070772855, -0.7957378174433814566, 0.000000000000000000 ) ) ;
#39710 = CARTESIAN_POINT ( 'NONE',  ( 17.25242200676955306, 190.7677522451419065, -5.000000000000047962 ) ) ;
#39711 = CARTESIAN_POINT ( 'NONE',  ( 89.26784699199328088, 222.3458772461660544, 9.188101187500095079 ) ) ;
#39712 = CARTESIAN_POINT ( 'NONE',  ( 82.33219852380105408, 40.34800253957620697, -1.053958929052360549 ) ) ;
#39713 = CARTESIAN_POINT ( 'NONE',  ( 14.35886136108867994, 13.45404122711132011, -8.090169943749478065 ) ) ;
#39714 = CARTESIAN_POINT ( 'NONE',  ( 167.6527552166903376, 278.6792754734481719, -13.36931194722780170 ) ) ;
#39716 = CARTESIAN_POINT ( 'NONE',  ( 75.62574292670869625, 65.55640874641136406, 13.80250227997792756 ) ) ;
#39715 = CARTESIAN_POINT ( 'NONE',  ( 6.129408228687162286, 174.3458772461660828, 9.188101187500095079 ) ) ;
#39717 = VECTOR ( 'NONE', #35129, 1000.000000000000114 ) ;
#39718 = LINE ( 'NONE', #63546, #2631 ) ;
#39719 = VERTEX_POINT ( 'NONE', #7200 ) ;
#39720 = EDGE_LOOP ( 'NONE', ( #35477, #62857, #24152 ) ) ;
#39721 = DIRECTION ( 'NONE',  ( 0.5000000000000003331, -0.8660254037844385966, 0.000000000000000000 ) ) ;
#39722 = CARTESIAN_POINT ( 'NONE',  ( 197.5944296959598319, 265.4027214831109518, -2.921024236943222885 ) ) ;
#39723 = CARTESIAN_POINT ( 'NONE',  ( 83.25269581296497279, 46.42390702885197129, -11.11998686039522433 ) ) ;
#39724 = CARTESIAN_POINT ( 'NONE',  ( 23.53456118939196529, 35.36126292948896577, 6.180339887498949913 ) ) ;
#39725 = FACE_OUTER_BOUND ( 'NONE', #38455, .T. ) ;
#39726 = CARTESIAN_POINT ( 'NONE',  ( 74.25334530965831448, 67.88333409418525832, -11.69134486559788044 ) ) ;
#39727 = CARTESIAN_POINT ( 'NONE',  ( 30.18841615574984516, 197.4244531367911293, -4.594050593750046652 ) ) ;
#39728 = CARTESIAN_POINT ( 'NONE',  ( 100.8960422556166634, 222.3927522451418213, 10.00000000000009948 ) ) ;
#39729 = ORIENTED_EDGE ( 'NONE', *, *, #56731, .T. ) ;
#39730 = CARTESIAN_POINT ( 'NONE',  ( 150.0434472053995307, 271.6953193618362548, -11.68999578780283244 ) ) ;
#39731 = CARTESIAN_POINT ( 'NONE',  ( 182.6142383756292418, 260.6848368803231892, -10.84370499219341077 ) ) ;
#39732 = CARTESIAN_POINT ( 'NONE',  ( 152.2705230281304409, 271.0405980996342237, 14.27451841150712042 ) ) ;
#39733 = CARTESIAN_POINT ( 'NONE',  ( 157.2464636617698375, 258.2881309577184652, 18.14284729738657731 ) ) ;
#39734 = CARTESIAN_POINT ( 'NONE',  ( 155.4216552449402684, 261.4487918497463284, 18.51722274565528892 ) ) ;
#39735 = CARTESIAN_POINT ( 'NONE',  ( 161.3773209892555371, 251.1332761876949746, -14.50043705923759241 ) ) ;
#39736 = VECTOR ( 'NONE', #25689, 1000.000000000000000 ) ;
#39737 = DIRECTION ( 'NONE',  ( 0.000000000000000000, 0.000000000000000000, 1.000000000000000000 ) ) ;
#39738 = CARTESIAN_POINT ( 'NONE',  ( 148.0346525705264469, 274.2434557974783615, -9.381294579651672905 ) ) ;
#39739 = ADVANCED_FACE ( 'NONE', ( #38084 ), #71029, .T. ) ;
#39740 = EDGE_CURVE ( 'NONE', #90942, #23100, #64507, .T. ) ;
#39741 = CARTESIAN_POINT ( 'NONE',  ( 190.7982574810033611, 262.8194055429554510, 8.405793748174573921 ) ) ;
#39742 = CARTESIAN_POINT ( 'NONE',  ( 171.7060500237028862, 279.6726968596310030, 14.88215948178559245 ) ) ;
#39743 = CARTESIAN_POINT ( 'NONE',  ( 189.9686529740312153, 299.6116365339944423, 6.575253125843024016 ) ) ;
#39744 = CARTESIAN_POINT ( 'NONE',  ( 68.75179611904260923, 68.50344063802555183, 6.907652022257806834 ) ) ;
#39745 = CARTESIAN_POINT ( 'NONE',  ( 147.6430623265936219, 274.9217099957185155, 8.258152514891218487 ) ) ;
#39746 = CARTESIAN_POINT ( 'NONE',  ( 65.74726825304114186, 69.08659106095529978, 2.128305819671951817E-12 ) ) ;
#39747 = ORIENTED_EDGE ( 'NONE', *, *, #82806, .F. ) ;
#39748 = AXIS2_PLACEMENT_3D ( 'NONE', #23425, #40120, #24933 ) ;
#39749 = CARTESIAN_POINT ( 'NONE',  ( 73.67824366217406862, 55.52431661998091528, 16.58293631993679540 ) ) ;
#39750 = CARTESIAN_POINT ( 'NONE',  ( 161.8840393808384022, 251.8702681966305477, -13.97960957670215087 ) ) ;
#39751 = CARTESIAN_POINT ( 'NONE',  ( 104.9102572999672276, 237.5024278399160949, 9.188101187500095079 ) ) ;
#39752 = CARTESIAN_POINT ( 'NONE',  ( 13.72994409607376731, 16.43085787977761569, -9.188101187500008038 ) ) ;
#39753 = CARTESIAN_POINT ( 'NONE',  ( -15.06115086838940442, 172.1115022471903160, -5.000000000000047962 ) ) ;
#39754 = EDGE_CURVE ( 'NONE', #48297, #68650, #66064, .T. ) ;
#39755 = PLANE ( 'NONE',  #82429 ) ;
#39757 = CARTESIAN_POINT ( 'NONE',  ( 191.5711784964392166, 276.9236626822979588, 16.85412083571288022 ) ) ;
#39756 = CARTESIAN_POINT ( 'NONE',  ( 157.5520850189458884, 257.7587792392113215, 16.71892742266126319 ) ) ;
#39758 = CARTESIAN_POINT ( 'NONE',  ( 150.8870980228296332, 269.3028753482705611, -13.88216063016896307 ) ) ;
#39759 = CARTESIAN_POINT ( 'NONE',  ( 192.9146452215483123, 263.8600050127276972, -4.623449015741573298 ) ) ;
#39760 = CARTESIAN_POINT ( 'NONE',  ( 149.8974208606144600, 271.7624278638419355, -11.58230692921836358 ) ) ;
#39761 = CARTESIAN_POINT ( 'NONE',  ( 116.3166592645429205, 226.4155109091896350, 2.679491924311254714 ) ) ;
#39762 = DIRECTION ( 'NONE',  ( 0.2359789242578316237, 0.9717581732643758574, 0.000000000000000000 ) ) ;
#39763 = LINE ( 'NONE', #78313, #78206 ) ;
#39764 = VERTEX_POINT ( 'NONE', #9735 ) ;
#39765 = CARTESIAN_POINT ( 'NONE',  ( 190.2885894641050868, 266.2465236892521148, 10.78400978751670003 ) ) ;
#39766 = CARTESIAN_POINT ( 'NONE',  ( 178.9380535331071655, 280.8279290640091403, 16.38556303516354262 ) ) ;
#39767 = CARTESIAN_POINT ( 'NONE',  ( 196.5175218668017862, 267.6197207801589002, 9.577823450216618184 ) ) ;
#39768 = EDGE_CURVE ( 'NONE', #57662, #82888, #59638, .T. ) ;
#39769 = ADVANCED_FACE ( 'NONE', ( #56294 ), #79683, .F. ) ;
#39770 = ORIENTED_EDGE ( 'NONE', *, *, #54704, .F. ) ;
#39771 = CARTESIAN_POINT ( 'NONE',  ( 83.68684867813932726, 42.36207227428623412, 5.946836090295558819 ) ) ;
#39772 = CARTESIAN_POINT ( 'NONE',  ( 183.5722823471954257, 264.5482469279784823, -13.32579016364044655 ) ) ;
#39773 = CARTESIAN_POINT ( 'NONE',  ( 9.830230629461709668, 30.95267373526312227, 10.00000000000000000 ) ) ;
#39774 = CARTESIAN_POINT ( 'NONE',  ( 192.0523540417460993, 298.0025604169266558, 12.03387399082417275 ) ) ;
#39775 = ORIENTED_EDGE ( 'NONE', *, *, #33012, .T. ) ;
#39776 = CARTESIAN_POINT ( 'NONE',  ( 201.0718222649304607, 273.3369752706136069, -13.40913439694983289 ) ) ;
#39777 = CARTESIAN_POINT ( 'NONE',  ( 37.65389587561885776, 30.24335787977765833, -9.188101187500008038 ) ) ;
#39778 = CARTESIAN_POINT ( 'NONE',  ( 73.08568754922542610, 70.50375409671433147, -7.993246346743384301 ) ) ;
#39779 = ORIENTED_EDGE ( 'NONE', *, *, #95511, .F. ) ;
#39780 = CARTESIAN_POINT ( 'NONE',  ( 167.1424731200726228, 249.5982725804538802, 6.966350190857109048 ) ) ;
#39781 = LINE ( 'NONE', #16511, #32144 ) ;
#39782 = DIRECTION ( 'NONE',  ( -0.8660254037844387076, -0.4999999999999998890, -0.000000000000000000 ) ) ;
#39783 = ORIENTED_EDGE ( 'NONE', *, *, #74094, .T. ) ;
#39784 = CARTESIAN_POINT ( 'NONE',  ( 79.57595289148407858, 59.38824344631919416, 16.55667218292645870 ) ) ;
#39785 = CARTESIAN_POINT ( 'NONE',  ( 83.53204454370725784, 52.39401912150449903, -15.17729711222452238 ) ) ;
#39786 = CARTESIAN_POINT ( 'NONE',  ( -62.95439910331221256, 68.06504152958493137, 60.00000000000000000 ) ) ;
#39787 = LINE ( 'NONE', #71745, #96814 ) ;
#39788 = VECTOR ( 'NONE', #32020, 1000.000000000000227 ) ;
#39789 = CARTESIAN_POINT ( 'NONE',  ( 43.45144817956826699, 30.80170272979930601, 7.433330006724137462 ) ) ;
#39790 = CARTESIAN_POINT ( 'NONE',  ( 203.2187760522547819, 278.6617501559703101, -15.08675642319914978 ) ) ;
#39791 = VERTEX_POINT ( 'NONE', #4607 ) ;
#39793 = ORIENTED_EDGE ( 'NONE', *, *, #87572, .T. ) ;
#39792 =( BOUNDED_CURVE ( )  B_SPLINE_CURVE ( 2, ( #35494, #81151, #11718, #42580, #96341, #17818, #57291, #65400, #26413 ),
 .UNSPECIFIED., .F., .T. ) 
 B_SPLINE_CURVE_WITH_KNOTS ( ( 3, 2, 2, 2, 3 ),
 ( 0.5443548387096773800, 0.5456989247311827551, 0.5483870967741935054, 0.5510752688172042557, 0.5524193548387096309 ),
 .UNSPECIFIED. ) 
 CURVE ( )  GEOMETRIC_REPRESENTATION_ITEM ( )  RATIONAL_B_SPLINE_CURVE ( ( 0.9330127018922194093, 0.9330127018922194093, 1.000000000000000000, 0.8660254037844387076, 1.000000000000000000, 0.8660254037844387076, 1.000000000000000000, 0.9330127018922194093, 0.9330127018922194093 ) ) 
 REPRESENTATION_ITEM ( '' )  );
#39795 = AXIS2_PLACEMENT_3D ( 'NONE', #27653, #50926, #51430 ) ;
#39794 = CARTESIAN_POINT ( 'NONE',  ( 175.7956577457310345, 258.6345868136107242, 13.14558633677379973 ) ) ;
#39796 = VERTEX_POINT ( 'NONE', #60149 ) ;
#39797 = CARTESIAN_POINT ( 'NONE',  ( 77.22954108468842094, 49.67394351277923192, -14.99406558715285165 ) ) ;
#39798 = EDGE_LOOP ( 'NONE', ( #17428, #32955, #98816, #53152 ) ) ;
#39799 = CARTESIAN_POINT ( 'NONE',  ( 87.09644473823584576, 45.85687564672072369, -8.636203292310963064 ) ) ;
#39800 = CARTESIAN_POINT ( 'NONE',  ( 155.6066474290145720, 261.1283759879266881, -18.16552045242181279 ) ) ;
#39801 = ORIENTED_EDGE ( 'NONE', *, *, #15010, .T. ) ;
#39802 = CARTESIAN_POINT ( 'NONE',  ( 165.7267109360765573, 274.6484224846600455, -15.16830425928928072 ) ) ;
#39803 = CARTESIAN_POINT ( 'NONE',  ( 206.4839639422192192, 273.0062788342933118, -11.22308919026441210 ) ) ;
#39804 = CARTESIAN_POINT ( 'NONE',  ( 190.5841104648970088, 300.5456328899159644, 3.298325803792328870 ) ) ;
#39805 = CARTESIAN_POINT ( 'NONE',  ( 196.1252721995043942, 284.4712197134549001, -17.81715240067734030 ) ) ;
#39806 = CARTESIAN_POINT ( 'NONE',  ( 82.53920793150861357, 41.02048457221435740, 1.071569650286623210 ) ) ;
#39808 = CARTESIAN_POINT ( 'NONE',  ( 171.5407152967187017, 250.9167206134208072, -5.638389805452348469 ) ) ;
#39807 = B_SPLINE_CURVE_WITH_KNOTS ( 'NONE', 3,
 ( #57011, #4316, #43807, #34228, #28114, #87990, #80371, #10942, #96071, #42307, #80882, #34716, #96572, #41812, #99032, #7303, #38184, #68604, #76238, #91961, #36205, #30613, #36702, #45788, #77208, #83352, #75233, #59495, #90473, #13918, #60489 ),
 .UNSPECIFIED., .F., .F.,
 ( 4, 3, 3, 3, 3, 3, 3, 3, 3, 3, 4 ),
 ( 0.000000000000000000, 0.1333490885032358464, 0.3007194338854307092, 0.4699862290245053198, 0.5844252810809311693, 0.6686540514502750110, 0.7354980260655511470, 0.8028463152565725736, 0.8633854507757335872, 0.9437142632667383513, 1.000000000000000000 ),
 .UNSPECIFIED. ) ;
#39809 = CARTESIAN_POINT ( 'NONE',  ( -13.11024591527734628, 6.000000000000000000, 32.50000000000000000 ) ) ;
#39810 = CARTESIAN_POINT ( 'NONE',  ( 156.9561170169907030, 280.4813240094630373, 2.086493405815429636 ) ) ;
#39811 = CARTESIAN_POINT ( 'NONE',  ( 130.4855038751826726, 236.9548013555409796, -4.594050593750042211 ) ) ;
#39812 = ORIENTED_EDGE ( 'NONE', *, *, #20917, .F. ) ;
#39813 = CARTESIAN_POINT ( 'NONE',  ( 186.5674233539620275, 262.7087872174366225, -9.046917918335617870 ) ) ;
#39814 = CARTESIAN_POINT ( 'NONE',  ( 42.56377214068922399, 30.28920272979930672, -7.433330006724141015 ) ) ;
#39815 = EDGE_LOOP ( 'NONE', ( #41976, #11086, #74851, #62014 ) ) ;
#39816 = ADVANCED_FACE ( 'NONE', ( #21678 ), #19340, .T. ) ;
#39817 = CARTESIAN_POINT ( 'NONE',  ( 85.74775437209392237, 48.65322352004045570, -12.36257617231559180 ) ) ;
#39818 = CARTESIAN_POINT ( 'NONE',  ( 200.0648741936326189, 273.7901900051996336, 13.73784782553251205 ) ) ;
#39819 = CARTESIAN_POINT ( 'NONE',  ( 180.5509916577576348, 256.1221220636168141, 1.304812651851478433 ) ) ;
#39820 = ADVANCED_FACE ( 'NONE', ( #14074 ), #88268, .T. ) ;
#39821 = DIRECTION ( 'NONE',  ( 0.000000000000000000, 0.000000000000000000, 1.000000000000000000 ) ) ;
#39822 = CARTESIAN_POINT ( 'NONE',  ( 147.4382974802994113, 275.2763731131041141, 3.664996198306503583 ) ) ;
#39823 = CARTESIAN_POINT ( 'NONE',  ( 73.20519886181777736, 66.25595127750490576, 12.42694502862597083 ) ) ;
#39824 = CARTESIAN_POINT ( 'NONE',  ( 80.71670901379776808, 43.21196966927421101, 9.964580085028348577 ) ) ;
#39825 = CARTESIAN_POINT ( 'NONE',  ( 77.83148668010572635, 49.86468963568243851, 15.45682205838144796 ) ) ;
#39826 = VECTOR ( 'NONE', #86422, 1000.000000000000227 ) ;
#39827 = LINE ( 'NONE', #69254, #25291 ) ;
#39828 = CARTESIAN_POINT ( 'NONE',  ( 176.5702065357462516, 255.6409285000345619, -7.288246984450118759 ) ) ;
#39829 = VERTEX_POINT ( 'NONE', #75900 ) ;
#39830 = CARTESIAN_POINT ( 'NONE',  ( 194.9220242159064185, 293.0321458743159724, -14.92681063007793263 ) ) ;
#39831 = CARTESIAN_POINT ( 'NONE',  ( 66.06214068257197880, 68.71579393632852373, -0.4716098740908712950 ) ) ;
#39832 = EDGE_LOOP ( 'NONE', ( #71390, #1344, #53423, #39695 ) ) ;
#39834 = EDGE_CURVE ( 'NONE', #94451, #94798, #18583, .T. ) ;
#39833 = CARTESIAN_POINT ( 'NONE',  ( 188.3791492419724420, 266.3799810227098419, -11.83448844734568794 ) ) ;
#39835 = CARTESIAN_POINT ( 'NONE',  ( 160.0965860327900145, 279.1799484724489275, 10.77100507046937139 ) ) ;
#39836 = CARTESIAN_POINT ( 'NONE',  ( 152.4791540838723449, 266.5453533620465691, -15.88447083262123272 ) ) ;
#39837 = CARTESIAN_POINT ( 'NONE',  ( 148.9694607950094394, 272.6243204573405592, 11.81236034532910573 ) ) ;
#39838 = CARTESIAN_POINT ( 'NONE',  ( -21.31413092498266693, 24.33771760303832465, -10.00000000000000000 ) ) ;
#39840 = CARTESIAN_POINT ( 'NONE',  ( 151.4835999992953930, 274.9817874143876111, -8.672836155307052763 ) ) ;
#39839 = CARTESIAN_POINT ( 'NONE',  ( 161.5256564828909234, 281.5214332243310196, -6.610724726001431684 ) ) ;
#39841 = DIRECTION ( 'NONE',  ( 0.000000000000000000, 0.000000000000000000, 1.000000000000000000 ) ) ;
#39842 = ORIENTED_EDGE ( 'NONE', *, *, #16554, .F. ) ;
#39843 = CARTESIAN_POINT ( 'NONE',  ( 190.1696443193688708, 301.2635093119881162, -4.804312979389741223 ) ) ;
#39844 = CARTESIAN_POINT ( 'NONE',  ( 187.2655409194766207, 261.7880714798743043, -8.837611146579153143 ) ) ;
#39845 = CARTESIAN_POINT ( 'NONE',  ( 155.7631971310857750, 279.9683759737790183, 6.348568169051404197 ) ) ;
#39846 = CARTESIAN_POINT ( 'NONE',  ( 194.7023383591533161, 288.5740446449341334, -17.20894952458154137 ) ) ;
#39847 = EDGE_CURVE ( 'NONE', #23972, #32492, #25654, .T. ) ;
#39848 = CARTESIAN_POINT ( 'NONE',  ( 184.7240172173571295, 296.8390834670735785, -4.377300740651686617 ) ) ;
#39849 = ADVANCED_FACE ( 'NONE', ( #84020 ), #14579, .T. ) ;
#39850 = CARTESIAN_POINT ( 'NONE',  ( 85.38599379065072981, 47.65918632720038062, 11.17564927697190136 ) ) ;
#39851 = CARTESIAN_POINT ( 'NONE',  ( 74.39841895140679640, 68.21392270468032848, 11.95628786500076579 ) ) ;
#39852 = CARTESIAN_POINT ( 'NONE',  ( 74.39150450060409980, 68.40979575363469678, 11.28709398736407721 ) ) ;
#39853 = CARTESIAN_POINT ( 'NONE',  ( 71.56705445201096438, 71.62942160774694855, -3.393990791292070597 ) ) ;
#39854 = CARTESIAN_POINT ( 'NONE',  ( -10.43332761869022640, 164.7833772461660544, -9.188101187500095079 ) ) ;
#39855 = CARTESIAN_POINT ( 'NONE',  ( 84.85626976964255164, 228.9869531367911293, 4.594050593750046652 ) ) ;
#39856 = DIRECTION ( 'NONE',  ( -0.7467472232290888190, 0.000000000000000000, 0.6651079495838592148 ) ) ;
#39857 = CARTESIAN_POINT ( 'NONE',  ( 146.8153075009282134, 276.3554234099810287, -4.113808735271278216 ) ) ;
#39858 = CARTESIAN_POINT ( 'NONE',  ( 147.7963747854073802, 275.1547895869376248, 4.489566192750358731 ) ) ;
#39859 = DIRECTION ( 'NONE',  ( -0.8660254037844387076, -0.4999999999999998890, -0.000000000000000000 ) ) ;
#39860 = CARTESIAN_POINT ( 'NONE',  ( 207.8575108622103755, 270.6272257822888037, -6.381720258959569847 ) ) ;
#39861 = CARTESIAN_POINT ( 'NONE',  ( 84.83678198214029464, 50.32733779148675524, -13.41632123680453148 ) ) ;
#39862 = CIRCLE ( 'NONE', #96571, 70.00000000000001421 ) ;
#39863 = CARTESIAN_POINT ( 'NONE',  ( -22.42236680055709641, 157.8615022471902591, 0.000000000000000000 ) ) ;
#39865 = CARTESIAN_POINT ( 'NONE',  ( 75.83659763066778225, 51.68804710209467856, 15.74957237791803699 ) ) ;
#39864 = CARTESIAN_POINT ( 'NONE',  ( 66.96593609093110899, 67.02900701502181846, 8.585446814251463721 ) ) ;
#39866 = CARTESIAN_POINT ( 'NONE',  ( 177.9223291652669445, 289.9174720514999990, 9.664897302444829918 ) ) ;
#39867 = ADVANCED_FACE ( 'NONE', ( #15544 ), #32260, .T. ) ;
#39868 = CARTESIAN_POINT ( 'NONE',  ( 193.7563803396631670, 267.3524183776476661, 11.90297280730822571 ) ) ;
#39869 = CARTESIAN_POINT ( 'NONE',  ( 161.4733487491374717, 251.3868574054517921, 13.04233661072845329 ) ) ;
#39870 = CARTESIAN_POINT ( 'NONE',  ( 196.4994169513186364, 290.3000215130921902, 16.82935102260526961 ) ) ;
#39871 = AXIS2_PLACEMENT_3D ( 'NONE', #57650, #10576, #41451 ) ;
#39872 = DIRECTION ( 'NONE',  ( 1.000000000000000000, 0.000000000000000000, 0.000000000000000000 ) ) ;
#39873 = CARTESIAN_POINT ( 'NONE',  ( 80.15404930735284950, 58.24487849859600885, -16.60713908503101521 ) ) ;
#39874 = EDGE_CURVE ( 'NONE', #86151, #35869, #90486, .T. ) ;
#39875 = CARTESIAN_POINT ( 'NONE',  ( 38.41565749170202082, 202.1744531367911293, 4.594050593750047540 ) ) ;
#39876 = CARTESIAN_POINT ( 'NONE',  ( 63.34103791831414298, 213.5024278399161233, 9.188101187500095079 ) ) ;
#39877 = CARTESIAN_POINT ( 'NONE',  ( 65.47921168356349142, 198.6115022471902023, -5.000000000000041744 ) ) ;
#39878 = CARTESIAN_POINT ( 'NONE',  ( 88.20050489759562140, 44.09937366127426372, 0.5204581161859789251 ) ) ;
#39879 = ADVANCED_FACE ( 'NONE', ( #54536 ), #76861, .T. ) ;
#39880 = CARTESIAN_POINT ( 'NONE',  ( 84.19158505125736269, 49.36735266572484448, -13.01182045415430011 ) ) ;
#39882 = CARTESIAN_POINT ( 'NONE',  ( 71.64387245797139769, 71.15203705842421300, -6.128722539184691342 ) ) ;
#39881 = CARTESIAN_POINT ( 'NONE',  ( 81.65367170574366185, 42.93584830628305582, -8.967313168971410065 ) ) ;
#39883 = CARTESIAN_POINT ( 'NONE',  ( 200.2233614854171435, 270.9342182064973485, -11.47649089687903334 ) ) ;
#39884 = EDGE_CURVE ( 'NONE', #5726, #41965, #20866, .T. ) ;
#39885 = CARTESIAN_POINT ( 'NONE',  ( 29.48197064213787044, 19.94754757982090609, 5.678558825948272215 ) ) ;
#39886 = CARTESIAN_POINT ( 'NONE',  ( 198.6894790592683080, 286.5067226703918095, -17.06774375037124614 ) ) ;
#39887 = CARTESIAN_POINT ( 'NONE',  ( 148.9504735598738137, 272.6572073132907690, -11.88406006066344744 ) ) ;
#39888 = CARTESIAN_POINT ( 'NONE',  ( 14.44138481658839090, 10.19860640527290663, 2.839279412974134775 ) ) ;
#39889 = CARTESIAN_POINT ( 'NONE',  ( 59.38997056143013964, 205.0958772461660828, -9.188101187500095079 ) ) ;
#39890 = CARTESIAN_POINT ( 'NONE',  ( 76.67779265155198232, 63.58935824677200088, 15.33226443842420927 ) ) ;
#39891 = CYLINDRICAL_SURFACE ( 'NONE', #59139, 10.00000000000010658 ) ;
#39892 = CIRCLE ( 'NONE', #60940, 70.00000000000001421 ) ;
#39893 = CARTESIAN_POINT ( 'NONE',  ( 159.9671766634011192, 253.5757178060795809, 16.49140845334465411 ) ) ;
#39894 = CARTESIAN_POINT ( 'NONE',  ( 73.71491122270572305, 65.62341685233879218, 13.03582331581120002 ) ) ;
#39895 = CARTESIAN_POINT ( 'NONE',  ( 198.9721957120447655, 281.0613474150461570, 17.36564602955951386 ) ) ;
#39896 = ADVANCED_FACE ( 'NONE', ( #9476 ), #2898, .T. ) ;
#39897 = VECTOR ( 'NONE', #94221, 999.9999999999998863 ) ;
#39898 = CARTESIAN_POINT ( 'NONE',  ( 149.0247308281161622, 274.5285899518638075, 9.115861392502811356 ) ) ;
#39899 = CARTESIAN_POINT ( 'NONE',  ( 113.6157903772485298, 229.7365022471902023, -10.00000000000009059 ) ) ;
#39900 = CARTESIAN_POINT ( 'NONE',  ( 33.47037235539275457, 49.41749479597460493, -10.00000000000000000 ) ) ;
#39901 = CARTESIAN_POINT ( 'NONE',  ( 207.1122325394003951, 271.9180857031755636, 7.794245785756032774 ) ) ;
#39902 = ORIENTED_EDGE ( 'NONE', *, *, #12935, .T. ) ;
#39903 = CARTESIAN_POINT ( 'NONE',  ( 76.92873890057781239, 49.89429371730488327, 15.13083596839045519 ) ) ;
#39904 = CARTESIAN_POINT ( 'NONE',  ( 188.0932163354825093, 273.3618889904262801, 15.64081734860616990 ) ) ;
#39905 = ORIENTED_EDGE ( 'NONE', *, *, #40464, .F. ) ;
#39906 = CARTESIAN_POINT ( 'NONE',  ( 206.5081929095101998, 272.9643130319303737, -9.215516226794479238 ) ) ;
#39907 = CARTESIAN_POINT ( 'NONE',  ( 187.4304084080513348, 276.9874324135936376, -16.75430557518339825 ) ) ;
#39908 = CARTESIAN_POINT ( 'NONE',  ( 72.31018532003172083, 68.81932238651856437, -9.557321504549943114 ) ) ;
#39909 = ORIENTED_EDGE ( 'NONE', *, *, #98038, .T. ) ;
#39910 = CARTESIAN_POINT ( 'NONE',  ( 177.2936775833025251, 253.0977458076815765, -0.2642580955292048728 ) ) ;
#39911 = VERTEX_POINT ( 'NONE', #87547 ) ;
#39912 = CARTESIAN_POINT ( 'NONE',  ( 77.21491844529388970, 44.98415679381832888, 0.000000000000000000 ) ) ;
#39913 = CARTESIAN_POINT ( 'NONE',  ( 166.2081174782295534, 287.2918692684091297, 1.312827985884416737 ) ) ;
#39914 = CARTESIAN_POINT ( 'NONE',  ( 176.9878821292914211, 283.3466992399841615, -15.40003107629192769 ) ) ;
#39915 = ORIENTED_EDGE ( 'NONE', *, *, #14341, .T. ) ;
#39916 = CARTESIAN_POINT ( 'NONE',  ( 27.86299091144838869, 21.80170272979927404, 7.433330006724137462 ) ) ;
#39917 = CARTESIAN_POINT ( 'NONE',  ( 79.80790316897787307, 44.74020498821185043, 11.30572903481763092 ) ) ;
#39918 = CARTESIAN_POINT ( 'NONE',  ( 29.01593374150824189, 180.8927522451417929, -10.00000000000009237 ) ) ;
#39919 = CARTESIAN_POINT ( 'NONE',  ( 75.23790730487549183, 66.45095094376505074, -13.14850644163485605 ) ) ;
#39920 = CARTESIAN_POINT ( 'NONE',  ( 79.92738415168659571, 49.14675435996891650, -14.16998936058186409 ) ) ;
#39921 = VERTEX_POINT ( 'NONE', #80417 ) ;
#39922 = CARTESIAN_POINT ( 'NONE',  ( 167.7129959498070093, 276.7492194616727375, 15.67174948013163061 ) ) ;
#39923 = LINE ( 'NONE', #23734, #36773 ) ;
#39924 = VERTEX_POINT ( 'NONE', #63663 ) ;
#39925 = CARTESIAN_POINT ( 'NONE',  ( 170.8911557219925612, 284.9263958063596078, 11.11643632232859602 ) ) ;
#39927 = CARTESIAN_POINT ( 'NONE',  ( 67.69593324464777595, 65.81863650441331970, -10.57774228775840974 ) ) ;
#39926 = CARTESIAN_POINT ( 'NONE',  ( 68.20804129788332659, 65.51386583450461387, 10.45502995425724357 ) ) ;
#39928 = CARTESIAN_POINT ( 'NONE',  ( 81.73360701239045056, 55.69478791075532342, -15.98344718738445991 ) ) ;
#39929 = CARTESIAN_POINT ( 'NONE',  ( 155.4216552449402684, 261.4487918497463284, 18.51722274565528892 ) ) ;
#39930 = CARTESIAN_POINT ( 'NONE',  ( 185.4339105455779304, 292.4495553130619214, -11.40531104680791152 ) ) ;
#39931 = CARTESIAN_POINT ( 'NONE',  ( 164.3024481966923531, 265.7778226775905068, -17.31441928355125270 ) ) ;
#39932 = CARTESIAN_POINT ( 'NONE',  ( 208.0534104968160420, 270.2879176619674695, -3.858664761683422206 ) ) ;
#39933 = CARTESIAN_POINT ( 'NONE',  ( 204.6979730149710690, 269.6043557618498880, 2.446051969963311201 ) ) ;
#39934 = DIRECTION ( 'NONE',  ( -0.9819794923402673792, 0.1889875038809470387, 0.000000000000000000 ) ) ;
#39935 = CARTESIAN_POINT ( 'NONE',  ( 87.96880888631662287, 221.5958772461660544, -9.188101187500095079 ) ) ;
#39936 = ORIENTED_EDGE ( 'NONE', *, *, #64941, .T. ) ;
#39938 = B_SPLINE_CURVE_WITH_KNOTS ( 'NONE', 3,
 ( #26928, #57807, #12232, #82672 ),
 .UNSPECIFIED., .F., .F.,
 ( 4, 4 ),
 ( 0.002905392229856628220, 0.01085320331254635735 ),
 .UNSPECIFIED. ) ;
#39937 = CARTESIAN_POINT ( 'NONE',  ( 151.1926529451685326, 268.7736386982768408, 14.30343427984827365 ) ) ;
#39939 = LINE ( 'NONE', #63265, #47941 ) ;
#39940 = DIRECTION ( 'NONE',  ( -0.000000000000000000, 0.000000000000000000, -1.000000000000000000 ) ) ;
#39941 = AXIS2_PLACEMENT_3D ( 'NONE', #70150, #63066, #53946 ) ;
#39942 = ORIENTED_EDGE ( 'NONE', *, *, #27450, .T. ) ;
#39943 = CARTESIAN_POINT ( 'NONE',  ( 195.9349871089815167, 291.2776426773277194, -17.14268251872402971 ) ) ;
#39944 = VECTOR ( 'NONE', #94574, 1000.000000000000114 ) ;
#39945 = ORIENTED_EDGE ( 'NONE', *, *, #14466, .T. ) ;
#39946 = CARTESIAN_POINT ( 'NONE',  ( 79.93105292411557627, 44.72761662377413927, -11.22918178349264551 ) ) ;
#39947 = CARTESIAN_POINT ( 'NONE',  ( -28.78056054657192320, 23.66266410781089391, -10.00000000000000000 ) ) ;
#39949 = B_SPLINE_SURFACE_WITH_KNOTS ( 'NONE', 3, 1, ( 
 ( #69500, #92838 ),
 ( #62899, #24406 ),
 ( #23389, #54279 ),
 ( #53301, #6712 ),
 ( #84254, #23894 ),
 ( #78118, #37590 ),
 ( #68502, #45684 ),
 ( #99424, #42096 ),
 ( #72534, #48204 ),
 ( #48721, #87782 ),
 ( #80652, #11230 ),
 ( #71527, #86262 ),
 ( #64913, #17300 ),
 ( #80150, #10217 ),
 ( #9733, #25924 ),
 ( #78622, #47687 ),
 ( #56797, #49219 ),
 ( #55774, #86766 ),
 ( #16801, #79151 ),
 ( #9209, #41084 ),
 ( #71027, #17820 ),
 ( #57295, #40588 ),
 ( #96343, #79653 ),
 ( #26414, #49699 ),
 ( #34025, #72020 ),
 ( #2117, #40082 ),
 ( #32513, #1629 ),
 ( #95858, #2624 ),
 ( #64408, #63405 ),
 ( #65402, #18320 ),
 ( #26910, #18814 ),
 ( #95371, #33001 ),
 ( #10716, #41592 ),
 ( #73028, #33513 ) ),
 .UNSPECIFIED., .T., .F., .F.,
 ( 4, 2, 2, 2, 2, 2, 2, 2, 2, 2, 2, 2, 2, 2, 2, 2, 4 ),
 ( 2, 2 ),
 ( 0.000000000000000000, 0.06250000000000000000, 0.1250000000000000000, 0.1875000000000000000, 0.2500000000000000000, 0.3125000000000000000, 0.3750000000000000000, 0.4375000000000000000, 0.5000000000000000000, 0.5625000000000000000, 0.6250000000000000000, 0.6875000000000000000, 0.7500000000000000000, 0.8125000000000000000, 0.8750000000000000000, 0.9375000000000000000, 1.000000000000000000 ),
 ( 0.000000000000000000, 1.000000000000000000 ),
 .UNSPECIFIED. ) ;
#39948 = DIRECTION ( 'NONE',  ( -1.000000000000000000, -1.804112415015878984E-15, 0.000000000000000000 ) ) ;
#39950 = CARTESIAN_POINT ( 'NONE',  ( 81.25645528111445515, 55.75359181263093689, 16.38715272843555226 ) ) ;
#39951 = CARTESIAN_POINT ( 'NONE',  ( 78.69678629884484167, 48.79589717492678602, -14.33111529692661890 ) ) ;
#39952 = CARTESIAN_POINT ( 'NONE',  ( 162.4702972292363086, 249.2401858085828508, 11.41296778546566060 ) ) ;
#39953 = CARTESIAN_POINT ( 'NONE',  ( 79.95842099707557793, 204.7202760586659167, -5.415160957724236172E-17 ) ) ;
#39954 = ORIENTED_EDGE ( 'NONE', *, *, #29657, .F. ) ;
#39955 = CIRCLE ( 'NONE', #67439, 70.00000000000001421 ) ;
#39956 = VERTEX_POINT ( 'NONE', #78889 ) ;
#39957 = CARTESIAN_POINT ( 'NONE',  ( 124.1108878986028543, 230.9155109091896065, 2.679491924311254714 ) ) ;
#39958 = CARTESIAN_POINT ( 'NONE',  ( 200.3443106254163411, 283.6404703198547850, -17.85865425939682538 ) ) ;
#39959 = ORIENTED_EDGE ( 'NONE', *, *, #45700, .T. ) ;
#39960 = EDGE_CURVE ( 'NONE', #91080, #54771, #48974, .T. ) ;
#39961 = CARTESIAN_POINT ( 'NONE',  ( 44.85937643310610667, 116.8208962945185050, 10.00000000000000000 ) ) ;
#39962 = CARTESIAN_POINT ( 'NONE',  ( 161.7013249288979182, 284.4161495234801009, 0.5351470228536304719 ) ) ;
#39963 = CARTESIAN_POINT ( 'NONE',  ( 183.8183646926467816, 261.3479267577503720, -11.63888974307716495 ) ) ;
#39964 = CARTESIAN_POINT ( 'NONE',  ( 87.58565344165421607, 44.63638434534234278, 4.979176973005301932 ) ) ;
#39965 = ORIENTED_EDGE ( 'NONE', *, *, #70963, .F. ) ;
#39966 = CIRCLE ( 'NONE', #48083, 0.1418229129680863287 ) ;
#39967 = CARTESIAN_POINT ( 'NONE',  ( 188.6809246227683445, 295.1128069315126368, 11.75850413834363550 ) ) ;
#39968 = CARTESIAN_POINT ( 'NONE',  ( 184.8538874427280518, 260.0470281449409526, 6.326053503214689400 ) ) ;
#39969 = CARTESIAN_POINT ( 'NONE',  ( 206.8775514429320026, 272.3245652858344670, -9.838455694836268250 ) ) ;
#39970 = CARTESIAN_POINT ( 'NONE',  ( 191.3077102587145646, 274.7514833773715850, 16.90660339326615969 ) ) ;
#39972 = ADVANCED_FACE ( 'NONE', ( #9981 ), #3871, .F. ) ;
#39971 = CARTESIAN_POINT ( 'NONE',  ( 71.70607908956505128, 59.57266618253179757, -15.70866010994346595 ) ) ;
#39973 = CARTESIAN_POINT ( 'NONE',  ( 198.7408816115379864, 285.9624092822338071, -17.04496721243561197 ) ) ;
#39974 = ADVANCED_FACE ( 'NONE', ( #96112 ), #56560, .F. ) ;
#39975 = LINE ( 'NONE', #33399, #48589 ) ;
#39976 = VERTEX_POINT ( 'NONE', #65655 ) ;
#39977 = CARTESIAN_POINT ( 'NONE',  ( 203.5562810614256364, 277.6620430705328317, -14.30492976707583708 ) ) ;
#39978 = CARTESIAN_POINT ( 'NONE',  ( 200.8769374536528858, 282.7179335918746688, 17.26928237494566787 ) ) ;
#39979 = AXIS2_PLACEMENT_3D ( 'NONE', #57219, #59073, #71950 ) ;
#39980 = CARTESIAN_POINT ( 'NONE',  ( 79.14312167556931854, 57.64441083166269664, 0.000000000000000000 ) ) ;
#39981 = CARTESIAN_POINT ( 'NONE',  ( 171.5357040741050980, 251.2175910118344859, 7.330095994321424335 ) ) ;
#39982 = CARTESIAN_POINT ( 'NONE',  ( 84.06109941699628507, 51.61974178474097386, 14.72645736870185651 ) ) ;
#39983 = CARTESIAN_POINT ( 'NONE',  ( 156.4350627803543148, 272.1488426913780927, 14.19226130382477358 ) ) ;
#39984 = VERTEX_POINT ( 'NONE', #96613 ) ;
#39985 = CARTESIAN_POINT ( 'NONE',  ( -14.20026547392215477, 102.9308592454766966, 44.15637032012459429 ) ) ;
#39986 = CARTESIAN_POINT ( 'NONE',  ( 164.9971748156432056, 244.8635054444190757, -1.825016704039769788 ) ) ;
#39987 = CARTESIAN_POINT ( 'NONE',  ( 73.65144064479261488, 55.37666558215569523, 16.11406811069710443 ) ) ;
#39988 = CARTESIAN_POINT ( 'NONE',  ( 176.0413199817918724, 285.4093408875521618, -13.23764318957976371 ) ) ;
#39989 = CARTESIAN_POINT ( 'NONE',  ( 33.73794667537109149, 19.28848085856232686, 1.475505719884397138E-15 ) ) ;
#39990 = B_SPLINE_CURVE_WITH_KNOTS ( 'NONE', 3,
 ( #20634, #30589, #43909, #78195, #61475, #92423, #22973, #84823, #36311, #51519 ),
 .UNSPECIFIED., .F., .F.,
 ( 4, 2, 2, 2, 4 ),
 ( 0.000000000000000000, 0.2500000000000000000, 0.5000000000000000000, 0.7500000000000000000, 1.000000000000000000 ),
 .UNSPECIFIED. ) ;
#39991 = CARTESIAN_POINT ( 'NONE',  ( 172.0067041090704549, 274.8475428133772311, 16.34631960249475569 ) ) ;
#39992 = CARTESIAN_POINT ( 'NONE',  ( 163.1007186844803982, 284.1234281835157276, -3.987921137952420647 ) ) ;
#39993 = CARTESIAN_POINT ( 'NONE',  ( -11.40312891409031693, 78.77562236714182120, 59.97499999999998721 ) ) ;
#39994 = CARTESIAN_POINT ( 'NONE',  ( 8.106622824862185439, 30.17147933776455204, 10.00000000000000000 ) ) ;
#39995 = CARTESIAN_POINT ( 'NONE',  ( 195.3642010211272861, 265.2768603898356332, -7.559402155732556139 ) ) ;
#39996 = EDGE_CURVE ( 'NONE', #9356, #96111, #64677, .T. ) ;
#39997 = CARTESIAN_POINT ( 'NONE',  ( -1.069254392388470976, 164.0643266524160140, 9.188101187500095079 ) ) ;
#39998 = CARTESIAN_POINT ( 'NONE',  ( 41.85954357502990320, 126.4744881464662001, -10.00000000000000000 ) ) ;
#39999 = EDGE_LOOP ( 'NONE', ( #39425, #73606, #28167, #18300 ) ) ;
#40000 = CARTESIAN_POINT ( 'NONE',  ( 174.9585859693524696, 255.2860589088032839, 8.263831412499913043 ) ) ;
#40001 = EDGE_CURVE ( 'NONE', #51335, #86428, #72804, .T. ) ;
#40002 = LINE ( 'NONE', #25321, #45110 ) ;
#40003 = CARTESIAN_POINT ( 'NONE',  ( 81.87492437171775350, 41.18014386121605241, 5.628296993625497180 ) ) ;
#40004 = CARTESIAN_POINT ( 'NONE',  ( 17.98295739510416524, 187.3149278399160949, -9.188101187500095079 ) ) ;
#40005 = AXIS2_PLACEMENT_3D ( 'NONE', #66898, #6606, #82662 ) ;
#40006 = DIRECTION ( 'NONE',  ( -0.8660254037844379305, -0.5000000000000014433, -0.000000000000000000 ) ) ;
#40007 = CARTESIAN_POINT ( 'NONE',  ( 34.04375301561599798, 21.78380873178788946, -6.180339887498949025 ) ) ;
#40008 = CARTESIAN_POINT ( 'NONE',  ( 191.6517533181996100, 265.3842329497505261, -11.14382704138352054 ) ) ;
#40009 = CARTESIAN_POINT ( 'NONE',  ( 191.6723191112861855, 298.6608002251342100, -9.737039817265848995 ) ) ;
#40010 = VECTOR ( 'NONE', #82829, 1000.000000000000000 ) ;
#40011 = CARTESIAN_POINT ( 'NONE',  ( 81.68759648889933089, 55.58869686435339474, 15.96161034574013904 ) ) ;
#40012 = CARTESIAN_POINT ( 'NONE',  ( 172.1631122144370920, 275.2657131827085664, -17.28304708590200889 ) ) ;
#40013 = B_SPLINE_CURVE_WITH_KNOTS ( 'NONE', 3,
 ( #32574, #16863, #39141, #1179, #93915, #31553, #55836, #25467, #72086, #24959, #54861, #81573, #86832, #86326, #85840, #17364 ),
 .UNSPECIFIED., .F., .F.,
 ( 4, 2, 2, 2, 2, 2, 2, 4 ),
 ( 8.156114889773229926E-15, 0.0005317649415277559332, 0.0007976474122876054925, 0.001063529883047454943, 0.001329412353807304719, 0.001595294824567154062, 0.001861177295327003838, 0.002127059766086853397 ),
 .UNSPECIFIED. ) ;
#40014 = ADVANCED_FACE ( 'NONE', ( #87033 ), #1876, .F. ) ;
#40015 = CARTESIAN_POINT ( 'NONE',  ( 86.98925081226386169, 46.40596221211884398, -8.809588356812493970 ) ) ;
#40016 = CARTESIAN_POINT ( 'NONE',  ( 198.0355408163131585, 287.6393769322024241, 18.20720360189982756 ) ) ;
#40017 = CARTESIAN_POINT ( 'NONE',  ( 69.37632600059342280, 210.8615022471902591, -10.00000000000009592 ) ) ;
#40018 = PLANE ( 'NONE',  #97603 ) ;
#40019 = CARTESIAN_POINT ( 'NONE',  ( -19.65312891409030271, 93.06504152958497400, 10.00000000000000888 ) ) ;
#40020 = CARTESIAN_POINT ( 'NONE',  ( 206.3531636607249879, 271.3592212809042508, 6.161143238982110582 ) ) ;
#40021 = CARTESIAN_POINT ( 'NONE',  ( 28.05084980986327281, 180.8768266524160140, -9.188101187500091527 ) ) ;
#40022 = CARTESIAN_POINT ( 'NONE',  ( 159.2554912534056939, 254.8083930951974878, 16.49944922174842432 ) ) ;
#40023 = CARTESIAN_POINT ( 'NONE',  ( -4.653128914090328472, 79.21777907560398546, 13.72050197239993707 ) ) ;
#40024 = CARTESIAN_POINT ( 'NONE',  ( 198.9369963555428740, 286.0780101374919013, -18.58432392708837710 ) ) ;
#40025 = CARTESIAN_POINT ( 'NONE',  ( -19.65312891409030271, 93.06504152958497400, 59.99999999999999289 ) ) ;
#40026 = ORIENTED_EDGE ( 'NONE', *, *, #61393, .T. ) ;
#40027 = AXIS2_PLACEMENT_3D ( 'NONE', #48556, #87628, #41944 ) ;
#40028 = CARTESIAN_POINT ( 'NONE',  ( 78.13225151398272317, 227.4637435831425023, 2.679491924311251605 ) ) ;
#40029 = CARTESIAN_POINT ( 'NONE',  ( 167.6278246310154714, 282.5728663012718584, -12.21306354836790220 ) ) ;
#40030 = CARTESIAN_POINT ( 'NONE',  ( 163.1717563955264438, 281.1342508170415613, -10.22479631152172352 ) ) ;
#40031 = CARTESIAN_POINT ( 'NONE',  ( -13.11024591527734628, 6.000000000000000000, -45.00000000000000000 ) ) ;
#40032 = CARTESIAN_POINT ( 'NONE',  ( 22.39139443204644664, 24.87878583063842086, -9.188101187500006262 ) ) ;
#40033 = CARTESIAN_POINT ( 'NONE',  ( 202.9216520459657147, 279.1763840310111391, 15.75371595331685803 ) ) ;
#40034 = CARTESIAN_POINT ( 'NONE',  ( 111.1205068418362742, 223.4155109091896065, 2.679491924311254714 ) ) ;
#40035 = CARTESIAN_POINT ( 'NONE',  ( 185.5354357917608752, 267.5855751454028564, -14.72482343138568339 ) ) ;
#40036 = EDGE_LOOP ( 'NONE', ( #27547, #89212, #66831, #27064 ) ) ;
#40037 = CARTESIAN_POINT ( 'NONE',  ( 36.54023192077972482, 39.83478043621391151, -8.090169943749479842 ) ) ;
#40038 = CARTESIAN_POINT ( 'NONE',  ( 12.18311320154372801, 9.960047579820882291, -5.678558825948275768 ) ) ;
#40039 = CARTESIAN_POINT ( 'NONE',  ( 72.76330120127171597, 59.97484020424936091, -15.29220549501611259 ) ) ;
#40040 = CARTESIAN_POINT ( 'NONE',  ( 71.94509386275791485, 72.64380087153907084, -0.7818115889975479904 ) ) ;
#40041 = ORIENTED_EDGE ( 'NONE', *, *, #68385, .T. ) ;
#40042 = CARTESIAN_POINT ( 'NONE',  ( 185.1775619574503366, 280.9945881611855043, 17.59732015342263267 ) ) ;
#40043 = CARTESIAN_POINT ( 'NONE',  ( 71.68256357803392120, 71.39422369264570989, -4.342351502620559245 ) ) ;
#40045 = CARTESIAN_POINT ( 'NONE',  ( 151.3284628043366524, 268.5384091220288383, 14.49047510809488237 ) ) ;
#40044 = B_SPLINE_CURVE_WITH_KNOTS ( 'NONE', 3,
 ( #95340, #18292, #78087, #55743 ),
 .UNSPECIFIED., .F., .F.,
 ( 4, 4 ),
 ( 0.008346957882847750101, 0.01470164726671086691 ),
 .UNSPECIFIED. ) ;
#40046 = CARTESIAN_POINT ( 'NONE',  ( 181.0230527394317619, 257.6990957149607198, -7.502503115033712255 ) ) ;
#40047 = EDGE_LOOP ( 'NONE', ( #73119, #10195, #60156, #97295 ) ) ;
#40048 = CIRCLE ( 'NONE', #7745, 70.00000000000001421 ) ;
#40050 = CARTESIAN_POINT ( 'NONE',  ( 81.70142411701870344, 42.24897359289763443, -6.860144861392842408 ) ) ;
#40049 = CARTESIAN_POINT ( 'NONE',  ( 207.8575108622103755, 270.6272257822888037, -6.381720258959569847 ) ) ;
#40051 = ORIENTED_EDGE ( 'NONE', *, *, #60560, .T. ) ;
#40052 = CARTESIAN_POINT ( 'NONE',  ( 200.7134601498536028, 283.0010845879393742, -16.98649239173277792 ) ) ;
#40053 = CARTESIAN_POINT ( 'NONE',  ( -19.65312891409030271, 93.06504152958497400, 177.5919119679930134 ) ) ;
#40054 = CARTESIAN_POINT ( 'NONE',  ( 72.80354425691618303, 56.98564078552313106, -16.40249550304353221 ) ) ;
#40055 = DIRECTION ( 'NONE',  ( 1.000000000000000000, 0.000000000000000000, 0.000000000000000000 ) ) ;
#40056 = EDGE_CURVE ( 'NONE', #21527, #91318, #49461, .T. ) ;
#40057 = CARTESIAN_POINT ( 'NONE',  ( 189.9052851100924215, 301.7213928939034986, -1.077181946533001256 ) ) ;
#40058 = CARTESIAN_POINT ( 'NONE',  ( 91.43256340568937901, 235.8464784336661637, 1.353441290958777525E-15 ) ) ;
#40059 = B_SPLINE_CURVE_WITH_KNOTS ( 'NONE', 3,
 ( #50821, #87911, #11852, #89395, #89869, #19946 ),
 .UNSPECIFIED., .F., .F.,
 ( 4, 2, 4 ),
 ( 0.01904094441108342833, 0.02356434879539306276, 0.02808775317970270066 ),
 .UNSPECIFIED. ) ;
#40060 = CARTESIAN_POINT ( 'NONE',  ( 203.3286960320409094, 267.8359400968079171, 2.569349860321338941 ) ) ;
#40061 = EDGE_LOOP ( 'NONE', ( #15046, #56942, #10300, #73856 ) ) ;
#40062 = CARTESIAN_POINT ( 'NONE',  ( 161.8637969276452679, 267.0824340876292240, 16.50456879414842959 ) ) ;
#40063 = VERTEX_POINT ( 'NONE', #25157 ) ;
#40064 = CARTESIAN_POINT ( 'NONE',  ( 31.32709252658613508, 23.80170272979928114, 7.433330006724137462 ) ) ;
#40065 = CARTESIAN_POINT ( 'NONE',  ( 197.9952413503812352, 287.7091776547143809, 17.17611241386010690 ) ) ;
#40066 = CARTESIAN_POINT ( 'NONE',  ( 68.42576582225177617, 70.23325100905495333, -3.401356179981240402 ) ) ;
#40067 = CARTESIAN_POINT ( 'NONE',  ( 52.94873307290090025, 207.5024278399160949, 9.188101187500095079 ) ) ;
#40068 = CARTESIAN_POINT ( 'NONE',  ( 74.04232911944542650, 68.62205345152153768, 10.92009053252770734 ) ) ;
#40069 = CARTESIAN_POINT ( 'NONE',  ( 160.7489855951974675, 254.2215850144021658, 15.85577744295692248 ) ) ;
#40070 = CARTESIAN_POINT ( 'NONE',  ( 198.0384979254556015, 287.6342550689238351, 17.28192639992792579 ) ) ;
#40071 = CARTESIAN_POINT ( 'NONE',  ( 176.4670716382853470, 273.1881962802569319, 17.38719208580632269 ) ) ;
#40072 = ORIENTED_EDGE ( 'NONE', *, *, #83049, .T. ) ;
#40073 = DIRECTION ( 'NONE',  ( -0.8660254037844387076, -0.4999999999999998890, -0.000000000000000000 ) ) ;
#40074 = CARTESIAN_POINT ( 'NONE',  ( 190.2648877593310317, 301.0985428348857340, -4.426259207433023590 ) ) ;
#40075 = CARTESIAN_POINT ( 'NONE',  ( 147.6618183892331331, 274.8892235422768522, 8.990680574201936892 ) ) ;
#40076 = AXIS2_PLACEMENT_3D ( 'NONE', #8272, #62961, #33574 ) ;
#40077 = ORIENTED_EDGE ( 'NONE', *, *, #99481, .T. ) ;
#40078 = CARTESIAN_POINT ( 'NONE',  ( 175.4521479476684647, 261.2799168608980267, -14.40428220072110932 ) ) ;
#40079 = CARTESIAN_POINT ( 'NONE',  ( 170.6367097137389806, 275.3559257912166345, -16.50175916787543784 ) ) ;
#40080 = CARTESIAN_POINT ( 'NONE',  ( 207.5462191418491500, 271.1663988579299485, -5.239401497773396699 ) ) ;
#40081 = CARTESIAN_POINT ( 'NONE',  ( 147.3236643320416022, 275.4749235501183193, -5.185334239426818037 ) ) ;
#40082 = CARTESIAN_POINT ( 'NONE',  ( 149.2561433752359505, 272.1277716627430436, 12.99353668144589946 ) ) ;
#40083 = VECTOR ( 'NONE', #67291, 1000.000000000000114 ) ;
#40084 = CARTESIAN_POINT ( 'NONE',  ( 179.7440261010970062, 270.5841209280236512, 17.43403005247386517 ) ) ;
#40085 = DIRECTION ( 'NONE',  ( 0.4999999999999998890, -0.8660254037844385966, 0.000000000000000000 ) ) ;
#40086 = CARTESIAN_POINT ( 'NONE',  ( 76.00671579873834105, 65.53670222276893753, 13.92362488849856739 ) ) ;
#40087 = CARTESIAN_POINT ( 'NONE',  ( 154.6934824199911702, 264.1949505326113581, -17.20522734258247866 ) ) ;
#40088 = CARTESIAN_POINT ( 'NONE',  ( 207.5583741822599393, 271.1453457103705205, 3.140867606700001424 ) ) ;
#40089 = VECTOR ( 'NONE', #72363, 1000.000000000000227 ) ;
#40090 = CARTESIAN_POINT ( 'NONE',  ( 109.6190968851625911, 246.3464784336661353, 1.353441290958777327E-15 ) ) ;
#40091 = EDGE_LOOP ( 'NONE', ( #33249, #8111, #32350, #53130 ) ) ;
#40092 = CARTESIAN_POINT ( 'NONE',  ( 149.0458102676470560, 272.4920792916013284, -12.77276851155236059 ) ) ;
#40093 = CARTESIAN_POINT ( 'NONE',  ( 84.17777703092687602, 41.88998738275029154, -0.4096941387594014161 ) ) ;
#40094 = CARTESIAN_POINT ( 'NONE',  ( 155.5587153255869453, 261.2113968263770971, -18.30500480654006878 ) ) ;
#40095 = EDGE_CURVE ( 'NONE', #100032, #947, #43810, .T. ) ;
#40096 = CARTESIAN_POINT ( 'NONE',  ( 163.8040269124969939, 246.9300982336122559, 6.025552750865228013 ) ) ;
#40097 = ADVANCED_FACE ( 'NONE', ( #43348 ), #21085, .F. ) ;
#40098 = CARTESIAN_POINT ( 'NONE',  ( 83.65902391768069890, 51.64235791857056768, -14.83937710116058639 ) ) ;
#40099 = CARTESIAN_POINT ( 'NONE',  ( 176.2336582595617358, 254.2209709748362627, 4.925071008084640489 ) ) ;
#40100 = EDGE_LOOP ( 'NONE', ( #70538, #60427, #59860, #45831 ) ) ;
#40101 = CARTESIAN_POINT ( 'NONE',  ( 162.7738416911812180, 248.7144313781379310, -11.09964294874192525 ) ) ;
#40102 = MECHANICAL_DESIGN_GEOMETRIC_PRESENTATION_REPRESENTATION (  '', ( #85513 ), #96784 ) ;
#40103 =( BOUNDED_CURVE ( )  B_SPLINE_CURVE ( 2, ( #25633, #8920, #78842, #819, #31695, #9425, #40300, #71242, #63618, #79374, #62603, #9937, #2338 ),
 .UNSPECIFIED., .F., .T. ) 
 B_SPLINE_CURVE_WITH_KNOTS ( ( 3, 2, 2, 2, 2, 2, 3 ),
 ( 0.4625000000000000222, 0.4650000000000000244, 0.4699999999999999734, 0.4749999999999999778, 0.4799999999999999822, 0.4849999999999999867, 0.4874999999999999889 ),
 .UNSPECIFIED. ) 
 CURVE ( )  GEOMETRIC_REPRESENTATION_ITEM ( )  RATIONAL_B_SPLINE_CURVE ( ( 0.9755282581475768211, 0.9755282581475768211, 1.000000000000000000, 0.9510565162951535312, 1.000000000000000000, 0.9510565162951535312, 1.000000000000000000, 0.9510565162951535312, 1.000000000000000000, 0.9510565162951535312, 1.000000000000000000, 0.9755282581475768211, 0.9755282581475768211 ) ) 
 REPRESENTATION_ITEM ( '' )  );
#40104 = CARTESIAN_POINT ( 'NONE',  ( 156.1631927981498222, 273.8066032555324796, -12.73205779767400969 ) ) ;
#40105 = CARTESIAN_POINT ( 'NONE',  ( 184.2589036364679771, 261.5973822520062413, 9.577938735879747867 ) ) ;
#40106 = CARTESIAN_POINT ( 'NONE',  ( 206.2410742340367165, 271.7831106908868719, 8.101945950764607218 ) ) ;
#40107 = CARTESIAN_POINT ( 'NONE',  ( 137.1700506867025808, 243.8768266524160140, -9.188101187500093303 ) ) ;
#40108 = CARTESIAN_POINT ( 'NONE',  ( 198.6894790592683080, 286.5067226703918095, -17.06774375037124614 ) ) ;
#40109 = AXIS2_PLACEMENT_3D ( 'NONE', #67348, #4058, #74975 ) ;
#40110 = LINE ( 'NONE', #16327, #82100 ) ;
#40111 = CARTESIAN_POINT ( 'NONE',  ( 196.4351339088274813, 290.4113630087520050, 17.20526457544535504 ) ) ;
#40112 = DIRECTION ( 'NONE',  ( 1.000000000000000000, 0.000000000000000000, 0.000000000000000000 ) ) ;
#40113 = CARTESIAN_POINT ( 'NONE',  ( 49.94514132322986910, 190.4548013555409796, -4.594050593750042211 ) ) ;
#40114 = CARTESIAN_POINT ( 'NONE',  ( 75.19165711449073797, 61.00119534238836394, -15.88670729749929578 ) ) ;
#40115 = CARTESIAN_POINT ( 'NONE',  ( 87.93887446415499198, 44.76116579897428238, -4.704258403839747693 ) ) ;
#40116 =( NAMED_UNIT ( * ) SI_UNIT ( $, .STERADIAN. ) SOLID_ANGLE_UNIT ( ) );
#40117 = CARTESIAN_POINT ( 'NONE',  ( 171.3314046892768090, 260.1076107119635026, 14.81378772054287474 ) ) ;
#40118 = CARTESIAN_POINT ( 'NONE',  ( 38.12092316966794669, 88.62496094012092840, 59.99999999999999289 ) ) ;
#40119 = CARTESIAN_POINT ( 'NONE',  ( 178.8916920429171000, 291.7792318689755007, -6.177336454205645033 ) ) ;
#40120 = DIRECTION ( 'NONE',  ( 0.000000000000000000, 0.000000000000000000, 1.000000000000000000 ) ) ;
#40121 = CARTESIAN_POINT ( 'NONE',  ( 9.004826742577897392, 187.5530062829863027, -4.648177544792955347E-16 ) ) ;
#40122 = CIRCLE ( 'NONE', #51490, 70.00000000000001421 ) ;
#40123 = EDGE_CURVE ( 'NONE', #62531, #22014, #66161, .T. ) ;
#40124 = CARTESIAN_POINT ( 'NONE',  ( 112.8760603413013399, 242.6427522451419350, 10.00000000000009237 ) ) ;
#40125 = DIRECTION ( 'NONE',  ( -0.3105719460338542404, -0.9505498757754611283, 0.000000000000000000 ) ) ;
#40126 = ORIENTED_EDGE ( 'NONE', *, *, #90573, .F. ) ;
#40127 = CARTESIAN_POINT ( 'NONE',  ( 202.3139361598622372, 280.2289788223093865, 15.93832709035092421 ) ) ;
#40128 = CARTESIAN_POINT ( 'NONE',  ( 87.94090206498698592, 44.79893454962108734, 4.853345500095875842 ) ) ;
#40129 = CARTESIAN_POINT ( 'NONE',  ( 19.79611131033658111, 191.4244531367911293, -4.594050593750046652 ) ) ;
#40130 = CARTESIAN_POINT ( 'NONE',  ( 10.48369258086752787, 24.79103043416547791, 8.090169943749478065 ) ) ;
#40131 = CARTESIAN_POINT ( 'NONE',  ( 81.77131458871032521, 208.0177522451417929, 5.000000000000051514 ) ) ;
#40132 = CARTESIAN_POINT ( 'NONE',  ( 30.68386671255119325, 44.42157463747831514, 177.5919119679930134 ) ) ;
#40133 = CARTESIAN_POINT ( 'NONE',  ( 27.58098951138967436, 43.10352854649765675, 10.00000000000000000 ) ) ;
#40135 = CARTESIAN_POINT ( 'NONE',  ( 52.32645086003936541, 201.0177522451418497, -10.00000000000009592 ) ) ;
#40134 = CARTESIAN_POINT ( 'NONE',  ( 198.1230357675706557, 277.7030879543556239, -15.67994595731362217 ) ) ;
#40136 = CARTESIAN_POINT ( 'NONE',  ( 172.8524532584847861, 287.5566872288061404, 7.496887191024062425 ) ) ;
#40137 = CARTESIAN_POINT ( 'NONE',  ( 184.7866525864025107, 257.7151715236021232, 1.373357544146073250 ) ) ;
#40138 = CARTESIAN_POINT ( 'NONE',  ( 205.2941531242069857, 275.0670916224857478, -13.92605142593109058 ) ) ;
#40139 = CARTESIAN_POINT ( 'NONE',  ( 13.32519098795206780, 19.64441083166259361, -10.00000000000000533 ) ) ;
#40140 = EDGE_LOOP ( 'NONE', ( #64659, #20984, #7063, #2318 ) ) ;
#40141 = CARTESIAN_POINT ( 'NONE',  ( 161.5791065876047128, 267.6385769225021249, 16.61089899141252246 ) ) ;
#40142 = CARTESIAN_POINT ( 'NONE',  ( 32.93109025799834200, 176.4865022471901455, 1.119607411625061291E-15 ) ) ;
#40143 = CARTESIAN_POINT ( 'NONE',  ( 150.1604317434691325, 251.3768266524160140, -9.188101187500091527 ) ) ;
#40144 = CARTESIAN_POINT ( 'NONE',  ( 202.5511585997265911, 279.8180975037686835, 17.12781264818056925 ) ) ;
#40145 = VECTOR ( 'NONE', #76614, 1000.000000000000000 ) ;
#40146 = CARTESIAN_POINT ( 'NONE',  ( -8.322217149083147802, 159.8768266524159856, -9.188101187500091527 ) ) ;
#40147 = CARTESIAN_POINT ( 'NONE',  ( 37.97865540203802937, 30.43085787977766188, -9.188101187500008038 ) ) ;
#40149 = CARTESIAN_POINT ( 'NONE',  ( 170.2387432371133684, 263.6005831635989125, 15.83122915802868214 ) ) ;
#40148 = CARTESIAN_POINT ( 'NONE',  ( 45.88188149789386472, 72.29567966924398092, -10.00000000000000000 ) ) ;
#40150 = CARTESIAN_POINT ( 'NONE',  ( 188.3259911839309098, 288.6587601801259098, -15.98176789963882349 ) ) ;
#40151 = CARTESIAN_POINT ( 'NONE',  ( 206.4943150373521803, 272.9883502116088039, 11.34100825923693101 ) ) ;
#40153 = VECTOR ( 'NONE', #50135, 1000.000000000000227 ) ;
#40152 = CARTESIAN_POINT ( 'NONE',  ( 186.2095639655686341, 259.2069574296129417, -2.346516652132980774 ) ) ;
#40154 = CARTESIAN_POINT ( 'NONE',  ( 66.08354252224813763, 69.04860372161006410, 2.576220482760897212 ) ) ;
#40155 = ORIENTED_EDGE ( 'NONE', *, *, #11542, .F. ) ;
#40156 = CARTESIAN_POINT ( 'NONE',  ( -115.0954152546897973, 78.37593066204027537, 37.50000000000002132 ) ) ;
#40157 = EDGE_CURVE ( 'NONE', #90906, #30881, #6319, .T. ) ;
#40158 = CARTESIAN_POINT ( 'NONE',  ( 180.3366176027714971, 286.6329442896284263, 13.14786923958608966 ) ) ;
#40159 = CARTESIAN_POINT ( 'NONE',  ( 153.2950423568359781, 277.6701191893376972, -5.326679232739844672 ) ) ;
#40160 = CARTESIAN_POINT ( 'NONE',  ( 6.852252633650415703, 22.14336893147753571, 7.433330006724141015 ) ) ;
#40161 = CARTESIAN_POINT ( 'NONE',  ( 160.5941949179546384, 252.4896903319198600, 14.95613949087054628 ) ) ;
#40162 = VECTOR ( 'NONE', #59887, 1000.000000000000114 ) ;
#40163 = CARTESIAN_POINT ( 'NONE',  ( 206.5081929095101998, 272.9643130319303737, -9.215516226794479238 ) ) ;
#40164 = CARTESIAN_POINT ( 'NONE',  ( 192.0963028965829551, 297.9264387674147656, 11.34530024772836754 ) ) ;
#40165 = DIRECTION ( 'NONE',  ( 0.4972609476841349796, -0.8612812260087746585, 0.1045284632676570652 ) ) ;
#40166 = CARTESIAN_POINT ( 'NONE',  ( 66.10228174246465471, 68.64626758112467542, 4.271897712866680408 ) ) ;
#40167 = CARTESIAN_POINT ( 'NONE',  ( 87.90004739103230236, 45.00901072816738235, 6.408389154966701362 ) ) ;
#40168 = CARTESIAN_POINT ( 'NONE',  ( 193.7118145980225279, 295.1282904202991517, 14.61271143546694162 ) ) ;
#40169 = ORIENTED_EDGE ( 'NONE', *, *, #93761, .F. ) ;
#40170 = CIRCLE ( 'NONE', #49965, 70.00000000000001421 ) ;
#40171 = EDGE_LOOP ( 'NONE', ( #49087, #92573, #77996, #26655 ) ) ;
#40172 = CARTESIAN_POINT ( 'NONE',  ( 136.9984762794283881, 243.2365022471901739, -10.00000000000009237 ) ) ;
#40173 = CARTESIAN_POINT ( 'NONE',  ( 85.87397059692905543, 47.49916506119975423, 10.81363086110046190 ) ) ;
#40174 = EDGE_LOOP ( 'NONE', ( #55988, #97573, #83478, #19764 ) ) ;
#40175 = CARTESIAN_POINT ( 'NONE',  ( 25.97889144642132919, 17.12755873383626692, -6.180339887498949025 ) ) ;
#40176 = CARTESIAN_POINT ( 'NONE',  ( 199.9502294570856407, 265.6703872523112295, 6.360370400932541246E-13 ) ) ;
#40177 = ORIENTED_EDGE ( 'NONE', *, *, #39513, .F. ) ;
#40178 = CARTESIAN_POINT ( 'NONE',  ( 191.0702043019150835, 299.7036936669546776, -8.800021049343948576 ) ) ;
#40179 = FACE_OUTER_BOUND ( 'NONE', #81970, .T. ) ;
#40180 = CARTESIAN_POINT ( 'NONE',  ( 19.03539854152464628, 16.15404122711133184, 8.090169943749479842 ) ) ;
#40181 = ORIENTED_EDGE ( 'NONE', *, *, #45697, .T. ) ;
#40182 = CARTESIAN_POINT ( 'NONE',  ( -19.65312891409030271, 93.06504152958497400, 10.00000000000000888 ) ) ;
#40183 = DIRECTION ( 'NONE',  ( -0.000000000000000000, -0.000000000000000000, -1.000000000000000000 ) ) ;
#40184 = CARTESIAN_POINT ( 'NONE',  ( 190.8094645593471341, 300.1553081486349015, 8.399847186519689757 ) ) ;
#40185 = CARTESIAN_POINT ( 'NONE',  ( -19.65312891409030271, 93.06504152958497400, 10.00000000000000888 ) ) ;
#40186 = B_SPLINE_SURFACE_WITH_KNOTS ( 'NONE', 3, 1, ( 
 ( #8256, #17341 ),
 ( #46222, #38639 ),
 ( #85292, #1157 ),
 ( #77144, #62423 ),
 ( #61927, #39120 ),
 ( #92879, #48249 ),
 ( #32031, #62941 ),
 ( #24448, #23433 ),
 ( #9255, #54320 ),
 ( #80696, #11271 ),
 ( #41631, #18359 ),
 ( #3663, #50725 ),
 ( #3179, #65934 ),
 ( #34541, #26947 ),
 ( #19859, #42134 ),
 ( #42623, #81681 ),
 ( #96888, #73065 ),
 ( #17863, #11759 ),
 ( #88811, #80189 ),
 ( #57831, #27458 ),
 ( #19377, #63942 ),
 ( #40630, #65439 ),
 ( #72573, #56333 ),
 ( #71566, #96384 ),
 ( #87331, #25965 ),
 ( #73552, #58329 ),
 ( #48761, #50236 ),
 ( #94879, #49252 ),
 ( #2162, #34064 ),
 ( #81191, #35030 ),
 ( #89304, #57334 ),
 ( #33043, #25443 ),
 ( #79694, #41125 ),
 ( #4136, #64955 ) ),
 .UNSPECIFIED., .T., .F., .F.,
 ( 4, 2, 2, 2, 2, 2, 2, 2, 2, 2, 2, 2, 2, 2, 2, 2, 4 ),
 ( 2, 2 ),
 ( 0.000000000000000000, 0.06250000000000000000, 0.1250000000000000000, 0.1875000000000000000, 0.2500000000000000000, 0.3125000000000000000, 0.3750000000000000000, 0.4375000000000000000, 0.5000000000000000000, 0.5625000000000000000, 0.6250000000000000000, 0.6875000000000000000, 0.7500000000000000000, 0.8125000000000000000, 0.8750000000000000000, 0.9375000000000000000, 1.000000000000000000 ),
 ( 0.000000000000000000, 1.000000000000000000 ),
 .UNSPECIFIED. ) ;
#40187 = ORIENTED_EDGE ( 'NONE', *, *, #9251, .F. ) ;
#40188 = CARTESIAN_POINT ( 'NONE',  ( 195.6968381273587454, 265.0589268724819476, 7.395276693337085483 ) ) ;
#40189 = ORIENTED_EDGE ( 'NONE', *, *, #12103, .T. ) ;
#40190 = EDGE_LOOP ( 'NONE', ( #96307, #14445, #70919, #42498, #89955 ) ) ;
#40191 = CARTESIAN_POINT ( 'NONE',  ( 74.19807589368119238, 65.03689309259050333, 13.58590908905372352 ) ) ;
#40192 = ORIENTED_EDGE ( 'NONE', *, *, #50199, .T. ) ;
#40193 = CARTESIAN_POINT ( 'NONE',  ( 164.0781508658037637, 275.4055464209769752, 15.63836535835214114 ) ) ;
#40194 = ORIENTED_EDGE ( 'NONE', *, *, #32610, .F. ) ;
#40195 = AXIS2_PLACEMENT_3D ( 'NONE', #90277, #58806, #51740 ) ;
#40196 = CARTESIAN_POINT ( 'NONE',  ( 82.47798474638348409, 46.77785881030774107, 11.77598945167534161 ) ) ;
#40197 = CARTESIAN_POINT ( 'NONE',  ( 70.93889008731977697, 68.42943192159272314, 9.010113148257101301 ) ) ;
#40198 = CARTESIAN_POINT ( 'NONE',  ( 194.1789525331299728, 294.3191837825503967, -15.34533909744314961 ) ) ;
#40199 = CARTESIAN_POINT ( 'NONE',  ( -72.48190909937208914, 49.06123820388767598, -10.00000000000000000 ) ) ;
#40200 = CARTESIAN_POINT ( 'NONE',  ( 8.774901663922227257, 164.3262482093457777, 3.021315404115420679E-15 ) ) ;
#40201 = DIRECTION ( 'NONE',  ( -0.7713848165480284846, 0.6363689690731033632, 0.000000000000000000 ) ) ;
#40202 = CARTESIAN_POINT ( 'NONE',  ( 26.13094010387951371, 20.80170272979927049, 7.433330006724137462 ) ) ;
#40203 = CARTESIAN_POINT ( 'NONE',  ( 164.2813349609167517, 246.1033764428878214, 1.949810150281061638 ) ) ;
#40204 = CARTESIAN_POINT ( 'NONE',  ( 110.0000000000000000, 15.00000000000000000, -9.212605237762131694 ) ) ;
#40206 = VERTEX_POINT ( 'NONE', #20575 ) ;
#40205 = DIRECTION ( 'NONE',  ( 0.2702110370271901818, 0.9515975153008194853, 0.1464519181915934776 ) ) ;
#40207 = DIRECTION ( 'NONE',  ( -0.8660254037844379305, -0.5000000000000014433, -0.000000000000000000 ) ) ;
#40208 = FACE_OUTER_BOUND ( 'NONE', #17158, .T. ) ;
#40209 = CARTESIAN_POINT ( 'NONE',  ( 206.6703863510205679, 272.6833857505801006, -10.72500664779635393 ) ) ;
#40210 = DIRECTION ( 'NONE',  ( 0.000000000000000000, 0.000000000000000000, 1.000000000000000000 ) ) ;
#40211 = EDGE_CURVE ( 'NONE', #69571, #6423, #70365, .T. ) ;
#40212 = CARTESIAN_POINT ( 'NONE',  ( 200.4775477985258760, 283.4096967665721536, 16.80647240730505487 ) ) ;
#40213 = ADVANCED_FACE ( 'NONE', ( #37729 ), #61027, .F. ) ;
#40214 = CARTESIAN_POINT ( 'NONE',  ( 71.96330895120250659, 59.12713099295166330, 15.87581820695405455 ) ) ;
#40215 = ORIENTED_EDGE ( 'NONE', *, *, #79460, .F. ) ;
#40216 = CARTESIAN_POINT ( 'NONE',  ( 155.4594742945911321, 261.3832873342573180, -17.01475918255801645 ) ) ;
#40217 = DIRECTION ( 'NONE',  ( 0.4999999999999998890, -0.8660254037844385966, 0.000000000000000000 ) ) ;
#40218 = CARTESIAN_POINT ( 'NONE',  ( 74.92223598134692963, 66.83043205548882781, -13.20899543911387930 ) ) ;
#40219 = ADVANCED_FACE ( 'NONE', ( #53433 ), #99559, .F. ) ;
#40220 = VECTOR ( 'NONE', #37715, 1000.000000000000114 ) ;
#40221 = LINE ( 'NONE', #32132, #83964 ) ;
#40222 = EDGE_CURVE ( 'NONE', #88994, #19414, #38957, .T. ) ;
#40223 = CARTESIAN_POINT ( 'NONE',  ( 20.35567970366385993, 175.8927522451418213, 10.00000000000009592 ) ) ;
#40224 = CARTESIAN_POINT ( 'NONE',  ( 90.56688509766992468, 223.0958772461660260, -9.188101187500095079 ) ) ;
#40225 = DIRECTION ( 'NONE',  ( 0.2091919045418505763, 0.9778746070300391446, 0.000000000000000000 ) ) ;
#40226 = VECTOR ( 'NONE', #31653, 1000.000000000000114 ) ;
#40227 = CARTESIAN_POINT ( 'NONE',  ( 174.5555281753831025, 282.3909387449837709, -14.50095961335927264 ) ) ;
#40228 = CARTESIAN_POINT ( 'NONE',  ( 166.7187202459675746, 278.5591580196478958, -14.78021074750266273 ) ) ;
#40229 = AXIS2_PLACEMENT_3D ( 'NONE', #34361, #2480, #80004 ) ;
#40231 = CARTESIAN_POINT ( 'NONE',  ( 75.59035046094346910, 65.27760725598233194, 14.33377162271303540 ) ) ;
#40230 = CARTESIAN_POINT ( 'NONE',  ( 0.1751364819041374699, 183.1589784336661637, -6.496448406907675876E-16 ) ) ;
#40232 = CARTESIAN_POINT ( 'NONE',  ( 200.4403816905005158, 283.4740703539914648, 16.81798557643505987 ) ) ;
#40233 = VERTEX_POINT ( 'NONE', #244 ) ;
#40234 = VECTOR ( 'NONE', #42900, 1000.000000000000000 ) ;
#40235 = ORIENTED_EDGE ( 'NONE', *, *, #70081, .F. ) ;
#40236 = DIRECTION ( 'NONE',  ( 0.000000000000000000, 0.000000000000000000, 1.000000000000000000 ) ) ;
#40237 = CARTESIAN_POINT ( 'NONE',  ( 197.7056209715021851, 265.0177529662663574, -2.988310547816667828 ) ) ;
#40238 = CARTESIAN_POINT ( 'NONE',  ( 68.74458750670157769, 70.20414421525195792, 1.682888519748420908 ) ) ;
#40239 = FACE_OUTER_BOUND ( 'NONE', #99253, .T. ) ;
#40240 = LINE ( 'NONE', #71182, #39826 ) ;
#40241 = VECTOR ( 'NONE', #9181, 1000.000000000000000 ) ;
#40242 = LINE ( 'NONE', #100083, #91892 ) ;
#40243 = CARTESIAN_POINT ( 'NONE',  ( 74.43781217983632814, 68.33376311026280803, -11.38208125649862801 ) ) ;
#40244 = CARTESIAN_POINT ( 'NONE',  ( 28.70002176693659379, 193.5024278399160949, -9.188101187500093303 ) ) ;
#40245 = CARTESIAN_POINT ( 'NONE',  ( 73.03889176721715160, 219.6427522451419065, -10.00000000000009415 ) ) ;
#40246 = CARTESIAN_POINT ( 'NONE',  ( 199.2997933464620530, 277.4527719018980747, 15.18799710326758579 ) ) ;
#40247 = ORIENTED_EDGE ( 'NONE', *, *, #82211, .F. ) ;
#40248 = CARTESIAN_POINT ( 'NONE',  ( 153.0823121780915983, 273.6142464696663410, -11.82140495845541039 ) ) ;
#40249 = B_SPLINE_CURVE_WITH_KNOTS ( 'NONE', 3,
 ( #68245, #76375, #75377, #75886, #5466, #82997, #36350, #14061, #98686, #5961, #91096, #36852, #6946, #13574, #67761, #21664, #28761, #67253, #84492, #53541, #52544, #69242, #37343, #99169, #98180, #15035, #44444, #29757, #59642, #45927, #90613, #37838, #38334, #60629, #91583, #22157, #53047, #68744, #99667, #30253, #92111, #76844, #7442, #30758, #61636, #92588 ),
 .UNSPECIFIED., .F., .F.,
 ( 4, 2, 2, 2, 2, 2, 2, 2, 2, 2, 2, 2, 2, 2, 2, 2, 2, 2, 2, 2, 2, 2, 4 ),
 ( 0.0004441887608673076183, 0.0008957827227663670705, 0.001121579703715850067, 0.001347376684665332848, 0.001460275175140070443, 0.001573173665614808038, 0.001798970646564274989, 0.002250564608463331839, 0.003153752532261445973, 0.004056940456059559240, 0.004960128379857672506, 0.005411722341756729573, 0.005637519322706221678, 0.005750417813181006761, 0.005806867058418394532, 0.005863316303655782304, 0.005919765548893170075, 0.005976214794130558713, 0.006089113284605340327, 0.006314910265554874932, 0.006766504227453943275, 0.007218098189353012485, 0.007669692151252081695 ),
 .UNSPECIFIED. ) ;
#40250 = CARTESIAN_POINT ( 'NONE',  ( 175.1808269137907246, 281.3498469887747433, -14.26151238791351261 ) ) ;
#40251 = AXIS2_PLACEMENT_3D ( 'NONE', #15828, #46733, #15316 ) ;
#40252 = CARTESIAN_POINT ( 'NONE',  ( -10.43332761869022640, 164.7833772461660544, -9.188101187500095079 ) ) ;
#40253 = CARTESIAN_POINT ( 'NONE',  ( 66.75734579356596043, 67.35081300050364916, -6.869089300961301880 ) ) ;
#40254 = CARTESIAN_POINT ( 'NONE',  ( 68.81249350320682368, 63.82265338634812935, -12.23679878556980150 ) ) ;
#40255 = CARTESIAN_POINT ( 'NONE',  ( 151.1451503555562113, 268.8559155969762742, -15.81507177720227553 ) ) ;
#40256 = CARTESIAN_POINT ( 'NONE',  ( 186.1033490533799579, 283.4419393130733624, 16.98975762302446668 ) ) ;
#40257 = CARTESIAN_POINT ( 'NONE',  ( 194.8598199529639317, 293.1398868181796615, -15.91766051364927570 ) ) ;
#40258 = CARTESIAN_POINT ( 'NONE',  ( 72.89924121220336417, 67.41618724535075557, 11.90048241206199897 ) ) ;
#40259 = CARTESIAN_POINT ( 'NONE',  ( 164.2712161151136172, 246.1209027979328710, 7.276091357954241445 ) ) ;
#40260 = CARTESIAN_POINT ( 'NONE',  ( 191.0481192767711036, 299.7419460525905492, -9.103377665618040737 ) ) ;
#40261 = CARTESIAN_POINT ( 'NONE',  ( 190.5726849661229210, 300.5654224342945326, -0.2192718484028965964 ) ) ;
#40262 = ORIENTED_EDGE ( 'NONE', *, *, #26433, .F. ) ;
#40263 = CARTESIAN_POINT ( 'NONE',  ( 153.2106226585791831, 267.1006197558320991, -16.38176366188328359 ) ) ;
#40264 = CARTESIAN_POINT ( 'NONE',  ( 161.5029716424245407, 251.3413373469583973, -13.00020995489466458 ) ) ;
#40265 = CARTESIAN_POINT ( 'NONE',  ( 106.3178956768819319, 226.0643266524159856, -9.188101187500093303 ) ) ;
#40266 = CARTESIAN_POINT ( 'NONE',  ( 14.05589992062122917, 20.06628583063840310, -9.188101187500006262 ) ) ;
#40267 = DIRECTION ( 'NONE',  ( -0.000000000000000000, -0.000000000000000000, -1.000000000000000000 ) ) ;
#40268 = DIRECTION ( 'NONE',  ( -0.000000000000000000, -0.000000000000000000, -1.000000000000000000 ) ) ;
#40270 = CARTESIAN_POINT ( 'NONE',  ( 6.117390533544191378, 29.33055864014942316, -10.00000000000000000 ) ) ;
#40269 = CARTESIAN_POINT ( 'NONE',  ( 157.2168982216852555, 258.3393398020932636, 18.09635675623264106 ) ) ;
#40271 = CARTESIAN_POINT ( 'NONE',  ( 191.3729584906539003, 299.1793080298546101, -7.317708866624486497 ) ) ;
#40272 = CARTESIAN_POINT ( 'NONE',  ( 196.5806080813426888, 290.1593943507663766, -16.31912166233602690 ) ) ;
#40273 = EDGE_CURVE ( 'NONE', #76267, #16766, #31125, .T. ) ;
#40274 = CARTESIAN_POINT ( 'NONE',  ( 181.8129518053731033, 270.5384970965435514, -17.23398818032472946 ) ) ;
#40275 = CARTESIAN_POINT ( 'NONE',  ( 173.1810892923022038, 289.7194164501482305, -1.146283512214450351 ) ) ;
#40276 = LINE ( 'NONE', #69691, #19993 ) ;
#40277 = CARTESIAN_POINT ( 'NONE',  ( 68.47753283764532739, 66.06621294245498177, -10.79241679792292530 ) ) ;
#40278 = CARTESIAN_POINT ( 'NONE',  ( 26.00142736512681907, 15.41603393254325560, -1.583844403245362020 ) ) ;
#40279 = CARTESIAN_POINT ( 'NONE',  ( 196.5361253761390685, 267.7136571270361287, 9.529754956671661503 ) ) ;
#40280 = ORIENTED_EDGE ( 'NONE', *, *, #2311, .F. ) ;
#40281 = CARTESIAN_POINT ( 'NONE',  ( 176.7131714061462162, 273.8257724863759108, 17.80520185479879203 ) ) ;
#40283 = EDGE_CURVE ( 'NONE', #88729, #47896, #19306, .T. ) ;
#40282 = CARTESIAN_POINT ( 'NONE',  ( 183.6324539711410750, 256.9743827782117478, 4.698106744110496891 ) ) ;
#40284 = CARTESIAN_POINT ( 'NONE',  ( 184.7157775894015117, 297.3647472220100099, -4.497232409310948142 ) ) ;
#40285 = CARTESIAN_POINT ( 'NONE',  ( 174.3506819931331506, 286.9267872025895940, 11.76311152586403885 ) ) ;
#40286 = EDGE_LOOP ( 'NONE', ( #52439, #73382, #81370, #76506 ) ) ;
#40287 = CARTESIAN_POINT ( 'NONE',  ( 32.24342178309110096, 47.97677246190463052, 10.00000000000000000 ) ) ;
#40288 = VECTOR ( 'NONE', #94603, 1000.000000000000000 ) ;
#40289 = CARTESIAN_POINT ( 'NONE',  ( 40.50696180670117741, 29.10170272979929962, -7.433330006724141015 ) ) ;
#40290 = CARTESIAN_POINT ( 'NONE',  ( 84.21805166483638061, 41.46905487699226711, 1.456718203712574322 ) ) ;
#40291 = ORIENTED_EDGE ( 'NONE', *, *, #27210, .F. ) ;
#40292 = CARTESIAN_POINT ( 'NONE',  ( 164.1828665376937408, 279.9707757242401840, 12.51912677511460181 ) ) ;
#40293 = EDGE_CURVE ( 'NONE', #26784, #64892, #43482, .T. ) ;
#40294 = CYLINDRICAL_SURFACE ( 'NONE', #82323, 10.00000000000010658 ) ;
#40295 = CARTESIAN_POINT ( 'NONE',  ( 83.07746382761068560, 43.99571311473679458, -9.259344712981764758 ) ) ;
#40296 = ORIENTED_EDGE ( 'NONE', *, *, #90378, .T. ) ;
#40297 = CARTESIAN_POINT ( 'NONE',  ( 79.55938800887707885, 59.45545654668635649, 16.55147640184673463 ) ) ;
#40298 = CARTESIAN_POINT ( 'NONE',  ( -59.65739779450132829, 37.15562860896454112, 10.00000000000000000 ) ) ;
#40299 = CARTESIAN_POINT ( 'NONE',  ( 164.0741338217690668, 246.4622593432776796, 7.359073626423302983 ) ) ;
#40300 = CARTESIAN_POINT ( 'NONE',  ( 22.85147042958088193, 25.14441083166261137, 10.00000000000000533 ) ) ;
#40301 = FACE_OUTER_BOUND ( 'NONE', #79023, .T. ) ;
#40302 = AXIS2_PLACEMENT_3D ( 'NONE', #31260, #94111, #62651 ) ;
#40303 = CARTESIAN_POINT ( 'NONE',  ( 72.18990340680744566, 72.03918383723207342, -3.149060597287207219 ) ) ;
#40304 = CARTESIAN_POINT ( 'NONE',  ( 80.21951685124797393, 44.77929739833423639, 11.12462274611551116 ) ) ;
#40305 = CARTESIAN_POINT ( 'NONE',  ( 155.5211745099813356, 261.2764194263634749, -17.18163098020766810 ) ) ;
#40306 = ORIENTED_EDGE ( 'NONE', *, *, #52129, .F. ) ;
#40307 = ORIENTED_EDGE ( 'NONE', *, *, #68585, .T. ) ;
#40308 = FACE_OUTER_BOUND ( 'NONE', #92446, .T. ) ;
#40309 = ORIENTED_EDGE ( 'NONE', *, *, #87890, .T. ) ;
#40310 = CARTESIAN_POINT ( 'NONE',  ( 77.22023733200087747, 49.61776833328874403, -15.48932739092899347 ) ) ;
#40311 = ORIENTED_EDGE ( 'NONE', *, *, #67907, .F. ) ;
#40312 = DIRECTION ( 'NONE',  ( -1.000000000000000000, 0.000000000000000000, 0.000000000000000000 ) ) ;
#40314 = CARTESIAN_POINT ( 'NONE',  ( 78.80037227254219090, 51.26846376261736538, 15.25722946762347298 ) ) ;
#40313 = VECTOR ( 'NONE', #31340, 1000.000000000000000 ) ;
#40315 = ORIENTED_EDGE ( 'NONE', *, *, #89040, .T. ) ;
#40316 = CARTESIAN_POINT ( 'NONE',  ( 76.90746743093833970, 62.93938289886319382, -15.23233999435670150 ) ) ;
#40317 = CARTESIAN_POINT ( 'NONE',  ( 190.6865851974790473, 300.3681414465920625, 2.985923517389160509 ) ) ;
#40318 = LINE ( 'NONE', #1851, #67432 ) ;
#40319 = FACE_OUTER_BOUND ( 'NONE', #54881, .T. ) ;
#40320 = CARTESIAN_POINT ( 'NONE',  ( 185.5568049818104726, 266.1438378612298834, 14.60334785453874140 ) ) ;
#40321 = CARTESIAN_POINT ( 'NONE',  ( 45.12761469462908792, 206.8615022471902876, 5.000000000000046185 ) ) ;
#40322 = B_SPLINE_CURVE_WITH_KNOTS ( 'NONE', 3,
 ( #7967, #100177, #23139, #16053 ),
 .UNSPECIFIED., .F., .F.,
 ( 4, 4 ),
 ( 0.003503662168842324939, 0.007090156351249257347 ),
 .UNSPECIFIED. ) ;
#40323 = CARTESIAN_POINT ( 'NONE',  ( 156.7043981061308102, 280.3628295831616697, 2.089248679677577325 ) ) ;
#40324 = CARTESIAN_POINT ( 'NONE',  ( 132.6505673846437503, 238.2048013555409796, 4.594050593750051981 ) ) ;
#40325 = CARTESIAN_POINT ( 'NONE',  ( 184.2837900991036690, 261.1937265540972817, -9.136837574883312385 ) ) ;
#40326 = CARTESIAN_POINT ( 'NONE',  ( 43.68478726420265446, 28.14754757982094802, -5.678558825948276656 ) ) ;
#40327 = VERTEX_POINT ( 'NONE', #84383 ) ;
#40328 = AXIS2_PLACEMENT_3D ( 'NONE', #67953, #99859, #53244 ) ;
#40330 = ORIENTED_EDGE ( 'NONE', *, *, #75706, .T. ) ;
#40329 = CARTESIAN_POINT ( 'NONE',  ( 84.56191477375736554, 43.45664822029007723, -7.163795276308541737 ) ) ;
#40331 = CARTESIAN_POINT ( 'NONE',  ( 203.5079006281358431, 276.1533853654332802, 13.32764713983298499 ) ) ;
#40332 = ADVANCED_FACE ( 'NONE', ( #38732 ), #14457, .F. ) ;
#40333 = CARTESIAN_POINT ( 'NONE',  ( 181.1417631960959511, 255.6584326465087713, 0.5790604069595610692 ) ) ;
#40334 = CARTESIAN_POINT ( 'NONE',  ( 176.0127109592394277, 252.6004560315867593, -4.768680066900455650 ) ) ;
#40335 = CARTESIAN_POINT ( 'NONE',  ( 192.1174645699329346, 297.8897856739996541, 12.27388818933617110 ) ) ;
#40336 = CYLINDRICAL_SURFACE ( 'NONE', #98577, 10.00000000000010658 ) ;
#40337 = DIRECTION ( 'NONE',  ( -0.000000000000000000, -0.000000000000000000, -1.000000000000000000 ) ) ;
#40338 = CARTESIAN_POINT ( 'NONE',  ( 174.7842343859746563, 287.5387069739456365, -9.405270440949729860 ) ) ;
#40339 = CARTESIAN_POINT ( 'NONE',  ( 34.62385580964452458, 25.15404122711136026, 8.090169943749479842 ) ) ;
#40340 = CARTESIAN_POINT ( 'NONE',  ( -48.47243291925848752, 30.64988553008148031, 10.00000000000000000 ) ) ;
#40341 = ORIENTED_EDGE ( 'NONE', *, *, #76713, .T. ) ;
#40342 = CARTESIAN_POINT ( 'NONE',  ( 194.8708600166808651, 293.1207648669033006, -14.79199694356877970 ) ) ;
#40343 = CARTESIAN_POINT ( 'NONE',  ( 3.808674319871268921, 184.5530062829863027, -4.648177544792955347E-16 ) ) ;
#40344 = ORIENTED_EDGE ( 'NONE', *, *, #9117, .T. ) ;
#40345 = EDGE_CURVE ( 'NONE', #79781, #66505, #77243, .T. ) ;
#40346 = DIRECTION ( 'NONE',  ( -0.9762143704923770260, 0.2168075248790319320, 0.000000000000000000 ) ) ;
#40347 = ADVANCED_FACE ( 'NONE', ( #61536 ), #16438, .T. ) ;
#40348 = CARTESIAN_POINT ( 'NONE',  ( 190.6445454741162280, 284.1381220441062396, -17.32122990259229667 ) ) ;
#40349 = CARTESIAN_POINT ( 'NONE',  ( 192.1722555058605337, 297.7948849891782857, -10.50817311975818491 ) ) ;
#40350 = CARTESIAN_POINT ( 'NONE',  ( 149.0323968763055689, 272.5153119669064949, 11.64231532207353403 ) ) ;
#40351 = CARTESIAN_POINT ( 'NONE',  ( 163.2437751800324293, 247.9004826992694461, 9.806027032984305336 ) ) ;
#40353 = CARTESIAN_POINT ( 'NONE',  ( 160.7277267915518451, 281.8993980653820017, 6.551854072316369404 ) ) ;
#40352 = CARTESIAN_POINT ( 'NONE',  ( 161.6984845383829565, 281.6232062658947939, -6.601711233045046257 ) ) ;
#40354 = CARTESIAN_POINT ( 'NONE',  ( 199.9279498498847261, 267.4457311908202541, 6.228283794749674307 ) ) ;
#40355 = ORIENTED_EDGE ( 'NONE', *, *, #98341, .F. ) ;
#40356 = CARTESIAN_POINT ( 'NONE',  ( 190.1607982559816890, 301.2788311432216233, -4.972636536415983244 ) ) ;
#40357 = CARTESIAN_POINT ( 'NONE',  ( 187.1961889814599544, 261.9078172817692121, -8.752267960438080863 ) ) ;
#40358 = CARTESIAN_POINT ( 'NONE',  ( -86.81108781737714253, 4.999999999999999112, -14.21260523776213347 ) ) ;
#40359 = CARTESIAN_POINT ( 'NONE',  ( 87.87749860556357362, 43.91202660816024661, 0.3985875973167696262 ) ) ;
#40360 = CARTESIAN_POINT ( 'NONE',  ( 129.9777503372646095, 257.3967562850347122, -4.648177544792955347E-16 ) ) ;
#40361 = CARTESIAN_POINT ( 'NONE',  ( 153.3703256797887775, 265.0017988796566897, 16.44314709207578318 ) ) ;
#40362 = CARTESIAN_POINT ( 'NONE',  ( -19.65312891409030271, 93.06504152958497400, -10.00000000000000888 ) ) ;
#40363 = CARTESIAN_POINT ( 'NONE',  ( 193.9495889092963807, 294.7164532324382549, 15.46986001312306058 ) ) ;
#40364 = CARTESIAN_POINT ( 'NONE',  ( 68.24846459439849866, 69.97058443567007657, 1.257665481745562586 ) ) ;
#40365 = CARTESIAN_POINT ( 'NONE',  ( -6.184650803196579893, 176.4244531367911293, -4.594050593750046652 ) ) ;
#40366 = CARTESIAN_POINT ( 'NONE',  ( 90.56688509766992468, 223.0958772461660260, -9.188101187500095079 ) ) ;
#40367 = CARTESIAN_POINT ( 'NONE',  ( 67.16288355292338963, 68.85776602768420673, 5.438331637600131607 ) ) ;
#40368 = CARTESIAN_POINT ( 'NONE',  ( 88.13402233310422673, 44.37312773088997631, -4.489783613381812089 ) ) ;
#40369 = CARTESIAN_POINT ( 'NONE',  ( 148.1316126177475496, 276.0755160693871630, 5.020219949272568094 ) ) ;
#40371 = LINE ( 'NONE', #86062, #17249 ) ;
#40370 = AXIS2_PLACEMENT_3D ( 'NONE', #29696, #7903, #100113 ) ;
#40372 = AXIS2_PLACEMENT_3D ( 'NONE', #4033, #56219, #42031 ) ;
#40373 = CARTESIAN_POINT ( 'NONE',  ( -22.42236680055709641, 157.8615022471902591, 0.000000000000000000 ) ) ;
#40374 = LINE ( 'NONE', #16591, #40392 ) ;
#40376 = CARTESIAN_POINT ( 'NONE',  ( 163.4055107321044318, 247.6203485056908846, -10.24153090796238530 ) ) ;
#40375 = CARTESIAN_POINT ( 'NONE',  ( 73.80638704669732419, 68.31061168272384521, -11.57820046455322149 ) ) ;
#40377 = CARTESIAN_POINT ( 'NONE',  ( 178.4671845014859741, 289.9579026316837371, 9.503558631820238745 ) ) ;
#40378 = CARTESIAN_POINT ( 'NONE',  ( 166.0486951412649148, 249.5559827260773886, -9.134215000997858880 ) ) ;
#40379 = CARTESIAN_POINT ( 'NONE',  ( 73.39426628506285510, 56.64220877263274190, -16.01712807892389634 ) ) ;
#40380 = CARTESIAN_POINT ( 'NONE',  ( -13.92449252947024263, 172.7677522451419350, -5.000000000000047962 ) ) ;
#40381 = CARTESIAN_POINT ( 'NONE',  ( 161.8750289368003621, 250.2712207352165592, -13.97436367953006098 ) ) ;
#40382 = VECTOR ( 'NONE', #86684, 1000.000000000000227 ) ;
#40383 = CARTESIAN_POINT ( 'NONE',  ( 37.90188877791127453, 186.5643266524160424, 9.188101187500095079 ) ) ;
#40384 = CARTESIAN_POINT ( 'NONE',  ( 77.00376392975798012, 63.39239755058648029, -15.46687034352795109 ) ) ;
#40385 = CARTESIAN_POINT ( 'NONE',  ( 74.27495573685767738, 207.5643266524160424, 9.188101187500095079 ) ) ;
#40386 = CARTESIAN_POINT ( 'NONE',  ( 183.2462649708989773, 258.1020939971272128, 7.820152278097399545 ) ) ;
#40387 = CARTESIAN_POINT ( 'NONE',  ( 88.44311045277898131, 43.83777140359737956, 0.09123111681703632847 ) ) ;
#40388 = CARTESIAN_POINT ( 'NONE',  ( 166.9983013567537000, 259.4879522421344973, 16.46229539392700048 ) ) ;
#40390 = CARTESIAN_POINT ( 'NONE',  ( 70.57897896622060330, 71.00804091966597298, -4.942816957066797023 ) ) ;
#40389 = CARTESIAN_POINT ( 'NONE',  ( 80.93613592869992601, 42.95327845849681836, -9.503115154567232992 ) ) ;
#40392 = VECTOR ( 'NONE', #93630, 999.9999999999998863 ) ;
#40391 = CARTESIAN_POINT ( 'NONE',  ( 176.1400978288397994, 269.8946129783859078, -16.59496141468774510 ) ) ;
#40393 = EDGE_CURVE ( 'NONE', #1103, #28901, #38219, .T. ) ;
#40394 = CARTESIAN_POINT ( 'NONE',  ( 28.23826220571969969, 31.70171378149920471, -9.188101187500004485 ) ) ;
#40395 = CARTESIAN_POINT ( 'NONE',  ( 81.27194768136315872, 46.27379842166399726, 12.52033010236089261 ) ) ;
#40396 = CARTESIAN_POINT ( 'NONE',  ( 79.69317059041301832, 47.75519670552719731, -13.50432480851453931 ) ) ;
#40397 = ORIENTED_EDGE ( 'NONE', *, *, #81244, .F. ) ;
#40398 = CARTESIAN_POINT ( 'NONE',  ( 23.64951029700315743, 14.44966523072494624, -2.296566073217252530E-15 ) ) ;
#40399 = CARTESIAN_POINT ( 'NONE',  ( 57.33281313167710636, 216.1589784336662206, -6.496448406907676862E-16 ) ) ;
#40400 = DIRECTION ( 'NONE',  ( -0.8660254037844379305, -0.5000000000000014433, -0.000000000000000000 ) ) ;
#40401 = CARTESIAN_POINT ( 'NONE',  ( 11.76667899187106059, 31.90941714274742225, 10.00000000000000000 ) ) ;
#40402 = CARTESIAN_POINT ( 'NONE',  ( 173.1206616589821010, 289.7470628071918668, -0.8130285733345999910 ) ) ;
#40403 = CARTESIAN_POINT ( 'NONE',  ( 49.51900556837681222, 105.3795262313705763, 10.00000000000000000 ) ) ;
#40404 = CARTESIAN_POINT ( 'NONE',  ( 153.9658056652968980, 263.9703972898665825, 16.69902601383360619 ) ) ;
#40405 = ADVANCED_FACE ( 'NONE', ( #68638 ), #15421, .F. ) ;
#40406 = CIRCLE ( 'NONE', #14544, 70.00000000000001421 ) ;
#40407 = EDGE_LOOP ( 'NONE', ( #53412, #32614, #9174, #10224, #75729 ) ) ;
#40408 =( BOUNDED_CURVE ( )  B_SPLINE_CURVE ( 2, ( #37779, #77296, #8395, #92048, #68681, #24085, #39265, #84434, #31669 ),
 .UNSPECIFIED., .F., .T. ) 
 B_SPLINE_CURVE_WITH_KNOTS ( ( 3, 2, 2, 2, 3 ),
 ( 0.9475806451612903691, 0.9489247311827957443, 0.9516129032258064946, 0.9543010752688172449, 0.9556451612903226200 ),
 .UNSPECIFIED. ) 
 CURVE ( )  GEOMETRIC_REPRESENTATION_ITEM ( )  RATIONAL_B_SPLINE_CURVE ( ( 0.9330127018922194093, 0.9330127018922194093, 1.000000000000000000, 0.8660254037844387076, 1.000000000000000000, 0.8660254037844387076, 1.000000000000000000, 0.9330127018922194093, 0.9330127018922194093 ) ) 
 REPRESENTATION_ITEM ( '' )  );
#40409 = CARTESIAN_POINT ( 'NONE',  ( 192.4413533297683330, 287.8524838211871497, 16.04042031060856033 ) ) ;
#40410 = CARTESIAN_POINT ( 'NONE',  ( 123.0699010352285825, 251.8615022471902876, 5.000000000000046185 ) ) ;
#40411 = CARTESIAN_POINT ( 'NONE',  ( 20.30386484825465132, 170.9824982072973967, 3.021315404115420679E-15 ) ) ;
#40412 = DIRECTION ( 'NONE',  ( -0.8660254037844387076, -0.4999999999999998890, -0.000000000000000000 ) ) ;
#40413 = CARTESIAN_POINT ( 'NONE',  ( 149.3545991938273971, 273.9572411826421217, -10.14243178476390028 ) ) ;
#40414 = CARTESIAN_POINT ( 'NONE',  ( 188.3480435840147322, 273.1765081552686070, 15.60535422690979424 ) ) ;
#40415 = ORIENTED_EDGE ( 'NONE', *, *, #4791, .T. ) ;
#40416 = CARTESIAN_POINT ( 'NONE',  ( 159.8188415394622268, 253.8326417772889840, -15.43862849427313222 ) ) ;
#40417 = CARTESIAN_POINT ( 'NONE',  ( 151.9706434441667113, 279.1253449119590186, -0.3226571599251377709 ) ) ;
#40418 = EDGE_CURVE ( 'NONE', #65011, #86855, #75940, .T. ) ;
#40419 = CARTESIAN_POINT ( 'NONE',  ( 73.01258037670726253, 68.72995673837564823, -10.14057597975430447 ) ) ;
#40420 = VERTEX_POINT ( 'NONE', #70124 ) ;
#40421 = CARTESIAN_POINT ( 'NONE',  ( 177.1809705214487849, 253.2799522049397751, -0.2609578167311901176 ) ) ;
#40422 = ORIENTED_EDGE ( 'NONE', *, *, #88325, .T. ) ;
#40423 = CARTESIAN_POINT ( 'NONE',  ( 79.48876273271771709, 46.38894273206648222, -12.71961528548988873 ) ) ;
#40424 = CARTESIAN_POINT ( 'NONE',  ( 167.5224888712764084, 247.9179630693595300, 3.541551421311048387 ) ) ;
#40425 = CARTESIAN_POINT ( 'NONE',  ( 148.8264412599648097, 273.9886447002814975, 8.871318654940013815 ) ) ;
#40426 = ORIENTED_EDGE ( 'NONE', *, *, #99553, .F. ) ;
#40427 = CARTESIAN_POINT ( 'NONE',  ( 22.55378097864968012, 33.99752408145592852, 5.678558825948276656 ) ) ;
#40428 = CARTESIAN_POINT ( 'NONE',  ( 84.60239308390620749, 50.60453406874029270, -14.06751209996561158 ) ) ;
#40429 = CARTESIAN_POINT ( 'NONE',  ( 83.78198294410601932, 48.18673714097705840, -12.33272353593454085 ) ) ;
#40430 = ORIENTED_EDGE ( 'NONE', *, *, #93462, .T. ) ;
#40431 = CARTESIAN_POINT ( 'NONE',  ( 167.0784635423869986, 276.4927169897987369, 15.85967558429602775 ) ) ;
#40432 = EDGE_CURVE ( 'NONE', #37717, #70938, #92479, .T. ) ;
#40433 = CARTESIAN_POINT ( 'NONE',  ( 165.3929592122126451, 286.2279243276498732, 4.432946431554212197 ) ) ;
#40434 = B_SPLINE_CURVE_WITH_KNOTS ( 'NONE', 3,
 ( #29781, #4488, #90639, #20201, #66293, #67784, #44467, #29294, #75909, #60653, #58667, #27794, #89639, #23656, #7988, #69770, #84029, #23162, #16073, #99692, #92134, #22687, #22182, #38864, #378, #15063, #46975, #76400, #100199, #53075, #69271, #39351, #45466, #61166, #31267, #53566, #68768, #46456, #62153, #14588, #70265, #6976, #38361, #45953, #37859, #76870 ),
 .UNSPECIFIED., .F., .F.,
 ( 4, 1, 1, 1, 2, 2, 1, 1, 1, 2, 2, 1, 1, 2, 2, 1, 1, 2, 2, 1, 1, 2, 2, 1, 2, 2, 1, 2, 2, 4 ),
 ( 0.000000000000000000, 0.06250000000000216493, 0.09375000000000272005, 0.1093750000000035388, 0.1171875000000033029, 0.1250000000000030809, 0.1874999999999965861, 0.2187499999999915623, 0.2343749999999891476, 0.2421874999999873990, 0.2499999999999856504, 0.3124999999999859557, 0.3437499999999861777, 0.3593749999999880096, 0.3749999999999898415, 0.4374999999999897304, 0.4687499999999908407, 0.4843749999999908962, 0.4999999999999909517, 0.5624999999999934497, 0.5937499999999930056, 0.6093749999999941158, 0.6249999999999952260, 0.6874999999999963363, 0.7187499999999952260, 0.7499999999999941158, 0.8124999999999952260, 0.8437499999999956701, 0.8749999999999961142, 1.000000000000000000 ),
 .UNSPECIFIED. ) ;
#40435 = VERTEX_POINT ( 'NONE', #53919 ) ;
#40436 = ORIENTED_EDGE ( 'NONE', *, *, #83221, .F. ) ;
#40437 = CARTESIAN_POINT ( 'NONE',  ( 183.1883525905292913, 295.7849739342112798, 1.003725237841741613 ) ) ;
#40439 = CARTESIAN_POINT ( 'NONE',  ( 147.6095889327917803, 274.9796876144846465, -8.460961150142429332 ) ) ;
#40438 = CARTESIAN_POINT ( 'NONE',  ( 67.71951918407867765, 65.69802484793109443, 10.71695699751798969 ) ) ;
#40440 = CARTESIAN_POINT ( 'NONE',  ( 81.76940595752934371, 55.36688792037507056, -15.93096493606815933 ) ) ;
#40441 = CARTESIAN_POINT ( 'NONE',  ( 193.7261517370125432, 295.1034577671335342, 14.97744313279139661 ) ) ;
#40442 = CARTESIAN_POINT ( 'NONE',  ( 185.4422274959847527, 292.4385988784968617, -11.34057656226370447 ) ) ;
#40443 = CARTESIAN_POINT ( 'NONE',  ( 205.2391015854675516, 275.1624436846170738, -14.01434138479280911 ) ) ;
#40444 = CARTESIAN_POINT ( 'NONE',  ( 145.4512450625087467, 254.7833772461660544, -9.188101187500095079 ) ) ;
#40445 = CIRCLE ( 'NONE', #53393, 0.1418229129684436818 ) ;
#40446 = CARTESIAN_POINT ( 'NONE',  ( 71.97605894070565569, 62.66438405307972204, -14.59188024022812691 ) ) ;
#40447 = CARTESIAN_POINT ( 'NONE',  ( 79.49274628814450239, 59.57836040576013659, 16.53926144102299034 ) ) ;
#40448 = CARTESIAN_POINT ( 'NONE',  ( 80.17458025225667484, 217.0958772461660544, -9.188101187500095079 ) ) ;
#40449 = ORIENTED_EDGE ( 'NONE', *, *, #79059, .T. ) ;
#40450 = CARTESIAN_POINT ( 'NONE',  ( 190.8443993347725325, 300.0947993426467519, 8.522468760355437212 ) ) ;
#40451 = CARTESIAN_POINT ( 'NONE',  ( 78.12682272674805972, 61.49995998885079729, -16.15539878443392396 ) ) ;
#40452 = ORIENTED_EDGE ( 'NONE', *, *, #43624, .T. ) ;
#40453 = CARTESIAN_POINT ( 'NONE',  ( 180.1800635485680573, 295.0721525882481160, 3.264262412682620962 ) ) ;
#40454 = ORIENTED_EDGE ( 'NONE', *, *, #57873, .T. ) ;
#40455 = EDGE_CURVE ( 'NONE', #79518, #79225, #71662, .T. ) ;
#40456 = CARTESIAN_POINT ( 'NONE',  ( 80.05471186046345622, 44.29272515403749821, -11.46072743220592294 ) ) ;
#40457 = DIRECTION ( 'NONE',  ( 0.8660254037844385966, 0.5000000000000002220, 3.252519625699450438E-16 ) ) ;
#40458 = CARTESIAN_POINT ( 'NONE',  ( 198.2505066714982149, 285.2670451491296149, 0.000000000000000000 ) ) ;
#40459 = CARTESIAN_POINT ( 'NONE',  ( 82.28273451354495194, 47.89750625978791021, -12.72550930769195254 ) ) ;
#40460 = CARTESIAN_POINT ( 'NONE',  ( 207.9312334543074599, 270.4995345071110933, 1.552289074598145469 ) ) ;
#40461 = CARTESIAN_POINT ( 'NONE',  ( 91.40610752940987993, 214.3923013555409796, 4.594050593750050204 ) ) ;
#40462 = ORIENTED_EDGE ( 'NONE', *, *, #47713, .T. ) ;
#40463 = VECTOR ( 'NONE', #63796, 1000.000000000000000 ) ;
#40464 = EDGE_CURVE ( 'NONE', #31220, #8428, #736, .T. ) ;
#40465 = ORIENTED_EDGE ( 'NONE', *, *, #98665, .F. ) ;
#40466 = B_SPLINE_SURFACE_WITH_KNOTS ( 'NONE', 3, 1, ( 
 ( #84652, #70409 ),
 ( #78531, #9115 ),
 ( #92745, #78026 ),
 ( #93759, #15700 ),
 ( #24317, #55192 ),
 ( #30912, #31404 ),
 ( #86176, #62291 ),
 ( #22815, #39987 ),
 ( #70928, #32414 ),
 ( #93247, #2017 ),
 ( #55683, #38500 ),
 ( #1533, #23300 ),
 ( #17203, #54691 ),
 ( #15195, #48105 ),
 ( #79048, #92267 ),
 ( #9637, #54189 ),
 ( #53695, #46598 ),
 ( #46093, #77005 ),
 ( #7611, #61799 ),
 ( #69415, #77531 ),
 ( #8124, #38997 ),
 ( #57195, #71927 ),
 ( #19728, #25306 ),
 ( #27318, #65793 ),
 ( #96752, #26321 ),
 ( #19244, #88174 ),
 ( #87189, #18721 ),
 ( #50109, #42007 ),
 ( #56194, #17722 ),
 ( #72940, #48625 ),
 ( #41499, #34409 ) ),
 .UNSPECIFIED., .F., .F., .F.,
 ( 4, 3, 3, 3, 3, 3, 3, 3, 3, 3, 4 ),
 ( 2, 2 ),
 ( 0.000000000000000000, 0.1122669598086659254, 0.2243161639709550792, 0.3396355846218998553, 0.4553962076584952556, 0.5677860799922195278, 0.6749047109689478852, 0.7773884377078161823, 0.8775581155834035751, 0.9782364162377661376, 1.000000000000000000 ),
 ( 0.000000000000000000, 1.000000000000000000 ),
 .UNSPECIFIED. ) ;
#40467 = CARTESIAN_POINT ( 'NONE',  ( 80.44215978124604760, 58.39441083166272506, 0.000000000000000000 ) ) ;
#40468 = VERTEX_POINT ( 'NONE', #54934 ) ;
#40469 = EDGE_CURVE ( 'NONE', #17797, #78693, #69134, .T. ) ;
#40470 = EDGE_CURVE ( 'NONE', #74770, #73478, #25551, .T. ) ;
#40471 = CARTESIAN_POINT ( 'NONE',  ( 75.91641493099308491, 64.71284702731330185, -14.30921724464636924 ) ) ;
#40472 = CARTESIAN_POINT ( 'NONE',  ( 68.20353262459525467, 69.11303344777483915, -4.901384820270958897 ) ) ;
#40473 = CARTESIAN_POINT ( 'NONE',  ( 99.68721513304873838, 238.3615022471903160, 5.000000000000046185 ) ) ;
#40474 = CARTESIAN_POINT ( 'NONE',  ( 88.26872550477153823, 44.38513711945522289, 4.282355379009170626 ) ) ;
#40475 = ORIENTED_EDGE ( 'NONE', *, *, #69116, .T. ) ;
#40476 = CARTESIAN_POINT ( 'NONE',  ( 85.86066238541921791, 43.85667369948165373, -5.309618687222620537 ) ) ;
#40477 = EDGE_CURVE ( 'NONE', #39976, #29044, #86907, .T. ) ;
#40478 = CARTESIAN_POINT ( 'NONE',  ( 80.75588300432519873, 45.91452481213949710, 11.84376094130757018 ) ) ;
#40479 = CARTESIAN_POINT ( 'NONE',  ( 206.6298919378964740, 272.7535241315335384, -9.267551915974392429 ) ) ;
#40480 = EDGE_CURVE ( 'NONE', #87662, #53811, #83047, .T. ) ;
#40481 = DIRECTION ( 'NONE',  ( -0.5000000000000003331, 0.8660254037844383745, -9.251858538542983907E-17 ) ) ;
#40482 = CARTESIAN_POINT ( 'NONE',  ( 177.1365833152386244, 284.6974615985632795, 13.05344454345314986 ) ) ;
#40483 = CARTESIAN_POINT ( 'NONE',  ( 162.8839417982861448, 263.3994626277539055, 17.77684832337497767 ) ) ;
#40484 = CARTESIAN_POINT ( 'NONE',  ( 195.4347729807024905, 279.6077732330228400, -17.24073704596056089 ) ) ;
#40485 = VERTEX_POINT ( 'NONE', #63537 ) ;
#40486 = CARTESIAN_POINT ( 'NONE',  ( 202.7724833007839891, 277.6125776806421186, -15.34270362070550497 ) ) ;
#40487 = CARTESIAN_POINT ( 'NONE',  ( 200.3765029811139584, 283.5847115241710981, 16.85207472104531590 ) ) ;
#40488 = CARTESIAN_POINT ( 'NONE',  ( 84.69116302952653541, 43.17850746977291010, 5.277877534678879989 ) ) ;
#40489 = FACE_OUTER_BOUND ( 'NONE', #7942, .T. ) ;
#40490 = CARTESIAN_POINT ( 'NONE',  ( 83.46272733064347449, 51.93221652752757933, 15.00972995268700139 ) ) ;
#40491 = CARTESIAN_POINT ( 'NONE',  ( 175.0130774361952035, 290.1460611646906500, -6.342396626919687641 ) ) ;
#40492 = FACE_OUTER_BOUND ( 'NONE', #25260, .T. ) ;
#40493 = ORIENTED_EDGE ( 'NONE', *, *, #80291, .F. ) ;
#40494 = CARTESIAN_POINT ( 'NONE',  ( 168.6156890688689884, 286.4116463664167895, -8.226575548882113509 ) ) ;
#40495 = CARTESIAN_POINT ( 'NONE',  ( 206.9408877595175511, 272.2148635675444552, 6.707071080545934372 ) ) ;
#40496 = LINE ( 'NONE', #24804, #81980 ) ;
#40497 = CARTESIAN_POINT ( 'NONE',  ( 200.5914588262792222, 282.7033700937254821, -16.73555027083989444 ) ) ;
#40498 = CARTESIAN_POINT ( 'NONE',  ( 31.67936943677743855, 23.45404122711135386, -8.090169943749478065 ) ) ;
#40499 = CARTESIAN_POINT ( 'NONE',  ( 77.95436975687957215, 48.11784896437987413, 14.20357318872345331 ) ) ;
#40500 = CARTESIAN_POINT ( 'NONE',  ( 168.8069195673892580, 272.9388147432762253, 15.96133530879710172 ) ) ;
#40501 = CARTESIAN_POINT ( 'NONE',  ( 183.5555461010262661, 274.8638377643932813, 16.36404075196846364 ) ) ;
#40502 = DIRECTION ( 'NONE',  ( -0.000000000000000000, -0.000000000000000000, 1.000000000000000000 ) ) ;
#40503 = CARTESIAN_POINT ( 'NONE',  ( 188.8764293144468240, 259.6972905960182061, 3.583694637520717041 ) ) ;
#40504 = CARTESIAN_POINT ( 'NONE',  ( -21.75249381947928740, 146.7012482093458914, 37.49999999999996447 ) ) ;
#40505 = CARTESIAN_POINT ( 'NONE',  ( 4.126898030318161936, 167.0643266524160424, 9.188101187500095079 ) ) ;
#40506 = CARTESIAN_POINT ( 'NONE',  ( 82.51799120075359895, 48.96200246141732038, 13.33826670467029984 ) ) ;
#40507 = ORIENTED_EDGE ( 'NONE', *, *, #98843, .T. ) ;
#40508 = CARTESIAN_POINT ( 'NONE',  ( 174.9245405914076343, 255.2035582809694176, 9.090376104202114504 ) ) ;
#40509 = CARTESIAN_POINT ( 'NONE',  ( 33.41142024434631708, 24.45404122711135386, -8.090169943749478065 ) ) ;
#40510 = CARTESIAN_POINT ( 'NONE',  ( 82.10237303103902207, 41.84040927510496033, 5.493823265887765928 ) ) ;
#40511 = CARTESIAN_POINT ( 'NONE',  ( 14.27519936121077926, 188.2369531367911293, -4.594050593750048428 ) ) ;
#40512 = CARTESIAN_POINT ( 'NONE',  ( 175.0125019719911847, 292.0719086349095051, 3.303583340955516423 ) ) ;
#40513 = CARTESIAN_POINT ( 'NONE',  ( 31.01079167849261964, 40.83705186507756224, 3.090169943749475401 ) ) ;
#40514 = CARTESIAN_POINT ( 'NONE',  ( 177.8194257969418288, 292.8449071177858514, 6.006967295066290013 ) ) ;
#40515 = CARTESIAN_POINT ( 'NONE',  ( 173.5658952278579363, 272.9572349787487724, -16.37894178319135818 ) ) ;
#40516 = CARTESIAN_POINT ( 'NONE',  ( 196.6640600515679580, 290.0148512983446949, 16.35009042604046314 ) ) ;
#40517 = CARTESIAN_POINT ( 'NONE',  ( 133.5964594837526533, 259.4860189848785694, -2.679491924311252493 ) ) ;
#40518 = CARTESIAN_POINT ( 'NONE',  ( 169.9907874252009492, 274.9766311711105118, 17.04400878134698161 ) ) ;
#40519 = APPLICATION_CONTEXT ( 'automotive_design' ) ;
#40520 = CARTESIAN_POINT ( 'NONE',  ( 187.1121570753812193, 296.0775264014479831, -7.699669239627596973 ) ) ;
#40521 = CARTESIAN_POINT ( 'NONE',  ( 83.53052282221433700, 51.97849157102297823, 15.01265415031365258 ) ) ;
#40522 = CIRCLE ( 'NONE', #92362, 0.1418229129680863287 ) ;
#40523 = CARTESIAN_POINT ( 'NONE',  ( 192.9866187040997829, 295.5921736933902935, -12.74678698041507197 ) ) ;
#40524 = CARTESIAN_POINT ( 'NONE',  ( 68.07728789491679322, 200.1115022471901739, -5.000000000000041744 ) ) ;
#40525 = CARTESIAN_POINT ( 'NONE',  ( 72.75575765633803371, 66.35992158122787998, -12.11670373630936304 ) ) ;
#40526 = CYLINDRICAL_SURFACE ( 'NONE', #73284, 70.00000000000002842 ) ;
#40527 = CARTESIAN_POINT ( 'NONE',  ( 203.3903727158224228, 270.0836496803775049, 6.045350443737255830 ) ) ;
#40528 = CARTESIAN_POINT ( 'NONE',  ( 34.97905304013878691, 184.8768266524159856, 9.188101187500098632 ) ) ;
#40529 = CARTESIAN_POINT ( 'NONE',  ( 198.0792648159935538, 287.5636447432459022, 17.04758482866669667 ) ) ;
#40530 = CARTESIAN_POINT ( 'NONE',  ( -4.653128914090328472, 78.77562236714182120, 13.81405534229504717 ) ) ;
#40531 = CARTESIAN_POINT ( 'NONE',  ( 150.6916211261701619, 269.6414512649903941, -15.44346024757110847 ) ) ;
#40532 = EDGE_CURVE ( 'NONE', #69750, #63734, #40221, .T. ) ;
#40533 = CARTESIAN_POINT ( 'NONE',  ( 67.30637966541804929, 66.39985843937958521, -8.834011029012955873 ) ) ;
#40534 = VERTEX_POINT ( 'NONE', #18968 ) ;
#40535 = CARTESIAN_POINT ( 'NONE',  ( 3.630564096624801174, 166.2365022471902307, 10.00000000000009948 ) ) ;
#40536 = CARTESIAN_POINT ( 'NONE',  ( 144.9899443387551798, 254.5170451491295296, 0.000000000000000000 ) ) ;
#40537 = FACE_OUTER_BOUND ( 'NONE', #69328, .T. ) ;
#40538 = CARTESIAN_POINT ( 'NONE',  ( 162.8839417982861448, 263.3994626277539055, 17.77684832337497767 ) ) ;
#40539 = CARTESIAN_POINT ( 'NONE',  ( 30.03287232231581072, 25.84335787977764554, 9.188101187500006262 ) ) ;
#40540 = CARTESIAN_POINT ( 'NONE',  ( 162.6626107288841467, 248.9070890562113902, 10.12509462564867313 ) ) ;
#40541 = CARTESIAN_POINT ( 'NONE',  ( 149.4908848037268001, 271.7211875819559737, -12.92288068979413573 ) ) ;
#40542 = CARTESIAN_POINT ( 'NONE',  ( 185.6900645067668165, 267.8684138037842786, -14.44923933729529963 ) ) ;
#40543 = ORIENTED_EDGE ( 'NONE', *, *, #36810, .F. ) ;
#40544 = CARTESIAN_POINT ( 'NONE',  ( 10.54248283575963008, 11.80170272979924206, 7.433330006724137462 ) ) ;
#40545 = CARTESIAN_POINT ( 'NONE',  ( 78.23242879811255079, 58.04918888810001931, -16.20759052872706718 ) ) ;
#40546 = CARTESIAN_POINT ( 'NONE',  ( 71.86256228778262312, 72.60615528678948749, -0.5650332253008888417 ) ) ;
#40547 = EDGE_CURVE ( 'NONE', #48375, #76464, #59676, .T. ) ;
#40548 = ORIENTED_EDGE ( 'NONE', *, *, #25961, .T. ) ;
#40549 = CARTESIAN_POINT ( 'NONE',  ( 106.0403798229140619, 220.4824982072973683, 3.021315404115420679E-15 ) ) ;
#40550 = CARTESIAN_POINT ( 'NONE',  ( 85.26988926578472672, 49.08626644514237114, 12.44667837020937995 ) ) ;
#40551 = EDGE_CURVE ( 'NONE', #86134, #30236, #29295, .T. ) ;
#40552 = CARTESIAN_POINT ( 'NONE',  ( 177.3939513230285172, 256.1386864175269125, -7.257050990210307084 ) ) ;
#40553 = CARTESIAN_POINT ( 'NONE',  ( 190.4841013044967042, 300.7188538369516095, 4.682298117523464143 ) ) ;
#40554 = ORIENTED_EDGE ( 'NONE', *, *, #70081, .T. ) ;
#40555 = ORIENTED_EDGE ( 'NONE', *, *, #9370, .T. ) ;
#40556 = CARTESIAN_POINT ( 'NONE',  ( 186.3138662162842820, 272.0885644523062865, -16.12950033991073795 ) ) ;
#40557 = ORIENTED_EDGE ( 'NONE', *, *, #81441, .F. ) ;
#40558 = CARTESIAN_POINT ( 'NONE',  ( 44.68504016816520164, 27.92755873383629961, 6.180339887498953466 ) ) ;
#40559 = PLANE ( 'NONE',  #44796 ) ;
#40560 = CARTESIAN_POINT ( 'NONE',  ( 72.71055119297287206, 57.13306343736743287, -15.89095181684541380 ) ) ;
#40561 = CARTESIAN_POINT ( 'NONE',  ( 4.767924915890233706, 21.49103043416546654, -8.090169943749479842 ) ) ;
#40562 = CARTESIAN_POINT ( 'NONE',  ( 205.2391015854675516, 275.1624436846170738, -14.01434138479280911 ) ) ;
#40563 = CARTESIAN_POINT ( 'NONE',  ( 106.4801018922090066, 232.2833772461660544, -9.188101187500095079 ) ) ;
#40564 = CARTESIAN_POINT ( 'NONE',  ( 199.0746189151364831, 265.2438329385483939, 1.559867394473611002 ) ) ;
#40565 = EDGE_LOOP ( 'NONE', ( #88723, #12446, #66970, #88419 ) ) ;
#40566 = CARTESIAN_POINT ( 'NONE',  ( 161.7243182998967939, 267.0551689734765546, 16.50076583471866343 ) ) ;
#40567 = ORIENTED_EDGE ( 'NONE', *, *, #88010, .T. ) ;
#40568 = CARTESIAN_POINT ( 'NONE',  ( 34.69977369993912220, 22.96004757982091959, -5.678558825948276656 ) ) ;
#40569 = CARTESIAN_POINT ( 'NONE',  ( 82.57480368249606784, 41.04376301281222794, 1.111617510708536205 ) ) ;
#40570 = CARTESIAN_POINT ( 'NONE',  ( 78.55309808138584060, 47.92462935717776418, -14.48522603925180796 ) ) ;
#40571 = CARTESIAN_POINT ( 'NONE',  ( 59.55252387252222945, 199.0643266524159856, -9.188101187500093303 ) ) ;
#40572 = CARTESIAN_POINT ( 'NONE',  ( 73.78595477147815984, 68.43622263357737268, 11.45456581244437011 ) ) ;
#40573 = CARTESIAN_POINT ( 'NONE',  ( 191.1489696025915919, 299.5672681643093256, 8.892130899335590755 ) ) ;
#40574 = DIRECTION ( 'NONE',  ( -0.8660254037844387076, -0.4999999999999998890, -0.000000000000000000 ) ) ;
#40575 = CARTESIAN_POINT ( 'NONE',  ( 176.2720603235588612, 273.0790378244862495, 17.50981446612852821 ) ) ;
#40576 = VERTEX_POINT ( 'NONE', #63040 ) ;
#40577 = EDGE_CURVE ( 'NONE', #57230, #80767, #53184, .T. ) ;
#40578 = CARTESIAN_POINT ( 'NONE',  ( 75.66128580626863709, 58.22407134023451647, -16.00779004018875895 ) ) ;
#40579 = DIRECTION ( 'NONE',  ( 0.000000000000000000, -0.5906904945688825626, -0.8068982213550659477 ) ) ;
#40580 = CARTESIAN_POINT ( 'NONE',  ( 189.8763472015711216, 301.7715148217271803, -0.1184663095182975079 ) ) ;
#40581 = ORIENTED_EDGE ( 'NONE', *, *, #13400, .T. ) ;
#40582 = CARTESIAN_POINT ( 'NONE',  ( 175.4182666330609095, 261.1119833641568562, -14.60109906219532228 ) ) ;
#40583 = CARTESIAN_POINT ( 'NONE',  ( 71.63782333154907178, 69.86052725181824030, -7.572626888899040232 ) ) ;
#40584 = CARTESIAN_POINT ( 'NONE',  ( 161.1492466472929266, 251.5283125358769212, -13.33353587056634915 ) ) ;
#40585 = CARTESIAN_POINT ( 'NONE',  ( 192.5143468344189728, 297.2023654272867361, -12.06830393602581530 ) ) ;
#40586 = EDGE_CURVE ( 'NONE', #39956, #80413, #33660, .T. ) ;
#40587 = EDGE_CURVE ( 'NONE', #82833, #57607, #93984, .T. ) ;
#40588 = CARTESIAN_POINT ( 'NONE',  ( 149.6071296322179194, 271.5198456328920997, 12.75640156477042453 ) ) ;
#40589 = CARTESIAN_POINT ( 'NONE',  ( 180.0263293189807143, 270.7602331593356553, 17.37738868372918333 ) ) ;
#40590 = CARTESIAN_POINT ( 'NONE',  ( 83.61201429516752626, 42.51031818454811884, -6.362242280625504343 ) ) ;
#40591 = CARTESIAN_POINT ( 'NONE',  ( 67.54027896650161722, 66.67046411983839960, 8.643862525530476404 ) ) ;
#40592 = CARTESIAN_POINT ( 'NONE',  ( 71.32056415648651182, 65.32475367386736309, -12.23164579019822185 ) ) ;
#40593 = FACE_OUTER_BOUND ( 'NONE', #35977, .T. ) ;
#40594 = ADVANCED_FACE ( 'NONE', ( #1762 ), #48914, .F. ) ;
#40595 = CARTESIAN_POINT ( 'NONE',  ( 113.3268549190559753, 245.4244531367911293, -4.594050593750046652 ) ) ;
#40596 = EDGE_LOOP ( 'NONE', ( #89140, #18220, #15802, #86894 ) ) ;
#40597 = CARTESIAN_POINT ( 'NONE',  ( 147.2999496562918296, 275.5159985734018164, -0.1418322875769767455 ) ) ;
#40598 = CARTESIAN_POINT ( 'NONE',  ( -19.65312891409030271, 93.06504152958497400, -10.00000000000000888 ) ) ;
#40599 = EDGE_CURVE ( 'NONE', #91566, #50040, #50004, .T. ) ;
#40600 = ADVANCED_FACE ( 'NONE', ( #44216 ), #81287, .T. ) ;
#40601 = CARTESIAN_POINT ( 'NONE',  ( 155.4661767250933622, 261.3716783840932294, -17.10192542004562810 ) ) ;
#40602 = CARTESIAN_POINT ( 'NONE',  ( 163.9149533033796047, 246.7379680887036670, 7.273005089308705706 ) ) ;
#40603 = CARTESIAN_POINT ( 'NONE',  ( 83.67142796774817270, 51.47602654951222689, -14.37994367775212012 ) ) ;
#40604 = CIRCLE ( 'NONE', #32590, 0.1418229129681557177 ) ;
#40605 = CARTESIAN_POINT ( 'NONE',  ( 177.4875709022480805, 255.0843569672325373, 4.885038851980863406 ) ) ;
#40606 = EDGE_LOOP ( 'NONE', ( #92715, #26510, #40426, #67481 ) ) ;
#40607 = CARTESIAN_POINT ( 'NONE',  ( 172.3986314675530309, 263.7922717222033384, -16.89442142407995107 ) ) ;
#40608 = B_SPLINE_CURVE_WITH_KNOTS ( 'NONE', 3,
 ( #36512, #45112, #83662, #14224 ),
 .UNSPECIFIED., .F., .F.,
 ( 4, 4 ),
 ( 0.009430154199042148702, 0.01486991593141949626 ),
 .UNSPECIFIED. ) ;
#40609 = CARTESIAN_POINT ( 'NONE',  ( 158.5191741753731094, 275.0318726483118894, -12.49859467851711514 ) ) ;
#40610 = CARTESIAN_POINT ( 'NONE',  ( 185.6923914186591276, 262.0522634787053562, 9.806237466387484503 ) ) ;
#40611 = CARTESIAN_POINT ( 'NONE',  ( 206.0977829604818510, 273.6751639155793896, -9.820003938885891515 ) ) ;
#40612 = CARTESIAN_POINT ( 'NONE',  ( 131.6216415740022398, 255.9869531367911009, 4.594050593750046652 ) ) ;
#40613 = CARTESIAN_POINT ( 'NONE',  ( 198.7136873185829984, 286.4647927352960437, -18.57144721070432070 ) ) ;
#40614 = CARTESIAN_POINT ( 'NONE',  ( 190.1413301607522044, 298.8649611522849341, -8.184056379218567656 ) ) ;
#40615 = FACE_OUTER_BOUND ( 'NONE', #21620, .T. ) ;
#40616 = CARTESIAN_POINT ( 'NONE',  ( 63.55789136502527015, 201.3768266524160140, 9.188101187500098632 ) ) ;
#40617 = CARTESIAN_POINT ( 'NONE',  ( 85.52974044692305711, 48.30270382619246305, -11.71869337694238133 ) ) ;
#40618 = CARTESIAN_POINT ( 'NONE',  ( -25.62627769214125451, 24.57763045674671076, -10.00000000000000000 ) ) ;
#40619 = CARTESIAN_POINT ( 'NONE',  ( 80.44297273216874089, 44.73620253192707708, -11.65665792466250039 ) ) ;
#40620 = CARTESIAN_POINT ( 'NONE',  ( 171.6722295479746947, 260.3874344878792044, 14.68526897012709220 ) ) ;
#40621 = CARTESIAN_POINT ( 'NONE',  ( 155.0819613845161768, 280.3159068740167186, -0.8634000510104499204 ) ) ;
#40622 = CARTESIAN_POINT ( 'NONE',  ( 178.8456940037896743, 291.7693823845650059, -6.757125974697903992 ) ) ;
#40623 = B_SPLINE_CURVE_WITH_KNOTS ( 'NONE', 3,
 ( #89740, #58769, #76849, #22664, #12203, #20303, #69247, #45932, #98307, #97813, #28381, #58284, #59260, #51701, #13208, #23135, #84496, #7446, #74518, #100175, #27889, #30761, #67381, #19810, #82649, #28897, #59775, #61641, #92591, #89261, #54030, #84986, #15531, #43066, #4593, #46431, #51177, #77360, #35488, #7965, #5097, #38838, #69744, #50677, #35978, #9462 ),
 .UNSPECIFIED., .F., .F.,
 ( 4, 1, 1, 1, 2, 2, 1, 1, 1, 2, 2, 1, 1, 2, 2, 1, 1, 2, 2, 1, 1, 2, 2, 1, 2, 2, 1, 2, 2, 4 ),
 ( 0.000000000000000000, 0.06249999999997488120, 0.09374999999996232181, 0.1093749999999545780, 0.1171874999999524686, 0.1249999999999503730, 0.1874999999999391320, 0.2187499999999332756, 0.2343749999999326095, 0.2421874999999322764, 0.2499999999999319433, 0.3124999999999383826, 0.3437499999999411027, 0.3593749999999437672, 0.3749999999999464317, 0.4374999999999532041, 0.4687499999999584221, 0.4843749999999609201, 0.4999999999999634737, 0.5624999999999631406, 0.5937499999999624745, 0.6093749999999615863, 0.6249999999999606981, 0.6874999999999623634, 0.7187499999999655831, 0.7499999999999688027, 0.8124999999999790168, 0.8437499999999847899, 0.8749999999999904521, 1.000000000000000000 ),
 .UNSPECIFIED. ) ;
#40624 = CARTESIAN_POINT ( 'NONE',  ( 203.3349860717029571, 278.4604684979374838, -16.59553970625579566 ) ) ;
#40625 = CARTESIAN_POINT ( 'NONE',  ( 157.2843776208655697, 270.8446288838524652, -14.72886913550468257 ) ) ;
#40626 = CARTESIAN_POINT ( 'NONE',  ( 120.7424577590100654, 230.5177522451417929, 5.000000000000051514 ) ) ;
#40627 = CARTESIAN_POINT ( 'NONE',  ( 79.56977700121861119, 52.24079475247017257, -15.41399356243466379 ) ) ;
#40628 = ORIENTED_EDGE ( 'NONE', *, *, #93507, .F. ) ;
#40629 = EDGE_CURVE ( 'NONE', #25829, #6621, #93371, .T. ) ;
#40630 = CARTESIAN_POINT ( 'NONE',  ( 190.5154909595809727, 300.6644853595138329, -0.04129855346138300298 ) ) ;
#40631 = B_SPLINE_CURVE_WITH_KNOTS ( 'NONE', 3,
 ( #19516, #67066, #81329, #51368 ),
 .UNSPECIFIED., .F., .F.,
 ( 4, 4 ),
 ( 0.008479649949678834397, 0.01357937252561114416 ),
 .UNSPECIFIED. ) ;
#40632 = B_SPLINE_CURVE_WITH_KNOTS ( 'NONE', 3,
 ( #78703, #53864, #84825, #46261, #93928, #7790, #32071 ),
 .UNSPECIFIED., .F., .F.,
 ( 4, 3, 4 ),
 ( 6.109341443789230770E-15, 0.001498044977023242066, 0.004247078789804528687 ),
 .UNSPECIFIED. ) ;
#40633 = CARTESIAN_POINT ( 'NONE',  ( 35.03300607999280913, 191.0333772461660544, 9.188101187500095079 ) ) ;
#40634 = CARTESIAN_POINT ( 'NONE',  ( 11.95823279523498073, 29.83705186507753027, 3.090169943749475401 ) ) ;
#40635 = CARTESIAN_POINT ( 'NONE',  ( 43.57052534665006505, 184.4155109091896065, 2.679491924311254714 ) ) ;
#40636 = CARTESIAN_POINT ( 'NONE',  ( 188.7612856390439333, 290.4500619787207825, -14.79637974347269491 ) ) ;
#40637 = CARTESIAN_POINT ( 'NONE',  ( 71.86822536019646179, 59.56647301316700549, -15.73804542241091475 ) ) ;
#40638 = CARTESIAN_POINT ( 'NONE',  ( 66.46590124120757537, 67.88977592199039179, -6.664539190546268976 ) ) ;
#40640 = CARTESIAN_POINT ( 'NONE',  ( 59.32682287396359300, 198.3927522451418213, 10.00000000000009592 ) ) ;
#40639 = CARTESIAN_POINT ( 'NONE',  ( 46.80869107419874098, 110.6443039040113092, -10.00000000000000000 ) ) ;
#40641 = CARTESIAN_POINT ( 'NONE',  ( 128.4024327899592208, 233.3932355074535678, -2.679491924311248496 ) ) ;
#40642 = CARTESIAN_POINT ( 'NONE',  ( 184.3152199276001966, 257.8157294273448201, 1.347602273921576499 ) ) ;
#40643 = CARTESIAN_POINT ( 'NONE',  ( 157.1850763439666139, 258.3944569110938687, -16.98181238659443437 ) ) ;
#40644 = PLANE ( 'NONE',  #32058 ) ;
#40645 = ORIENTED_EDGE ( 'NONE', *, *, #36136, .T. ) ;
#40646 = CARTESIAN_POINT ( 'NONE',  ( 28.67313202272483252, 177.3615022471902023, 5.000000000000051514 ) ) ;
#40647 = CARTESIAN_POINT ( 'NONE',  ( 147.7245617474428911, 256.0958772461660828, -9.188101187500095079 ) ) ;
#40648 = CARTESIAN_POINT ( 'NONE',  ( 202.6560281492536717, 279.6364581158209717, 17.15553667345918853 ) ) ;
#40649 = CARTESIAN_POINT ( 'NONE',  ( 148.9967968810750563, 247.6423013555410080, -4.594050593750043987 ) ) ;
#40650 = CARTESIAN_POINT ( 'NONE',  ( 39.71070620960689723, 31.43085787977766898, -9.188101187500008038 ) ) ;
#40652 = CARTESIAN_POINT ( 'NONE',  ( 170.4714877815671343, 263.5862471893055954, 15.80051778782658900 ) ) ;
#40651 = CARTESIAN_POINT ( 'NONE',  ( -13.11024591527723615, 6.000000000000000000, -32.50000000000017053 ) ) ;
#40653 = CARTESIAN_POINT ( 'NONE',  ( 192.4202172926039793, 297.3654025762033370, 10.98569444949570872 ) ) ;
#40654 = CARTESIAN_POINT ( 'NONE',  ( 35.02453322635827959, 23.14754757982091959, -5.678558825948276656 ) ) ;
#40655 = CARTESIAN_POINT ( 'NONE',  ( 164.2545401858843945, 246.1497863546213978, 2.275217130759496609 ) ) ;
#40656 = ADVANCED_FACE ( 'NONE', ( #66043 ), #27054, .F. ) ;
#40657 = CARTESIAN_POINT ( 'NONE',  ( 77.72205534048291042, 61.52847525230063042, 16.09962475150207339 ) ) ;
#40658 = CARTESIAN_POINT ( 'NONE',  ( 65.83236371457655878, 68.94654938641845376, 2.326923034581525940 ) ) ;
#40659 = ORIENTED_EDGE ( 'NONE', *, *, #67907, .T. ) ;
#40660 = CARTESIAN_POINT ( 'NONE',  ( 193.2752197284765998, 263.9480352582601768, 7.898392093415175452 ) ) ;
#40661 = CARTESIAN_POINT ( 'NONE',  ( 55.77019854693759271, 214.5530062829863311, -4.648177544792955347E-16 ) ) ;
#40662 = CARTESIAN_POINT ( 'NONE',  ( 15.30080465516770616, 11.76004757982088300, 5.678558825948272215 ) ) ;
#40663 = CARTESIAN_POINT ( 'NONE',  ( 166.4691412992503672, 285.8895934590825050, 0.4981257345838445705 ) ) ;
#40664 = CARTESIAN_POINT ( 'NONE',  ( 10.03310832875943603, 27.83396525600388571, -2.839279412974133887 ) ) ;
#40665 = CARTESIAN_POINT ( 'NONE',  ( 160.4469838632686844, 252.7446673580718368, 14.71213094057149995 ) ) ;
#40666 = CARTESIAN_POINT ( 'NONE',  ( 84.83352707183692587, 50.23671165375215253, -13.78554283518410095 ) ) ;
#40667 = CARTESIAN_POINT ( 'NONE',  ( 159.2289198208967775, 254.8544161663325838, -15.88961297684315888 ) ) ;
#40668 = ADVANCED_FACE ( 'NONE', ( #83771 ), #52814, .T. ) ;
#40669 = VERTEX_POINT ( 'NONE', #92366 ) ;
#40670 = CYLINDRICAL_SURFACE ( 'NONE', #79759, 10.00000000000010658 ) ;
#40671 = CARTESIAN_POINT ( 'NONE',  ( 164.9836323268835940, 244.8869617230113249, -2.696511969808454534 ) ) ;
#40672 = CARTESIAN_POINT ( 'NONE',  ( 66.27522152577653003, 68.24883630604136897, 4.052617218417564615 ) ) ;
#40673 = ADVANCED_FACE ( 'NONE', ( #14332 ), #83620, .T. ) ;
#40674 = CARTESIAN_POINT ( 'NONE',  ( 207.6523394534040392, 270.9825930866021508, -2.115019688068903392 ) ) ;
#40675 = CARTESIAN_POINT ( 'NONE',  ( 194.1493756275458793, 294.3704124857528655, 13.94613522129020744 ) ) ;
#40676 = ORIENTED_EDGE ( 'NONE', *, *, #45585, .F. ) ;
#40677 = VERTEX_POINT ( 'NONE', #41104 ) ;
#40678 = CARTESIAN_POINT ( 'NONE',  ( 157.0110656778546740, 277.1938971196430543, -9.979977716902725504 ) ) ;
#40679 = CARTESIAN_POINT ( 'NONE',  ( 86.00254776313695970, 47.63876908572450475, 10.87982004645334122 ) ) ;
#40680 = EDGE_LOOP ( 'NONE', ( #4444, #93383, #71977, #72397 ) ) ;
#40681 = CARTESIAN_POINT ( 'NONE',  ( 40.70814378237798081, 60.14496435084704018, -10.00000000000000000 ) ) ;
#40682 = CARTESIAN_POINT ( 'NONE',  ( 188.5140216088474006, 298.0167532018325005, 7.839324137471839649 ) ) ;
#40683 = ORIENTED_EDGE ( 'NONE', *, *, #12801, .T. ) ;
#40684 = CARTESIAN_POINT ( 'NONE',  ( 78.37845639280004661, 61.47534692751145968, -15.83465071172797067 ) ) ;
#40685 = CARTESIAN_POINT ( 'NONE',  ( 79.18361146787275118, 59.08720699360743112, -16.21979195788916783 ) ) ;
#40686 = CARTESIAN_POINT ( 'NONE',  ( 10.82157445631582249, 29.18080186712591839, 3.090169943749475401 ) ) ;
#40687 = ORIENTED_EDGE ( 'NONE', *, *, #79519, .F. ) ;
#40688 = CARTESIAN_POINT ( 'NONE',  ( 200.3414094930810165, 283.6454952284590263, 16.87912319229835489 ) ) ;
#40689 = LINE ( 'NONE', #68724, #25530 ) ;
#40690 = CARTESIAN_POINT ( 'NONE',  ( 191.2729698983822288, 299.3524933518466469, 8.871011392605806734 ) ) ;
#40691 = CARTESIAN_POINT ( 'NONE',  ( 151.4273961969814764, 275.0250855714808154, -8.568716987504124916 ) ) ;
#40692 = ORIENTED_EDGE ( 'NONE', *, *, #92076, .T. ) ;
#40693 = CARTESIAN_POINT ( 'NONE',  ( 170.6620473226114143, 255.5658883142887703, -11.58147698829965222 ) ) ;
#40694 = CARTESIAN_POINT ( 'NONE',  ( 163.1691520398773321, 248.0297337694385931, 11.21816141384514331 ) ) ;
#40695 = VERTEX_POINT ( 'NONE', #72555 ) ;
#40696 = VERTEX_POINT ( 'NONE', #56817 ) ;
#40697 = CARTESIAN_POINT ( 'NONE',  ( 79.91647412519343163, 45.34541341733537934, 11.77874049927093658 ) ) ;
#40698 = ORIENTED_EDGE ( 'NONE', *, *, #55203, .F. ) ;
#40699 = CARTESIAN_POINT ( 'NONE',  ( 161.1561989937922021, 271.1185073049681478, 16.16522359423900923 ) ) ;
#40700 = ORIENTED_EDGE ( 'NONE', *, *, #89795, .T. ) ;
#40701 =( BOUNDED_CURVE ( )  B_SPLINE_CURVE ( 2, ( #21991, #13417, #43785, #98014, #68090, #5308, #7285, #20517, #13897 ),
 .UNSPECIFIED., .F., .T. ) 
 B_SPLINE_CURVE_WITH_KNOTS ( ( 3, 2, 2, 2, 3 ),
 ( 0.9717741935483871218, 0.9731182795698924970, 0.9758064516129032473, 0.9784946236559139976, 0.9798387096774193727 ),
 .UNSPECIFIED. ) 
 CURVE ( )  GEOMETRIC_REPRESENTATION_ITEM ( )  RATIONAL_B_SPLINE_CURVE ( ( 0.9330127018922194093, 0.9330127018922194093, 1.000000000000000000, 0.8660254037844387076, 1.000000000000000000, 0.8660254037844387076, 1.000000000000000000, 0.9330127018922194093, 0.9330127018922194093 ) ) 
 REPRESENTATION_ITEM ( '' )  );
#40702 = EDGE_CURVE ( 'NONE', #35306, #2734, #48741, .T. ) ;
#40703 = CARTESIAN_POINT ( 'NONE',  ( 81.53569239047196504, 44.59779901518734846, 10.21677624337819346 ) ) ;
#40704 = DIRECTION ( 'NONE',  ( 0.000000000000000000, -1.000000000000000000, 0.000000000000000000 ) ) ;
#40706 = CARTESIAN_POINT ( 'NONE',  ( 72.08205655898075292, 70.58418997119434835, 6.795652346931509769 ) ) ;
#40705 = B_SPLINE_CURVE_WITH_KNOTS ( 'NONE', 3,
 ( #18716, #86664, #26314, #84773, #49598, #87181, #72936, #94244, #95260, #71922, #3527, #80047, #17196, #40491, #71421, #48099, #94738, #56187, #25300, #95762, #57189, #48617, #18218, #1525, #79040, #88168, #79556, #25826, #34404, #10111, #2524, #10614, #53809, #15309, #72435, #77126, #7732, #38620, #52091, #4500, #90139, #42483, #59680, #65789 ),
 .UNSPECIFIED., .F., .F.,
 ( 4, 2, 2, 2, 2, 2, 2, 2, 2, 2, 2, 2, 2, 2, 2, 2, 2, 2, 2, 2, 2, 4 ),
 ( 0.001166255102719954443, 0.001645796290616598646, 0.002125337478513243065, 0.002365108072461565708, 0.002604878666409887918, 0.002724763963384048589, 0.002844649260358210127, 0.002964534557332370798, 0.003084419854306532337, 0.003563961042203122112, 0.004043502230099711020, 0.005002584605892812508, 0.005961666981685913996, 0.006441208169582427444, 0.006920749357478940891, 0.007040634654453109369, 0.007100577302940112509, 0.007160519951427115649, 0.007400290545375051883, 0.007879831733270893993, 0.008359372921166736969, 0.008838914109062578212 ),
 .UNSPECIFIED. ) ;
#40707 = CARTESIAN_POINT ( 'NONE',  ( 192.0332533962074706, 298.0356437054567778, 11.70630383928353346 ) ) ;
#40708 = CARTESIAN_POINT ( 'NONE',  ( 82.68398936210410000, 53.28103025482077015, -15.29235669276918763 ) ) ;
#40709 = CARTESIAN_POINT ( 'NONE',  ( 123.0902549634681407, 230.3262482093457777, 3.021315404115420679E-15 ) ) ;
#40710 = VERTEX_POINT ( 'NONE', #16818 ) ;
#40711 = DIRECTION ( 'NONE',  ( -0.000000000000000000, -1.000000000000000000, -0.000000000000000000 ) ) ;
#40712 = CARTESIAN_POINT ( 'NONE',  ( 23.32475077058400004, 14.26216523072494446, -2.296566073217252530E-15 ) ) ;
#40713 = CARTESIAN_POINT ( 'NONE',  ( 164.7762319088960794, 245.2461897844768828, 2.994040459560653122 ) ) ;
#40714 = CARTESIAN_POINT ( 'NONE',  ( 190.3443929803903814, 298.9608357525441420, -8.219721500574586059 ) ) ;
#40716 = ORIENTED_EDGE ( 'NONE', *, *, #3717, .F. ) ;
#40715 = CARTESIAN_POINT ( 'NONE',  ( 207.0309969265819063, 271.4803781728614354, 5.109250008308237945 ) ) ;
#40717 = ORIENTED_EDGE ( 'NONE', *, *, #72071, .T. ) ;
#40718 = CARTESIAN_POINT ( 'NONE',  ( 168.4288024578681302, 257.2676070226289085, -14.34928285719503727 ) ) ;
#40719 = EDGE_CURVE ( 'NONE', #82888, #73927, #72925, .T. ) ;
#40720 = DIRECTION ( 'NONE',  ( -0.000000000000000000, -0.000000000000000000, 1.000000000000000000 ) ) ;
#40721 = CARTESIAN_POINT ( 'NONE',  ( 161.7910648966377209, 250.4166507187868831, 13.19274492748169436 ) ) ;
#40722 = CARTESIAN_POINT ( 'NONE',  ( 190.9750444319660119, 261.6428408136690109, -0.08634532216184034881 ) ) ;
#40723 = ORIENTED_EDGE ( 'NONE', *, *, #36321, .T. ) ;
#40724 = CARTESIAN_POINT ( 'NONE',  ( 67.16327201103491973, 67.73731889023999031, 6.573435314091262249 ) ) ;
#40725 = CARTESIAN_POINT ( 'NONE',  ( 139.8153705705071843, 239.9824982072973967, 3.021315404115420679E-15 ) ) ;
#40726 = CARTESIAN_POINT ( 'NONE',  ( 207.6727254509676186, 270.9472835030587703, 7.315149605389819953 ) ) ;
#40727 = CARTESIAN_POINT ( 'NONE',  ( 21.07736754015091662, 169.6427522451417644, 1.119607411625061291E-15 ) ) ;
#40728 = CARTESIAN_POINT ( 'NONE',  ( 96.71051312758956442, 217.4548013555409511, -4.594050593750042211 ) ) ;
#40729 = CARTESIAN_POINT ( 'NONE',  ( 82.35941855622118624, 40.93148445005448366, -1.241598412671953922 ) ) ;
#40730 = CARTESIAN_POINT ( 'NONE',  ( 90.43156862655462191, 233.0177522451419350, 5.000000000000046185 ) ) ;
#40731 = CARTESIAN_POINT ( 'NONE',  ( 207.9670239186021377, 270.4375436045261836, 3.151456135821919968 ) ) ;
#40732 = EDGE_CURVE ( 'NONE', #94679, #23520, #24918, .T. ) ;
#40734 = CYLINDRICAL_SURFACE ( 'NONE', #88554, 10.00000000000010658 ) ;
#40733 = CARTESIAN_POINT ( 'NONE',  ( -0.2035760843690503918, 176.8149278399160949, -9.188101187500095079 ) ) ;
#40735 = CARTESIAN_POINT ( 'NONE',  ( 200.7079229450794173, 283.0106753079404029, 16.90512463913211505 ) ) ;
#40736 = ORIENTED_EDGE ( 'NONE', *, *, #84876, .T. ) ;
#40737 = ORIENTED_EDGE ( 'NONE', *, *, #52182, .F. ) ;
#40738 = DIRECTION ( 'NONE',  ( -0.4999999999999998890, 0.8660254037844387076, 0.000000000000000000 ) ) ;
#40739 = CARTESIAN_POINT ( 'NONE',  ( 67.05324003527370280, 68.69434906313091460, 4.069319704320632169 ) ) ;
#40740 = CARTESIAN_POINT ( 'NONE',  ( 83.25380727528489899, 42.56249626881286474, 5.709386246556279687 ) ) ;
#40741 = CARTESIAN_POINT ( 'NONE',  ( 161.8935665241663457, 250.2391126920490194, -13.69501063978231770 ) ) ;
#40742 = CARTESIAN_POINT ( 'NONE',  ( 182.9576018746647890, 284.4981050466655006, 14.97526635527638739 ) ) ;
#40743 = CARTESIAN_POINT ( 'NONE',  ( 74.11971290936233459, 68.38772044953262252, -11.66991619212280895 ) ) ;
#40744 = CARTESIAN_POINT ( 'NONE',  ( 26.10194555558327778, 192.0024278399160949, -9.188101187500093303 ) ) ;
#40745 = CARTESIAN_POINT ( 'NONE',  ( 83.57553417992789946, 212.3927522451417929, -10.00000000000009059 ) ) ;
#40746 = CARTESIAN_POINT ( 'NONE',  ( 92.25929090966846502, 235.6199935810940929, 2.679491924311251605 ) ) ;
#40747 = ORIENTED_EDGE ( 'NONE', *, *, #8507, .F. ) ;
#40748 = CARTESIAN_POINT ( 'NONE',  ( 82.78588454431675814, 44.52977094881507725, 9.342758750263890022 ) ) ;
#40749 = DIRECTION ( 'NONE',  ( -0.8660254037844380415, -0.5000000000000011102, 0.000000000000000000 ) ) ;
#40750 = CARTESIAN_POINT ( 'NONE',  ( -6.887775800123916881, 157.6423013555410080, -4.594050593750043987 ) ) ;
#40751 = FACE_OUTER_BOUND ( 'NONE', #76015, .T. ) ;
#40752 = CARTESIAN_POINT ( 'NONE',  ( 207.8431546909062320, 270.6520914003897360, -6.441273666418043220 ) ) ;
#40753 = CARTESIAN_POINT ( 'NONE',  ( 192.0969986600162827, 271.0201763999182845, -15.22553433325905736 ) ) ;
#40754 = CARTESIAN_POINT ( 'NONE',  ( 148.2670916631250861, 273.8408594794321971, -7.980554973576580835 ) ) ;
#40755 = CARTESIAN_POINT ( 'NONE',  ( -11.40312891409031693, 78.77562236714182120, 59.99999999999999289 ) ) ;
#40756 = CARTESIAN_POINT ( 'NONE',  ( 171.4574698082410009, 280.1005400806686225, 15.30362981370621611 ) ) ;
#40757 = CARTESIAN_POINT ( 'NONE',  ( 146.9235493515124062, 276.1679430252639804, 0.7994986043261682607 ) ) ;
#40758 = FACE_OUTER_BOUND ( 'NONE', #38771, .T. ) ;
#40759 = ORIENTED_EDGE ( 'NONE', *, *, #17732, .F. ) ;
#40760 = CARTESIAN_POINT ( 'NONE',  ( 164.4678285797544106, 245.7803600197737524, -6.875991496205872799 ) ) ;
#40761 = DIRECTION ( 'NONE',  ( -0.5346708562974005208, -0.8450603975019800318, 0.000000000000000000 ) ) ;
#40762 = CARTESIAN_POINT ( 'NONE',  ( 110.0256537107753161, 225.1423013555409796, -4.594050593750043987 ) ) ;
#40763 = CARTESIAN_POINT ( 'NONE',  ( 21.85012855468117721, 24.56628583063841376, 9.188101187500006262 ) ) ;
#40764 = FACE_OUTER_BOUND ( 'NONE', #23379, .T. ) ;
#40765 = DIRECTION ( 'NONE',  ( -0.8660254037844387076, -0.4999999999999998890, -0.000000000000000000 ) ) ;
#40767 = DIRECTION ( 'NONE',  ( -0.8035972437015875824, -0.5951734788405910193, 0.000000000000000000 ) ) ;
#40766 = DIRECTION ( 'NONE',  ( -0.000000000000000000, -0.000000000000000000, -1.000000000000000000 ) ) ;
#40768 = CARTESIAN_POINT ( 'NONE',  ( 204.3238350981471001, 272.7781662703540064, -9.746153380280240697 ) ) ;
#40769 = CARTESIAN_POINT ( 'NONE',  ( 190.0900669226457751, 261.8932147952297669, -4.414057574442162846 ) ) ;
#40770 = CARTESIAN_POINT ( 'NONE',  ( 148.9194629746633893, 272.7109192224475009, -12.27648025871169679 ) ) ;
#40771 = CARTESIAN_POINT ( 'NONE',  ( 110.7831656154889970, 234.7677522451418497, 10.00000000000009592 ) ) ;
#40772 = CARTESIAN_POINT ( 'NONE',  ( 203.5517807763935991, 276.4131063546051337, 14.32831804246049678 ) ) ;
#40773 = CARTESIAN_POINT ( 'NONE',  ( 86.28285115951177886, 47.67076295942541009, 10.74768692570409279 ) ) ;
#40774 = ORIENTED_EDGE ( 'NONE', *, *, #21881, .F. ) ;
#40775 = CARTESIAN_POINT ( 'NONE',  ( 46.22371820283660782, 112.7232458147606451, -10.00000000000000000 ) ) ;
#40776 = CARTESIAN_POINT ( 'NONE',  ( 16.98118013718471886, 32.73705186507753950, -3.090169943749475845 ) ) ;
#40777 = CARTESIAN_POINT ( 'NONE',  ( 167.9438064097205370, 271.4634641811414895, -17.49863926106802126 ) ) ;
#40778 = VERTEX_POINT ( 'NONE', #34522 ) ;
#40779 = B_SPLINE_SURFACE_WITH_KNOTS ( 'NONE', 3, 1, ( 
 ( #64535, #8824 ),
 ( #79778, #80276 ),
 ( #64029, #94971 ),
 ( #87419, #10343 ),
 ( #72149, #16919 ),
 ( #2754, #33644 ),
 ( #95494, #78243 ),
 ( #47808, #1749 ),
 ( #56916, #18447 ),
 ( #94465, #32116 ),
 ( #86892, #49336 ),
 ( #63025, #93970 ),
 ( #32628, #63525 ),
 ( #17426, #57415 ),
 ( #34622, #50320 ),
 ( #4219, #12849 ),
 ( #66520, #36603 ),
 ( #80787, #81763 ),
 ( #20946, #51304 ),
 ( #42215, #97447 ),
 ( #82276, #59391 ),
 ( #44201, #81272 ),
 ( #36105, #88902 ),
 ( #43708, #12337 ),
 ( #11846, #74650 ),
 ( #73635, #18950 ),
 ( #28017, #20436 ),
 ( #42703, #28510 ),
 ( #65522, #58891 ),
 ( #35117, #50814 ),
 ( #90367, #96471 ),
 ( #43202, #82769 ),
 ( #5714, #5227 ),
 ( #11361, #27039 ) ),
 .UNSPECIFIED., .T., .F., .F.,
 ( 4, 2, 2, 2, 2, 2, 2, 2, 2, 2, 2, 2, 2, 2, 2, 2, 4 ),
 ( 2, 2 ),
 ( 0.000000000000000000, 0.06250000000000000000, 0.1250000000000000000, 0.1875000000000000000, 0.2500000000000000000, 0.3125000000000000000, 0.3750000000000000000, 0.4375000000000000000, 0.5000000000000000000, 0.5625000000000000000, 0.6250000000000000000, 0.6875000000000000000, 0.7500000000000000000, 0.8125000000000000000, 0.8750000000000000000, 0.9375000000000000000, 1.000000000000000000 ),
 ( 0.000000000000000000, 1.000000000000000000 ),
 .UNSPECIFIED. ) ;
#40780 = EDGE_CURVE ( 'NONE', #91328, #99484, #88558, .T. ) ;
#40781 = CARTESIAN_POINT ( 'NONE',  ( 198.1925917153872376, 271.8148388623765186, 12.14180242448621527 ) ) ;
#40782 = CARTESIAN_POINT ( 'NONE',  ( 83.87116762653428736, 51.60433200805344711, -14.38557393531113071 ) ) ;
#40783 = ADVANCED_FACE ( 'NONE', ( #49719 ), #65421, .T. ) ;
#40784 = CARTESIAN_POINT ( 'NONE',  ( -64.74139798177010618, 41.16849083240310847, -10.00000000000000000 ) ) ;
#40785 = CARTESIAN_POINT ( 'NONE',  ( 74.89921650030801459, 53.29654407186357901, -16.52566481002074639 ) ) ;
#40786 = CARTESIAN_POINT ( 'NONE',  ( 192.7259387352017939, 296.8358775046606297, 11.24705370801146209 ) ) ;
#40787 = ORIENTED_EDGE ( 'NONE', *, *, #51901, .F. ) ;
#40788 = CYLINDRICAL_SURFACE ( 'NONE', #18073, 10.00000000000010658 ) ;
#40789 = ADVANCED_FACE ( 'NONE', ( #91983 ), #99546, .T. ) ;
#40790 = CARTESIAN_POINT ( 'NONE',  ( 38.30580752471379213, 37.51421378149922958, -9.188101187500004485 ) ) ;
#40791 = CARTESIAN_POINT ( 'NONE',  ( 174.1430845602542945, 272.9649943977126441, -16.36010906446035307 ) ) ;
#40792 = ORIENTED_EDGE ( 'NONE', *, *, #53213, .F. ) ;
#40793 = CARTESIAN_POINT ( 'NONE',  ( 77.72825959162678089, 61.57464001967338163, 16.09025617263268515 ) ) ;
#40794 = EDGE_CURVE ( 'NONE', #43088, #62301, #61011, .T. ) ;
#40795 = CARTESIAN_POINT ( 'NONE',  ( -22.42236680055709641, 157.8615022471902591, 0.000000000000000000 ) ) ;
#40796 = CARTESIAN_POINT ( 'NONE',  ( 164.4430760075033788, 246.2065693058222564, -1.743745055932603538 ) ) ;
#40797 = ORIENTED_EDGE ( 'NONE', *, *, #28353, .F. ) ;
#40798 = CARTESIAN_POINT ( 'NONE',  ( 79.06677544641175359, 59.81915678714237572, 16.49560342610751462 ) ) ;
#40799 = CARTESIAN_POINT ( 'NONE',  ( 187.6671935738553714, 292.4988616513966235, 12.35105147068263065 ) ) ;
#40800 = LINE ( 'NONE', #86989, #30439 ) ;
#40801 = CARTESIAN_POINT ( 'NONE',  ( 83.03630717809630823, 50.34759745827115296, -13.97564751877582090 ) ) ;
#40802 = CARTESIAN_POINT ( 'NONE',  ( 202.9547455376043672, 279.1190644220934018, -15.19669173352461478 ) ) ;
#40803 = VERTEX_POINT ( 'NONE', #76258 ) ;
#40804 = VERTEX_POINT ( 'NONE', #722 ) ;
#40805 = CARTESIAN_POINT ( 'NONE',  ( 178.6928612807282946, 260.5973771377355774, 11.99803804170878863 ) ) ;
#40806 = ORIENTED_EDGE ( 'NONE', *, *, #89458, .F. ) ;
#40807 = CARTESIAN_POINT ( 'NONE',  ( 77.36673626426795636, 49.72045831782982361, -15.49538004450117334 ) ) ;
#40808 = EDGE_LOOP ( 'NONE', ( #77204, #43660, #51150, #73637 ) ) ;
#40809 = CARTESIAN_POINT ( 'NONE',  ( -32.94356256989595977, 94.88921800892812541, 45.19948692389422717 ) ) ;
#40810 = CARTESIAN_POINT ( 'NONE',  ( 79.17960166781870157, 53.06255416066780839, 15.69067566303936445 ) ) ;
#40811 = ORIENTED_EDGE ( 'NONE', *, *, #34268, .T. ) ;
#40812 = DIRECTION ( 'NONE',  ( 0.7490285521785712275, -0.6625377181876315191, 0.000000000000000000 ) ) ;
#40813 = CARTESIAN_POINT ( 'NONE',  ( 190.5561904564986833, 300.5939917630097966, 3.348721477520653966 ) ) ;
#40814 = CARTESIAN_POINT ( 'NONE',  ( 196.7432902728890269, 284.8136100218615070, -17.21513713512148058 ) ) ;
#40815 = DIRECTION ( 'NONE',  ( -0.9404163354663446217, -0.3400251696390308442, 0.000000000000000000 ) ) ;
#40816 = CARTESIAN_POINT ( 'NONE',  ( 201.4520623681621316, 281.7217880192456505, -17.56577389517433119 ) ) ;
#40817 = CARTESIAN_POINT ( 'NONE',  ( 70.80322137413752159, 60.50400129575321273, -14.70302039727343413 ) ) ;
#40818 = CARTESIAN_POINT ( 'NONE',  ( 157.8621261317385915, 281.2061543397735477, 2.756635258921121601 ) ) ;
#40819 = CARTESIAN_POINT ( 'NONE',  ( 121.9060058492368483, 247.3149278399160949, -9.188101187500095079 ) ) ;
#40820 = ORIENTED_EDGE ( 'NONE', *, *, #3660, .F. ) ;
#40822 = PLANE ( 'NONE',  #31782 ) ;
#40821 = B_SPLINE_CURVE_WITH_KNOTS ( 'NONE', 3,
 ( #2877, #96093, #87014, #73258, #3853, #56020, #34736, #65638, #81392, #35240, #66143, #17543, #97091, #5346, #35742, #58528, #74768, #22025, #36227, #28630, #43330, #99053, #20556, #21066, #50933, #66638, #43828, #51943, #82882, #67132, #98054, #82401, #60018, #97567, #12967, #59515, #74276, #20060, #29635, #60508, #51435, #14439, #4860, #90493, #81882, #68125 ),
 .UNSPECIFIED., .F., .F.,
 ( 4, 1, 1, 1, 2, 2, 1, 1, 1, 2, 2, 1, 1, 2, 2, 1, 1, 2, 2, 1, 1, 2, 2, 1, 2, 2, 1, 2, 2, 4 ),
 ( 0.000000000000000000, 0.06249999999999522604, 0.09374999999999183986, 0.1093749999999901468, 0.1171874999999888423, 0.1249999999999875377, 0.1874999999999799050, 0.2187499999999756584, 0.2343749999999725497, 0.2421874999999724387, 0.2499999999999722999, 0.3124999999999747979, 0.3437499999999756306, 0.3593749999999750200, 0.3749999999999744649, 0.4374999999999698019, 0.4687499999999688582, 0.4843749999999679701, 0.4999999999999671374, 0.5624999999999653610, 0.5937499999999638067, 0.6093749999999638067, 0.6249999999999636957, 0.6874999999999688027, 0.7187499999999713562, 0.7499999999999740208, 0.8124999999999810152, 0.8437499999999844569, 0.8749999999999880096, 1.000000000000000000 ),
 .UNSPECIFIED. ) ;
#40823 = B_SPLINE_CURVE_WITH_KNOTS ( 'NONE', 3,
 ( #68076, #75204, #36669, #84814, #67577, #15353, #98999, #38151, #29583, #30579, #7778, #60460, #91415, #90937, #38669, #69572 ),
 .UNSPECIFIED., .F., .F.,
 ( 4, 1, 2, 2, 2, 1, 2, 2, 4 ),
 ( 0.000000000000000000, 0.1249999999999976685, 0.1874999999999974742, 0.2499999999999972800, 0.4999999999999968914, 0.6249999999999961142, 0.6874999999999962252, 0.7499999999999964473, 1.000000000000000000 ),
 .UNSPECIFIED. ) ;
#40824 = CARTESIAN_POINT ( 'NONE',  ( 45.79150443358504674, 28.29860640527296667, -2.839279412974138328 ) ) ;
#40825 = VERTEX_POINT ( 'NONE', #23507 ) ;
#40826 = CARTESIAN_POINT ( 'NONE',  ( 85.71994772693146558, 48.50907089644480408, -12.26219287530961743 ) ) ;
#40827 = CARTESIAN_POINT ( 'NONE',  ( 203.5517529213690295, 276.4076950671145596, 13.56830733209305251 ) ) ;
#40828 = DIRECTION ( 'NONE',  ( 0.8660254037844379305, 0.5000000000000014433, 0.000000000000000000 ) ) ;
#40829 = DIRECTION ( 'NONE',  ( 0.000000000000000000, 0.000000000000000000, 1.000000000000000000 ) ) ;
#40830 = CARTESIAN_POINT ( 'NONE',  ( 192.0519773745460554, 298.0032128236547351, 11.68523422658327249 ) ) ;
#40831 = CARTESIAN_POINT ( 'NONE',  ( 153.3750525283932689, 276.8757596813744044, 7.147645658179857087 ) ) ;
#40832 = LINE ( 'NONE', #62635, #93380 ) ;
#40833 = CARTESIAN_POINT ( 'NONE',  ( 174.3376866340771869, 288.4003068613999972, -10.07124184041177450 ) ) ;
#40834 = CARTESIAN_POINT ( 'NONE',  ( 192.6470520760290981, 292.3461483602033013, -14.37014842569768192 ) ) ;
#40835 = DIRECTION ( 'NONE',  ( 0.000000000000000000, 0.000000000000000000, 1.000000000000000000 ) ) ;
#40836 = ORIENTED_EDGE ( 'NONE', *, *, #77542, .T. ) ;
#40837 = CARTESIAN_POINT ( 'NONE',  ( 147.9133274879049793, 274.4535970048112290, -9.359166267164972908 ) ) ;
#40838 = CARTESIAN_POINT ( 'NONE',  ( 152.5693996133281587, 273.3850609750195417, 11.87574206830028878 ) ) ;
#40839 = ORIENTED_EDGE ( 'NONE', *, *, #32486, .F. ) ;
#40840 = CARTESIAN_POINT ( 'NONE',  ( 47.05668214639808156, 76.45164061169337799, -10.00000000000000000 ) ) ;
#40841 = CARTESIAN_POINT ( 'NONE',  ( 191.0043802832096844, 283.4987559632036778, -16.57480583703641130 ) ) ;
#40842 = CARTESIAN_POINT ( 'NONE',  ( 191.7656802644930849, 298.4990939643267893, -9.391040447064041174 ) ) ;
#40843 = CARTESIAN_POINT ( 'NONE',  ( 149.6877696051026305, 271.3801731027346591, 11.89134584187677390 ) ) ;
#40844 = EDGE_CURVE ( 'NONE', #329, #17646, #63195, .T. ) ;
#40845 = CARTESIAN_POINT ( 'NONE',  ( 202.4017613376760494, 280.0768611521521620, 15.73960524502980540 ) ) ;
#40847 = CARTESIAN_POINT ( 'NONE',  ( 160.9022227064159836, 281.5926560585749598, 6.018336957399161413 ) ) ;
#40846 = CARTESIAN_POINT ( 'NONE',  ( 153.5022104429997398, 269.9741907477366567, 14.95430817309988747 ) ) ;
#40848 = AXIS2_PLACEMENT_3D ( 'NONE', #96923, #5175, #4167 ) ;
#40849 = CARTESIAN_POINT ( 'NONE',  ( 152.8721808860877616, 265.8646109718731623, -17.65676496037632504 ) ) ;
#40850 = EDGE_LOOP ( 'NONE', ( #76497, #72688, #10305, #2369 ) ) ;
#40851 = CARTESIAN_POINT ( 'NONE',  ( 164.6353421851925702, 280.3989608998424501, -11.20704416911448753 ) ) ;
#40852 = CARTESIAN_POINT ( 'NONE',  ( 77.47753981885827557, 60.62937987968794573, -15.85731085967187504 ) ) ;
#40853 = CARTESIAN_POINT ( 'NONE',  ( 193.0512205562391159, 275.6825563886401369, -16.88465587640301280 ) ) ;
#40854 = DIRECTION ( 'NONE',  ( -0.8660254037844387076, -0.4999999999999998890, -0.000000000000000000 ) ) ;
#40855 = AXIS2_PLACEMENT_3D ( 'NONE', #68955, #84703, #15244 ) ;
#40856 = CARTESIAN_POINT ( 'NONE',  ( 14.99168702176358892, 167.9155109091896065, 2.679491924311228512 ) ) ;
#40857 = CARTESIAN_POINT ( 'NONE',  ( 85.36105550139274101, 47.58428912729043958, 11.11794341640556105 ) ) ;
#40858 = CARTESIAN_POINT ( 'NONE',  ( 73.81469611240122219, 68.48838210847161179, 11.42215486908102839 ) ) ;
#40859 = FACE_OUTER_BOUND ( 'NONE', #45181, .T. ) ;
#40860 = CARTESIAN_POINT ( 'NONE',  ( 68.94813988800106586, 70.44622341501073493, 0.2739619411755226386 ) ) ;
#40861 = CARTESIAN_POINT ( 'NONE',  ( -17.68663747114990770, 172.8464784336661353, 1.353441290958777525E-15 ) ) ;
#40862 = CARTESIAN_POINT ( 'NONE',  ( 89.26784699199328088, 222.3458772461660544, 9.188101187500095079 ) ) ;
#40863 = CARTESIAN_POINT ( 'NONE',  ( 155.5211745099813356, 261.2764194263634749, -17.18163098020766810 ) ) ;
#40864 = CARTESIAN_POINT ( 'NONE',  ( 192.4867975473904949, 297.2500821921321972, -13.04960750009181325 ) ) ;
#40865 = CARTESIAN_POINT ( 'NONE',  ( 147.7236348786572933, 275.2192751642206190, 4.007618914242884856 ) ) ;
#40866 = EDGE_CURVE ( 'NONE', #50800, #2973, #22107, .T. ) ;
#40867 = DIRECTION ( 'NONE',  ( 0.4999999999999998890, -0.8660254037844385966, 0.000000000000000000 ) ) ;
#40868 = CARTESIAN_POINT ( 'NONE',  ( 78.49761452932601458, 57.83882379195031831, 16.22345952510868727 ) ) ;
#40869 = CARTESIAN_POINT ( 'NONE',  ( 161.0423214198712856, 281.7177014927175946, 5.594616910120793207 ) ) ;
#40871 = CARTESIAN_POINT ( 'NONE',  ( 162.8480293090835005, 248.5859346546387769, -9.753154585358942086 ) ) ;
#40870 = DIRECTION ( 'NONE',  ( -0.7715546603183444097, -0.6361630342459738685, 0.000000000000000000 ) ) ;
#40872 = CARTESIAN_POINT ( 'NONE',  ( 177.8711684648900757, 290.0939523432613214, 9.786701248066272285 ) ) ;
#40873 = B_SPLINE_CURVE_WITH_KNOTS ( 'NONE', 3,
 ( #69433, #30933, #28955, #61816, #45131, #92768, #85178, #15723, #46626, #77554, #8142, #67435, #16235, #62313, #94770, #78552 ),
 .UNSPECIFIED., .F., .F.,
 ( 4, 1, 2, 2, 2, 1, 2, 2, 4 ),
 ( 0.000000000000000000, 0.1250000000000014155, 0.1875000000000014433, 0.2500000000000014988, 0.5000000000000001110, 0.6249999999999990008, 0.6874999999999993339, 0.7499999999999996669, 1.000000000000000000 ),
 .UNSPECIFIED. ) ;
#40874 = CARTESIAN_POINT ( 'NONE',  ( 151.1237910559533475, 270.8929109891034841, -13.93008610078706688 ) ) ;
#40875 = CARTESIAN_POINT ( 'NONE',  ( 82.29791713453792568, 53.38160488945237603, -15.38503680549501418 ) ) ;
#40876 = CARTESIAN_POINT ( 'NONE',  ( 74.57652347799796644, 55.50245127849832727, -16.60469772587055814 ) ) ;
#40877 = CARTESIAN_POINT ( 'NONE',  ( 71.85396936473564722, 72.11868129461186072, -1.696172015788008247 ) ) ;
#40878 = CARTESIAN_POINT ( 'NONE',  ( 36.84650709099022947, 182.8923013555409796, 4.594050593750050204 ) ) ;
#40879 = CARTESIAN_POINT ( 'NONE',  ( 77.05240863693448716, 63.46827552167501096, -15.45063268884610785 ) ) ;
#40880 = CARTESIAN_POINT ( 'NONE',  ( 70.62149783858335184, 202.3923013555409796, 4.594050593750050204 ) ) ;
#40881 = CARTESIAN_POINT ( 'NONE',  ( 161.1747502674735415, 251.4841389699472529, -13.25152330924089839 ) ) ;
#40882 = CARTESIAN_POINT ( 'NONE',  ( 81.16557949073278166, 51.79492549539191515, -15.46120199680615670 ) ) ;
#40883 = CARTESIAN_POINT ( 'NONE',  ( 165.3184754677606918, 258.9335273930299195, 15.57829592379341044 ) ) ;
#40885 = CARTESIAN_POINT ( 'NONE',  ( 199.9968460962569452, 284.2422965381864515, 16.92744394710046762 ) ) ;
#40884 = CARTESIAN_POINT ( 'NONE',  ( 198.4146594612899719, 286.4472197769862873, -17.06352273131960473 ) ) ;
#40886 = CARTESIAN_POINT ( 'NONE',  ( 173.6170773432991155, 268.4804802943822892, -16.29536237713207569 ) ) ;
#40887 = CARTESIAN_POINT ( 'NONE',  ( 30.51038259252555207, 29.56628583063842441, 9.188101187500006262 ) ) ;
#40888 = LINE ( 'NONE', #48525, #88786 ) ;
#40889 = CARTESIAN_POINT ( 'NONE',  ( 78.76087375241728239, 47.95963633988191077, -13.89607590865744413 ) ) ;
#40890 = ORIENTED_EDGE ( 'NONE', *, *, #98844, .T. ) ;
#40891 = CARTESIAN_POINT ( 'NONE',  ( 14.21828646722447154, 29.18502408145591431, 5.678558825948277544 ) ) ;
#40892 = CARTESIAN_POINT ( 'NONE',  ( 78.52397964811635234, 206.9548013555409796, -4.594050593750042211 ) ) ;
#40893 = CARTESIAN_POINT ( 'NONE',  ( 193.7190926099759736, 281.1151242756019997, 17.77946842270920413 ) ) ;
#40894 = CARTESIAN_POINT ( 'NONE',  ( 169.1636391637144357, 288.4733247442767379, -1.122355453443255602 ) ) ;
#40895 = CARTESIAN_POINT ( 'NONE',  ( -73.66720466879951346, 50.53642055324488780, -10.00000000000000000 ) ) ;
#40896 = LINE ( 'NONE', #71845, #89802 ) ;
#40897 = B_SPLINE_CURVE_WITH_KNOTS ( 'NONE', 3,
 ( #89766, #20336, #64434, #89291 ),
 .UNSPECIFIED., .F., .F.,
 ( 4, 4 ),
 ( 0.02882533845999755637, 0.03798746942113730152 ),
 .UNSPECIFIED. ) ;
#40898 = VERTEX_POINT ( 'NONE', #68129 ) ;
#40899 = FACE_OUTER_BOUND ( 'NONE', #65803, .T. ) ;
#40900 = CARTESIAN_POINT ( 'NONE',  ( 189.7676554596182825, 286.5697828033414112, 16.74390813620514251 ) ) ;
#40901 = CARTESIAN_POINT ( 'NONE',  ( 122.6368883333363584, 251.6115022471903160, -5.000000000000047962 ) ) ;
#40902 = CARTESIAN_POINT ( 'NONE',  ( 161.8811854682448939, 250.2605573099562264, 13.51112293479948789 ) ) ;
#40903 = CARTESIAN_POINT ( 'NONE',  ( 19.15050853525752927, 34.55466486950700045, 7.012934429366973338E-14 ) ) ;
#40904 = ORIENTED_EDGE ( 'NONE', *, *, #90380, .F. ) ;
#40905 = CARTESIAN_POINT ( 'NONE',  ( 188.6573459026649857, 272.6511070077579575, 15.94497187152243356 ) ) ;
#40906 = ORIENTED_EDGE ( 'NONE', *, *, #32915, .F. ) ;
#40907 = CARTESIAN_POINT ( 'NONE',  ( 162.8042930031641049, 248.6616881586264469, 11.14389129512055554 ) ) ;
#40908 = CARTESIAN_POINT ( 'NONE',  ( 70.01283242295176024, 62.80173547756309915, -13.36538303052352283 ) ) ;
#40909 = CARTESIAN_POINT ( 'NONE',  ( 66.92974135600969987, 68.45175875912458707, -4.590911461443917929 ) ) ;
#40910 = ADVANCED_FACE ( 'NONE', ( #69122 ), #14918, .F. ) ;
#40911 = ORIENTED_EDGE ( 'NONE', *, *, #14721, .T. ) ;
#40912 = CYLINDRICAL_SURFACE ( 'NONE', #12648, 70.00000000000002842 ) ;
#40913 = VERTEX_POINT ( 'NONE', #30635 ) ;
#40914 = LINE ( 'NONE', #95187, #65190 ) ;
#40915 = CARTESIAN_POINT ( 'NONE',  ( 164.9101359252495627, 286.5608941336866451, 1.040025780022917790 ) ) ;
#40916 = CARTESIAN_POINT ( 'NONE',  ( 182.8075329105516289, 285.5996758505444291, -15.91971760981349071 ) ) ;
#40917 = AXIS2_PLACEMENT_3D ( 'NONE', #34198, #48396, #79836 ) ;
#40918 = ORIENTED_EDGE ( 'NONE', *, *, #18080, .F. ) ;
#40919 = CARTESIAN_POINT ( 'NONE',  ( 28.99364183777449000, 25.24335787977764767, -9.188101187500008038 ) ) ;
#40920 = CARTESIAN_POINT ( 'NONE',  ( 74.70969265356583833, 66.80295132244255285, -13.14574923971307641 ) ) ;
#40921 = CARTESIAN_POINT ( 'NONE',  ( 80.15338731764678926, 49.08938989525468344, -14.08338104835611482 ) ) ;
#40922 = VECTOR ( 'NONE', #7131, 1000.000000000000114 ) ;
#40923 = CARTESIAN_POINT ( 'NONE',  ( 167.5026854337390034, 276.6728444866564587, 15.74913442802015950 ) ) ;
#40924 = CARTESIAN_POINT ( 'NONE',  ( 75.41814989884494480, 225.8967562850346837, -4.648177544792955347E-16 ) ) ;
#40925 = ORIENTED_EDGE ( 'NONE', *, *, #50313, .F. ) ;
#40926 = ORIENTED_EDGE ( 'NONE', *, *, #2150, .T. ) ;
#40927 = CARTESIAN_POINT ( 'NONE',  ( 198.2943784004556846, 286.7604802059595954, 16.98915255761611576 ) ) ;
#40929 = CARTESIAN_POINT ( 'NONE',  ( 147.9311236323648870, 274.4227731784279172, -7.799459659034405412 ) ) ;
#40928 = CARTESIAN_POINT ( 'NONE',  ( 162.6094341192679735, 284.9563523671238272, -2.779506450940901541 ) ) ;
#40930 = CARTESIAN_POINT ( 'NONE',  ( 163.4222916751007801, 247.5912830598222172, -10.52132777929285012 ) ) ;
#40931 = CARTESIAN_POINT ( 'NONE',  ( 155.2098048002210930, 261.8157275836062468, 16.98811268941991059 ) ) ;
#40932 = CARTESIAN_POINT ( 'NONE',  ( 39.74423100597210379, 28.11029122506297639, -8.090169943749478065 ) ) ;
#40933 = DIRECTION ( 'NONE',  ( -0.8660254037844387076, -0.4999999999999998890, -0.000000000000000000 ) ) ;
#40934 = CARTESIAN_POINT ( 'NONE',  ( 207.5716517802669046, 271.1223482360200023, -3.664688748148826836 ) ) ;
#40935 = CARTESIAN_POINT ( 'NONE',  ( 206.4636530084236483, 270.6281364296536367, 2.534735893817217089 ) ) ;
#40936 = AXIS2_PLACEMENT_3D ( 'NONE', #35309, #27726, #88586 ) ;
#40937 = CARTESIAN_POINT ( 'NONE',  ( 175.7824178399792174, 285.8628427244275372, -13.39878279634721103 ) ) ;
#40938 = CARTESIAN_POINT ( 'NONE',  ( 86.94057726720511425, 214.8768266524160140, 9.188101187500098632 ) ) ;
#40939 = ORIENTED_EDGE ( 'NONE', *, *, #17705, .T. ) ;
#40940 = CARTESIAN_POINT ( 'NONE',  ( 149.8083888948594335, 271.5779462620446338, 11.70101749353969645 ) ) ;
#40941 = CARTESIAN_POINT ( 'NONE',  ( 78.17513785305828833, 61.62242163703883335, -16.13566992787025356 ) ) ;
#40942 = EDGE_LOOP ( 'NONE', ( #70466, #48848, #59866, #60514 ) ) ;
#40943 = CARTESIAN_POINT ( 'NONE',  ( 167.5469267500292574, 266.7168544022062520, -17.80679023418265672 ) ) ;
#40944 = VERTEX_POINT ( 'NONE', #92467 ) ;
#40945 = CARTESIAN_POINT ( 'NONE',  ( 80.13920462361059549, 44.63425843043530961, -11.72084457139943581 ) ) ;
#40946 = CARTESIAN_POINT ( 'NONE',  ( 78.46959274033001464, 216.1115022471902591, 10.00000000000009592 ) ) ;
#40947 = PLANE ( 'NONE',  #72491 ) ;
#40948 = CARTESIAN_POINT ( 'NONE',  ( 28.13532114344887347, 38.01751292744058475, 6.180339887498949913 ) ) ;
#40949 = CARTESIAN_POINT ( 'NONE',  ( 79.60209170223603792, 48.56606275781557969, -13.98513249790191892 ) ) ;
#40950 = CARTESIAN_POINT ( 'NONE',  ( 162.9968728533147271, 248.3281300736514652, 11.73082768548638910 ) ) ;
#40951 = CARTESIAN_POINT ( 'NONE',  ( 90.89164462408909628, 223.2833772461660260, -9.188101187500095079 ) ) ;
#40952 = ORIENTED_EDGE ( 'NONE', *, *, #32286, .T. ) ;
#40953 = ORIENTED_EDGE ( 'NONE', *, *, #50076, .F. ) ;
#40954 = LINE ( 'NONE', #2498, #96523 ) ;
#40955 = CARTESIAN_POINT ( 'NONE',  ( 161.2859416640352208, 251.2915498217379024, -13.80521263047813996 ) ) ;
#40956 = VERTEX_POINT ( 'NONE', #44821 ) ;
#40957 = PLANE ( 'NONE',  #19095 ) ;
#40958 = EDGE_CURVE ( 'NONE', #72572, #23641, #53908, .T. ) ;
#40959 = CARTESIAN_POINT ( 'NONE',  ( 165.4994878024789102, 285.5423758539902792, 1.070543995922314862 ) ) ;
#40960 = CARTESIAN_POINT ( 'NONE',  ( -6.563276597302431625, 157.0177522451417929, 5.000000000000051514 ) ) ;
#40961 = CARTESIAN_POINT ( 'NONE',  ( 88.25652195435415592, 44.39905568574920380, 4.349260828767085307 ) ) ;
#40962 = ORIENTED_EDGE ( 'NONE', *, *, #29723, .T. ) ;
#40963 = CARTESIAN_POINT ( 'NONE',  ( 204.7462429809936282, 276.0160998285135179, 13.10238900943261342 ) ) ;
#40964 = CARTESIAN_POINT ( 'NONE',  ( 159.4491226731523454, 254.4730136382542582, -15.39140229921534520 ) ) ;
#40965 = CARTESIAN_POINT ( 'NONE',  ( 188.8614500713004247, 269.5370965013109412, 14.80401887895223645 ) ) ;
#40966 = CARTESIAN_POINT ( 'NONE',  ( 176.2504776146596157, 284.2477974488793961, 13.12230192542356910 ) ) ;
#40967 = DIRECTION ( 'NONE',  ( -0.2938926261462390666, 0.5090369604551334692, 0.8090169943749425663 ) ) ;
#40968 = CARTESIAN_POINT ( 'NONE',  ( -22.90719435785855751, 144.7012482093458630, 8.500145032286354763E-14 ) ) ;
#40969 = ORIENTED_EDGE ( 'NONE', *, *, #90035, .F. ) ;
#40970 = LINE ( 'NONE', #34400, #72099 ) ;
#40971 =( BOUNDED_CURVE ( )  B_SPLINE_CURVE ( 2, ( #18960, #13345, #34149, #65041, #7716, #30518, #67519, #44703, #91355 ),
 .UNSPECIFIED., .F., .T. ) 
 B_SPLINE_CURVE_WITH_KNOTS ( ( 3, 2, 2, 2, 3 ),
 ( 0.3508064516129032473, 0.3521505376344086224, 0.3548387096774193727, 0.3575268817204301230, 0.3588709677419354982 ),
 .UNSPECIFIED. ) 
 CURVE ( )  GEOMETRIC_REPRESENTATION_ITEM ( )  RATIONAL_B_SPLINE_CURVE ( ( 0.9330127018922194093, 0.9330127018922194093, 1.000000000000000000, 0.8660254037844387076, 1.000000000000000000, 0.8660254037844387076, 1.000000000000000000, 0.9330127018922194093, 0.9330127018922194093 ) ) 
 REPRESENTATION_ITEM ( '' )  );
#40972 = CARTESIAN_POINT ( 'NONE',  ( 200.3414094930810165, 283.6454952284590263, 16.87912319229835489 ) ) ;
#40973 = CARTESIAN_POINT ( 'NONE',  ( 84.87540209878125097, 43.40687427765107742, 5.588507731394742883 ) ) ;
#40974 = CARTESIAN_POINT ( 'NONE',  ( 171.4444819528139021, 251.6572025020039121, 7.136088224024340398 ) ) ;
#40975 = CARTESIAN_POINT ( 'NONE',  ( 77.85177817260189670, 62.02389414260930067, 15.65016476958103198 ) ) ;
#40976 = PLANE ( 'NONE',  #60783 ) ;
#40977 = EDGE_CURVE ( 'NONE', #63364, #4682, #30540, .T. ) ;
#40978 = PLANE ( 'NONE',  #80260 ) ;
#40979 = ORIENTED_EDGE ( 'NONE', *, *, #82938, .T. ) ;
#40980 = AXIS2_PLACEMENT_3D ( 'NONE', #79962, #18127, #88086 ) ;
#40981 = CARTESIAN_POINT ( 'NONE',  ( 74.97115493809580755, 63.69788091252335960, -14.47858387620434506 ) ) ;
#40982 = CARTESIAN_POINT ( 'NONE',  ( 182.5087044554237252, 264.6871601893720936, 13.42516869467857532 ) ) ;
#40983 = CARTESIAN_POINT ( 'NONE',  ( 69.73423326249884724, 62.23649111975013426, -13.60044372541333857 ) ) ;
#40984 = CARTESIAN_POINT ( 'NONE',  ( 24.50477583610994259, 37.08080186712593473, -3.090169943749475845 ) ) ;
#40986 = ADVANCED_FACE ( 'NONE', ( #32957 ), #10177, .T. ) ;
#40985 = LINE ( 'NONE', #34412, #30421 ) ;
#40987 = CARTESIAN_POINT ( 'NONE',  ( 172.2755583984224756, 275.1251726850771320, 16.76863583107396138 ) ) ;
#40988 =( BOUNDED_CURVE ( )  B_SPLINE_CURVE ( 2, ( #46, #46109, #63329, #78548, #15719, #47621, #1038, #78046, #61321 ),
 .UNSPECIFIED., .F., .T. ) 
 B_SPLINE_CURVE_WITH_KNOTS ( ( 3, 2, 2, 2, 3 ),
 ( 0.8588709677419354982, 0.8602150537634408733, 0.8629032258064516236, 0.8655913978494623739, 0.8669354838709677491 ),
 .UNSPECIFIED. ) 
 CURVE ( )  GEOMETRIC_REPRESENTATION_ITEM ( )  RATIONAL_B_SPLINE_CURVE ( ( 0.9330127018922194093, 0.9330127018922194093, 1.000000000000000000, 0.8660254037844387076, 1.000000000000000000, 0.8660254037844387076, 1.000000000000000000, 0.9330127018922194093, 0.9330127018922194093 ) ) 
 REPRESENTATION_ITEM ( '' )  );
#40989 = DIRECTION ( 'NONE',  ( 0.8660254037844385966, 0.5000000000000003331, 3.252519625699449945E-16 ) ) ;
#40990 = CARTESIAN_POINT ( 'NONE',  ( 71.94636440693795976, 59.33070143154711928, -15.31651758414362696 ) ) ;
#40991 = CARTESIAN_POINT ( 'NONE',  ( 188.4939758497592379, 260.3566504396036976, 3.747743627288043555 ) ) ;
#40992 = DIRECTION ( 'NONE',  ( -1.000000000000000000, 0.000000000000000000, 0.000000000000000000 ) ) ;
#40993 = CARTESIAN_POINT ( 'NONE',  ( 1.609577830863368586, 180.9244531367911577, -4.594050593750046652 ) ) ;
#40994 = AXIS2_PLACEMENT_3D ( 'NONE', #41400, #33838, #35305 ) ;
#40995 = CARTESIAN_POINT ( 'NONE',  ( 123.3201800421238090, 253.5530062829863311, -4.648177544792955347E-16 ) ) ;
#40996 = ORIENTED_EDGE ( 'NONE', *, *, #76851, .F. ) ;
#40997 = B_SPLINE_CURVE_WITH_KNOTS ( 'NONE', 3,
 ( #53839, #16360, #78174, #62955, #94398, #24459, #55341, #86317, #78677, #16853, #47741, #9268, #32564, #58343, #94895, #72078, #64969, #26472, #10270, #79707, #96903, #11287, #96398, #57348 ),
 .UNSPECIFIED., .F., .F.,
 ( 4, 2, 2, 2, 2, 2, 2, 2, 2, 2, 2, 4 ),
 ( 0.0002136614537458351754, 0.0007436913151772940860, 0.001008706245893013905, 0.001074959978571868834, 0.001108086844911295972, 0.001141213711250723328, 0.001207467443929577822, 0.001273721176608432317, 0.001538736107323809095, 0.001803751038039185439, 0.002068765968754562434, 0.002333780899469938778 ),
 .UNSPECIFIED. ) ;
#40999 = CARTESIAN_POINT ( 'NONE',  ( 175.0114272764108136, 255.3094567315552581, 8.250059182469716035 ) ) ;
#40998 = CIRCLE ( 'NONE', #13570, 1.449999999999993072 ) ;
#41000 = DIRECTION ( 'NONE',  ( -0.7135562106085678868, 0.7005979833698787740, 0.000000000000000000 ) ) ;
#41001 = CARTESIAN_POINT ( 'NONE',  ( 81.89611374139302313, 41.17756255496580309, 5.592514320812338013 ) ) ;
#41002 = CARTESIAN_POINT ( 'NONE',  ( 33.57141466322406131, 196.3149278399160949, -9.188101187500095079 ) ) ;
#41003 = CARTESIAN_POINT ( 'NONE',  ( 161.4844649541891499, 250.9476973967054789, 12.93553496455142415 ) ) ;
#41004 = CARTESIAN_POINT ( 'NONE',  ( -52.80137019779957086, 90.67440762873908966, -10.00000000000000000 ) ) ;
#41005 = CARTESIAN_POINT ( 'NONE',  ( 39.65533143765975410, 23.86426979415092475, -3.090169943749474069 ) ) ;
#41006 = CARTESIAN_POINT ( 'NONE',  ( 181.6818972446956195, 294.4829896772180859, 6.439555545740881293 ) ) ;
#41007 = LINE ( 'NONE', #2551, #72284 ) ;
#41008 = CARTESIAN_POINT ( 'NONE',  ( 196.9152821016313339, 289.5797219436533396, 17.82432002680865679 ) ) ;
#41009 = CARTESIAN_POINT ( 'NONE',  ( 81.03611213647164391, 56.10389352724613587, 16.10741472980589961 ) ) ;
#41010 = CARTESIAN_POINT ( 'NONE',  ( 15.23341505093859816, 9.764269794150882475, 3.090169943749476733 ) ) ;
#41011 = PRODUCT_DEFINITION_SHAPE ( 'NONE', 'NONE',  #100299 ) ;
#41012 = EDGE_CURVE ( 'NONE', #86855, #37817, #12779, .T. ) ;
#41013 = EDGE_CURVE ( 'NONE', #91836, #77883, #54746, .T. ) ;
#41014 = CARTESIAN_POINT ( 'NONE',  ( 186.8244161705717374, 295.8837896403537684, -7.711110150879106229 ) ) ;
#41015 = DIRECTION ( 'NONE',  ( -0.8660254037844387076, -0.4999999999999998890, -0.000000000000000000 ) ) ;
#41016 = EDGE_CURVE ( 'NONE', #86729, #61384, #17256, .T. ) ;
#41017 = CARTESIAN_POINT ( 'NONE',  ( 88.86189758574327868, 222.1115022471902591, 10.00000000000009592 ) ) ;
#41018 = CARTESIAN_POINT ( 'NONE',  ( 69.68416697561647766, 66.78355214756700775, -10.04849009066424870 ) ) ;
#41019 = CARTESIAN_POINT ( 'NONE',  ( 203.3519541875798495, 270.1197850214451819, 6.287554717287071604 ) ) ;
#41020 = CARTESIAN_POINT ( 'NONE',  ( 47.69862761034023180, 198.3458772461660544, 9.188101187500095079 ) ) ;
#41021 = CARTESIAN_POINT ( 'NONE',  ( 197.9598023461055902, 287.7705598106892921, 18.23120408239484291 ) ) ;
#41022 = EDGE_LOOP ( 'NONE', ( #15765, #49357, #10106 ) ) ;
#41023 = CARTESIAN_POINT ( 'NONE',  ( -9.047287092407536591, 85.10493810089948852, 14.06874990193072428 ) ) ;
#41024 = CARTESIAN_POINT ( 'NONE',  ( 147.1249913145849177, 275.8190353104462815, 3.637773609013635223 ) ) ;
#41025 = DIRECTION ( 'NONE',  ( -0.5000000000000015543, 0.8660254037844377084, 0.000000000000000000 ) ) ;
#41026 = ADVANCED_FACE ( 'NONE', ( #63367 ), #68199, .F. ) ;
#41027 = VERTEX_POINT ( 'NONE', #73476 ) ;
#41028 = CARTESIAN_POINT ( 'NONE',  ( 66.36268096397610350, 69.44190093015801324, 9.875986171954755521E-07 ) ) ;
#41029 = CARTESIAN_POINT ( 'NONE',  ( 168.0713720833696811, 281.8093708158166351, -11.21549903910966250 ) ) ;
#41030 = LINE ( 'NONE', #71967, #54161 ) ;
#41031 = CARTESIAN_POINT ( 'NONE',  ( 19.18375657693640335, 36.32959363016015431, -10.00000000000000000 ) ) ;
#41032 = CARTESIAN_POINT ( 'NONE',  ( 20.27385872851041526, 33.74646525600390135, 2.839279412974139660 ) ) ;
#41033 = CARTESIAN_POINT ( 'NONE',  ( 162.6476498368881494, 248.9330020812748785, 10.75824100428386743 ) ) ;
#41034 = CARTESIAN_POINT ( 'NONE',  ( 149.7072529793668707, 271.3464269086063041, -11.98883662638834657 ) ) ;
#41035 = CARTESIAN_POINT ( 'NONE',  ( 157.1187995864133882, 258.5092516225370218, 18.42986330599266509 ) ) ;
#41036 = EDGE_LOOP ( 'NONE', ( #87759, #22227, #48403, #83767 ) ) ;
#41037 = CARTESIAN_POINT ( 'NONE',  ( 15.30080465516770616, 11.76004757982088300, 5.678558825948272215 ) ) ;
#41038 = EDGE_CURVE ( 'NONE', #26456, #90241, #5068, .T. ) ;
#41039 = CARTESIAN_POINT ( 'NONE',  ( 171.7522488252528206, 252.8251119870537025, 8.533298209578807914 ) ) ;
#41040 = DIRECTION ( 'NONE',  ( -0.4999999999999987788, 0.8660254037844392627, 0.000000000000000000 ) ) ;
#41041 = EDGE_CURVE ( 'NONE', #89481, #91836, #65847, .T. ) ;
#41042 = ORIENTED_EDGE ( 'NONE', *, *, #58416, .F. ) ;
#41043 = CYLINDRICAL_SURFACE ( 'NONE', #61076, 17.82106496071139645 ) ;
#41044 = CARTESIAN_POINT ( 'NONE',  ( 191.0170959869219303, 299.7956799668270946, 7.353346939903929069 ) ) ;
#41045 = CYLINDRICAL_SURFACE ( 'NONE', #85746, 10.00000000000001066 ) ;
#41046 = CARTESIAN_POINT ( 'NONE',  ( 73.83222695958433235, 64.41044440392025194, -14.27322267731098648 ) ) ;
#41047 = VERTEX_POINT ( 'NONE', #35457 ) ;
#41048 = ORIENTED_EDGE ( 'NONE', *, *, #35890, .T. ) ;
#41050 = CARTESIAN_POINT ( 'NONE',  ( 151.2479124125312921, 269.2699359884643400, -14.13957473936566167 ) ) ;
#41049 = CARTESIAN_POINT ( 'NONE',  ( 189.7066971257315231, 274.2939208849840043, -15.68303241876299658 ) ) ;
#41051 = VERTEX_POINT ( 'NONE', #35950 ) ;
#41052 = CARTESIAN_POINT ( 'NONE',  ( 201.1060504099706350, 282.3210983108598384, -18.18000168485860257 ) ) ;
#41053 = CARTESIAN_POINT ( 'NONE',  ( 45.05588048050944394, 66.36777381976857271, 177.5919119679930134 ) ) ;
#41054 = CARTESIAN_POINT ( 'NONE',  ( 73.00396795751623813, 57.62093675937267534, -16.32480838639074960 ) ) ;
#41055 = CARTESIAN_POINT ( 'NONE',  ( 77.03033377257250436, 63.66679109869721742, 15.37730549896620147 ) ) ;
#41056 = CARTESIAN_POINT ( 'NONE',  ( 205.3708847852691406, 274.9341884869767227, -13.70973585089674174 ) ) ;
#41057 = CARTESIAN_POINT ( 'NONE',  ( 111.6762543149156386, 235.2833772461660544, -9.188101187500095079 ) ) ;
#41058 = CARTESIAN_POINT ( 'NONE',  ( 148.9504735598738137, 272.6572073132907690, -11.88406006066344744 ) ) ;
#41059 = CARTESIAN_POINT ( 'NONE',  ( 180.3887555915763414, 287.0315616845538216, -13.66997111987796032 ) ) ;
#41060 = ORIENTED_EDGE ( 'NONE', *, *, #905, .T. ) ;
#41061 = CARTESIAN_POINT ( 'NONE',  ( 164.3545367017254364, 245.9765873086048487, -5.942639963102972267 ) ) ;
#41062 = ORIENTED_EDGE ( 'NONE', *, *, #9669, .F. ) ;
#41063 = CARTESIAN_POINT ( 'NONE',  ( 25.47001115121704373, 36.74646525600391556, 2.839279412974139660 ) ) ;
#41064 = CARTESIAN_POINT ( 'NONE',  ( 159.2077906806335932, 254.8910129107889588, 16.14624949541834553 ) ) ;
#41065 = CARTESIAN_POINT ( 'NONE',  ( 78.21696194461939911, 47.89139066307899384, -14.01588872958974363 ) ) ;
#41066 = CARTESIAN_POINT ( 'NONE',  ( 66.48072710279772934, 203.0643266524160140, 9.188101187500095079 ) ) ;
#41067 = CARTESIAN_POINT ( 'NONE',  ( 74.41176536287696308, 68.30213538679808494, 11.88880159922068636 ) ) ;
#41068 = CARTESIAN_POINT ( 'NONE',  ( 151.3284628043366524, 268.5384091220288383, 14.49047510809488237 ) ) ;
#41069 = CARTESIAN_POINT ( 'NONE',  ( 150.5461004505574181, 269.8935004687035644, 13.73913105907748111 ) ) ;
#41070 = FACE_OUTER_BOUND ( 'NONE', #89483, .T. ) ;
#41071 = ORIENTED_EDGE ( 'NONE', *, *, #94596, .T. ) ;
#41072 = VECTOR ( 'NONE', #831, 1000.000000000000114 ) ;
#41073 = LINE ( 'NONE', #96838, #48009 ) ;
#41074 = CARTESIAN_POINT ( 'NONE',  ( 83.51844524235421829, 42.82187930146461952, -5.925958474313000046 ) ) ;
#41075 = CARTESIAN_POINT ( 'NONE',  ( 177.9640863285869159, 288.6651767168248170, 10.86720228571057945 ) ) ;
#41076 = CARTESIAN_POINT ( 'NONE',  ( 147.6947327179224487, 274.8322142526899370, 9.090449717876689206 ) ) ;
#41077 = VERTEX_POINT ( 'NONE', #57749 ) ;
#41078 = CARTESIAN_POINT ( 'NONE',  ( 105.7493929595398470, 231.8615022471902591, -10.00000000000009592 ) ) ;
#41079 = CARTESIAN_POINT ( 'NONE',  ( 68.00902249195229388, 69.32663607418423624, -3.845441495452403657 ) ) ;
#41080 = B_SPLINE_CURVE_WITH_KNOTS ( 'NONE', 3,
 ( #27781, #20190, #51058, #82019 ),
 .UNSPECIFIED., .F., .F.,
 ( 4, 4 ),
 ( 0.02373679057857851910, 0.03297336722804258130 ),
 .UNSPECIFIED. ) ;
#41081 = CARTESIAN_POINT ( 'NONE',  ( 191.0481356132114570, 299.7419177570458828, 9.104177228535229816 ) ) ;
#41082 = CARTESIAN_POINT ( 'NONE',  ( 82.56232498766836159, 52.00393866007731702, -15.24789231007047619 ) ) ;
#41083 = VECTOR ( 'NONE', #31581, 1000.000000000000114 ) ;
#41084 = CARTESIAN_POINT ( 'NONE',  ( 149.6896757981861583, 271.3768714794653647, 12.49809796062302603 ) ) ;
#41085 = CARTESIAN_POINT ( 'NONE',  ( 68.55513178119723250, 64.39780669069259034, 11.67030924314737206 ) ) ;
#41086 = ADVANCED_FACE ( 'NONE', ( #89231 ), #19781, .T. ) ;
#41087 = CARTESIAN_POINT ( 'NONE',  ( 164.6241018286200699, 245.5096868128744632, 3.031483545445131433 ) ) ;
#41088 = CARTESIAN_POINT ( 'NONE',  ( 76.13230372035420146, 65.40393639426625327, 14.02425539466697479 ) ) ;
#41089 = CARTESIAN_POINT ( 'NONE',  ( 167.8759064645936689, 255.9993705094734651, 13.57746339537463598 ) ) ;
#41090 = CARTESIAN_POINT ( 'NONE',  ( 19.15050853525752927, 34.55466486950700045, 7.012934429366973338E-14 ) ) ;
#41091 = CARTESIAN_POINT ( 'NONE',  ( 114.4365367415960293, 243.0024278399160949, -9.188101187500093303 ) ) ;
#41092 = VERTEX_POINT ( 'NONE', #66851 ) ;
#41093 = CARTESIAN_POINT ( 'NONE',  ( 85.28185142231448879, 44.17485613502010011, -6.750586009585262559 ) ) ;
#41094 = DIRECTION ( 'NONE',  ( -1.000000000000000000, 0.000000000000000000, 0.000000000000000000 ) ) ;
#41095 = EDGE_CURVE ( 'NONE', #33095, #7074, #25712, .T. ) ;
#41096 = CARTESIAN_POINT ( 'NONE',  ( 202.7754741559590173, 279.4295715634463022, -15.65855077192107636 ) ) ;
#41097 = CARTESIAN_POINT ( 'NONE',  ( 204.3951397407346064, 276.6242284793436852, 14.79595971842109137 ) ) ;
#41098 = CARTESIAN_POINT ( 'NONE',  ( 83.85460425676879481, 51.57915136420024282, -14.37880942938260098 ) ) ;
#41099 = DIRECTION ( 'NONE',  ( 0.2925570654631259870, 0.000000000000000000, -0.9562480658530003730 ) ) ;
#41100 = ORIENTED_EDGE ( 'NONE', *, *, #74008, .F. ) ;
#41101 = CARTESIAN_POINT ( 'NONE',  ( 80.29069729260778843, 58.15026982914754683, -16.60659103188077879 ) ) ;
#41102 = CARTESIAN_POINT ( 'NONE',  ( 155.5521066005403554, 273.5621557416596943, -12.84016899138273260 ) ) ;
#41104 = CARTESIAN_POINT ( 'NONE',  ( 40.82928596147627331, 60.38352576601455723, -10.00000000000000000 ) ) ;
#41103 = CARTESIAN_POINT ( 'NONE',  ( 72.42095758685501039, 70.73706075180957953, 7.727740079816332042 ) ) ;
#41105 = CARTESIAN_POINT ( 'NONE',  ( 165.0817809681736037, 244.7169632896033136, -1.727194264083430131 ) ) ;
#41106 = CARTESIAN_POINT ( 'NONE',  ( 140.8778087205959650, 242.9548013555409796, -4.594050593750042211 ) ) ;
#41107 = EDGE_CURVE ( 'NONE', #52411, #90599, #36440, .T. ) ;
#41108 = CARTESIAN_POINT ( 'NONE',  ( 101.3989120123781191, 240.8967562850346837, -4.648177544792955347E-16 ) ) ;
#41109 = CARTESIAN_POINT ( 'NONE',  ( 188.0009137200860039, 298.2175614353434412, 4.729959318426725012 ) ) ;
#41110 = CARTESIAN_POINT ( 'NONE',  ( -22.42236680055709641, 157.8615022471902591, 0.000000000000000000 ) ) ;
#41111 = CARTESIAN_POINT ( 'NONE',  ( 59.55217677675723564, 211.3149278399160949, -9.188101187500095079 ) ) ;
#41112 = CARTESIAN_POINT ( 'NONE',  ( 207.6007741873543750, 271.0719067473055475, 7.587922723682903658 ) ) ;
#41113 = CARTESIAN_POINT ( 'NONE',  ( 155.9742855435482909, 281.1012582971416123, 3.224975351481907282 ) ) ;
#41114 = EDGE_CURVE ( 'NONE', #75611, #13298, #40013, .T. ) ;
#41115 = CARTESIAN_POINT ( 'NONE',  ( 70.80369121223017714, 70.91613982041616282, -4.241969676397446598 ) ) ;
#41116 = ADVANCED_FACE ( 'NONE', ( #47750 ), #48272, .T. ) ;
#41117 = DIRECTION ( 'NONE',  ( -0.000000000000000000, -0.000000000000000000, -1.000000000000000000 ) ) ;
#41118 = LINE ( 'NONE', #27446, #36951 ) ;
#41119 = CARTESIAN_POINT ( 'NONE',  ( 169.6667690310781893, 285.3286781044860163, -7.966101626908379529 ) ) ;
#41120 = CARTESIAN_POINT ( 'NONE',  ( 203.5629025532486196, 278.0657055720176913, -15.85226727704602823 ) ) ;
#41121 = CARTESIAN_POINT ( 'NONE',  ( 193.0622221429366050, 289.4054684591471300, 16.71589558189321778 ) ) ;
#41122 = CARTESIAN_POINT ( 'NONE',  ( 130.1965684169902033, 232.6427522451417644, 1.119607411625061291E-15 ) ) ;
#41123 = CARTESIAN_POINT ( 'NONE',  ( 20.52402715336229377, 23.80066082961421969, 10.00000000000000533 ) ) ;
#41124 = EDGE_LOOP ( 'NONE', ( #76242, #69531, #98551, #47373 ) ) ;
#41125 = CARTESIAN_POINT ( 'NONE',  ( 147.6140518775699491, 274.9719575673779559, 8.457032797753797126 ) ) ;
#41126 = CARTESIAN_POINT ( 'NONE',  ( 166.8965953329662568, 259.4083194189263963, 16.50658842888446642 ) ) ;
#41127 = CARTESIAN_POINT ( 'NONE',  ( 38.76791418169571557, 187.0643266524159856, -9.188101187500093303 ) ) ;
#41128 = CARTESIAN_POINT ( 'NONE',  ( 25.79892497710874366, 15.86426979415090166, -3.090169943749474069 ) ) ;
#41129 = CARTESIAN_POINT ( 'NONE',  ( 192.9064638172013417, 270.9369261147751331, 14.92505667092759758 ) ) ;
#41130 = CARTESIAN_POINT ( 'NONE',  ( 75.99750771566300500, 65.44421971917601866, -13.95497799904430458 ) ) ;
#41131 = CARTESIAN_POINT ( 'NONE',  ( 147.3984236761635884, 275.3454365677582700, 5.108566646342994844 ) ) ;
#41132 = CARTESIAN_POINT ( 'NONE',  ( 73.88993811345744689, 55.02826134877724940, -16.60322266602316077 ) ) ;
#41133 = EDGE_CURVE ( 'NONE', #46853, #80971, #79218, .T. ) ;
#41135 = CARTESIAN_POINT ( 'NONE',  ( 68.78093353194373094, 200.5177522451417929, 5.000000000000051514 ) ) ;
#41134 = CARTESIAN_POINT ( 'NONE',  ( 2.749951498565457175, 23.36126292948892313, 6.180339887498949913 ) ) ;
#41136 = CARTESIAN_POINT ( 'NONE',  ( 174.4928008983406471, 289.3651385215947585, 7.878677603660426243 ) ) ;
#41137 = CARTESIAN_POINT ( 'NONE',  ( 180.8112268592145426, 256.2796902623131245, 1.435307982165026752 ) ) ;
#41138 = CARTESIAN_POINT ( 'NONE',  ( 157.7733463334721478, 257.3755434007023268, -16.94489513499352995 ) ) ;
#41139 = CARTESIAN_POINT ( 'NONE',  ( 71.76351473723394747, 71.84897031608997509, 2.971691788643012977 ) ) ;
#41140 = AXIS2_PLACEMENT_3D ( 'NONE', #25724, #58099, #66208 ) ;
#41141 = ADVANCED_FACE ( 'NONE', ( #79715 ), #25986, .F. ) ;
#41142 = CARTESIAN_POINT ( 'NONE',  ( 39.49844957003031709, 183.6115022471902023, -5.000000000000041744 ) ) ;
#41143 = CARTESIAN_POINT ( 'NONE',  ( 184.8810468967335225, 294.4243617658604535, 9.952176429897862775 ) ) ;
#41144 = CARTESIAN_POINT ( 'NONE',  ( 162.8042930031641049, 248.6616881586264469, 11.14389129512055554 ) ) ;
#41145 = CARTESIAN_POINT ( 'NONE',  ( 11.59636713795893925, 171.3768266524160140, 9.188101187500098632 ) ) ;
#41146 = CARTESIAN_POINT ( 'NONE',  ( 31.53879454291322659, 39.18502408145594984, 5.678558825948277544 ) ) ;
#41148 = CARTESIAN_POINT ( 'NONE',  ( 170.8728180971433801, 262.9177787688888088, 16.18685465067498797 ) ) ;
#41147 = CARTESIAN_POINT ( 'NONE',  ( 164.3310316338254609, 252.4241088064557061, 13.56221488630103345 ) ) ;
#41149 = CARTESIAN_POINT ( 'NONE',  ( 27.64472685218285264, 186.7677522451418497, 10.00000000000009592 ) ) ;
#41150 = CARTESIAN_POINT ( 'NONE',  ( 28.62558104116610380, 25.03085787977764198, 9.188101187500006262 ) ) ;
#41151 = CARTESIAN_POINT ( 'NONE',  ( 164.9617201910520237, 244.9249146555742414, 2.745022583679548767 ) ) ;
#41152 = VECTOR ( 'NONE', #62488, 1000.000000000000227 ) ;
#41153 = CARTESIAN_POINT ( 'NONE',  ( 183.2116848952928194, 257.8133941036112446, -2.270876890648756863 ) ) ;
#41154 = EDGE_CURVE ( 'NONE', #49332, #32899, #50621, .T. ) ;
#41155 = CARTESIAN_POINT ( 'NONE',  ( -54.45295541630240166, 33.76759809053437067, 10.00000000000000000 ) ) ;
#41156 = CARTESIAN_POINT ( 'NONE',  ( 65.02584505343169496, 219.8967562850346837, -4.648177544792955347E-16 ) ) ;
#41157 = FACE_OUTER_BOUND ( 'NONE', #52430, .T. ) ;
#41158 = CARTESIAN_POINT ( 'NONE',  ( 12.71236424662705566, 15.84335787977761534, 9.188101187500006262 ) ) ;
#41159 = CARTESIAN_POINT ( 'NONE',  ( 165.7072790779917284, 285.4338682230774111, 0.4788325442398248533 ) ) ;
#41160 = CARTESIAN_POINT ( 'NONE',  ( 15.51250667149479590, 27.14336893147754992, 7.433330006724141015 ) ) ;
#41161 = CARTESIAN_POINT ( 'NONE',  ( 76.32488315910845245, 203.3262482093458061, 3.021315404115420679E-15 ) ) ;
#41162 = ADVANCED_FACE ( 'NONE', ( #82082 ), #83570, .T. ) ;
#41163 = CARTESIAN_POINT ( 'NONE',  ( 153.8401448635538600, 275.1610109593079869, 10.49742240986545028 ) ) ;
#41164 = CARTESIAN_POINT ( 'NONE',  ( 159.9531724557437826, 253.5999738052623229, -15.71074128491364874 ) ) ;
#41165 = CARTESIAN_POINT ( 'NONE',  ( 62.88113547221017541, 197.1115022471902023, -5.000000000000041744 ) ) ;
#41166 = ORIENTED_EDGE ( 'NONE', *, *, #98793, .F. ) ;
#41167 = CARTESIAN_POINT ( 'NONE',  ( 192.0523540417460993, 298.0025604169266558, 12.03387399082417275 ) ) ;
#41168 = CARTESIAN_POINT ( 'NONE',  ( 206.9676408587583296, 272.1685258403992975, 7.544050792475608169 ) ) ;
#41169 = CARTESIAN_POINT ( 'NONE',  ( 66.05904967884808343, 68.59175798592418971, 4.366901512547229025 ) ) ;
#41170 = CARTESIAN_POINT ( 'NONE',  ( 87.24455917599382815, 45.43202867884257046, 7.120756001641662003 ) ) ;
#41171 = CARTESIAN_POINT ( 'NONE',  ( 154.8838596469624349, 262.3802811495310152, 18.07457254681616021 ) ) ;
#41172 = ORIENTED_EDGE ( 'NONE', *, *, #52337, .T. ) ;
#41173 = ORIENTED_EDGE ( 'NONE', *, *, #61638, .F. ) ;
#41174 = CARTESIAN_POINT ( 'NONE',  ( 159.4726537399769200, 278.3283626346205892, -9.792651960952584389 ) ) ;
#41175 = B_SPLINE_CURVE_WITH_KNOTS ( 'NONE', 3,
 ( #12753, #3650, #4125, #34053 ),
 .UNSPECIFIED., .F., .F.,
 ( 4, 4 ),
 ( 0.01409801504582384665, 0.02276995735195360901 ),
 .UNSPECIFIED. ) ;
#41176 = CARTESIAN_POINT ( 'NONE',  ( 86.10128179547638183, 47.01522930412662760, 10.71950609365847917 ) ) ;
#41177 = ORIENTED_EDGE ( 'NONE', *, *, #546, .T. ) ;
#41178 = CARTESIAN_POINT ( 'NONE',  ( 77.79862349870425930, 57.75687281312781352, 16.17549868577739147 ) ) ;
#41179 = DIRECTION ( 'NONE',  ( -0.8660254037844387076, -0.4999999999999998890, -0.000000000000000000 ) ) ;
#41180 = ORIENTED_EDGE ( 'NONE', *, *, #23408, .T. ) ;
#41181 = CARTESIAN_POINT ( 'NONE',  ( 44.85937643310610667, 116.8208962945185050, 10.00000000000000000 ) ) ;
#41182 = DIRECTION ( 'NONE',  ( 0.9538480676139723391, -0.3002896333693372277, 0.000000000000000000 ) ) ;
#41183 = CARTESIAN_POINT ( 'NONE',  ( 80.72039647166839416, 43.16609979737107494, 9.908769291271109836 ) ) ;
#41184 = VERTEX_POINT ( 'NONE', #35431 ) ;
#41185 = CARTESIAN_POINT ( 'NONE',  ( 161.5056331467593225, 250.9110330116698435, 14.52719814064025528 ) ) ;
#41186 = CARTESIAN_POINT ( 'NONE',  ( 169.4855280223256102, 276.4705657850510079, -15.92413266703292329 ) ) ;
#41187 = CARTESIAN_POINT ( 'NONE',  ( 50.59379163489128928, 94.40700863652010355, 10.00000000000000000 ) ) ;
#41188 = CARTESIAN_POINT ( 'NONE',  ( -64.74139798177012040, 41.16849083240310847, -10.00000000000000000 ) ) ;
#41189 = ORIENTED_EDGE ( 'NONE', *, *, #7852, .T. ) ;
#41190 = CARTESIAN_POINT ( 'NONE',  ( -19.52881935598935570, 92.99677094728539828, 59.99999999999999289 ) ) ;
#41191 = CARTESIAN_POINT ( 'NONE',  ( 33.00691499580853616, 42.55466486950702887, 7.012934429366973338E-14 ) ) ;
#41192 = VERTEX_POINT ( 'NONE', #5043 ) ;
#41193 = ORIENTED_EDGE ( 'NONE', *, *, #97085, .T. ) ;
#41194 = DIRECTION ( 'NONE',  ( -0.2347357813929480952, 0.4065742997269687908, 0.8829475928589233247 ) ) ;
#41195 = ORIENTED_EDGE ( 'NONE', *, *, #88231, .F. ) ;
#41196 = CARTESIAN_POINT ( 'NONE',  ( 160.9880467243960140, 270.9392944726602082, 15.98296159911883763 ) ) ;
#41197 = VERTEX_POINT ( 'NONE', #13639 ) ;
#41198 = DIRECTION ( 'NONE',  ( 0.000000000000000000, 0.000000000000000000, 1.000000000000000000 ) ) ;
#41199 = CARTESIAN_POINT ( 'NONE',  ( 194.0720430060108015, 294.5043565153341660, 13.95655032404117435 ) ) ;
#41200 = CARTESIAN_POINT ( 'NONE',  ( 177.3359723029854820, 288.7904352073793461, -9.432456604021657753 ) ) ;
#41201 = CARTESIAN_POINT ( 'NONE',  ( 71.22758957664390778, 69.00678633681690144, 8.474304139278888925 ) ) ;
#41202 = CARTESIAN_POINT ( 'NONE',  ( 192.1149248854976861, 297.8941845364767005, 12.26771790733441314 ) ) ;
#41203 = CARTESIAN_POINT ( 'NONE',  ( 175.4967466201937611, 291.2628096033125189, 6.560984766252938805 ) ) ;
#41204 = FACE_OUTER_BOUND ( 'NONE', #9980, .T. ) ;
#41205 = ORIENTED_EDGE ( 'NONE', *, *, #917, .F. ) ;
#41206 = CARTESIAN_POINT ( 'NONE',  ( 50.26447705663006360, 96.46038765672592774, 10.00000000000000000 ) ) ;
#41207 = CARTESIAN_POINT ( 'NONE',  ( 17.35762855594305520, 30.99752408145591431, 5.678558825948277544 ) ) ;
#41208 = CARTESIAN_POINT ( 'NONE',  ( 205.9240884482826175, 273.9760116357041966, 10.27504561427317142 ) ) ;
#41210 = CARTESIAN_POINT ( 'NONE',  ( 190.9468710165551784, 298.7780173384815043, -8.169303778663410398 ) ) ;
#41209 = CARTESIAN_POINT ( 'NONE',  ( 168.1726423428391399, 255.4859975196775963, 14.21197738914692366 ) ) ;
#41212 = VERTEX_POINT ( 'NONE', #13151 ) ;
#41211 = DIRECTION ( 'NONE',  ( 0.000000000000000000, 0.000000000000000000, 1.000000000000000000 ) ) ;
#41213 = ORIENTED_EDGE ( 'NONE', *, *, #42407, .T. ) ;
#41214 = CARTESIAN_POINT ( 'NONE',  ( 146.7017019969479463, 276.5521939148946444, -3.698925540390689104 ) ) ;
#41215 = CARTESIAN_POINT ( 'NONE',  ( 197.6616696696203803, 265.4270972886941991, 5.703842229917075457 ) ) ;
#41216 = CARTESIAN_POINT ( 'NONE',  ( 33.63407072503001416, 49.62913085183822659, -10.00000000000000000 ) ) ;
#41217 = LINE ( 'NONE', #39699, #13355 ) ;
#41218 = AXIS2_PLACEMENT_3D ( 'NONE', #11235, #81646, #12217 ) ;
#41219 = CARTESIAN_POINT ( 'NONE',  ( 161.8662906133268393, 250.2863559554455719, 14.03735902266321744 ) ) ;
#41220 = CARTESIAN_POINT ( 'NONE',  ( 71.40048854769935360, 59.28136089601005665, 15.74267823446789905 ) ) ;
#41221 = ORIENTED_EDGE ( 'NONE', *, *, #27516, .F. ) ;
#41222 = FACE_OUTER_BOUND ( 'NONE', #6913, .T. ) ;
#41223 = DIRECTION ( 'NONE',  ( -1.000000000000000000, -1.387778780781445478E-15, -0.000000000000000000 ) ) ;
#41224 = FACE_OUTER_BOUND ( 'NONE', #98649, .T. ) ;
#41225 = CARTESIAN_POINT ( 'NONE',  ( 164.7243055739305078, 245.3361288348881999, -1.445094907380085170 ) ) ;
#41226 = CARTESIAN_POINT ( 'NONE',  ( 10.75723147838630034, 177.0177522451418497, -10.00000000000009592 ) ) ;
#41227 = CARTESIAN_POINT ( 'NONE',  ( 102.5290345353249961, 223.8768266524159856, 9.188101187500096856 ) ) ;
#41229 = EDGE_CURVE ( 'NONE', #82089, #55525, #64272, .T. ) ;
#41228 = VECTOR ( 'NONE', #56089, 1000.000000000000114 ) ;
#41230 = CARTESIAN_POINT ( 'NONE',  ( 82.62228925795274392, 40.54765601476822923, -1.426017262080774728 ) ) ;
#41231 = LINE ( 'NONE', #48355, #43717 ) ;
#41232 = CARTESIAN_POINT ( 'NONE',  ( 170.2950668402331758, 280.6084956370413579, -13.85235648845468326 ) ) ;
#41233 = CARTESIAN_POINT ( 'NONE',  ( 21.71786549680706102, 183.3458772461660544, 9.188101187500095079 ) ) ;
#41234 = CYLINDRICAL_SURFACE ( 'NONE', #80318, 14.99999999999968381 ) ;
#41235 = ORIENTED_EDGE ( 'NONE', *, *, #86667, .T. ) ;
#41237 = VERTEX_POINT ( 'NONE', #66825 ) ;
#41236 = PRODUCT_DEFINITION_CONTEXT ( 'detailed design', #61525, 'design' ) ;
#41238 = CARTESIAN_POINT ( 'NONE',  ( -16.26211276271276063, 167.1916292661125283, 0.000000000000000000 ) ) ;
#41239 = EDGE_CURVE ( 'NONE', #55233, #96593, #4529, .T. ) ;
#41240 = CARTESIAN_POINT ( 'NONE',  ( 68.88891825534665259, 70.31481240275726918, 1.479671699557132847 ) ) ;
#41241 = EDGE_CURVE ( 'NONE', #21768, #24856, #60632, .T. ) ;
#41242 = CARTESIAN_POINT ( 'NONE',  ( 84.41257289432805067, 44.20851797303996733, 7.649024224649666692 ) ) ;
#41243 = LINE ( 'NONE', #80306, #22343 ) ;
#41244 = CARTESIAN_POINT ( 'NONE',  ( 45.79324619304848909, 117.8999360398438654, 10.00000000000000000 ) ) ;
#41245 = CARTESIAN_POINT ( 'NONE',  ( 181.9320025749308627, 285.0146321948373043, 15.19111020286634428 ) ) ;
#41246 = CARTESIAN_POINT ( 'NONE',  ( 74.32663207346742240, 67.92009797516583092, -11.69620558213257233 ) ) ;
#41247 = CARTESIAN_POINT ( 'NONE',  ( 36.49425040099653472, 198.0024278399160949, -9.188101187500093303 ) ) ;
#41248 = CARTESIAN_POINT ( 'NONE',  ( 87.40047971330916710, 211.2677522451417929, -5.000000000000041744 ) ) ;
#41249 = EDGE_LOOP ( 'NONE', ( #48923, #12574, #30718, #1388 ) ) ;
#41250 = CARTESIAN_POINT ( 'NONE',  ( 79.32566820500107951, 59.73991648520959075, -16.51753030644415077 ) ) ;
#41251 = CARTESIAN_POINT ( 'NONE',  ( 178.8406086741226204, 259.2614543872599597, -10.29665073561374733 ) ) ;
#41252 = B_SPLINE_CURVE_WITH_KNOTS ( 'NONE', 3,
 ( #35262, #41865, #27683, #90003, #3396, #34271, #81906, #12485, #43351, #74299, #96117, #66660, #28162, #68645, #29170, #53438, #16817, #76749, #5369, #51964, #44842, #21088, #74791, #28654, #82905, #67656, #37735, #21566, #22553, #98076, #67155, #44348, #62918, #29656, #32008, #13477, #61033, #36748, #14935, #37249, #76275, #99565, #83899, #5863, #36252, #6849 ),
 .UNSPECIFIED., .F., .F.,
 ( 4, 1, 1, 1, 2, 2, 1, 1, 1, 2, 2, 1, 1, 2, 2, 1, 1, 2, 2, 1, 1, 2, 2, 1, 2, 2, 1, 2, 2, 4 ),
 ( 0.000000000000000000, 0.06249999999999693301, 0.09374999999999547584, 0.1093749999999947542, 0.1171874999999927003, 0.1249999999999906325, 0.1874999999999749922, 0.2187499999999669986, 0.2343749999999645284, 0.2421874999999631406, 0.2499999999999617528, 0.3124999999999574785, 0.3437499999999567013, 0.3593749999999563682, 0.3749999999999560907, 0.4374999999999543143, 0.4687499999999536482, 0.4843749999999518718, 0.4999999999999500955, 0.5624999999999510392, 0.5937499999999500400, 0.6093749999999494849, 0.6249999999999489297, 0.6874999999999561462, 0.7187499999999611422, 0.7499999999999661382, 0.8124999999999761302, 0.8437499999999811262, 0.8749999999999861222, 1.000000000000000000 ),
 .UNSPECIFIED. ) ;
#41253 = CARTESIAN_POINT ( 'NONE',  ( -0.5819415548772214342, 158.2202760586659736, -5.415160957724236172E-17 ) ) ;
#41254 = CARTESIAN_POINT ( 'NONE',  ( 72.76446422349044951, 71.15534465558162935, -7.354170587574372142 ) ) ;
#41255 = CARTESIAN_POINT ( 'NONE',  ( 198.6894790592683080, 286.5067226703918095, -17.06774375037124614 ) ) ;
#41256 = CARTESIAN_POINT ( 'NONE',  ( 186.7303744183177230, 282.7117158418231497, 16.18601837252264630 ) ) ;
#41257 = CARTESIAN_POINT ( 'NONE',  ( 147.4824818982269790, 275.1998434563504929, -4.972419998968698351 ) ) ;
#41258 = CARTESIAN_POINT ( 'NONE',  ( 172.2547787113288678, 266.8662971372079369, 17.58576446449312058 ) ) ;
#41259 = FACE_OUTER_BOUND ( 'NONE', #32994, .T. ) ;
#41260 = CARTESIAN_POINT ( 'NONE',  ( 191.7934382699952494, 298.4510156884799699, -8.680100145728863126 ) ) ;
#41261 = CARTESIAN_POINT ( 'NONE',  ( 207.0200405408487541, 272.0777669287182334, 6.494273599193515878 ) ) ;
#41262 = VERTEX_POINT ( 'NONE', #43524 ) ;
#41263 = EDGE_CURVE ( 'NONE', #82867, #20583, #77553, .T. ) ;
#41264 = CARTESIAN_POINT ( 'NONE',  ( 145.6409484414103588, 245.7048013555409511, 4.594050593750051981 ) ) ;
#41265 = LINE ( 'NONE', #18002, #14280 ) ;
#41266 = CARTESIAN_POINT ( 'NONE',  ( 123.6384037525706958, 236.0643266524160140, 9.188101187500095079 ) ) ;
#41267 = CARTESIAN_POINT ( 'NONE',  ( 13.49720994389718598, 29.83396525600389637, -2.839279412974133887 ) ) ;
#41268 = CARTESIAN_POINT ( 'NONE',  ( 74.96142304803882439, 67.14338225477067112, 13.01358479607535479 ) ) ;
#41269 = CARTESIAN_POINT ( 'NONE',  ( -112.5954152546897120, 74.04580364311802043, 30.52142883766498116 ) ) ;
#41271 = DIRECTION ( 'NONE',  ( 0.4999999999999998890, -0.8660254037844385966, 0.000000000000000000 ) ) ;
#41270 = CARTESIAN_POINT ( 'NONE',  ( 144.9899443387551798, 254.5170451491295296, 0.000000000000000000 ) ) ;
#41272 = EDGE_CURVE ( 'NONE', #38622, #1218, #5533, .T. ) ;
#41273 = CARTESIAN_POINT ( 'NONE',  ( 151.0363639623897996, 269.0443391571128018, -14.33469264561397516 ) ) ;
#41274 = ORIENTED_EDGE ( 'NONE', *, *, #75091, .F. ) ;
#41275 = CARTESIAN_POINT ( 'NONE',  ( 192.9426785658947381, 263.8201562504407320, -4.863779990015462573 ) ) ;
#41276 = CARTESIAN_POINT ( 'NONE',  ( 196.4808189786114951, 290.3322341467384717, -17.84817245450773271 ) ) ;
#41277 = CARTESIAN_POINT ( 'NONE',  ( 182.2052959828711494, 288.8764495671124450, 13.90737013350400986 ) ) ;
#41278 = CARTESIAN_POINT ( 'NONE',  ( 172.8470737319805721, 290.2464512094754241, -1.885184669499159194 ) ) ;
#41279 = CARTESIAN_POINT ( 'NONE',  ( 81.50893757138975104, 55.16156497580061568, -15.92217606427533205 ) ) ;
#41280 = VERTEX_POINT ( 'NONE', #44512 ) ;
#41281 = CARTESIAN_POINT ( 'NONE',  ( 71.03936537156745601, 65.74473520561056716, -12.39895433411619763 ) ) ;
#41282 = CARTESIAN_POINT ( 'NONE',  ( 177.1415970308396481, 279.4433984593848663, 15.53509258474510979 ) ) ;
#41283 = CARTESIAN_POINT ( 'NONE',  ( -59.65739779450132829, 37.15562860896454112, -10.00000000000000000 ) ) ;
#41284 = ADVANCED_FACE ( 'NONE', ( #89687 ), #99242, .F. ) ;
#41285 = CARTESIAN_POINT ( 'NONE',  ( 80.40498937112451472, 56.16844747207684208, 16.11541614916188792 ) ) ;
#41286 = AXIS2_PLACEMENT_3D ( 'NONE', #88372, #4196, #74628 ) ;
#41287 = LINE ( 'NONE', #80863, #84983 ) ;
#41288 = CARTESIAN_POINT ( 'NONE',  ( 72.25718139279801733, 71.61371966692031776, -5.855127513239330561 ) ) ;
#41289 = CARTESIAN_POINT ( 'NONE',  ( 150.5438776023515004, 278.3016033182416322, -9.804454847755098641E-05 ) ) ;
#41290 =( BOUNDED_CURVE ( )  B_SPLINE_CURVE ( 2, ( #43738, #37627, #59423, #28047, #58922, #60422, #14835, #76646, #20469 ),
 .UNSPECIFIED., .F., .T. ) 
 B_SPLINE_CURVE_WITH_KNOTS ( ( 3, 2, 2, 2, 3 ),
 ( 0.7056451612903226200, 0.7069892473118279952, 0.7096774193548387455, 0.7123655913978494958, 0.7137096774193548709 ),
 .UNSPECIFIED. ) 
 CURVE ( )  GEOMETRIC_REPRESENTATION_ITEM ( )  RATIONAL_B_SPLINE_CURVE ( ( 0.9330127018922194093, 0.9330127018922194093, 1.000000000000000000, 0.8660254037844387076, 1.000000000000000000, 0.8660254037844387076, 1.000000000000000000, 0.9330127018922194093, 0.9330127018922194093 ) ) 
 REPRESENTATION_ITEM ( '' )  );
#41291 = ORIENTED_EDGE ( 'NONE', *, *, #83461, .T. ) ;
#41292 = CARTESIAN_POINT ( 'NONE',  ( 164.9009427471078766, 270.4319544559331234, -17.40525121274953335 ) ) ;
#41293 = B_SPLINE_SURFACE_WITH_KNOTS ( 'NONE', 3, 1, ( 
 ( #15185, #39475 ),
 ( #85147, #53687 ),
 ( #78523, #8116 ),
 ( #39982, #70917 ),
 ( #84644, #1011 ),
 ( #69406, #30904 ),
 ( #86663, #31889 ),
 ( #62795, #93751 ),
 ( #46085, #15693 ),
 ( #24310, #77525 ),
 ( #37983, #23796 ),
 ( #31396, #32404 ),
 ( #23292, #63301 ),
 ( #62283, #76996 ),
 ( #94243, #61792 ),
 ( #24795, #93237 ),
 ( #92738, #76520 ),
 ( #54681, #55186 ),
 ( #55676, #68894 ),
 ( #30405, #61297 ),
 ( #3526, #71420 ),
 ( #56186, #57188 ),
 ( #40490, #25299 ),
 ( #32896, #34889 ),
 ( #41489, #87180 ),
 ( #4003, #9629 ),
 ( #11621, #50103 ),
 ( #81058, #10613 ),
 ( #65303, #72434 ),
 ( #2010, #3038 ),
 ( #88167, #18715 ) ),
 .UNSPECIFIED., .F., .F., .F.,
 ( 4, 3, 3, 3, 3, 3, 3, 3, 3, 3, 4 ),
 ( 2, 2 ),
 ( 0.000000000000000000, 0.1333490885032338480, 0.3007194338854361493, 0.4699862290245140906, 0.5844252810809331677, 0.6686540514502653521, 0.7354980260655413771, 0.8028463152565569194, 0.8633854507757173780, 0.9437142632667304687, 1.000000000000000000 ),
 ( 0.000000000000000000, 1.000000000000000000 ),
 .UNSPECIFIED. ) ;
#41294 = CARTESIAN_POINT ( 'NONE',  ( 2.749951498565457175, 23.36126292948892313, 6.180339887498949913 ) ) ;
#41295 = CARTESIAN_POINT ( 'NONE',  ( 173.7847068915813793, 272.6461794896769675, -16.37293504331134741 ) ) ;
#41296 = VERTEX_POINT ( 'NONE', #60699 ) ;
#41297 = CARTESIAN_POINT ( 'NONE',  ( 77.90166149968712261, 61.78270738046986565, 16.06607043079731412 ) ) ;
#41298 = CARTESIAN_POINT ( 'NONE',  ( 194.9757425430702824, 292.9391030023704161, -15.21392314336593365 ) ) ;
#41299 = ORIENTED_EDGE ( 'NONE', *, *, #84079, .F. ) ;
#41300 = CARTESIAN_POINT ( 'NONE',  ( 78.85260902839583252, 60.08087593534391857, 16.11113849416598853 ) ) ;
#41301 = CARTESIAN_POINT ( 'NONE',  ( 186.5927565586945036, 291.7418713830221009, 12.22326468075236860 ) ) ;
#41302 = CARTESIAN_POINT ( 'NONE',  ( 88.26279489949382651, 43.89118386701247942, -2.126167786569203244 ) ) ;
#41303 = LINE ( 'NONE', #80367, #68834 ) ;
#41304 = CARTESIAN_POINT ( 'NONE',  ( 81.48361531348861320, 50.88580826621501529, -14.60796985947813731 ) ) ;
#41305 = CARTESIAN_POINT ( 'NONE',  ( 80.32637618523892797, 44.90515637106070557, 11.18374640163626843 ) ) ;
#41306 = CARTESIAN_POINT ( 'NONE',  ( 84.65937204597994992, 49.81022611792842270, -13.17500266760843353 ) ) ;
#41307 = EDGE_LOOP ( 'NONE', ( #98192, #34218, #88474, #48588 ) ) ;
#41308 = VERTEX_POINT ( 'NONE', #66334 ) ;
#41309 = CARTESIAN_POINT ( 'NONE',  ( 175.1720010258828495, 258.8074648690770800, 12.63278887511889081 ) ) ;
#41310 = B_SPLINE_CURVE_WITH_KNOTS ( 'NONE', 3,
 ( #10462, #34744, #27165, #11967, #4869, #97101, #41338, #42827, #73761, #27668, #65152, #81891, #3383, #58536, #34255, #12468, #96099, #35749, #57540, #66646, #97576, #28147, #95614, #33780 ),
 .UNSPECIFIED., .F., .F.,
 ( 4, 2, 2, 2, 2, 2, 2, 2, 2, 2, 2, 4 ),
 ( 0.000000000000000000, 0.1249999999999845401, 0.2499999999999690803, 0.3749999999999535927, 0.4374999999999542588, 0.4999999999999549249, 0.5624999999999555911, 0.6249999999999563682, 0.6874999999999570344, 0.7499999999999577005, 0.8749999999999787947, 1.000000000000000000 ),
 .UNSPECIFIED. ) ;
#41311 = EDGE_LOOP ( 'NONE', ( #79263, #8388, #22396, #66011 ) ) ;
#41312 = CARTESIAN_POINT ( 'NONE',  ( 21.20245638554209222, 36.22472881207375650, 10.00000000000000000 ) ) ;
#41314 = ORIENTED_EDGE ( 'NONE', *, *, #23774, .T. ) ;
#41313 = EDGE_CURVE ( 'NONE', #25484, #34369, #98248, .T. ) ;
#41315 = CARTESIAN_POINT ( 'NONE',  ( 74.60301285042477559, 56.94764521179947536, 16.05680618570769624 ) ) ;
#41316 = DIRECTION ( 'NONE',  ( -1.000000000000000000, -1.804112415015878984E-15, 0.000000000000000000 ) ) ;
#41317 = VERTEX_POINT ( 'NONE', #67835 ) ;
#41318 = CARTESIAN_POINT ( 'NONE',  ( 82.21903993916642150, 41.17462734708961847, 3.239289935595443648 ) ) ;
#41319 = CARTESIAN_POINT ( 'NONE',  ( 190.3365032855578249, 300.9745011048501624, 3.518936879699320563 ) ) ;
#41320 = LINE ( 'NONE', #26644, #61087 ) ;
#41321 = CARTESIAN_POINT ( 'NONE',  ( 146.9370072200009645, 276.1446333132804511, -3.799807221059707363 ) ) ;
#41323 = EDGE_CURVE ( 'NONE', #58606, #11558, #98755, .T. ) ;
#41322 = CARTESIAN_POINT ( 'NONE',  ( 201.3715986869907510, 281.8611552031986776, -17.89433714524984964 ) ) ;
#41324 = DIRECTION ( 'NONE',  ( -0.8660254037844379305, -0.5000000000000014433, -0.000000000000000000 ) ) ;
#41325 = CARTESIAN_POINT ( 'NONE',  ( 153.9970851639660623, 279.5717529699742840, 2.172531455066414097 ) ) ;
#41326 = B_SPLINE_CURVE_WITH_KNOTS ( 'NONE', 3,
 ( #90908, #44240, #89899, #60428, #59431, #37148, #51868, #50853, #82805, #5751, #83792, #27584, #68049, #74689, #19977, #43744, #81803, #82316, #12379, #36146, #91385, #21457, #12888, #13854, #52345, #90410, #20477, #58929, #20985, #98971, #35661, #29556, #43245, #58451, #89423, #66561, #13374, #1540, #32422, #1026, #17209, #62809, #63318, #70934, #39995, #24812, #9645, #71437 ),
 .UNSPECIFIED., .F., .F.,
 ( 4, 2, 2, 2, 2, 2, 2, 2, 2, 2, 2, 2, 2, 2, 2, 2, 2, 2, 2, 2, 2, 2, 2, 4 ),
 ( 0.0005856873627484591917, 0.001016685950634623565, 0.001232185244577682116, 0.001339934891549285009, 0.001447684538520887902, 0.001663183832464095856, 0.001878683126407304027, 0.002309681714293799950, 0.003171678890066790928, 0.004033676065839783206, 0.004895673241612774618, 0.005326671829499233027, 0.005542171123442425802, 0.005649920770414057318, 0.005703795593899839249, 0.005757670417385620312, 0.005811545240871401376, 0.005865420064357183307, 0.005973169711328742831, 0.006188669005271752593, 0.006619667593157770383, 0.007050666181043788172, 0.007266165474986736351, 0.007481664768929684531 ),
 .UNSPECIFIED. ) ;
#41327 = CARTESIAN_POINT ( 'NONE',  ( 133.4351425849996531, 247.8458772461660544, 9.188101187500095079 ) ) ;
#41328 = VERTEX_POINT ( 'NONE', #29337 ) ;
#41329 = CARTESIAN_POINT ( 'NONE',  ( 32.30839531297598910, 123.0650415295850593, 203.6502102582797420 ) ) ;
#41330 = FACE_OUTER_BOUND ( 'NONE', #29641, .T. ) ;
#41331 = CARTESIAN_POINT ( 'NONE',  ( 40.03666203415436797, 35.06628583063844928, -9.188101187500006262 ) ) ;
#41332 = ORIENTED_EDGE ( 'NONE', *, *, #5131, .T. ) ;
#41333 = AXIS2_PLACEMENT_3D ( 'NONE', #10471, #80921, #72801 ) ;
#41335 = ORIENTED_EDGE ( 'NONE', *, *, #24098, .T. ) ;
#41334 = CARTESIAN_POINT ( 'NONE',  ( 31.15319227796116053, 18.39040679176984128, -6.890680421881970419E-14 ) ) ;
#41336 = CARTESIAN_POINT ( 'NONE',  ( 39.77289032284286208, 58.49985355908044937, -10.00000000000000000 ) ) ;
#41337 = CARTESIAN_POINT ( 'NONE',  ( 180.3486785659322891, 255.9976438602005260, 1.309110463909484157 ) ) ;
#41338 = CARTESIAN_POINT ( 'NONE',  ( 76.24760352746896785, 65.19682467712520690, -14.16189420828948542 ) ) ;
#41339 = DIRECTION ( 'NONE',  ( 0.000000000000000000, 0.000000000000000000, 1.000000000000000000 ) ) ;
#41340 = CARTESIAN_POINT ( 'NONE',  ( 156.6370339646614411, 279.1166159043581843, 7.320210838852614366 ) ) ;
#41341 = DIRECTION ( 'NONE',  ( 1.000000000000000000, 0.000000000000000000, -0.000000000000000000 ) ) ;
#41342 = DIRECTION ( 'NONE',  ( -0.8660254037844387076, -0.4999999999999998890, -0.000000000000000000 ) ) ;
#41343 = AXIS2_PLACEMENT_3D ( 'NONE', #86139, #24277, #16669 ) ;
#41344 = CARTESIAN_POINT ( 'NONE',  ( 172.8794231584638226, 280.7410324931668697, 13.92705740956398053 ) ) ;
#41345 = DIRECTION ( 'NONE',  ( 0.9403255362191060840, -0.3402761906661271873, 0.000000000000000000 ) ) ;
#41346 = CARTESIAN_POINT ( 'NONE',  ( 177.0478225817679458, 255.9438551104777275, -7.283735771377678248 ) ) ;
#41347 = ORIENTED_EDGE ( 'NONE', *, *, #21213, .F. ) ;
#41348 = CARTESIAN_POINT ( 'NONE',  ( 185.0903458666867891, 273.1516923159391581, -16.67643005644730536 ) ) ;
#41349 = CARTESIAN_POINT ( 'NONE',  ( 193.7862695136616651, 274.3493697269946097, 16.30071627112327803 ) ) ;
#41350 = ORIENTED_EDGE ( 'NONE', *, *, #36896, .F. ) ;
#41351 = DIRECTION ( 'NONE',  ( -0.000000000000000000, 0.000000000000000000, -1.000000000000000000 ) ) ;
#41352 = CARTESIAN_POINT ( 'NONE',  ( 205.0491312206212342, 269.1753787081169662, -2.999829222793530370 ) ) ;
#41353 = CARTESIAN_POINT ( 'NONE',  ( 191.5024861053093730, 298.9549596202882640, -10.70987072427270803 ) ) ;
#41354 = CARTESIAN_POINT ( 'NONE',  ( 149.7128599965862463, 271.3367152699035501, 12.33532264622322394 ) ) ;
#41355 = CARTESIAN_POINT ( 'NONE',  ( 163.1014434023538513, 248.1470085697407058, 9.692260209037655727 ) ) ;
#41357 = CARTESIAN_POINT ( 'NONE',  ( 151.4940044683453095, 274.9262206533563813, -9.273972269532857027 ) ) ;
#41356 = CARTESIAN_POINT ( 'NONE',  ( 160.4962995477943650, 275.9333967852908813, 14.18032076246626794 ) ) ;
#41358 = CARTESIAN_POINT ( 'NONE',  ( 200.1754978754242984, 267.3235950566412953, 6.315888745726680575 ) ) ;
#41359 = ORIENTED_EDGE ( 'NONE', *, *, #63303, .F. ) ;
#41360 = AXIS2_PLACEMENT_3D ( 'NONE', #28323, #82083, #42032 ) ;
#41361 = CARTESIAN_POINT ( 'NONE',  ( 72.57128799697304089, 62.22197114735462975, -14.43632866411172344 ) ) ;
#41362 = CARTESIAN_POINT ( 'NONE',  ( 193.4852642841095189, 276.0130112962725093, -16.67970642947549464 ) ) ;
#41363 = ADVANCED_FACE ( 'NONE', ( #52611 ), #59718, .T. ) ;
#41364 = LINE ( 'NONE', #79428, #38641 ) ;
#41365 = VECTOR ( 'NONE', #47019, 1000.000000000000114 ) ;
#41366 = CARTESIAN_POINT ( 'NONE',  ( 152.9262073036446168, 265.7710344717137900, 16.19159804214501008 ) ) ;
#41367 = EDGE_CURVE ( 'NONE', #52913, #33351, #6536, .T. ) ;
#41368 = CARTESIAN_POINT ( 'NONE',  ( 80.80800637050489854, 42.99464212843047051, -9.644767597250195834 ) ) ;
#41369 = CARTESIAN_POINT ( 'NONE',  ( 67.04009420809389042, 68.98588012621723919, 2.960418080124604945 ) ) ;
#41370 = CARTESIAN_POINT ( 'NONE',  ( -7.294332625736643649, 178.8464784336661637, 1.353441290958777525E-15 ) ) ;
#41371 = EDGE_CURVE ( 'NONE', #16493, #41560, #56894, .T. ) ;
#41372 = CARTESIAN_POINT ( 'NONE',  ( 93.32716752435031538, 230.8149278399160949, -9.188101187500095079 ) ) ;
#41373 = CARTESIAN_POINT ( 'NONE',  ( 203.5080190724872011, 278.1607665491929993, -15.47044080916498743 ) ) ;
#41374 = CARTESIAN_POINT ( 'NONE',  ( 88.09111776262265892, 44.56188567158400815, -5.102872454969324068 ) ) ;
#41375 = DIRECTION ( 'NONE',  ( -1.000000000000000000, 0.000000000000000000, 0.000000000000000000 ) ) ;
#41376 = EDGE_CURVE ( 'NONE', #95472, #7334, #12132, .T. ) ;
#41377 = CARTESIAN_POINT ( 'NONE',  ( 180.9780804914473720, 282.7163897586885923, -16.62997927953544774 ) ) ;
#41378 = CARTESIAN_POINT ( 'NONE',  ( 74.45626529801648985, 55.41543688963572833, -16.12783148945726452 ) ) ;
#41379 = CARTESIAN_POINT ( 'NONE',  ( -110.0000000000000000, 15.00000000000000000, 59.99999999999999289 ) ) ;
#41380 = CARTESIAN_POINT ( 'NONE',  ( 161.7651517240504688, 282.1360828662558902, 5.605791128093589037 ) ) ;
#41382 = CARTESIAN_POINT ( 'NONE',  ( 207.6555576926778883, 270.9770189326688410, -1.235081510489080436 ) ) ;
#41381 = DIRECTION ( 'NONE',  ( -0.000000000000000000, -0.000000000000000000, -1.000000000000000000 ) ) ;
#41383 = CARTESIAN_POINT ( 'NONE',  ( 177.8726909305742652, 289.9607890038341793, 9.707458997688759084 ) ) ;
#41384 = CARTESIAN_POINT ( 'NONE',  ( 158.3585752585947262, 263.3710999200782226, 17.79390465796247156 ) ) ;
#41385 = CARTESIAN_POINT ( 'NONE',  ( 76.83221134703946120, 55.52632626272433924, -16.15978416529669914 ) ) ;
#41386 = CARTESIAN_POINT ( 'NONE',  ( 147.1562325744354496, 245.7677522451417929, -5.000000000000041744 ) ) ;
#41387 = CARTESIAN_POINT ( 'NONE',  ( 82.20432729060244981, 228.2677522451419350, -5.000000000000047962 ) ) ;
#41388 = DIRECTION ( 'NONE',  ( 0.000000000000000000, 0.000000000000000000, 1.000000000000000000 ) ) ;
#41389 = EDGE_CURVE ( 'NONE', #83009, #86318, #43613, .T. ) ;
#41390 = CARTESIAN_POINT ( 'NONE',  ( 77.02134436793002692, 63.41470467299149760, -15.46275534251473438 ) ) ;
#41391 = CARTESIAN_POINT ( 'NONE',  ( 63.96340690334295687, 216.9244531367911293, -4.594050593750046652 ) ) ;
#41392 = CARTESIAN_POINT ( 'NONE',  ( 161.1061647010182583, 251.6029326557136585, -13.56144933775657613 ) ) ;
#41393 = CARTESIAN_POINT ( 'NONE',  ( 75.31289280905393468, 53.62176160565092431, -16.53289957284814093 ) ) ;
#41394 = CARTESIAN_POINT ( 'NONE',  ( 81.51649937534789103, 59.53360007009536048, -0.2191855733945438922 ) ) ;
#41396 = CARTESIAN_POINT ( 'NONE',  ( 199.8780930708521453, 284.4479828117403031, 17.00188320299317368 ) ) ;
#41395 = LINE ( 'NONE', #72338, #88995 ) ;
#41397 = CARTESIAN_POINT ( 'NONE',  ( 11.60290295393121696, 189.0530062829863027, -4.648177544792955347E-16 ) ) ;
#41398 = CARTESIAN_POINT ( 'NONE',  ( 32.83301474718356161, 37.14336893147758900, 7.433330006724141015 ) ) ;
#41399 = CARTESIAN_POINT ( 'NONE',  ( 82.60066728560789784, 50.87129046802179033, 14.76979220338051491 ) ) ;
#41400 = CARTESIAN_POINT ( 'NONE',  ( -19.65312891409030271, 93.06504152958497400, 177.5919119679930134 ) ) ;
#41401 = ORIENTED_EDGE ( 'NONE', *, *, #91868, .F. ) ;
#41402 = CARTESIAN_POINT ( 'NONE',  ( 20.18540868186541459, 12.44966523072493914, -2.296566073217252530E-15 ) ) ;
#41403 = CARTESIAN_POINT ( 'NONE',  ( 81.12205585946965414, 208.4548013555409796, -4.594050593750042211 ) ) ;
#41404 = CARTESIAN_POINT ( 'NONE',  ( 94.05805000844991071, 225.1115022471902307, 10.00000000000009592 ) ) ;
#41405 = CARTESIAN_POINT ( 'NONE',  ( -89.11465314115665137, 93.37593066204027537, -37.49999999999999289 ) ) ;
#41406 = CARTESIAN_POINT ( 'NONE',  ( 147.0314375879888757, 275.9810751181479986, -5.168577011192616588 ) ) ;
#41407 = CARTESIAN_POINT ( 'NONE',  ( 31.94941146435350987, 203.6868197944959320, 22.50000000000001066 ) ) ;
#41408 = AXIS2_PLACEMENT_3D ( 'NONE', #53685, #21807, #84642 ) ;
#41409 = FACE_OUTER_BOUND ( 'NONE', #51466, .T. ) ;
#41410 = CARTESIAN_POINT ( 'NONE',  ( 189.7553949637821802, 286.5528735061270140, 16.71718042389977654 ) ) ;
#41411 = CARTESIAN_POINT ( 'NONE',  ( 72.56680254073344827, 71.38637538794351656, 5.777867564336608197 ) ) ;
#41412 = CARTESIAN_POINT ( 'NONE',  ( 133.5343746642906524, 241.2365022471902307, 10.00000000000009592 ) ) ;
#41413 = CARTESIAN_POINT ( 'NONE',  ( 13.06432082636536762, 189.8967562850346837, -4.648177544792955347E-16 ) ) ;
#41414 = CARTESIAN_POINT ( 'NONE',  ( 19.30862341340331412, 34.08080186712593473, -3.090169943749475845 ) ) ;
#41415 = ORIENTED_EDGE ( 'NONE', *, *, #89458, .T. ) ;
#41416 = CARTESIAN_POINT ( 'NONE',  ( 185.7548115650120906, 271.5664750103190954, 16.84803787444293022 ) ) ;
#41417 = ORIENTED_EDGE ( 'NONE', *, *, #94138, .F. ) ;
#41418 = CARTESIAN_POINT ( 'NONE',  ( 162.6937333994314656, 248.8531830095558632, 10.02305144031113926 ) ) ;
#41419 = DIRECTION ( 'NONE',  ( -0.9184028970038772277, -0.3956464567955659817, 0.000000000000000000 ) ) ;
#41420 = CARTESIAN_POINT ( 'NONE',  ( 201.1755594471486859, 282.2007051268825535, -18.15567516623250910 ) ) ;
#41421 = ORIENTED_EDGE ( 'NONE', *, *, #88809, .F. ) ;
#41422 = CARTESIAN_POINT ( 'NONE',  ( 77.10594840515625492, 62.91113679231831668, -15.28126102291101063 ) ) ;
#41423 = EDGE_LOOP ( 'NONE', ( #72151, #33748, #93859, #91188 ) ) ;
#41424 = CARTESIAN_POINT ( 'NONE',  ( 192.3546171244506411, 291.9418057657312602, 14.85604634385901690 ) ) ;
#41425 = CARTESIAN_POINT ( 'NONE',  ( 167.3984581500753848, 247.5600430218893280, 3.593632883392327670 ) ) ;
#41426 = CARTESIAN_POINT ( 'NONE',  ( 81.93977088949127108, 44.53106330606377838, 10.63662565672798443 ) ) ;
#41427 = EDGE_CURVE ( 'NONE', #8285, #8043, #96264, .T. ) ;
#41428 = ORIENTED_EDGE ( 'NONE', *, *, #95099, .T. ) ;
#41429 = CARTESIAN_POINT ( 'NONE',  ( 46.74164954608104949, 27.39040679176987325, -6.890680421881970419E-14 ) ) ;
#41430 = CARTESIAN_POINT ( 'NONE',  ( 35.44910642356613550, 21.26216523072496400, -2.296566073217252530E-15 ) ) ;
#41431 = VECTOR ( 'NONE', #45966, 1000.000000000000114 ) ;
#41432 = CARTESIAN_POINT ( 'NONE',  ( 80.17887552957238029, 44.29837527985885970, 11.40047595680318970 ) ) ;
#41433 = CARTESIAN_POINT ( 'NONE',  ( -27.52599651137557046, 146.7012482093458914, 1.732050807568941142 ) ) ;
#41434 = CARTESIAN_POINT ( 'NONE',  ( 167.7832046799460954, 276.7730461828406874, 15.64290657898813031 ) ) ;
#41435 = CARTESIAN_POINT ( 'NONE',  ( 82.65473243480592203, 40.50376448046697675, -0.5611958088008396350 ) ) ;
#41436 = VECTOR ( 'NONE', #44726, 1000.000000000000000 ) ;
#41437 = ORIENTED_EDGE ( 'NONE', *, *, #55034, .F. ) ;
#41438 = ORIENTED_EDGE ( 'NONE', *, *, #36924, .T. ) ;
#41439 = CARTESIAN_POINT ( 'NONE',  ( 186.2875372408365990, 298.3389836698145814, 1.055114130040206710 ) ) ;
#41441 = CARTESIAN_POINT ( 'NONE',  ( 148.0826818691893152, 274.1602666119424043, -9.371267383421741926 ) ) ;
#41440 = CARTESIAN_POINT ( 'NONE',  ( 163.7064929935861244, 247.0990319366274548, 6.401263337036986023 ) ) ;
#41442 = CARTESIAN_POINT ( 'NONE',  ( 85.59269861019149062, 48.32250421001948126, -11.70547994120720325 ) ) ;
#41443 = CARTESIAN_POINT ( 'NONE',  ( 155.6435836392643637, 261.0644005951349982, 17.58841156286628049 ) ) ;
#41444 = PLANE ( 'NONE',  #56068 ) ;
#41445 = CARTESIAN_POINT ( 'NONE',  ( -57.88150100324660485, 35.92665207732902388, -10.00000000000000000 ) ) ;
#41446 = CARTESIAN_POINT ( 'NONE',  ( 207.4225649187019087, 271.3805742549917568, -3.927239063805231023 ) ) ;
#41447 = CARTESIAN_POINT ( 'NONE',  ( 166.1957201800340442, 265.4536997604227508, 16.55608710447817344 ) ) ;
#41448 = CARTESIAN_POINT ( 'NONE',  ( 79.45469543192598394, 59.63697030301000979, 16.53293242656296869 ) ) ;
#41449 = CARTESIAN_POINT ( 'NONE',  ( 92.62404252742298638, 212.0327760586659451, 1.948934522072303157E-15 ) ) ;
#41450 = ORIENTED_EDGE ( 'NONE', *, *, #86480, .F. ) ;
#41451 = DIRECTION ( 'NONE',  ( -1.000000000000000000, 0.000000000000000000, 0.000000000000000000 ) ) ;
#41452 = CARTESIAN_POINT ( 'NONE',  ( 166.8158164543628459, 278.2249326526564914, -13.34744090285348683 ) ) ;
#41453 = ORIENTED_EDGE ( 'NONE', *, *, #2699, .T. ) ;
#41454 = ORIENTED_EDGE ( 'NONE', *, *, #7583, .T. ) ;
#41455 = CARTESIAN_POINT ( 'NONE',  ( 80.30560875578385094, 44.94112661401950248, -11.22675700711674374 ) ) ;
#41456 = CARTESIAN_POINT ( 'NONE',  ( 164.1828359708729863, 281.6525977458860552, 8.811343294891619493 ) ) ;
#41457 = CARTESIAN_POINT ( 'NONE',  ( 146.5046981847821428, 276.8934145268504494, 0.02269072295920678689 ) ) ;
#41458 = CARTESIAN_POINT ( 'NONE',  ( 68.25940382258694683, 65.54188025616944913, 10.45666766922404101 ) ) ;
#41459 = CARTESIAN_POINT ( 'NONE',  ( 206.8775514429320026, 272.3245652858344670, -9.838455694836268250 ) ) ;
#41461 = B_SPLINE_CURVE_WITH_KNOTS ( 'NONE', 3,
 ( #54995, #54480, #47397, #79358 ),
 .UNSPECIFIED., .F., .F.,
 ( 4, 4 ),
 ( 0.01697285580833185481, 0.02587605460899505133 ),
 .UNSPECIFIED. ) ;
#41460 = CARTESIAN_POINT ( 'NONE',  ( 207.9670239186021377, 270.4375436045261836, 3.151456135821919968 ) ) ;
#41462 = CARTESIAN_POINT ( 'NONE',  ( 84.74801659416949917, 228.9244531367911293, -4.594050593750046652 ) ) ;
#41463 = EDGE_LOOP ( 'NONE', ( #10077, #485, #76809, #32158 ) ) ;
#41464 = CARTESIAN_POINT ( 'NONE',  ( 200.4606599504492408, 283.4389473774714361, -18.16209435128261873 ) ) ;
#41465 = ORIENTED_EDGE ( 'NONE', *, *, #25964, .F. ) ;
#41466 = B_SPLINE_CURVE_WITH_KNOTS ( 'NONE', 3,
 ( #49028, #25215, #49514, #95169, #65217, #88585, #40894, #48531, #95680, #2954, #80469, #25738, #96159, #11039, #72850, #33844, #10032, #41916, #33319, #3442, #34319, #26722, #96658, #57604, #79468, #50020, #73333, #80974, #63722, #11539, #42399, #50503, #56617, #89093, #3920, #58112, #19642, #40402, #71843, #81457, #71339, #1931, #32817, #56100, #87091, #17628, #2441, #28712, #90566, #74344 ),
 .UNSPECIFIED., .F., .F.,
 ( 4, 2, 2, 2, 2, 2, 2, 2, 2, 2, 2, 2, 2, 2, 2, 2, 2, 2, 2, 2, 2, 2, 2, 2, 4 ),
 ( 0.0004158906835773414643, 0.001427088945389863150, 0.001932688076296212518, 0.002185487641749338846, 0.002311887424475821563, 0.002438287207202304279, 0.002564686989928787429, 0.002691086772655270579, 0.002943886338108236012, 0.003449485469014167312, 0.004460683730825979604, 0.005471881992637791028, 0.005977481123543697608, 0.006230280688996726358, 0.006483080254449755109, 0.006546280145813108790, 0.006609480037176460737, 0.006672679928539813551, 0.006735879819903165498, 0.006988679385356588031, 0.007494278516263348962, 0.007747078081716728126, 0.007999877647170108158, 0.008252677212623488190, 0.008505476778076868222 ),
 .UNSPECIFIED. ) ;
#41467 = CARTESIAN_POINT ( 'NONE',  ( 75.93815686453476133, 64.70849926024720844, -14.31753493372995933 ) ) ;
#41468 = CARTESIAN_POINT ( 'NONE',  ( 192.3713340522295709, 271.8780416168410170, 15.57788208939756380 ) ) ;
#41469 = CARTESIAN_POINT ( 'NONE',  ( 87.48880955142448101, 44.86412769470708639, -6.596395727433105094 ) ) ;
#41470 = DIRECTION ( 'NONE',  ( -0.000000000000000000, -1.000000000000000000, -0.000000000000000000 ) ) ;
#41471 = CARTESIAN_POINT ( 'NONE',  ( 87.76435223195018409, 44.22492802364795494, 4.686297260842065882 ) ) ;
#41473 = CARTESIAN_POINT ( 'NONE',  ( 156.6823612109870396, 259.2651850631482375, 17.57884712310819708 ) ) ;
#41472 = AXIS2_PLACEMENT_3D ( 'NONE', #98705, #76866, #7464 ) ;
#41474 = CARTESIAN_POINT ( 'NONE',  ( 160.7043946034031308, 275.5602053013725481, 12.99197331405084910 ) ) ;
#41475 = CARTESIAN_POINT ( 'NONE',  ( 206.6703863510205679, 272.6833857505801006, -10.72500664779635393 ) ) ;
#41476 = CARTESIAN_POINT ( 'NONE',  ( 191.5959239871531850, 271.5537089687533694, 14.17158143004904325 ) ) ;
#41477 = CARTESIAN_POINT ( 'NONE',  ( 174.7055293015415600, 283.6856165666803236, 13.49174788089805865 ) ) ;
#41478 = EDGE_CURVE ( 'NONE', #85923, #88235, #99741, .T. ) ;
#41479 = VECTOR ( 'NONE', #51557, 1000.000000000000000 ) ;
#41480 = FACE_OUTER_BOUND ( 'NONE', #24004, .T. ) ;
#41481 = CARTESIAN_POINT ( 'NONE',  ( -9.055497838557601042, 23.87190447404380222, 177.5919119679930134 ) ) ;
#41482 = ORIENTED_EDGE ( 'NONE', *, *, #12249, .F. ) ;
#41483 = EDGE_CURVE ( 'NONE', #57725, #7407, #53610, .T. ) ;
#41484 = CARTESIAN_POINT ( 'NONE',  ( 149.0570874715264154, 274.4997098312325079, 9.090637939377691268 ) ) ;
#41485 = B_SPLINE_CURVE_WITH_KNOTS ( 'NONE', 3,
 ( #12010, #68177, #91031, #4909 ),
 .UNSPECIFIED., .F., .F.,
 ( 4, 4 ),
 ( 0.01048086686357619333, 0.01574798419196724725 ),
 .UNSPECIFIED. ) ;
#41486 = CARTESIAN_POINT ( 'NONE',  ( 178.3666971430922672, 291.5231582936299333, 9.051735255157939974 ) ) ;
#41487 = CARTESIAN_POINT ( 'NONE',  ( 84.80509911768557174, 43.31890675800398327, 5.469368207548569671 ) ) ;
#41488 = CARTESIAN_POINT ( 'NONE',  ( 167.6848733776141671, 249.9537906194314303, 6.968395254000899541 ) ) ;
#41489 = CARTESIAN_POINT ( 'NONE',  ( 83.43050110256683638, 51.89332412091456348, 15.00139857044202074 ) ) ;
#41490 = FACE_OUTER_BOUND ( 'NONE', #90970, .T. ) ;
#41491 = FACE_OUTER_BOUND ( 'NONE', #49852, .T. ) ;
#41492 = EDGE_CURVE ( 'NONE', #78230, #16775, #19151, .T. ) ;
#41493 = ORIENTED_EDGE ( 'NONE', *, *, #100184, .F. ) ;
#41494 = CYLINDRICAL_SURFACE ( 'NONE', #35263, 17.82106496071139645 ) ;
#41495 = VECTOR ( 'NONE', #52096, 1000.000000000000000 ) ;
#41496 = VECTOR ( 'NONE', #25795, 1000.000000000000000 ) ;
#41497 = CARTESIAN_POINT ( 'NONE',  ( 75.42132300406277068, 63.53713694569018600, -14.66775701755491745 ) ) ;
#41499 = CARTESIAN_POINT ( 'NONE',  ( 74.32283972738726163, 55.33658384528776963, 16.60204640396233344 ) ) ;
#41498 = CARTESIAN_POINT ( 'NONE',  ( 180.4957999564819886, 267.2278171865779086, -15.18777883605170409 ) ) ;
#41500 = CARTESIAN_POINT ( 'NONE',  ( 69.66767063274500060, 62.28281038103965273, -13.55241073290247478 ) ) ;
#41501 = CARTESIAN_POINT ( 'NONE',  ( 28.73071361209859731, 38.36126292948897287, 6.180339887498949913 ) ) ;
#41502 = DIRECTION ( 'NONE',  ( -0.9932214622066116716, 0.1162373735601425623, 0.000000000000000000 ) ) ;
#41503 = CARTESIAN_POINT ( 'NONE',  ( 203.1526193585190470, 278.7763369107815379, -16.67658907091021447 ) ) ;
#41504 = DIRECTION ( 'NONE',  ( -0.000000000000000000, -0.000000000000000000, -1.000000000000000000 ) ) ;
#41505 = DIRECTION ( 'NONE',  ( 0.000000000000000000, 0.000000000000000000, 1.000000000000000000 ) ) ;
#41506 = CARTESIAN_POINT ( 'NONE',  ( 205.8387202508380653, 272.3240174465572636, -9.430873374051206071 ) ) ;
#41507 = CARTESIAN_POINT ( 'NONE',  ( 161.1232569692349443, 251.5733279787459367, -14.02750397520710557 ) ) ;
#41508 = CARTESIAN_POINT ( 'NONE',  ( 10.18907585680922878, 170.5643266524159571, -9.188101187500093303 ) ) ;
#41509 = CARTESIAN_POINT ( 'NONE',  ( 81.12568207579826662, 44.96798002130291394, 10.84245638387497657 ) ) ;
#41510 = ORIENTED_EDGE ( 'NONE', *, *, #96425, .F. ) ;
#41511 = CARTESIAN_POINT ( 'NONE',  ( 87.37270799788964837, 45.80620788475513905, 8.330021955613661433 ) ) ;
#41512 = CARTESIAN_POINT ( 'NONE',  ( 181.4283053378885597, 267.7238133557910373, 16.48022347432943135 ) ) ;
#41513 = CARTESIAN_POINT ( 'NONE',  ( 71.86256228778262312, 72.60615528678948749, -0.5650332253008816252 ) ) ;
#41514 = CARTESIAN_POINT ( 'NONE',  ( 30.97333845187074175, 194.8149278399160664, -9.188101187500095079 ) ) ;
#41515 = FACE_OUTER_BOUND ( 'NONE', #75342, .T. ) ;
#41516 = CARTESIAN_POINT ( 'NONE',  ( 146.8358616138309571, 276.3198226421291679, 4.054088818585255716 ) ) ;
#41517 = CARTESIAN_POINT ( 'NONE',  ( 40.07075743699687109, 22.94473085651394939, 1.475505719884397138E-15 ) ) ;
#41518 = CARTESIAN_POINT ( 'NONE',  ( 178.1014170928845033, 292.3538449268187378, 5.578751321692007714 ) ) ;
#41519 = PRODUCT_RELATED_PRODUCT_CATEGORY ( 'part', '', ( #65334 ) ) ;
#41520 = CARTESIAN_POINT ( 'NONE',  ( 177.4918489660068417, 292.2262405376345669, 2.581417131937560061 ) ) ;
#41521 = CARTESIAN_POINT ( 'NONE',  ( 149.3412472373495063, 271.9803674496423014, 11.49645634555178297 ) ) ;
#41522 = CARTESIAN_POINT ( 'NONE',  ( 179.3634369656868728, 278.6207563196031174, -17.18449886317435826 ) ) ;
#41523 = CARTESIAN_POINT ( 'NONE',  ( 173.2412943989675398, 277.7050541934257240, 16.79641741871846250 ) ) ;
#41524 = CARTESIAN_POINT ( 'NONE',  ( 167.0813381624552392, 257.8573864978880579, -15.59453214358795137 ) ) ;
#41525 = CARTESIAN_POINT ( 'NONE',  ( 83.73865579866679809, 51.98612588642360777, 14.96617132975018372 ) ) ;
#41526 = CARTESIAN_POINT ( 'NONE',  ( 182.6015398117219490, 296.6291243770974120, 1.816064570435409253 ) ) ;
#41527 = CARTESIAN_POINT ( 'NONE',  ( 84.17092664857760553, 212.7365022471902023, 10.00000000000009592 ) ) ;
#41528 = CARTESIAN_POINT ( 'NONE',  ( 177.8222571804544430, 286.5223583772871621, 13.77940225188420875 ) ) ;
#41529 = CARTESIAN_POINT ( 'NONE',  ( 178.2087173759056498, 281.9494420025493469, 16.33014707258442755 ) ) ;
#41530 = CARTESIAN_POINT ( 'NONE',  ( 56.25097556847656932, 191.0327760586659451, 1.948934522072303157E-15 ) ) ;
#41531 = CARTESIAN_POINT ( 'NONE',  ( 197.9002057575219453, 287.8737841300738296, 18.01270164875645818 ) ) ;
#41532 = ORIENTED_EDGE ( 'NONE', *, *, #59842, .F. ) ;
#41533 = CARTESIAN_POINT ( 'NONE',  ( -9.885233179245682678, 85.35632536023292971, 14.27670553151784283 ) ) ;
#41534 = CARTESIAN_POINT ( 'NONE',  ( 151.0426280674448378, 269.0334894088936153, -15.84467774422408581 ) ) ;
#41535 = CARTESIAN_POINT ( 'NONE',  ( 67.42404893004047040, 67.25264271294523155, -8.643519966047881198 ) ) ;
#41536 = VERTEX_POINT ( 'NONE', #57109 ) ;
#41537 = CARTESIAN_POINT ( 'NONE',  ( 171.1309707950161680, 286.4780903314298826, 7.470031319074768028 ) ) ;
#41538 = CARTESIAN_POINT ( 'NONE',  ( 164.6649740431187183, 245.4388940607451843, -1.430729255012818557 ) ) ;
#41539 = CARTESIAN_POINT ( 'NONE',  ( 193.3266656173557294, 295.7953880232976758, 13.75377347669239825 ) ) ;
#41540 = CARTESIAN_POINT ( 'NONE',  ( 95.19470834736912934, 215.7677522451417929, -5.000000000000041744 ) ) ;
#41541 = CARTESIAN_POINT ( 'NONE',  ( 31.61033844661487180, 20.11110640527293825, -2.839279412974138328 ) ) ;
#41542 = CARTESIAN_POINT ( 'NONE',  ( 202.8787628851569593, 279.2506702366259788, 17.01435431865322556 ) ) ;
#41544 = EDGE_CURVE ( 'NONE', #4742, #43464, #89838, .T. ) ;
#41543 = AXIS2_PLACEMENT_3D ( 'NONE', #1975, #48058, #70361 ) ;
#41545 = DIRECTION ( 'NONE',  ( 0.8660254037844384856, 0.5000000000000004441, 0.000000000000000000 ) ) ;
#41546 = ORIENTED_EDGE ( 'NONE', *, *, #7083, .F. ) ;
#41547 = CARTESIAN_POINT ( 'NONE',  ( 16.25825050073692069, 15.10170272979925876, -7.433330006724141015 ) ) ;
#41548 = CARTESIAN_POINT ( 'NONE',  ( 171.7111136159620344, 252.7683153775072071, 8.549686029849182134 ) ) ;
#41549 = LINE ( 'NONE', #3096, #44026 ) ;
#41550 = ORIENTED_EDGE ( 'NONE', *, *, #86564, .T. ) ;
#41551 = CARTESIAN_POINT ( 'NONE',  ( 72.03955433498997252, 71.50824183410490775, -5.808600603169774779 ) ) ;
#41552 = CARTESIAN_POINT ( 'NONE',  ( 82.42797444979642307, 40.90780339933488818, -0.3678846455753223554 ) ) ;
#41553 = DIRECTION ( 'NONE',  ( 1.000000000000000000, 0.000000000000000000, -1.082076799516502080E-16 ) ) ;
#41554 = CARTESIAN_POINT ( 'NONE',  ( 74.56414817410227158, 187.8759306620403322, 17.47570218321536473 ) ) ;
#41555 = ADVANCED_FACE ( 'NONE', ( #78957 ), #10037, .F. ) ;
#41556 = ORIENTED_EDGE ( 'NONE', *, *, #42609, .F. ) ;
#41557 = ORIENTED_EDGE ( 'NONE', *, *, #12926, .F. ) ;
#41559 = CARTESIAN_POINT ( 'NONE',  ( 151.0156108440694425, 269.4662454610033251, -13.81341911168381564 ) ) ;
#41558 = CARTESIAN_POINT ( 'NONE',  ( 207.3646600298985447, 271.4808684644054324, -5.284084612275558257 ) ) ;
#41560 = VERTEX_POINT ( 'NONE', #49519 ) ;
#41561 = CARTESIAN_POINT ( 'NONE',  ( 153.1627746953036535, 265.3612877299463548, -17.72069958822647351 ) ) ;
#41562 = CARTESIAN_POINT ( 'NONE',  ( 72.02714983513547509, 72.27104924840581646, -3.542005090554713576 ) ) ;
#41563 = CARTESIAN_POINT ( 'NONE',  ( 70.92012640611527274, 71.65591018854625815, -3.452294570978728050 ) ) ;
#41564 = CARTESIAN_POINT ( 'NONE',  ( 77.96869982513443631, 61.39881034122267778, -16.15742658069109439 ) ) ;
#41565 = EDGE_CURVE ( 'NONE', #19653, #92570, #72739, .T. ) ;
#41566 = CARTESIAN_POINT ( 'NONE',  ( 157.6036818288543486, 257.6694109429415107, -16.73826488331764395 ) ) ;
#41567 = CARTESIAN_POINT ( 'NONE',  ( 111.8384605302426991, 241.5024278399160949, -9.188101187500093303 ) ) ;
#41568 = CARTESIAN_POINT ( 'NONE',  ( 149.2223635749290622, 272.1862799931444670, -12.97307652490353647 ) ) ;
#41569 = CARTESIAN_POINT ( 'NONE',  ( 184.1784204912316909, 288.8332414524454634, -13.14701115336322346 ) ) ;
#41570 = VERTEX_POINT ( 'NONE', #13044 ) ;
#41571 = AXIS2_PLACEMENT_3D ( 'NONE', #90012, #65175, #11001 ) ;
#41572 = VECTOR ( 'NONE', #77510, 1000.000000000000000 ) ;
#41573 = CARTESIAN_POINT ( 'NONE',  ( 201.4453672590843212, 280.6253616217601916, 16.44210273926617560 ) ) ;
#41574 = ORIENTED_EDGE ( 'NONE', *, *, #90858, .F. ) ;
#41575 = CARTESIAN_POINT ( 'NONE',  ( 30.66616357392367220, 39.74646525600392977, 2.839279412974139660 ) ) ;
#41576 = CARTESIAN_POINT ( 'NONE',  ( 159.3528137482544196, 254.6398255893999476, 16.73628156321660398 ) ) ;
#41577 = CARTESIAN_POINT ( 'NONE',  ( 78.46624349761390249, 48.01460221765250225, -14.00587743556854115 ) ) ;
#41578 = CARTESIAN_POINT ( 'NONE',  ( 57.11665387649598813, 203.7833772461660828, -9.188101187500095079 ) ) ;
#41579 = CARTESIAN_POINT ( 'NONE',  ( 73.85129109314340212, 68.53037146055885387, 10.90305250113367741 ) ) ;
#41580 = CARTESIAN_POINT ( 'NONE',  ( 191.0816511748900268, 299.6838671013740623, 7.311127128005925790 ) ) ;
#41581 = CARTESIAN_POINT ( 'NONE',  ( 151.0254882145115971, 269.0631765050081299, 14.78274390654921078 ) ) ;
#41582 = LINE ( 'NONE', #2613, #68975 ) ;
#41583 = VERTEX_POINT ( 'NONE', #52504 ) ;
#41584 =( BOUNDED_CURVE ( )  B_SPLINE_CURVE ( 2, ( #85878, #25510, #79755, #17924, #16404, #31588, #1729, #93950, #78723, #55383, #48822, #93447, #9312 ),
 .UNSPECIFIED., .F., .T. ) 
 B_SPLINE_CURVE_WITH_KNOTS ( ( 3, 2, 2, 2, 2, 2, 3 ),
 ( 0.8125000000000000000, 0.8149999999999999467, 0.8199999999999999512, 0.8249999999999999556, 0.8299999999999999600, 0.8349999999999999645, 0.8375000000000000222 ),
 .UNSPECIFIED. ) 
 CURVE ( )  GEOMETRIC_REPRESENTATION_ITEM ( )  RATIONAL_B_SPLINE_CURVE ( ( 0.9755282581475768211, 0.9755282581475768211, 1.000000000000000000, 0.9510565162951535312, 1.000000000000000000, 0.9510565162951535312, 1.000000000000000000, 0.9510565162951535312, 1.000000000000000000, 0.9510565162951535312, 1.000000000000000000, 0.9755282581475761550, 0.9755282581475767101 ) ) 
 REPRESENTATION_ITEM ( '' )  );
#41585 = PLANE ( 'NONE',  #77149 ) ;
#41586 = CARTESIAN_POINT ( 'NONE',  ( 147.6140518775699491, 274.9719575673779559, 8.457032797753797126 ) ) ;
#41587 = ORIENTED_EDGE ( 'NONE', *, *, #63578, .T. ) ;
#41588 = CARTESIAN_POINT ( 'NONE',  ( 171.6932237194176025, 259.4651268520354961, -13.84549871016380607 ) ) ;
#41589 = CARTESIAN_POINT ( 'NONE',  ( 69.76281041485397338, 69.71141683662550292, -5.692271621175008178 ) ) ;
#41590 = CARTESIAN_POINT ( 'NONE',  ( 160.4864031019297954, 258.1637219028588675, -17.19673236967974006 ) ) ;
#41591 = CARTESIAN_POINT ( 'NONE',  ( 81.47742755412382110, 52.42827155326802568, -15.60484105884143169 ) ) ;
#41592 = CARTESIAN_POINT ( 'NONE',  ( 148.9232972370683399, 272.7042780851529642, 12.27045554427055940 ) ) ;
#41593 = CARTESIAN_POINT ( 'NONE',  ( 177.0733235261513983, 269.7023525544009885, 16.22382760421824699 ) ) ;
#41594 = CARTESIAN_POINT ( 'NONE',  ( 205.7668501412109663, 274.2483563724483133, 11.09689540819876896 ) ) ;
#41595 = DIRECTION ( 'NONE',  ( -0.9995486091367050685, 0.03004293549036784680, 0.000000000000000000 ) ) ;
#41596 = CARTESIAN_POINT ( 'NONE',  ( 153.9188684017919968, 264.4466852765838212, -16.50884978456451790 ) ) ;
#41597 = CARTESIAN_POINT ( 'NONE',  ( 208.1415148974628266, 270.1353163636768500, 3.453641150550738725 ) ) ;
#41598 = CARTESIAN_POINT ( 'NONE',  ( 123.7191597644692393, 251.4244531367911293, -4.594050593750046652 ) ) ;
#41599 = ORIENTED_EDGE ( 'NONE', *, *, #85845, .T. ) ;
#41600 = CARTESIAN_POINT ( 'NONE',  ( 86.35622788611077283, 44.22730618112566248, -5.622056245697837795 ) ) ;
#41601 = CARTESIAN_POINT ( 'NONE',  ( 83.60889825226890082, 41.79735538044917575, 2.466802602430361091 ) ) ;
#41602 = EDGE_CURVE ( 'NONE', #29582, #45874, #82453, .T. ) ;
#41603 = CARTESIAN_POINT ( 'NONE',  ( 205.7160570675956137, 273.8316721655138508, -10.27501494681582805 ) ) ;
#41604 = CARTESIAN_POINT ( 'NONE',  ( 164.4990934228277411, 245.7262077230798809, 6.470820838822735510 ) ) ;
#41605 = CARTESIAN_POINT ( 'NONE',  ( 73.99318389990696687, 57.32182924785170286, 15.98609978358631700 ) ) ;
#41606 = CARTESIAN_POINT ( 'NONE',  ( 177.9260618338437041, 255.3518848370148078, 4.867121141759041869 ) ) ;
#41607 = VERTEX_POINT ( 'NONE', #35313 ) ;
#41608 = CARTESIAN_POINT ( 'NONE',  ( 80.44596413951620661, 57.92004253751065335, -16.60216415864725903 ) ) ;
#41609 = CARTESIAN_POINT ( 'NONE',  ( 71.81466828470752262, 72.18675276203495628, 0.5721087574936188913 ) ) ;
#41610 = CARTESIAN_POINT ( 'NONE',  ( 185.8136036613169324, 262.0491945824166464, 9.850964508789044061 ) ) ;
#41611 = CARTESIAN_POINT ( 'NONE',  ( 164.2877295051262934, 246.0923007674255416, -1.726861278304287373 ) ) ;
#41612 = CARTESIAN_POINT ( 'NONE',  ( 137.4944631173567018, 256.3149278399160380, -9.188101187500095079 ) ) ;
#41613 = EDGE_CURVE ( 'NONE', #43017, #49470, #90062, .T. ) ;
#41614 = FACE_OUTER_BOUND ( 'NONE', #27969, .T. ) ;
#41615 = CARTESIAN_POINT ( 'NONE',  ( 68.00690384560408575, 68.82080238078589218, 5.313225612992173552 ) ) ;
#41616 = CARTESIAN_POINT ( 'NONE',  ( 63.63864737692379236, 216.7369531367911293, -4.594050593750048428 ) ) ;
#41617 = AXIS2_PLACEMENT_3D ( 'NONE', #68511, #60894, #21913 ) ;
#41618 = VECTOR ( 'NONE', #48530, 1000.000000000000114 ) ;
#41619 = CARTESIAN_POINT ( 'NONE',  ( 170.6781199183338344, 250.4769293299289927, 3.472362579247760372 ) ) ;
#41620 = B_SPLINE_SURFACE_WITH_KNOTS ( 'NONE', 3, 1, ( 
 ( #33202, #1313 ),
 ( #3331, #32196 ),
 ( #18021, #1814 ),
 ( #72226, #55974 ),
 ( #86466, #78823 ),
 ( #25613, #65102 ),
 ( #94539, #48407 ),
 ( #79848, #2832 ),
 ( #95567, #26610 ),
 ( #56989, #10919 ),
 ( #57485, #97523 ),
 ( #12415, #44282 ),
 ( #58965, #42776 ),
 ( #49902, #67085 ),
 ( #88979, #59468 ),
 ( #67586, #90450 ),
 ( #35192, #4292 ),
 ( #66100, #21019 ),
 ( #82842, #80860 ),
 ( #42286, #96543 ),
 ( #58482, #20013 ),
 ( #59973, #6790 ),
 ( #53862, #39154 ),
 ( #22487, #7279 ),
 ( #31071, #77705 ),
 ( #15873, #92425 ),
 ( #8289, #45280 ),
 ( #70069, #83329 ),
 ( #30087, #13892 ),
 ( #75708, #6294 ),
 ( #68086, #99008 ) ),
 .UNSPECIFIED., .F., .F., .F.,
 ( 4, 3, 3, 3, 3, 3, 3, 3, 3, 3, 4 ),
 ( 2, 2 ),
 ( 0.000000000000000000, 0.1333490885032311002, 0.3007194338854346505, 0.4699862290245186980, 0.5844252810809363874, 0.6686540514502655741, 0.7354980260655468172, 0.8028463152565521455, 0.8633854507757170449, 0.9437142632667351316, 1.000000000000000000 ),
 ( 0.000000000000000000, 1.000000000000000000 ),
 .UNSPECIFIED. ) ;
#41621 = CARTESIAN_POINT ( 'NONE',  ( 19.36651902841724038, 19.38052372038640669, 10.00000000000000533 ) ) ;
#41622 = CARTESIAN_POINT ( 'NONE',  ( 190.8187029736043883, 300.1393067457597681, 3.941064102378585954 ) ) ;
#41623 = CARTESIAN_POINT ( 'NONE',  ( 154.8332767207531901, 280.7459370637686220, -0.9958211956073632631 ) ) ;
#41624 = CARTESIAN_POINT ( 'NONE',  ( 170.2435210885388983, 285.6843656190501406, -7.971347355553285219 ) ) ;
#41625 = CARTESIAN_POINT ( 'NONE',  ( 198.0006249058153003, 287.6998530631771587, 18.31850453277666801 ) ) ;
#41626 = DIRECTION ( 'NONE',  ( -0.000000000000000000, 0.000000000000000000, -1.000000000000000000 ) ) ;
#41627 = AXIS2_PLACEMENT_3D ( 'NONE', #60769, #82664, #29897 ) ;
#41628 = CARTESIAN_POINT ( 'NONE',  ( 117.3505249275209366, 251.8927522451419634, 2.944929066748280225E-16 ) ) ;
#41629 = CARTESIAN_POINT ( 'NONE',  ( 82.33779659592744338, 51.32762991731738822, -14.58766645682115026 ) ) ;
#41630 = ORIENTED_EDGE ( 'NONE', *, *, #80152, .F. ) ;
#41631 = CARTESIAN_POINT ( 'NONE',  ( 190.3144310910409445, 301.0127312671879167, -1.334877248546042949 ) ) ;
#41632 = CARTESIAN_POINT ( 'NONE',  ( -6.102853504003020291, 155.0327760586659167, 1.948934522072302763E-15 ) ) ;
#41633 = CARTESIAN_POINT ( 'NONE',  ( 31.67681054456310008, 201.3464784336661353, 1.353441290958777327E-15 ) ) ;
#41634 = CARTESIAN_POINT ( 'NONE',  ( 27.07746054717988571, 174.8932355074535678, -2.679491924311248496 ) ) ;
#41635 = CARTESIAN_POINT ( 'NONE',  ( 18.62433137644124059, 29.49103043416549141, -8.090169943749479842 ) ) ;
#41636 = DIRECTION ( 'NONE',  ( 0.5011331959107180323, 0.8653701635463924013, 0.000000000000000000 ) ) ;
#41637 = AXIS2_PLACEMENT_3D ( 'NONE', #49709, #11729, #96354 ) ;
#41638 = CARTESIAN_POINT ( 'NONE',  ( 65.99211009093512814, 69.22537564306347235, 0.2727399908702655695 ) ) ;
#41639 = CARTESIAN_POINT ( 'NONE',  ( 72.09683433654826956, 72.38845567423071259, -3.220643376046866901 ) ) ;
#41640 = CARTESIAN_POINT ( 'NONE',  ( 147.0538900202505488, 275.9421863647172017, 5.192507380313251986 ) ) ;
#41641 = CARTESIAN_POINT ( 'NONE',  ( 73.92553126217202930, 55.61088272459142701, -16.58549581058217015 ) ) ;
#41643 = CARTESIAN_POINT ( 'NONE',  ( 58.82164138842269097, 194.7677522451418213, -5.000000000000041744 ) ) ;
#41642 = CARTESIAN_POINT ( 'NONE',  ( 198.0913710030449408, 277.7585867100321479, -16.26773035892281882 ) ) ;
#41644 = CARTESIAN_POINT ( 'NONE',  ( 163.1128098473768375, 255.9724106907921168, -14.93599513872953821 ) ) ;
#41645 = CARTESIAN_POINT ( 'NONE',  ( -2.640161845538968599, 180.8297689869269504, -2.679491924311240503 ) ) ;
#41646 = LINE ( 'NONE', #26964, #69455 ) ;
#41647 = B_SPLINE_CURVE_WITH_KNOTS ( 'NONE', 3,
 ( #58469, #89442, #19997, #50877 ),
 .UNSPECIFIED., .F., .F.,
 ( 4, 4 ),
 ( 0.01207516581926863092, 0.01741691159609244990 ),
 .UNSPECIFIED. ) ;
#41648 = CARTESIAN_POINT ( 'NONE',  ( 161.9621149929554065, 267.2142435603461763, 16.48812087427357653 ) ) ;
#41649 = CARTESIAN_POINT ( 'NONE',  ( 39.93146227192245590, 203.8615022471903160, 5.000000000000046185 ) ) ;
#41650 = CARTESIAN_POINT ( 'NONE',  ( 41.20449994286561690, 183.0494855054052152, -2.679491924311248496 ) ) ;
#41651 = VECTOR ( 'NONE', #90420, 1000.000000000000000 ) ;
#41652 = CARTESIAN_POINT ( 'NONE',  ( 163.4004183463084416, 247.6291687766210146, 10.19167732382099345 ) ) ;
#41653 = CARTESIAN_POINT ( 'NONE',  ( 5.858601742122021783, 180.3149278399161233, 9.188101187500093303 ) ) ;
#41654 = CARTESIAN_POINT ( 'NONE',  ( 32.92443518896833154, 39.98502408145596121, -5.678558825948271327 ) ) ;
#41655 = CARTESIAN_POINT ( 'NONE',  ( 163.9254889395286341, 247.2708555043535625, 6.667454687248093315 ) ) ;
#41656 = CARTESIAN_POINT ( 'NONE',  ( 192.0523540417460993, 298.0025604169266558, 12.03387399082417275 ) ) ;
#41657 = CARTESIAN_POINT ( 'NONE',  ( 37.13125039574066477, 23.29860640527294535, -2.839279412974138328 ) ) ;
#41658 = CARTESIAN_POINT ( 'NONE',  ( 165.0565241268390366, 244.7607094220335568, 2.191926263411719589 ) ) ;
#41659 = CARTESIAN_POINT ( 'NONE',  ( 180.1282168372663079, 277.0805460213222204, 16.30842645680661818 ) ) ;
#41660 = CARTESIAN_POINT ( 'NONE',  ( 32.07315653955450330, 47.77038272570916888, -10.00000000000000000 ) ) ;
#41661 = CARTESIAN_POINT ( 'NONE',  ( -14.06329310883398875, 23.28858607597028296, 177.5919119679930134 ) ) ;
#41662 = CARTESIAN_POINT ( 'NONE',  ( 11.83670304002995266, 9.760047579820874120, 5.678558825948272215 ) ) ;
#41663 = DIRECTION ( 'NONE',  ( -0.000000000000000000, -0.000000000000000000, -1.000000000000000000 ) ) ;
#41664 = CARTESIAN_POINT ( 'NONE',  ( 20.04711164229383513, 17.28920272979926764, -7.433330006724141015 ) ) ;
#41665 = FACE_OUTER_BOUND ( 'NONE', #17405, .T. ) ;
#41666 = EDGE_CURVE ( 'NONE', #41308, #70064, #61734, .T. ) ;
#41667 = DIRECTION ( 'NONE',  ( -0.8660254037844387076, -0.4999999999999998890, -0.000000000000000000 ) ) ;
#41668 = CARTESIAN_POINT ( 'NONE',  ( 21.58410742392950610, 28.16454794089041869, -10.00000000000000355 ) ) ;
#41669 = CARTESIAN_POINT ( 'NONE',  ( 88.17689713045484723, 44.18699809719895910, -1.761924701106883040 ) ) ;
#41670 = EDGE_CURVE ( 'NONE', #97296, #85165, #69103, .T. ) ;
#41671 = ORIENTED_EDGE ( 'NONE', *, *, #77669, .F. ) ;
#41672 = CARTESIAN_POINT ( 'NONE',  ( 192.6797324865049745, 296.9159090750308110, 12.42053959885222625 ) ) ;
#41673 = CARTESIAN_POINT ( 'NONE',  ( 164.9779129355220562, 244.8968679994381148, -1.771286574179712803 ) ) ;
#41674 = CARTESIAN_POINT ( 'NONE',  ( 66.04680300344115551, 68.56179634104172749, 4.439170754574295330 ) ) ;
#41675 = DIRECTION ( 'NONE',  ( 0.000000000000000000, 0.000000000000000000, 1.000000000000000000 ) ) ;
#41676 = ORIENTED_EDGE ( 'NONE', *, *, #51526, .T. ) ;
#41677 = ORIENTED_EDGE ( 'NONE', *, *, #69608, .F. ) ;
#41678 = CARTESIAN_POINT ( 'NONE',  ( 134.3282312844263231, 248.3615022471902591, -10.00000000000009592 ) ) ;
#41679 = CARTESIAN_POINT ( 'NONE',  ( 86.10659305072458380, 47.03284479452093336, 10.73441527774546245 ) ) ;
#41680 = VERTEX_POINT ( 'NONE', #69701 ) ;
#41681 = AXIS2_PLACEMENT_3D ( 'NONE', #67694, #20115, #35796 ) ;
#41682 = CARTESIAN_POINT ( 'NONE',  ( 40.60966550219796289, 208.6868197944957330, -17.47570218321533631 ) ) ;
#41683 = CARTESIAN_POINT ( 'NONE',  ( 177.2673766539031988, 263.0841653866659158, 15.51101798395150944 ) ) ;
#41685 = ADVANCED_FACE ( 'NONE', ( #93031 ), #76333, .F. ) ;
#41684 = ORIENTED_EDGE ( 'NONE', *, *, #38263, .T. ) ;
#41686 = CARTESIAN_POINT ( 'NONE',  ( 78.24512733555256716, 61.71755924530574333, -15.76113161412312813 ) ) ;
#41687 = CARTESIAN_POINT ( 'NONE',  ( 88.54102397196729157, 43.89880672352619229, -0.3772737106920456829 ) ) ;
#41688 = CARTESIAN_POINT ( 'NONE',  ( 196.4808189786114951, 290.3322341467384717, -17.84817245450773271 ) ) ;
#41689 = CONICAL_SURFACE ( 'NONE', #49798, 3.299999999999978950, 1.029744258676652313 ) ;
#41690 = CARTESIAN_POINT ( 'NONE',  ( 80.74112568426333780, 43.09697088413143007, 9.813618375449099318 ) ) ;
#41691 = ORIENTED_EDGE ( 'NONE', *, *, #41819, .F. ) ;
#41692 = CARTESIAN_POINT ( 'NONE',  ( 200.6449165581618956, 283.1198055712825976, 18.35107460171532523 ) ) ;
#41693 = CARTESIAN_POINT ( 'NONE',  ( 166.1079261098780080, 274.0347854768993443, -15.23724750118056193 ) ) ;
#41694 = AXIS2_PLACEMENT_3D ( 'NONE', #86328, #70564, #32056 ) ;
#41695 = CARTESIAN_POINT ( 'NONE',  ( 74.28011090699931174, 62.22829491240943867, 14.85767347728069154 ) ) ;
#41696 = ORIENTED_EDGE ( 'NONE', *, *, #99048, .F. ) ;
#41697 = CARTESIAN_POINT ( 'NONE',  ( 170.6619951277876623, 255.5210136367033726, -11.54849001391199970 ) ) ;
#41698 = CARTESIAN_POINT ( 'NONE',  ( 202.8787628851569593, 279.2506702366259788, 17.01435431865322556 ) ) ;
#41699 = EDGE_CURVE ( 'NONE', #89234, #70505, #26773, .T. ) ;
#41700 = ORIENTED_EDGE ( 'NONE', *, *, #39874, .T. ) ;
#41701 = EDGE_CURVE ( 'NONE', #21534, #30468, #90877, .T. ) ;
#41702 = ORIENTED_EDGE ( 'NONE', *, *, #80172, .F. ) ;
#41703 = CARTESIAN_POINT ( 'NONE',  ( 157.0136551185426868, 266.0997186349934509, -17.02801493162102986 ) ) ;
#41705 = ORIENTED_EDGE ( 'NONE', *, *, #50876, .T. ) ;
#41704 = B_SPLINE_CURVE_WITH_KNOTS ( 'NONE', 3,
 ( #11196, #42066, #65368, #5074 ),
 .UNSPECIFIED., .F., .F.,
 ( 4, 4 ),
 ( 0.008546822710145150076, 0.01492985447388818325 ),
 .UNSPECIFIED. ) ;
#41706 = DIRECTION ( 'NONE',  ( -1.000000000000000000, 0.000000000000000000, 0.000000000000000000 ) ) ;
#41707 = ORIENTED_EDGE ( 'NONE', *, *, #45585, .T. ) ;
#41708 = CARTESIAN_POINT ( 'NONE',  ( 147.8435824263222855, 274.5743989950495347, 6.098816573078369885 ) ) ;
#41709 = CARTESIAN_POINT ( 'NONE',  ( 180.5039422260482240, 291.5977753851293528, -9.856995586095885997 ) ) ;
#41710 = CARTESIAN_POINT ( 'NONE',  ( 188.2520712372829621, 265.6420100395978920, -13.17850047611677766 ) ) ;
#41711 = CARTESIAN_POINT ( 'NONE',  ( -30.18034446749236821, 25.12100238203590763, 10.00000000000000000 ) ) ;
#41712 = CARTESIAN_POINT ( 'NONE',  ( 158.3623000859935246, 256.3554455780269450, -16.52320444293775381 ) ) ;
#41713 = ORIENTED_EDGE ( 'NONE', *, *, #87410, .F. ) ;
#41714 = CARTESIAN_POINT ( 'NONE',  ( 100.9602528039918923, 217.5494855054051868, -2.679491924311248496 ) ) ;
#41715 = CARTESIAN_POINT ( 'NONE',  ( 23.18645373101242413, 19.10170272979927120, -7.433330006724141015 ) ) ;
#41717 = CARTESIAN_POINT ( 'NONE',  ( 190.4646797940841623, 298.9332177302380842, -8.185516204028834508 ) ) ;
#41716 = CARTESIAN_POINT ( 'NONE',  ( 196.7823306783968746, 289.8100005636337073, -17.85370042640856170 ) ) ;
#41719 = EDGE_LOOP ( 'NONE', ( #96568, #50171, #56000, #51930 ) ) ;
#41718 = CARTESIAN_POINT ( 'NONE',  ( -10.54235908185773773, 24.92402704602492491, -10.00000000000000000 ) ) ;
#41720 = AXIS2_PLACEMENT_3D ( 'NONE', #13563, #37824, #84481 ) ;
#41721 = ORIENTED_EDGE ( 'NONE', *, *, #11273, .F. ) ;
#41722 = CARTESIAN_POINT ( 'NONE',  ( 187.6504252453685240, 277.1264514418339786, 17.28725775733853709 ) ) ;
#41723 = EDGE_CURVE ( 'NONE', #66637, #85448, #44868, .T. ) ;
#41724 = CARTESIAN_POINT ( 'NONE',  ( 171.5016553172604574, 259.7020436333838802, -14.14659924787457435 ) ) ;
#41725 = CYLINDRICAL_SURFACE ( 'NONE', #44718, 17.82106496071139645 ) ;
#41726 = CARTESIAN_POINT ( 'NONE',  ( 79.10094814821772502, 46.07821729000689714, 13.26225723241342003 ) ) ;
#41727 = CARTESIAN_POINT ( 'NONE',  ( 161.8948331661419218, 250.2369188037922356, 13.64419044796309777 ) ) ;
#41728 = CARTESIAN_POINT ( 'NONE',  ( 148.4341346725819051, 273.5515325000037024, -10.40428456760419884 ) ) ;
#41729 = ORIENTED_EDGE ( 'NONE', *, *, #10882, .T. ) ;
#41731 = ADVANCED_FACE ( 'NONE', ( #92547 ), #72743, .F. ) ;
#41730 = LINE ( 'NONE', #26554, #39717 ) ;
#41732 = DIRECTION ( 'NONE',  ( -0.8660254037844387076, -0.4999999999999998890, -0.000000000000000000 ) ) ;
#41733 = CARTESIAN_POINT ( 'NONE',  ( 42.77981749017101976, 207.0530062829863311, -4.648177544792955347E-16 ) ) ;
#41734 = CARTESIAN_POINT ( 'NONE',  ( 164.5416088356626290, 245.6525688679454618, -1.463507744092769292 ) ) ;
#41735 = CARTESIAN_POINT ( 'NONE',  ( 27.64472685218290238, 176.7677522451417929, -5.000000000000041744 ) ) ;
#41736 = CARTESIAN_POINT ( 'NONE',  ( 98.90203251333015544, 240.1589784336661637, -6.496448406907676862E-16 ) ) ;
#41737 = CARTESIAN_POINT ( 'NONE',  ( 180.7892034029179626, 294.0795370620815561, -2.813581583843308032 ) ) ;
#41738 = EDGE_CURVE ( 'NONE', #45167, #54308, #63006, .T. ) ;
#41739 = LINE ( 'NONE', #94993, #87489 ) ;
#41740 = FACE_OUTER_BOUND ( 'NONE', #65857, .T. ) ;
#41741 = CARTESIAN_POINT ( 'NONE',  ( 13.16551753867071461, 190.6589784336661921, -6.496448406907675876E-16 ) ) ;
#41742 = EDGE_CURVE ( 'NONE', #21753, #7803, #2324, .T. ) ;
#41743 = DIRECTION ( 'NONE',  ( -1.000000000000000000, 0.000000000000000000, 0.000000000000000000 ) ) ;
#41744 = ORIENTED_EDGE ( 'NONE', *, *, #80771, .T. ) ;
#41745 = ORIENTED_EDGE ( 'NONE', *, *, #13280, .F. ) ;
#41746 = EDGE_CURVE ( 'NONE', #12322, #1361, #64614, .T. ) ;
#41747 = CARTESIAN_POINT ( 'NONE',  ( 186.7200758071169275, 260.8107248425581020, -5.831653652513626440 ) ) ;
#41748 = CARTESIAN_POINT ( 'NONE',  ( 181.8404918915032340, 261.1361780761246223, 12.51250699268308786 ) ) ;
#41749 = CARTESIAN_POINT ( 'NONE',  ( 83.29197815752417000, 42.60964419094407418, 5.769052513407811666 ) ) ;
#41750 = CARTESIAN_POINT ( 'NONE',  ( 193.0206257540501156, 263.7076866269070479, -4.037792959707156015 ) ) ;
#41751 = CARTESIAN_POINT ( 'NONE',  ( 161.1150691641480535, 251.5875096731584506, -13.48836942566120101 ) ) ;
#41752 = CARTESIAN_POINT ( 'NONE',  ( 182.0419006976227934, 284.8263522540155464, 14.99106680293229843 ) ) ;
#41753 = CARTESIAN_POINT ( 'NONE',  ( 74.20550489482296541, 67.87148625235720090, -11.67750707853813807 ) ) ;
#41754 = CARTESIAN_POINT ( 'NONE',  ( 45.69611741197122257, 191.0643266524160140, 9.188101187500095079 ) ) ;
#41755 = CARTESIAN_POINT ( 'NONE',  ( 87.90566119885008334, 214.8927522451418213, 10.00000000000009592 ) ) ;
#41756 = VECTOR ( 'NONE', #15563, 1000.000000000000000 ) ;
#41757 = ORIENTED_EDGE ( 'NONE', *, *, #5261, .T. ) ;
#41758 = CARTESIAN_POINT ( 'NONE',  ( 84.11025865604790397, 47.61814693595540149, 11.74156198426350706 ) ) ;
#41759 = CARTESIAN_POINT ( 'NONE',  ( 158.3433012654136292, 282.4888899867655141, -1.676262827589547921 ) ) ;
#41760 = AXIS2_PLACEMENT_3D ( 'NONE', #63925, #94864, #25423 ) ;
#41761 = CARTESIAN_POINT ( 'NONE',  ( 8.267668766103758671, 166.3923013555410080, 4.594050593750050204 ) ) ;
#41762 = CIRCLE ( 'NONE', #30484, 14.99999999999967493 ) ;
#41763 = CARTESIAN_POINT ( 'NONE',  ( 68.91072503222051182, 64.29678190498039214, -11.91033057008465157 ) ) ;
#41764 = CARTESIAN_POINT ( 'NONE',  ( 198.5970767652345899, 286.6667681383942181, -17.17073100918929640 ) ) ;
#41765 = CARTESIAN_POINT ( 'NONE',  ( 79.13689845121717781, 45.88162669096313806, -12.51413720753079772 ) ) ;
#41766 = CARTESIAN_POINT ( 'NONE',  ( 147.5540328368684300, 275.0759135952944234, -4.750028533202499403 ) ) ;
#41767 = CYLINDRICAL_SURFACE ( 'NONE', #83145, 11.89249999999999652 ) ;
#41768 = CARTESIAN_POINT ( 'NONE',  ( 163.7729086741176161, 246.9839966035275438, 6.099406794390714204 ) ) ;
#41769 = CARTESIAN_POINT ( 'NONE',  ( 191.2211340522693774, 299.4422756709672626, -8.405362570633277741 ) ) ;
#41770 = CARTESIAN_POINT ( 'NONE',  ( 206.9878665138179770, 272.1334939782196329, 6.566295309274049252 ) ) ;
#41771 = VERTEX_POINT ( 'NONE', #96054 ) ;
#41772 = VECTOR ( 'NONE', #63212, 1000.000000000000114 ) ;
#41773 = CARTESIAN_POINT ( 'NONE',  ( -3.441976700948170542, 175.4865022471903160, -10.00000000000009415 ) ) ;
#41774 = FACE_BOUND ( 'NONE', #89727, .T. ) ;
#41775 = CARTESIAN_POINT ( 'NONE',  ( 125.6141109788952122, 234.1423013555409796, -4.594050593750043987 ) ) ;
#41776 = CARTESIAN_POINT ( 'NONE',  ( 26.73894555032740783, 17.29860640527292759, -2.839279412974138328 ) ) ;
#41777 = CARTESIAN_POINT ( 'NONE',  ( 74.99774251554812565, 67.18734242688375957, 12.55770300872047507 ) ) ;
#41778 = CARTESIAN_POINT ( 'NONE',  ( 150.9724347302981187, 269.6954501832723849, 13.74844370660301784 ) ) ;
#41779 = VECTOR ( 'NONE', #35998, 1000.000000000000000 ) ;
#41781 = DIRECTION ( 'NONE',  ( -0.8080546441192405505, 0.5891075386695773242, 0.000000000000000000 ) ) ;
#41780 = CARTESIAN_POINT ( 'NONE',  ( 196.0034224882197975, 291.1591091234520263, 17.53794140922627776 ) ) ;
#41782 = CARTESIAN_POINT ( 'NONE',  ( 12.54686387532899516, 29.01751292744055277, 6.180339887498949913 ) ) ;
#41783 = ORIENTED_EDGE ( 'NONE', *, *, #44414, .T. ) ;
#41784 = CARTESIAN_POINT ( 'NONE',  ( 189.8675696937700650, 261.6596842279012662, -4.438983720181640891 ) ) ;
#41785 = CARTESIAN_POINT ( 'NONE',  ( 196.2379679265050925, 290.7528645076583871, -16.93678934971137906 ) ) ;
#41786 = CARTESIAN_POINT ( 'NONE',  ( 190.4937053644069920, 299.9959326328678912, 4.274138836246343942 ) ) ;
#41787 = CARTESIAN_POINT ( 'NONE',  ( 176.1878198624884249, 292.0021934572283158, -1.093827943886815923 ) ) ;
#41788 = CARTESIAN_POINT ( 'NONE',  ( 81.56133095906432118, 55.49845989692713744, -16.32137983002412085 ) ) ;
#41789 = ORIENTED_EDGE ( 'NONE', *, *, #53472, .F. ) ;
#41790 = CARTESIAN_POINT ( 'NONE',  ( 76.77731254116882553, 64.09355814141257213, -15.16545583891343263 ) ) ;
#41791 = CARTESIAN_POINT ( 'NONE',  ( -22.42236680055709641, 157.8615022471902591, 0.000000000000000000 ) ) ;
#41792 = CARTESIAN_POINT ( 'NONE',  ( 168.8502749405928398, 271.8395537308506960, -16.79921431673894361 ) ) ;
#41793 = CARTESIAN_POINT ( 'NONE',  ( 79.50884248659365028, 51.35306852090381824, 15.14975241329744193 ) ) ;
#41794 = CARTESIAN_POINT ( 'NONE',  ( 83.77581334972808236, 52.13813006813991535, -14.62973826141883826 ) ) ;
#41795 = CARTESIAN_POINT ( 'NONE',  ( 71.40824431555127205, 71.90448883543326986, -1.148190763236565326 ) ) ;
#41796 = CARTESIAN_POINT ( 'NONE',  ( 176.9361943346061992, 287.9860272245114174, 12.19037568368620938 ) ) ;
#41797 = VECTOR ( 'NONE', #85810, 1000.000000000000000 ) ;
#41798 = EDGE_LOOP ( 'NONE', ( #8168, #3155, #194, #42131, #45928, #61545 ) ) ;
#41799 = CARTESIAN_POINT ( 'NONE',  ( 167.5505310038667517, 261.6318463984700315, 17.07012949051403439 ) ) ;
#41800 = CARTESIAN_POINT ( 'NONE',  ( 3.893371226040319044, 25.18080186712590773, 3.090169943749475401 ) ) ;
#41801 = CARTESIAN_POINT ( 'NONE',  ( 192.3683084660635529, 288.2966816650776423, -15.88566354911130674 ) ) ;
#41802 = VERTEX_POINT ( 'NONE', #88471 ) ;
#41803 = CARTESIAN_POINT ( 'NONE',  ( 164.8075539017095252, 280.4672370525465226, 12.63796469268613265 ) ) ;
#41804 = CARTESIAN_POINT ( 'NONE',  ( 194.9455394410084921, 292.9914163096879065, -15.01116663483170655 ) ) ;
#41805 = CARTESIAN_POINT ( 'NONE',  ( 165.0319151415814645, 246.0072716476385608, -1.061671501984392751 ) ) ;
#41807 = EDGE_CURVE ( 'NONE', #6621, #14175, #17067, .T. ) ;
#41806 = ORIENTED_EDGE ( 'NONE', *, *, #45815, .F. ) ;
#41808 = CARTESIAN_POINT ( 'NONE',  ( 79.09523395582193928, 59.82262253747457237, 16.49691284064748587 ) ) ;
#41809 = LINE ( 'NONE', #3350, #55614 ) ;
#41810 = AXIS2_PLACEMENT_3D ( 'NONE', #4635, #25956, #3170 ) ;
#41811 = CARTESIAN_POINT ( 'NONE',  ( 83.55471316296232942, 50.16249053343400277, -13.72935981377203163 ) ) ;
#41812 = CARTESIAN_POINT ( 'NONE',  ( 73.43716180859617282, 69.78348016549323063, -9.856747356917667346 ) ) ;
#41813 = FACE_OUTER_BOUND ( 'NONE', #80499, .T. ) ;
#41814 = CARTESIAN_POINT ( 'NONE',  ( 203.3740894404336927, 278.3927394765486838, -15.19753795879846869 ) ) ;
#41815 = ORIENTED_EDGE ( 'NONE', *, *, #29384, .F. ) ;
#41816 = EDGE_CURVE ( 'NONE', #24657, #39565, #41287, .T. ) ;
#41817 = ORIENTED_EDGE ( 'NONE', *, *, #61006, .F. ) ;
#41818 = CARTESIAN_POINT ( 'NONE',  ( 106.0403798229140477, 220.4824982072973683, 3.021315404115420679E-15 ) ) ;
#41819 = EDGE_CURVE ( 'NONE', #62607, #72102, #79922, .T. ) ;
#41820 = ORIENTED_EDGE ( 'NONE', *, *, #40464, .T. ) ;
#41821 = DIRECTION ( 'NONE',  ( -0.3715724127386920705, 0.6435822975543701308, -0.6691306063588670083 ) ) ;
#41822 = VERTEX_POINT ( 'NONE', #86468 ) ;
#41823 = DIRECTION ( 'NONE',  ( -0.000000000000000000, -0.000000000000000000, 1.000000000000000000 ) ) ;
#41824 = CARTESIAN_POINT ( 'NONE',  ( 154.9903553346911735, 262.1958252075976361, -18.39016733948542637 ) ) ;
#41825 = ORIENTED_EDGE ( 'NONE', *, *, #93643, .T. ) ;
#41826 = CARTESIAN_POINT ( 'NONE',  ( 183.3723276922390539, 280.6706895461819045, -16.13205748088399005 ) ) ;
#41827 = CARTESIAN_POINT ( 'NONE',  ( 82.06339014627782547, 41.09835319584696123, 3.298898961656697715 ) ) ;
#41828 = CARTESIAN_POINT ( 'NONE',  ( 160.9268025830670865, 254.5507503617475038, -15.18711876478708511 ) ) ;
#41829 = CARTESIAN_POINT ( 'NONE',  ( 161.9036870859828809, 277.5393705136012272, -13.14925469141188508 ) ) ;
#41830 = CARTESIAN_POINT ( 'NONE',  ( 192.5076277540105423, 297.2140032159341558, -13.10094381206144298 ) ) ;
#41831 = VECTOR ( 'NONE', #60547, 1000.000000000000114 ) ;
#41832 = CARTESIAN_POINT ( 'NONE',  ( 200.8665851640556070, 282.7358642834317948, -16.69422397739980823 ) ) ;
#41833 = CARTESIAN_POINT ( 'NONE',  ( -13.11024591527734628, 27.99999999999999645, 32.50000000000000000 ) ) ;
#41835 = CARTESIAN_POINT ( 'NONE',  ( 155.1556490571049949, 279.7438825265072069, 2.118603912366986197 ) ) ;
#41834 = VECTOR ( 'NONE', #83191, 1000.000000000000000 ) ;
#41836 = CARTESIAN_POINT ( 'NONE',  ( 130.0789470495699618, 258.1589784336661637, -6.496448406907675876E-16 ) ) ;
#41837 = EDGE_LOOP ( 'NONE', ( #50215, #82364, #48683, #36729 ) ) ;
#41838 = CARTESIAN_POINT ( 'NONE',  ( 70.97253302420340049, 61.11785764705713575, -14.48731777010960009 ) ) ;
#41839 = CIRCLE ( 'NONE', #95266, 3.299999999999998934 ) ;
#41840 = ORIENTED_EDGE ( 'NONE', *, *, #34302, .F. ) ;
#41841 = AXIS2_PLACEMENT_3D ( 'NONE', #46797, #53873, #9299 ) ;
#41843 = EDGE_LOOP ( 'NONE', ( #97452, #7961, #59113, #50723, #5365 ) ) ;
#41842 = CARTESIAN_POINT ( 'NONE',  ( 85.65277752055500571, 48.41186657597218357, -12.21575983946769739 ) ) ;
#41844 = CARTESIAN_POINT ( 'NONE',  ( 202.3894997978090373, 280.0980987621804275, 16.95659012541789323 ) ) ;
#41845 = CARTESIAN_POINT ( 'NONE',  ( 23.64814127513158937, 118.0650415295850451, 60.00000000000000000 ) ) ;
#41846 = CARTESIAN_POINT ( 'NONE',  ( 190.0601721553029222, 300.2863949309033842, 3.228815124723532382 ) ) ;
#41847 = CARTESIAN_POINT ( 'NONE',  ( 47.96820964746023463, 80.67316705762479501, -10.00000000000000000 ) ) ;
#41848 = CARTESIAN_POINT ( 'NONE',  ( 152.9273493951901628, 265.7690563111299298, -17.70273273795505631 ) ) ;
#41849 = CARTESIAN_POINT ( 'NONE',  ( -19.56352399852919888, 92.95511110727130699, 59.99999999999999289 ) ) ;
#41850 = CARTESIAN_POINT ( 'NONE',  ( 192.8911265895718827, 292.5243652962839747, -14.36741178004102970 ) ) ;
#41851 = PLANE ( 'NONE',  #6254 ) ;
#41852 = CARTESIAN_POINT ( 'NONE',  ( -39.52511050156713424, 25.94496742513404541, -10.00000000000000000 ) ) ;
#41853 = VECTOR ( 'NONE', #66216, 1000.000000000000227 ) ;
#41854 = ORIENTED_EDGE ( 'NONE', *, *, #9669, .T. ) ;
#41856 = EDGE_CURVE ( 'NONE', #31200, #64025, #14736, .T. ) ;
#41855 = CARTESIAN_POINT ( 'NONE',  ( 194.1852025340051284, 294.3083584634874796, -15.46421316575964688 ) ) ;
#41857 = CARTESIAN_POINT ( 'NONE',  ( 75.91930487633969449, 61.92743185228299296, -15.32863521163103648 ) ) ;
#41858 = ORIENTED_EDGE ( 'NONE', *, *, #21602, .T. ) ;
#41859 = CARTESIAN_POINT ( 'NONE',  ( -19.71595605685117647, 92.93789402164532021, 59.99999999999999289 ) ) ;
#41860 = ADVANCED_FACE ( 'NONE', ( #16995 ), #97051, .T. ) ;
#41861 = B_SPLINE_CURVE_WITH_KNOTS ( 'NONE', 3,
 ( #44590, #61296, #59799, #60778, #30903, #6110, #67408, #53207, #69405, #38490, #52693, #37491, #76995, #37982, #7602, #29416, #83147, #51730, #21808, #18, #67915, #83655, #84160, #92259, #14706, #90265, #20838, #14213, #68399, #82673, #68893, #13238, #60285, #13715, #44092, #45105, #75036, #98835, #15184, #99820, #36505, #28927, #37005, #98333, #75525, #90770 ),
 .UNSPECIFIED., .F., .F.,
 ( 4, 1, 1, 1, 2, 2, 1, 1, 1, 2, 2, 1, 1, 2, 2, 1, 1, 2, 2, 1, 1, 2, 2, 1, 2, 2, 1, 2, 2, 4 ),
 ( 0.000000000000000000, 0.06249999999997910005, 0.09374999999997009337, 0.1093749999999655831, 0.1171874999999646949, 0.1249999999999638067, 0.1874999999999651112, 0.2187499999999650835, 0.2343749999999650835, 0.2421874999999658884, 0.2499999999999666933, 0.3124999999999751865, 0.3437499999999794609, 0.3593749999999806266, 0.3749999999999817368, 0.4374999999999826250, 0.4687499999999830136, 0.4843749999999821809, 0.4999999999999813483, 0.5624999999999810152, 0.5937499999999817923, 0.6093749999999825695, 0.6249999999999832356, 0.6874999999999895639, 0.7187499999999926725, 0.7499999999999957812, 0.8124999999999994449, 0.8437500000000004441, 0.8750000000000013323, 1.000000000000000000 ),
 .UNSPECIFIED. ) ;
#41862 = EDGE_CURVE ( 'NONE', #65003, #74614, #12240, .T. ) ;
#41863 = CARTESIAN_POINT ( 'NONE',  ( 201.2353357416039614, 267.9535537611733957, -2.850234977744889431 ) ) ;
#41864 = CARTESIAN_POINT ( 'NONE',  ( 192.0275136246134196, 298.0455852814817490, -9.520297513543107826 ) ) ;
#41865 = CARTESIAN_POINT ( 'NONE',  ( 80.51726034258919640, 44.91748552740171618, -11.09860402559229442 ) ) ;
#41866 = CARTESIAN_POINT ( 'NONE',  ( 202.2576150004249200, 280.3265299319959354, 16.24828394350762295 ) ) ;
#41868 = CARTESIAN_POINT ( 'NONE',  ( 87.98804127167099409, 43.77408088403165465, 2.388364124389103171 ) ) ;
#41867 = DIRECTION ( 'NONE',  ( 0.5000000000000013323, -0.8660254037844378194, 0.000000000000000000 ) ) ;
#41869 = AXIS2_PLACEMENT_3D ( 'NONE', #53698, #7614, #38502 ) ;
#41870 = DIRECTION ( 'NONE',  ( 1.000000000000000000, 0.000000000000000000, 0.000000000000000000 ) ) ;
#41871 = VERTEX_POINT ( 'NONE', #44285 ) ;
#41872 = PRODUCT_DEFINITION_SHAPE ( 'NONE', 'NONE',  #21746 ) ;
#41873 = CARTESIAN_POINT ( 'NONE',  ( 11.62325688217078223, 167.5177522451418213, 5.000000000000051514 ) ) ;
#41874 = EDGE_CURVE ( 'NONE', #96323, #54644, #83327, .T. ) ;
#41875 = CARTESIAN_POINT ( 'NONE',  ( 80.33434995892775987, 58.04101998076092883, 16.26088286722919207 ) ) ;
#41876 = EDGE_CURVE ( 'NONE', #23100, #49399, #36681, .T. ) ;
#41877 = CARTESIAN_POINT ( 'NONE',  ( -55.56624327025929944, 44.99999999999998579, -10.00000000000000000 ) ) ;
#41878 = CARTESIAN_POINT ( 'NONE',  ( 192.2185419806677942, 297.7147144631093170, 12.45868041609393728 ) ) ;
#41879 = CARTESIAN_POINT ( 'NONE',  ( 81.18390761377841613, 43.43123804279526468, -9.905827838957788956 ) ) ;
#41880 = CARTESIAN_POINT ( 'NONE',  ( -19.65312891409030271, 93.06504152958497400, -10.00000000000000888 ) ) ;
#41881 = CARTESIAN_POINT ( 'NONE',  ( 202.5245888501533216, 279.8641176599742266, 15.60152447840272494 ) ) ;
#41882 = CARTESIAN_POINT ( 'NONE',  ( 3.856091543753019213, 173.0333772461660828, 9.188101187500095079 ) ) ;
#41883 = CARTESIAN_POINT ( 'NONE',  ( 97.84665082640911749, 236.4869531367911293, 4.594050593750046652 ) ) ;
#41884 = CARTESIAN_POINT ( 'NONE',  ( 192.4663556654298588, 297.2854885702906245, -12.98646995774174684 ) ) ;
#41885 = CARTESIAN_POINT ( 'NONE',  ( 181.9272638006293619, 257.0174299096278219, -2.314174031938120102 ) ) ;
#41886 = CARTESIAN_POINT ( 'NONE',  ( 66.18968672761215544, 68.49487770601442094, -4.881532527435788360 ) ) ;
#41887 = CARTESIAN_POINT ( 'NONE',  ( 75.46732613426667058, 55.10851769043934922, -16.13625620877613542 ) ) ;
#41888 = CARTESIAN_POINT ( 'NONE',  ( 163.5826848823411410, 283.4162327659261678, 5.679725392094765013 ) ) ;
#41889 = CYLINDRICAL_SURFACE ( 'NONE', #24116, 16.60714546451156792 ) ;
#41890 = CARTESIAN_POINT ( 'NONE',  ( 207.9528294584847288, 270.4621291306354465, 5.874671256616545101 ) ) ;
#41891 = DIRECTION ( 'NONE',  ( 0.7235470741700498198, 0.1663964660674505380, -0.6699192843471699632 ) ) ;
#41892 = CARTESIAN_POINT ( 'NONE',  ( 184.5847840940699598, 267.9585090317841036, 15.85480517954647084 ) ) ;
#41893 = CARTESIAN_POINT ( 'NONE',  ( 78.28713622914533232, 54.32488346555809500, -16.43848886914129892 ) ) ;
#41894 = CARTESIAN_POINT ( 'NONE',  ( 76.80517106979452535, 63.30872754350402687, -15.45635652541256455 ) ) ;
#41895 = AXIS2_PLACEMENT_3D ( 'NONE', #73653, #35636, #89402 ) ;
#41896 = EDGE_CURVE ( 'NONE', #3452, #77804, #13775, .T. ) ;
#41897 = CARTESIAN_POINT ( 'NONE',  ( 75.30318735596920021, 214.2833772461660544, -9.188101187500095079 ) ) ;
#41898 = CARTESIAN_POINT ( 'NONE',  ( 207.5785076975260779, 271.1104734389944042, -6.824813054587777650 ) ) ;
#41899 = CARTESIAN_POINT ( 'NONE',  ( 87.88902802526534686, 43.91876200309240375, 0.4180276961672018121 ) ) ;
#41900 = VECTOR ( 'NONE', #33560, 1000.000000000000000 ) ;
#41901 = CARTESIAN_POINT ( 'NONE',  ( -16.76269525828470464, 104.1287493039388181, 12.66656182927058261 ) ) ;
#41903 = PLANE ( 'NONE',  #71698 ) ;
#41902 = CARTESIAN_POINT ( 'NONE',  ( 87.06600699492729234, 43.48165395943767209, -3.537923743661954390 ) ) ;
#41904 = B_SPLINE_CURVE_WITH_KNOTS ( 'NONE', 3,
 ( #82165, #81657, #43605, #60281, #12740, #98329, #66416, #27433, #74542, #5121, #35008, #36001, #44089, #28923, #58790, #83143, #65908, #6106, #96865, #43089, #66905, #74032, #58307, #89284, #4620, #97343, #67405, #51201, #52195, #19832, #35513, #89761, #91239, #59284, #21804, #20330, #90766, #97834, #75522, #90263, #36502, #59795, #75032, #21317, #13712, #67912 ),
 .UNSPECIFIED., .F., .F.,
 ( 4, 1, 2, 2, 1, 2, 2, 1, 1, 2, 2, 1, 1, 2, 2, 1, 1, 2, 2, 1, 1, 1, 2, 2, 1, 1, 1, 2, 2, 4 ),
 ( 0.000000000000000000, 0.06250000000000548173, 0.09375000000000714706, 0.1250000000000088263, 0.1875000000000137945, 0.2187500000000155154, 0.2500000000000172085, 0.3125000000000211497, 0.3437500000000230926, 0.3593750000000227596, 0.3750000000000223710, 0.4375000000000270339, 0.4687500000000286993, 0.4843750000000284772, 0.5000000000000283107, 0.5625000000000256462, 0.5937500000000244249, 0.6093750000000237588, 0.6250000000000232037, 0.6875000000000237588, 0.7187500000000250910, 0.7343750000000247580, 0.7421875000000246470, 0.7500000000000245359, 0.8125000000000205391, 0.8437500000000190958, 0.8593750000000174305, 0.8671875000000165423, 0.8750000000000156541, 1.000000000000000000 ),
 .UNSPECIFIED. ) ;
#41905 = B_SPLINE_CURVE_WITH_KNOTS ( 'NONE', 3,
 ( #48989, #64180, #11002, #33805, #9994, #71801, #65178, #87560, #2398, #96126, #73785, #88541, #33277, #10485, #72304, #95128, #80939, #11507, #42850, #34768, #65668, #96624, #25694, #4375, #27189, #56573, #58078, #35274, #66181, #27692, #2912, #89534, #64688, #95639, #70021, #44358, #31516, #13488, #84774, #28172, #15310, #53810, #23417, #90526, #59548, #93368 ),
 .UNSPECIFIED., .F., .F.,
 ( 4, 1, 2, 2, 1, 2, 2, 1, 1, 2, 2, 1, 1, 2, 2, 1, 1, 2, 2, 1, 1, 1, 2, 2, 1, 1, 1, 2, 2, 4 ),
 ( 0.000000000000000000, 0.06249999999999684974, 0.09374999999999356071, 0.1249999999999902578, 0.1874999999999888423, 0.2187499999999863165, 0.2499999999999837907, 0.3124999999999741318, 0.3437499999999710787, 0.3593749999999679146, 0.3749999999999648059, 0.4374999999999586997, 0.4687499999999537592, 0.4843749999999516498, 0.4999999999999495404, 0.5624999999999404920, 0.5937499999999356071, 0.6093749999999330536, 0.6249999999999305000, 0.6874999999999212852, 0.7187499999999167333, 0.7343749999999157341, 0.7421874999999152900, 0.7499999999999149569, 0.8124999999999369393, 0.8437499999999495959, 0.8593749999999559241, 0.8671874999999589217, 0.8749999999999620304, 1.000000000000000000 ),
 .UNSPECIFIED. ) ;
#41906 = B_SPLINE_CURVE_WITH_KNOTS ( 'NONE', 3,
 ( #48408, #24598, #61595, #31194, #71223, #23093, #53983, #78825, #93542, #46386, #62085, #93029, #85456, #63600, #70700, #1314, #1816, #32700, #41793, #88470, #27117, #97050, #72742, #18519, #42778, #48915, #81840, #2323, #19535, #50892, #88981, #10415, #3814, #72227, #34695, #73221, #79850, #33723, #87486, #50397, #11921, #41285, #65596, #65105, #73711, #96546 ),
 .UNSPECIFIED., .F., .F.,
 ( 4, 1, 1, 1, 2, 2, 1, 1, 1, 2, 2, 1, 1, 2, 2, 1, 1, 2, 2, 1, 1, 2, 2, 1, 2, 2, 1, 2, 2, 4 ),
 ( 0.000000000000000000, 0.06250000000001047773, 0.09375000000001570966, 0.1093750000000168893, 0.1171875000000168615, 0.1250000000000168199, 0.1875000000000120459, 0.2187500000000090761, 0.2343750000000066891, 0.2421875000000068279, 0.2500000000000069389, 0.3125000000000091593, 0.3437500000000087708, 0.3593750000000084932, 0.3750000000000082157, 0.4375000000000059397, 0.4687500000000043299, 0.4843750000000029976, 0.5000000000000016653, 0.5624999999999990008, 0.5937499999999972244, 0.6093749999999966693, 0.6249999999999962252, 0.6874999999999936717, 0.7187499999999926725, 0.7499999999999916733, 0.8124999999999918954, 0.8437499999999930056, 0.8749999999999941158, 1.000000000000000000 ),
 .UNSPECIFIED. ) ;
#41907 = AXIS2_PLACEMENT_3D ( 'NONE', #92762, #18111, #63706 ) ;
#41908 = CARTESIAN_POINT ( 'NONE',  ( 173.3300473466945277, 268.3110915217967545, -16.29280547201360818 ) ) ;
#41909 = CARTESIAN_POINT ( 'NONE',  ( 28.07469292777547309, 37.18502408145592852, 5.678558825948276656 ) ) ;
#41910 = DIRECTION ( 'NONE',  ( -1.538313725856140942E-15, 3.076627451712281884E-15, -1.000000000000000000 ) ) ;
#41911 = DIRECTION ( 'NONE',  ( -0.8660254037844387076, -0.4999999999999998890, -0.000000000000000000 ) ) ;
#41912 = ORIENTED_EDGE ( 'NONE', *, *, #74800, .F. ) ;
#41913 = CARTESIAN_POINT ( 'NONE',  ( 12.48623565965559479, 28.18502408145590721, 5.678558825948277544 ) ) ;
#41914 = CARTESIAN_POINT ( 'NONE',  ( 68.21243081460160340, 216.3149278399160664, 9.188101187500093303 ) ) ;
#41915 = CARTESIAN_POINT ( 'NONE',  ( 198.7134558283731280, 282.8386145195935910, 17.66748989068429054 ) ) ;
#41916 = CARTESIAN_POINT ( 'NONE',  ( 169.9373325680253117, 288.2255053123109860, -1.082792927354846446 ) ) ;
#41917 = CARTESIAN_POINT ( 'NONE',  ( 192.7705129102570822, 296.7586727687594816, -13.39629674907774692 ) ) ;
#41918 = CARTESIAN_POINT ( 'NONE',  ( 199.3579472636792786, 281.3827632249817725, 17.38534755126016407 ) ) ;
#41919 = CARTESIAN_POINT ( 'NONE',  ( -14.83894680564148238, 24.48641780169620219, -10.00000000000000000 ) ) ;
#41920 = CARTESIAN_POINT ( 'NONE',  ( 189.7468387718738541, 286.5256409918453073, 16.65683580306518863 ) ) ;
#41921 = CARTESIAN_POINT ( 'NONE',  ( 72.40694465691628068, 71.58314657692716310, 5.120125831695425234 ) ) ;
#41922 = VECTOR ( 'NONE', #52550, 1000.000000000000227 ) ;
#41923 = CARTESIAN_POINT ( 'NONE',  ( 118.7397740163064128, 239.3615022471902307, -10.00000000000009592 ) ) ;
#41924 = CARTESIAN_POINT ( 'NONE',  ( 205.3704330671644414, 274.9349708856848338, -13.01557521325596944 ) ) ;
#41925 = CARTESIAN_POINT ( 'NONE',  ( 26.48321701407081363, 20.45404122711134320, -8.090169943749478065 ) ) ;
#41926 = ORIENTED_EDGE ( 'NONE', *, *, #46855, .F. ) ;
#41927 = CARTESIAN_POINT ( 'NONE',  ( 165.9969153545198708, 246.1123342570000716, -1.176638740111072723 ) ) ;
#41928 = VERTEX_POINT ( 'NONE', #45283 ) ;
#41929 = CARTESIAN_POINT ( 'NONE',  ( 162.8789161433191452, 248.5324370884573568, 9.731756914259689140 ) ) ;
#41930 = CARTESIAN_POINT ( 'NONE',  ( 66.66342508697567837, 67.67433879810248243, 6.129251300726011209 ) ) ;
#41931 = DIRECTION ( 'NONE',  ( -0.000000000000000000, -0.000000000000000000, 1.000000000000000000 ) ) ;
#41932 = ORIENTED_EDGE ( 'NONE', *, *, #44688, .T. ) ;
#41933 = CARTESIAN_POINT ( 'NONE',  ( 77.28032690913880742, 63.06041134881660781, -15.26474268318221483 ) ) ;
#41935 = EDGE_CURVE ( 'NONE', #98181, #76921, #73273, .T. ) ;
#41934 = ORIENTED_EDGE ( 'NONE', *, *, #36509, .F. ) ;
#41936 = CARTESIAN_POINT ( 'NONE',  ( 159.9635946688021022, 268.7707599091479551, -17.14635356962945778 ) ) ;
#41937 = FACE_OUTER_BOUND ( 'NONE', #64883, .T. ) ;
#41938 = CARTESIAN_POINT ( 'NONE',  ( 194.1483379205519100, 280.7941404440221049, -17.33680858677280767 ) ) ;
#41939 = CARTESIAN_POINT ( 'NONE',  ( 83.45060835225783080, 48.62234384012960930, 13.28461130177331739 ) ) ;
#41940 = CIRCLE ( 'NONE', #19339, 70.00000000000001421 ) ;
#41941 = ORIENTED_EDGE ( 'NONE', *, *, #92875, .F. ) ;
#41942 = CARTESIAN_POINT ( 'NONE',  ( 33.57875857642567752, 25.10170272979928896, -7.433330006724141015 ) ) ;
#41943 = CARTESIAN_POINT ( 'NONE',  ( 81.02328614318113864, 48.86991784794459193, -13.72398778456469515 ) ) ;
#41945 = EDGE_CURVE ( 'NONE', #17025, #27367, #77184, .T. ) ;
#41944 = DIRECTION ( 'NONE',  ( -1.000000000000000000, 0.000000000000000000, 0.000000000000000000 ) ) ;
#41946 = DIRECTION ( 'NONE',  ( -1.000000000000000000, 0.000000000000000000, 0.000000000000000000 ) ) ;
#41947 = EDGE_CURVE ( 'NONE', #39213, #38622, #70072, .T. ) ;
#41948 = ORIENTED_EDGE ( 'NONE', *, *, #46771, .F. ) ;
#41949 = EDGE_LOOP ( 'NONE', ( #16698, #68541, #70135, #19531, #84328, #29909 ) ) ;
#41950 = CARTESIAN_POINT ( 'NONE',  ( 198.8081898473356262, 282.3983615885804284, -17.60554210735202574 ) ) ;
#41952 = CARTESIAN_POINT ( 'NONE',  ( 194.8432095198904221, 293.1686569321988145, -14.74101036184996616 ) ) ;
#41951 = CARTESIAN_POINT ( 'NONE',  ( 204.3276935076901850, 276.7410487817560920, 13.46217427333259309 ) ) ;
#41953 = CARTESIAN_POINT ( 'NONE',  ( 85.66185486794186943, 48.65504738537000406, 12.40237352552430750 ) ) ;
#41954 = DIRECTION ( 'NONE',  ( -0.8660254037844387076, -0.4999999999999998890, -0.000000000000000000 ) ) ;
#41955 = CARTESIAN_POINT ( 'NONE',  ( 129.4748805805031395, 238.8927522451418781, 10.00000000000009948 ) ) ;
#41956 = CARTESIAN_POINT ( 'NONE',  ( 187.6335173687660927, 291.4025380883284697, -13.88432507550760953 ) ) ;
#41957 = CARTESIAN_POINT ( 'NONE',  ( 207.6895561066261280, 270.9181319523335674, -5.172192454743582246 ) ) ;
#41958 = CARTESIAN_POINT ( 'NONE',  ( 166.8954640849737530, 265.8187516957161165, 16.54619064527818395 ) ) ;
#41959 = CARTESIAN_POINT ( 'NONE',  ( 73.02433024948126672, 69.66517378990663190, 9.714162469163342806 ) ) ;
#41960 = CARTESIAN_POINT ( 'NONE',  ( 104.8563042601131770, 231.3458772461660544, 9.188101187500095079 ) ) ;
#41961 = VERTEX_POINT ( 'NONE', #76691 ) ;
#41962 = DIRECTION ( 'NONE',  ( -0.8660254037844384856, -0.5000000000000002220, -3.252519625699449945E-16 ) ) ;
#41963 = LINE ( 'NONE', #3490, #36657 ) ;
#41964 = CARTESIAN_POINT ( 'NONE',  ( 163.1341141637884959, 276.8030541846430310, -14.24718853740416868 ) ) ;
#41965 = VERTEX_POINT ( 'NONE', #69083 ) ;
#41966 = VERTEX_POINT ( 'NONE', #6297 ) ;
#41967 = CARTESIAN_POINT ( 'NONE',  ( 87.16910242261623409, 46.28252156386203353, -8.511466890639647787 ) ) ;
#41968 = CARTESIAN_POINT ( 'NONE',  ( 71.81073432603291451, 59.04159436426002827, 15.37513943015642326 ) ) ;
#41969 = CARTESIAN_POINT ( 'NONE',  ( 68.32264545644088116, 65.60716676607681563, 10.42805899469778730 ) ) ;
#41970 = CARTESIAN_POINT ( 'NONE',  ( 206.8106726053982811, 272.4404028303941914, -10.47827087991598560 ) ) ;
#41971 = CARTESIAN_POINT ( 'NONE',  ( 94.51795245455393513, 231.5024278399160949, 9.188101187500095079 ) ) ;
#41972 = VERTEX_POINT ( 'NONE', #6793 ) ;
#41973 = EDGE_LOOP ( 'NONE', ( #6238, #40581, #29893, #60394 ) ) ;
#41974 = EDGE_CURVE ( 'NONE', #23996, #14901, #25511, .T. ) ;
#41975 = CARTESIAN_POINT ( 'NONE',  ( 208.1612901671020381, 270.1010645919285480, -2.401583477149568768 ) ) ;
#41976 = ORIENTED_EDGE ( 'NONE', *, *, #50591, .T. ) ;
#41977 = CIRCLE ( 'NONE', #97062, 70.00000000000001421 ) ;
#41978 = CARTESIAN_POINT ( 'NONE',  ( 76.13295803453654287, 64.73339994552033261, -14.36036996180405190 ) ) ;
#41979 = CARTESIAN_POINT ( 'NONE',  ( 94.62531631345288474, 236.9860189848785410, -2.679491924311252493 ) ) ;
#41980 = CARTESIAN_POINT ( 'NONE',  ( 165.5677502601071183, 285.3540468067780580, 0.5650785607410294675 ) ) ;
#41982 = CARTESIAN_POINT ( 'NONE',  ( 198.8170977036201066, 284.5390304616801700, 17.67078396476120261 ) ) ;
#41981 = CARTESIAN_POINT ( 'NONE',  ( 134.8963869060034142, 254.8149278399161233, -9.188101187500095079 ) ) ;
#41983 = FACE_OUTER_BOUND ( 'NONE', #71541, .T. ) ;
#41984 = CARTESIAN_POINT ( 'NONE',  ( -19.65312891409030271, 93.06504152958497400, 10.00000000000000888 ) ) ;
#41985 = VECTOR ( 'NONE', #12492, 999.9999999999998863 ) ;
#41986 = VERTEX_POINT ( 'NONE', #54359 ) ;
#41987 = CARTESIAN_POINT ( 'NONE',  ( 204.3341445623842674, 276.7298752272635625, 14.23430099947301031 ) ) ;
#41988 = CARTESIAN_POINT ( 'NONE',  ( 160.7782940569628920, 275.4437765362630444, 13.33882116160937237 ) ) ;
#41989 = CARTESIAN_POINT ( 'NONE',  ( 82.80564809338142140, 40.64392876451551473, -1.326136484204850197 ) ) ;
#41990 = CARTESIAN_POINT ( 'NONE',  ( 192.2804853811905730, 271.9156663614426179, 14.15980414719692604 ) ) ;
#41991 = DIRECTION ( 'NONE',  ( 1.000000000000000000, 0.000000000000000000, 0.000000000000000000 ) ) ;
#41992 = CARTESIAN_POINT ( 'NONE',  ( -22.42236680055716036, 157.8615022471903444, 5.188172501216621122E-14 ) ) ;
#41993 = CARTESIAN_POINT ( 'NONE',  ( 198.8081898473356262, 282.3983615885804284, -17.60554210735202574 ) ) ;
#41994 = FACE_OUTER_BOUND ( 'NONE', #71346, .T. ) ;
#41995 = AXIS2_PLACEMENT_3D ( 'NONE', #7151, #84700, #51395 ) ;
#41996 = CARTESIAN_POINT ( 'NONE',  ( 153.4689407916852701, 266.8309924954582470, 16.62268559038933091 ) ) ;
#41997 = CARTESIAN_POINT ( 'NONE',  ( 82.94122475514203074, 41.44431412578434504, 2.647178600289170625 ) ) ;
#41998 = CARTESIAN_POINT ( 'NONE',  ( 206.7893622945242385, 272.4773133715531230, -10.52881283832460291 ) ) ;
#41999 = CARTESIAN_POINT ( 'NONE',  ( 78.13210272222134734, 61.89790046927922162, 15.71296101541392431 ) ) ;
#42000 = CARTESIAN_POINT ( 'NONE',  ( 118.0101279445459284, 227.3932355074535394, -2.679491924311248496 ) ) ;
#42001 = DIRECTION ( 'NONE',  ( -0.5803476755362181327, -0.8143688203140567738, 0.000000000000000000 ) ) ;
#42002 = CARTESIAN_POINT ( 'NONE',  ( 188.5410240070633563, 293.7196559869043426, 13.01390607220156248 ) ) ;
#42003 = EDGE_CURVE ( 'NONE', #21873, #33698, #84752, .T. ) ;
#42004 = CIRCLE ( 'NONE', #97094, 16.60714546451156792 ) ;
#42005 = CARTESIAN_POINT ( 'NONE',  ( 164.3524132573224392, 245.9802652221976587, -2.749586949851067441 ) ) ;
#42007 = CARTESIAN_POINT ( 'NONE',  ( 74.24776760725281122, 55.43361526745665202, 16.12181039901651403 ) ) ;
#42006 = CARTESIAN_POINT ( 'NONE',  ( 180.4743659044432036, 267.2657980451650133, -15.36156412806984406 ) ) ;
#42008 = LINE ( 'NONE', #27809, #77316 ) ;
#42009 = CARTESIAN_POINT ( 'NONE',  ( 31.60618414714233637, 41.18080186712595747, 3.090169943749475401 ) ) ;
#42010 = DIRECTION ( 'NONE',  ( 0.000000000000000000, 0.000000000000000000, 1.000000000000000000 ) ) ;
#42011 = CYLINDRICAL_SURFACE ( 'NONE', #63795, 10.00000000000010658 ) ;
#42012 = DIRECTION ( 'NONE',  ( -0.9439450758449140499, 0.3301025504114431519, 0.000000000000000000 ) ) ;
#42013 = CARTESIAN_POINT ( 'NONE',  ( 160.9546831504796387, 273.1595514402344520, -15.05126160413894176 ) ) ;
#42014 = CARTESIAN_POINT ( 'NONE',  ( 87.04297504979803080, 43.76764958495436275, -2.970215472454977412 ) ) ;
#42015 = CARTESIAN_POINT ( 'NONE',  ( 25.39882055865593458, 173.2202760586659736, -5.415160957724236172E-17 ) ) ;
#42016 = CARTESIAN_POINT ( 'NONE',  ( -19.65312891409030271, 93.06504152958497400, -10.00000000000000888 ) ) ;
#42017 = EDGE_LOOP ( 'NONE', ( #53409, #73127, #31343, #11950, #29464, #1839, #26524, #59025 ) ) ;
#42018 = CARTESIAN_POINT ( 'NONE',  ( 86.56732525555858615, 46.29823956478880120, 9.017236280094351741 ) ) ;
#42019 = CARTESIAN_POINT ( 'NONE',  ( 37.35373998880870516, 180.8262482093457493, 3.021315404115420679E-15 ) ) ;
#42020 = CARTESIAN_POINT ( 'NONE',  ( 164.0179800784044915, 246.5595204798204065, -5.772998092557310557 ) ) ;
#42021 = CARTESIAN_POINT ( 'NONE',  ( 82.22687830799615938, 41.30244536609086481, 5.429731213283951696 ) ) ;
#42022 = CARTESIAN_POINT ( 'NONE',  ( 34.70824655357364463, 190.8458772461660544, 9.188101187500095079 ) ) ;
#42023 = CARTESIAN_POINT ( 'NONE',  ( 161.8662906133268393, 250.2863559554455719, 14.03735902266321744 ) ) ;
#42024 = CARTESIAN_POINT ( 'NONE',  ( 190.3791419447713906, 300.9006487807255326, -5.688668718458480988 ) ) ;
#42025 = CARTESIAN_POINT ( 'NONE',  ( 41.21417716447173518, 24.76426979415093044, 3.090169943749476733 ) ) ;
#42026 = CARTESIAN_POINT ( 'NONE',  ( 178.8069409143749340, 291.7769763296440715, 6.074930007927774156 ) ) ;
#42027 = CARTESIAN_POINT ( 'NONE',  ( 146.5157004908022031, 276.8743579738231233, -0.1877253132609108255 ) ) ;
#42028 = CARTESIAN_POINT ( 'NONE',  ( 179.1308850641379138, 278.3362884085181008, -16.57857069867015554 ) ) ;
#42029 = CARTESIAN_POINT ( 'NONE',  ( 8.420521286406058792, 20.56454794089039240, 10.00000000000000355 ) ) ;
#42030 = CARTESIAN_POINT ( 'NONE',  ( 165.7783219637343848, 257.4631878547201609, -15.00105737115166527 ) ) ;
#42031 = DIRECTION ( 'NONE',  ( -0.9481851146622203297, -0.3177184104407421716, 0.000000000000000000 ) ) ;
#42032 = DIRECTION ( 'NONE',  ( -0.9923183454821322691, -0.1237105541964931832, 0.000000000000000000 ) ) ;
#42033 = CARTESIAN_POINT ( 'NONE',  ( 73.27344031762333998, 223.1115022471903160, -5.000000000000047962 ) ) ;
#42034 = CARTESIAN_POINT ( 'NONE',  ( 29.59124024723001156, 43.31574901297117464, 177.5919119679930134 ) ) ;
#42035 = DIRECTION ( 'NONE',  ( 0.000000000000000000, 0.000000000000000000, 1.000000000000000000 ) ) ;
#42036 = CARTESIAN_POINT ( 'NONE',  ( 52.11020483269097525, 191.7048013555409796, 4.594050593750051981 ) ) ;
#42037 = ORIENTED_EDGE ( 'NONE', *, *, #57213, .T. ) ;
#42038 = CARTESIAN_POINT ( 'NONE',  ( -6.063985638175826587, 82.91156382185207008, 13.42466032036877266 ) ) ;
#42039 = CARTESIAN_POINT ( 'NONE',  ( 150.6626254231123880, 269.6916732958875969, -15.32062296289003811 ) ) ;
#42041 = LINE ( 'NONE', #50145, #92001 ) ;
#42040 = VECTOR ( 'NONE', #55636, 1000.000000000000000 ) ;
#42042 = ORIENTED_EDGE ( 'NONE', *, *, #98548, .T. ) ;
#42043 = CARTESIAN_POINT ( 'NONE',  ( 167.6793603611326944, 285.0233743312336969, 7.699659890578392840 ) ) ;
#42044 = CARTESIAN_POINT ( 'NONE',  ( 207.4764081617721843, 271.2873150223495600, 6.359972247200924578 ) ) ;
#42045 = CARTESIAN_POINT ( 'NONE',  ( -17.42236680055705023, 149.2012482093457777, 0.000000000000000000 ) ) ;
#42046 = CARTESIAN_POINT ( 'NONE',  ( 31.84670776885679899, 24.10170272979928541, -7.433330006724141015 ) ) ;
#42047 = CARTESIAN_POINT ( 'NONE',  ( 72.99862419887072917, 70.74432240184056297, -7.503600154403820000 ) ) ;
#42048 = CARTESIAN_POINT ( 'NONE',  ( 86.34910853269747122, 47.57366130196511023, -10.59375139789182008 ) ) ;
#42049 = CARTESIAN_POINT ( 'NONE',  ( 171.3238289833617500, 255.7752812501198889, 11.47896718753802858 ) ) ;
#42050 = ORIENTED_EDGE ( 'NONE', *, *, #25564, .F. ) ;
#42051 = CARTESIAN_POINT ( 'NONE',  ( 17.19524200933981817, 21.87878583063841020, -9.188101187500006262 ) ) ;
#42052 = DIRECTION ( 'NONE',  ( 0.4330127018922168558, -0.7499999999999987788, 0.5000000000000039968 ) ) ;
#42053 = VERTEX_POINT ( 'NONE', #44776 ) ;
#42055 = ADVANCED_FACE ( 'NONE', ( #68089 ), #53865, .T. ) ;
#42054 = CARTESIAN_POINT ( 'NONE',  ( 72.41184042289110323, 71.17856470982957262, -6.087003264457405471 ) ) ;
#42056 = DIRECTION ( 'NONE',  ( -0.8660254037844387076, -0.4999999999999998890, -0.000000000000000000 ) ) ;
#42057 = CARTESIAN_POINT ( 'NONE',  ( 177.9144328244200040, 254.9604715414552345, -7.067334745369662663 ) ) ;
#42058 = DIRECTION ( 'NONE',  ( 0.6066398774942437511, -0.7949767663484065272, 0.000000000000000000 ) ) ;
#42059 = ADVANCED_FACE ( 'NONE', ( #85331 ), #100008, .T. ) ;
#42060 = ORIENTED_EDGE ( 'NONE', *, *, #153, .T. ) ;
#42061 = AXIS2_PLACEMENT_3D ( 'NONE', #59046, #95641, #50469 ) ;
#42062 = ORIENTED_EDGE ( 'NONE', *, *, #94145, .T. ) ;
#42064 = CYLINDRICAL_SURFACE ( 'NONE', #49209, 70.00000000000002842 ) ;
#42063 = CARTESIAN_POINT ( 'NONE',  ( 207.8232941427535536, 270.6864908788566026, -6.505149060073906142 ) ) ;
#42065 = B_SPLINE_CURVE_WITH_KNOTS ( 'NONE', 3,
 ( #10010, #8997, #23186, #93634, #62681, #70806, #69296, #30805, #25191, #31290, #40378, #55082, #401, #54571, #55575, #54079, #8503, #70288, #69791, #100220, #56073, #77410, #24201, #85032, #87067, #61685, #86068, #8015, #16594, #17599, #92637, #79445, #63699, #1909, #32294, #32790, #47490, #38888, #86558, #39373, #900, #15578 ),
 .UNSPECIFIED., .F., .F.,
 ( 4, 2, 2, 2, 2, 2, 2, 2, 2, 2, 2, 2, 2, 2, 2, 2, 2, 2, 2, 2, 4 ),
 ( 0.0009151626340143699393, 0.001011832196295166806, 0.001108501758575963780, 0.001205171320856760755, 0.001301840883137557730, 0.001495180007699081857, 0.001688519132260605984, 0.002461875630506861218, 0.004008588626999308804, 0.004781945125245484242, 0.005168623374368607956, 0.005361962498930214482, 0.005458632061211052440, 0.005555301623491891265, 0.005603636404632282055, 0.005651971185772672844, 0.005748640748053380697, 0.005941979872614794669, 0.006328658121737632154, 0.006715336370860470507, 0.007102014619983307124 ),
 .UNSPECIFIED. ) ;
#42066 = CARTESIAN_POINT ( 'NONE',  ( 186.2990562447640741, 264.8370073322022336, -13.43280071233020934 ) ) ;
#42067 = ORIENTED_EDGE ( 'NONE', *, *, #60928, .F. ) ;
#42068 = CARTESIAN_POINT ( 'NONE',  ( 65.90172229746312382, 68.93994708409050531, -2.596590423560799277 ) ) ;
#42069 = EDGE_CURVE ( 'NONE', #40669, #13902, #39583, .T. ) ;
#42070 = DIRECTION ( 'NONE',  ( 0.8660254037844382635, 0.5000000000000005551, 0.000000000000000000 ) ) ;
#42071 = CARTESIAN_POINT ( 'NONE',  ( 72.87657325132509811, 57.63168087469550471, -16.31100355619141595 ) ) ;
#42072 = CARTESIAN_POINT ( 'NONE',  ( 78.01756760496483878, 61.41364688087467272, -16.16017056289257425 ) ) ;
#42074 = ADVANCED_FACE ( 'NONE', ( #31569 ), #84826, .T. ) ;
#42073 = CARTESIAN_POINT ( 'NONE',  ( 205.3704330671644414, 274.9349708856848338, -13.01557521325596944 ) ) ;
#42075 = CARTESIAN_POINT ( 'NONE',  ( 109.6190968851625769, 246.3464784336661353, 1.353441290958777525E-15 ) ) ;
#42076 = B_SPLINE_CURVE_WITH_KNOTS ( 'NONE', 3,
 ( #14538, #38309, #69217, #100145 ),
 .UNSPECIFIED., .F., .F.,
 ( 4, 4 ),
 ( 0.002091524323244029187, 0.007431800589236895946 ),
 .UNSPECIFIED. ) ;
#42077 = CARTESIAN_POINT ( 'NONE',  ( 164.4915767550571957, 245.7392269735623529, -6.407198159945809657 ) ) ;
#42078 = ORIENTED_EDGE ( 'NONE', *, *, #23312, .T. ) ;
#42079 = CARTESIAN_POINT ( 'NONE',  ( 33.72069078606260462, 37.65586893147758474, -7.433330006724137462 ) ) ;
#42080 = CARTESIAN_POINT ( 'NONE',  ( 198.3523905153085423, 287.0905771551796306, 18.52598547438866206 ) ) ;
#42081 = CARTESIAN_POINT ( 'NONE',  ( 204.7753828612366931, 275.5785558422823556, -12.39807726186342052 ) ) ;
#42082 = CARTESIAN_POINT ( 'NONE',  ( 69.59257202794182717, 220.1744531367911293, 4.594050593750047540 ) ) ;
#42083 = CARTESIAN_POINT ( 'NONE',  ( -31.86071352217370034, 96.30357957927230927, 12.03701289477871761 ) ) ;
#42084 = CARTESIAN_POINT ( 'NONE',  ( 191.0170959869219303, 299.7956799668270946, 7.353346939903929069 ) ) ;
#42085 = CARTESIAN_POINT ( 'NONE',  ( 198.7255181831150423, 286.4443010768291629, 17.42756903872921725 ) ) ;
#42086 = CARTESIAN_POINT ( 'NONE',  ( 175.6569888586722072, 278.3733240093107497, 15.53892781902675857 ) ) ;
#42087 = VERTEX_POINT ( 'NONE', #8787 ) ;
#42088 = CARTESIAN_POINT ( 'NONE',  ( 75.61360636200772944, 58.23975808111319452, -16.00195830399037789 ) ) ;
#42089 = CARTESIAN_POINT ( 'NONE',  ( 86.32174514625263839, 43.39275037566977034, -2.929684509001238446 ) ) ;
#42090 = CARTESIAN_POINT ( 'NONE',  ( 66.23050080230359526, 68.70569274131929660, -4.319124887654028022 ) ) ;
#42091 = ORIENTED_EDGE ( 'NONE', *, *, #89789, .F. ) ;
#42092 = CARTESIAN_POINT ( 'NONE',  ( 191.4738032422262677, 260.7793432447242594, -0.2951778641931921410 ) ) ;
#42093 = CARTESIAN_POINT ( 'NONE',  ( -110.0000000000000142, -8.000000000000000000, 14.21260523776214590 ) ) ;
#42094 = CARTESIAN_POINT ( 'NONE',  ( 160.9608998348622890, 258.6124335639508445, -16.62975727638092494 ) ) ;
#42095 = CARTESIAN_POINT ( 'NONE',  ( 206.5803147552910275, 270.4199738506200674, 1.964338299035684576 ) ) ;
#42096 = CARTESIAN_POINT ( 'NONE',  ( 149.1856130393175306, 272.2499337880290682, 11.44243872309708188 ) ) ;
#42097 = CARTESIAN_POINT ( 'NONE',  ( 176.9380622633689768, 269.9288259353154444, 16.55129804831395646 ) ) ;
#42098 = CARTESIAN_POINT ( 'NONE',  ( 165.0020474182383339, 244.8550658491588479, 1.825383354618924425 ) ) ;
#42099 = CARTESIAN_POINT ( 'NONE',  ( -22.42236680055709641, 157.8615022471902591, 0.000000000000000000 ) ) ;
#42100 = CARTESIAN_POINT ( 'NONE',  ( 164.8383744266741928, 254.7166954803307704, 14.02974467908927814 ) ) ;
#42101 = CARTESIAN_POINT ( 'NONE',  ( 164.4405316900629259, 245.8276396196081350, -6.144538123479245328 ) ) ;
#42102 = CARTESIAN_POINT ( 'NONE',  ( 115.9249311304092771, 246.9244531367911293, -4.594050593750046652 ) ) ;
#42103 = ORIENTED_EDGE ( 'NONE', *, *, #41935, .F. ) ;
#42104 = CARTESIAN_POINT ( 'NONE',  ( 87.14406544511430752, 44.30059231523330965, -4.700414329343145958 ) ) ;
#42105 = CARTESIAN_POINT ( 'NONE',  ( 84.75647422269858566, 42.83139927231500366, 4.116084768947018802 ) ) ;
#42106 = CARTESIAN_POINT ( 'NONE',  ( 203.2369479875374623, 278.6302754407888074, -16.66242713208754367 ) ) ;
#42107 = CARTESIAN_POINT ( 'NONE',  ( 163.9942050550062049, 246.6007000282974673, 5.791111691696777974 ) ) ;
#42108 = CARTESIAN_POINT ( 'NONE',  ( 75.00576775672064400, 62.30322666060470738, 15.01846280378952692 ) ) ;
#42109 = CARTESIAN_POINT ( 'NONE',  ( 177.8766753057446408, 255.3238193400180194, 4.872644976819591633 ) ) ;
#42110 = EDGE_LOOP ( 'NONE', ( #71596, #74362, #85756, #66750, #90845, #29725, #13055, #50868, #58399, #57989, #13915, #77697, #70188, #18926, #28848, #58992, #65234, #23343, #29013, #25073 ) ) ;
#42111 = CARTESIAN_POINT ( 'NONE',  ( 80.07812099633126479, 57.44764983040322903, -16.59488970948942921 ) ) ;
#42112 = CARTESIAN_POINT ( 'NONE',  ( 71.69140363859698084, 72.11128586088413783, 0.6349804937391964055 ) ) ;
#42114 = DIRECTION ( 'NONE',  ( 0.000000000000000000, 0.000000000000000000, 1.000000000000000000 ) ) ;
#42113 = CARTESIAN_POINT ( 'NONE',  ( 147.6620395981771878, 275.3265400130114244, 3.458083620816670312 ) ) ;
#42115 = CARTESIAN_POINT ( 'NONE',  ( 164.7349053118283564, 245.3177695503021027, -2.492200678360605437 ) ) ;
#42116 = CARTESIAN_POINT ( 'NONE',  ( 139.7681268980558968, 245.3768266524160140, -9.188101187500093303 ) ) ;
#42117 = VECTOR ( 'NONE', #26695, 1000.000000000000000 ) ;
#42118 = CARTESIAN_POINT ( 'NONE',  ( 146.8729474948188454, 276.2555880120147549, 3.934020695290606273 ) ) ;
#42119 = CARTESIAN_POINT ( 'NONE',  ( 68.26860836083196205, 69.12837558592964626, 4.919393711847383166 ) ) ;
#42120 = EDGE_CURVE ( 'NONE', #68198, #67601, #86928, .T. ) ;
#42121 = CARTESIAN_POINT ( 'NONE',  ( 171.3262007583307138, 250.8544493858235285, 3.410168526935229760 ) ) ;
#42122 = B_SPLINE_CURVE_WITH_KNOTS ( 'NONE', 3,
 ( #83218, #45174, #21877, #69473, #92324, #77070, #45659, #22378, #53276, #20914, #91317, #37079, #52763, #30476, #87, #14777 ),
 .UNSPECIFIED., .F., .F.,
 ( 4, 1, 2, 2, 2, 1, 2, 2, 4 ),
 ( 0.000000000000000000, 0.1249999999999992784, 0.1874999999999985567, 0.2499999999999978351, 0.4999999999999981126, 0.6249999999999982236, 0.6874999999999981126, 0.7499999999999980016, 1.000000000000000000 ),
 .UNSPECIFIED. ) ;
#42123 = CARTESIAN_POINT ( 'NONE',  ( 16.98334746987260147, 25.50829794293879615, -10.00000000000000355 ) ) ;
#42124 = CARTESIAN_POINT ( 'NONE',  ( 149.2511585606875428, 272.1364056148075292, 11.40684181024752242 ) ) ;
#42125 = CARTESIAN_POINT ( 'NONE',  ( 154.9848759717382336, 280.4844015978009111, -0.8777400808273079225 ) ) ;
#42126 = CARTESIAN_POINT ( 'NONE',  ( 171.4620503856968412, 287.6916138556427995, -8.596052341455351353 ) ) ;
#42127 = CARTESIAN_POINT ( 'NONE',  ( 160.7872435741957133, 280.1341495971591939, 10.66000836593391199 ) ) ;
#42128 = CARTESIAN_POINT ( 'NONE',  ( 157.4866207245044052, 271.0942435755181350, -14.66448764132394089 ) ) ;
#42129 = CARTESIAN_POINT ( 'NONE',  ( 132.8668134119921547, 247.5177522451418497, -10.00000000000009592 ) ) ;
#42130 = CARTESIAN_POINT ( 'NONE',  ( 77.49896415157103036, 52.88957495811840204, -15.80880303492994443 ) ) ;
#42131 = ORIENTED_EDGE ( 'NONE', *, *, #22404, .T. ) ;
#42132 = EDGE_CURVE ( 'NONE', #22055, #7928, #87859, .T. ) ;
#42133 = CARTESIAN_POINT ( 'NONE',  ( 196.2609093297512857, 290.7131288316392670, 16.03897268885959448 ) ) ;
#42134 = CARTESIAN_POINT ( 'NONE',  ( 148.4016473149517594, 273.6078022540229426, 8.470066617688926769 ) ) ;
#42135 = CARTESIAN_POINT ( 'NONE',  ( -4.262896616726100874, 168.3458772461660544, 9.188101187500095079 ) ) ;
#42136 = CARTESIAN_POINT ( 'NONE',  ( 43.58535403812915376, 183.7202760586659736, -5.415160957724236172E-17 ) ) ;
#42137 = CARTESIAN_POINT ( 'NONE',  ( 178.5646908849556951, 273.7108284848578705, -17.39287981145522721 ) ) ;
#42138 = CARTESIAN_POINT ( 'NONE',  ( 88.14558033319170249, 43.66656252067526367, 0.1579512601322914100 ) ) ;
#42139 = DIRECTION ( 'NONE',  ( -0.8660254037844387076, -0.4999999999999998890, -0.000000000000000000 ) ) ;
#42140 = CARTESIAN_POINT ( 'NONE',  ( 72.26473847452083987, 72.05163828152960548, -3.296940183535202351 ) ) ;
#42141 = CARTESIAN_POINT ( 'NONE',  ( 190.7569505155522904, 300.2462651405980978, -5.670926626284815697 ) ) ;
#42142 = CARTESIAN_POINT ( 'NONE',  ( 73.83097814971496575, 55.11266741107668565, -16.12521890440442718 ) ) ;
#42144 = CARTESIAN_POINT ( 'NONE',  ( 64.01779381112933720, 197.7677522451418213, -5.000000000000041744 ) ) ;
#42143 = CARTESIAN_POINT ( 'NONE',  ( 166.5497620933320775, 284.9599651698292178, -8.643830016708903941 ) ) ;
#42145 = CARTESIAN_POINT ( 'NONE',  ( 181.0761428174893126, 255.7875309544736524, 2.145717405531494926 ) ) ;
#42146 = CARTESIAN_POINT ( 'NONE',  ( 157.3661765229227285, 258.0807821998820373, -18.27254492731150748 ) ) ;
#42147 = CARTESIAN_POINT ( 'NONE',  ( 167.4564344753456453, 270.0695307704535821, -17.68371939062425824 ) ) ;
#42148 = CARTESIAN_POINT ( 'NONE',  ( 161.6411385815104609, 267.5259986109867327, 16.53943407798323761 ) ) ;
#42149 = CARTESIAN_POINT ( 'NONE',  ( 52.48883062679690426, 191.1115022471902023, -5.000000000000041744 ) ) ;
#42150 = CARTESIAN_POINT ( 'NONE',  ( 181.6034186054171187, 291.9446207410121019, 9.020533753185340231 ) ) ;
#42151 = CARTESIAN_POINT ( 'NONE',  ( -105.0000000000000000, 4.999999999999999112, 59.99999999999999289 ) ) ;
#42152 = CARTESIAN_POINT ( 'NONE',  ( 5.344833028331274605, 164.7048013555410080, 4.594050593750051981 ) ) ;
#42153 = CARTESIAN_POINT ( 'NONE',  ( 37.36761971798259196, 27.28920272979929607, -7.433330006724141015 ) ) ;
#42155 = CARTESIAN_POINT ( 'NONE',  ( 165.0735250206753619, 246.7312630101393722, 5.989302113854410692 ) ) ;
#42154 = B_SPLINE_CURVE_WITH_KNOTS ( 'NONE', 3,
 ( #24122, #76349, #85991, #16518 ),
 .UNSPECIFIED., .F., .F.,
 ( 4, 4 ),
 ( 0.007172802622825931278, 0.01294203102117486362 ),
 .UNSPECIFIED. ) ;
#42156 = CARTESIAN_POINT ( 'NONE',  ( 152.6757560589063303, 266.2048287524194166, 16.73757896668104195 ) ) ;
#42157 = CARTESIAN_POINT ( 'NONE',  ( 30.81771801958594281, 39.83396525600392835, -2.839279412974133887 ) ) ;
#42158 = CARTESIAN_POINT ( 'NONE',  ( 206.5117639185820906, 272.9581278627833285, 11.28485531511759099 ) ) ;
#42159 = CARTESIAN_POINT ( 'NONE',  ( 182.5090719219444395, 278.4899130783974215, 16.60092655590875310 ) ) ;
#42160 = CARTESIAN_POINT ( 'NONE',  ( 81.19656099875513178, 43.43094936621162105, -9.896970666190503252 ) ) ;
#42161 = CARTESIAN_POINT ( 'NONE',  ( 196.2293283710122012, 290.7678286567270902, -17.07152402978540096 ) ) ;
#42162 = CARTESIAN_POINT ( 'NONE',  ( 176.5849886759608864, 260.5643506436040866, -13.27287686889044593 ) ) ;
#42163 = DIRECTION ( 'NONE',  ( 0.000000000000000000, 0.000000000000000000, 1.000000000000000000 ) ) ;
#42164 = CARTESIAN_POINT ( 'NONE',  ( 11.67313376208573139, 15.24335787977761747, -9.188101187500008038 ) ) ;
#42165 = CARTESIAN_POINT ( 'NONE',  ( 165.5685896552094221, 285.4467981318400120, 0.1671104821641794524 ) ) ;
#42166 = CARTESIAN_POINT ( 'NONE',  ( 13.49720994389718598, 29.83396525600389637, -2.839279412974133887 ) ) ;
#42167 = CARTESIAN_POINT ( 'NONE',  ( 159.1502228898632154, 259.4266978733254518, 16.68670530085068648 ) ) ;
#42168 = CARTESIAN_POINT ( 'NONE',  ( 152.9700320981889092, 277.5340873795012726, -5.209865602531399631 ) ) ;
#42169 = CARTESIAN_POINT ( 'NONE',  ( 156.8724508569020202, 276.4746155548443198, 10.35837630302414425 ) ) ;
#42170 = B_SPLINE_CURVE_WITH_KNOTS ( 'NONE', 3,
 ( #5312, #35202, #97054, #75217 ),
 .UNSPECIFIED., .F., .F.,
 ( 4, 4 ),
 ( 0.009368188378409090036, 0.01456212696257992191 ),
 .UNSPECIFIED. ) ;
#42171 = CARTESIAN_POINT ( 'NONE',  ( 159.7132918459648181, 254.0154592091499239, -16.90058287995827158 ) ) ;
#42172 = EDGE_CURVE ( 'NONE', #70733, #68153, #43177, .T. ) ;
#42173 = VERTEX_POINT ( 'NONE', #79735 ) ;
#42174 = LINE ( 'NONE', #52751, #97522 ) ;
#42175 = CARTESIAN_POINT ( 'NONE',  ( 206.8968397926183229, 272.2911568841838061, 7.145103750817420440 ) ) ;
#42176 = CARTESIAN_POINT ( 'NONE',  ( 203.1399666651039695, 272.9695736541691531, -12.09293310806949684 ) ) ;
#42177 = CARTESIAN_POINT ( 'NONE',  ( 87.54989630752690744, 45.07147448993671901, 6.930566558073848249 ) ) ;
#42178 = ORIENTED_EDGE ( 'NONE', *, *, #11686, .F. ) ;
#42179 =( BOUNDED_CURVE ( )  B_SPLINE_CURVE ( 2, ( #99414, #45674, #46168, #30987, #67997, #62370, #76599, #99909, #61873, #93327, #30494, #92337, #29498 ),
 .UNSPECIFIED., .F., .T. ) 
 B_SPLINE_CURVE_WITH_KNOTS ( ( 3, 2, 2, 2, 2, 2, 3 ),
 ( 0.8125000000000000000, 0.8149999999999999467, 0.8199999999999999512, 0.8249999999999999556, 0.8299999999999999600, 0.8349999999999999645, 0.8375000000000000222 ),
 .UNSPECIFIED. ) 
 CURVE ( )  GEOMETRIC_REPRESENTATION_ITEM ( )  RATIONAL_B_SPLINE_CURVE ( ( 0.9755282581475768211, 0.9755282581475768211, 1.000000000000000000, 0.9510565162951535312, 1.000000000000000000, 0.9510565162951535312, 1.000000000000000000, 0.9510565162951535312, 1.000000000000000000, 0.9510565162951535312, 1.000000000000000000, 0.9755282581475761550, 0.9755282581475767101 ) ) 
 REPRESENTATION_ITEM ( '' )  );
#42180 = ORIENTED_EDGE ( 'NONE', *, *, #88176, .T. ) ;
#42181 = CARTESIAN_POINT ( 'NONE',  ( 159.5098919638083146, 279.0616708731288327, -9.454383224537151520 ) ) ;
#42182 = CARTESIAN_POINT ( 'NONE',  ( 86.12260107077111115, 47.06852444819536885, 10.76136662946663947 ) ) ;
#42183 = ORIENTED_EDGE ( 'NONE', *, *, #25840, .T. ) ;
#42184 = CARTESIAN_POINT ( 'NONE',  ( 80.15404930735284950, 58.24487849859603017, -16.60713908503101877 ) ) ;
#42185 = CARTESIAN_POINT ( 'NONE',  ( 174.3232990571352730, 262.5854648150144044, 14.90850430120301340 ) ) ;
#42186 = ORIENTED_EDGE ( 'NONE', *, *, #24850, .F. ) ;
#42188 = EDGE_CURVE ( 'NONE', #26733, #59353, #93929, .T. ) ;
#42187 = CARTESIAN_POINT ( 'NONE',  ( 28.73071361209859731, 38.36126292948897287, 6.180339887498949913 ) ) ;
#42189 = CARTESIAN_POINT ( 'NONE',  ( 79.79546047556335964, 49.97060089421696460, -14.59098784290960538 ) ) ;
#42190 = CARTESIAN_POINT ( 'NONE',  ( 149.7072529793668707, 271.3464269086063041, -11.98883662638834657 ) ) ;
#42191 = CARTESIAN_POINT ( 'NONE',  ( 43.23318412030279489, 185.7677522451417929, -5.000000000000041744 ) ) ;
#42192 = VERTEX_POINT ( 'NONE', #47766 ) ;
#42193 = CARTESIAN_POINT ( 'NONE',  ( 161.6673510627899191, 250.6309293646106653, 13.01175935005004192 ) ) ;
#42194 = CARTESIAN_POINT ( 'NONE',  ( 166.1236709775900238, 274.1391546445065615, -15.19174922871369837 ) ) ;
#42195 = DIRECTION ( 'NONE',  ( -1.110223024625156343E-15, 1.000000000000000000, 0.000000000000000000 ) ) ;
#42196 = ORIENTED_EDGE ( 'NONE', *, *, #70287, .F. ) ;
#42197 = CARTESIAN_POINT ( 'NONE',  ( 174.6250001500969518, 276.7190186761092150, -16.51844552091739615 ) ) ;
#42198 = VERTEX_POINT ( 'NONE', #78705 ) ;
#42199 = CARTESIAN_POINT ( 'NONE',  ( 156.9962301082478859, 266.1307905592512952, -17.22057167171774950 ) ) ;
#42200 = ORIENTED_EDGE ( 'NONE', *, *, #42792, .F. ) ;
#42201 = CARTESIAN_POINT ( 'NONE',  ( 157.5483139352812998, 268.8664552472071705, 15.62089565001041791 ) ) ;
#42202 = VECTOR ( 'NONE', #63492, 1000.000000000000114 ) ;
#42203 = VERTEX_POINT ( 'NONE', #79240 ) ;
#42204 = CARTESIAN_POINT ( 'NONE',  ( 193.6030392054437357, 295.3166949268590997, 13.33385638216535263 ) ) ;
#42205 = CARTESIAN_POINT ( 'NONE',  ( 189.5599828453989346, 263.0657735508838186, -9.804501003715218488 ) ) ;
#42206 = CARTESIAN_POINT ( 'NONE',  ( 71.65767651694793017, 69.82614052466774979, 7.647303713463401209 ) ) ;
#42207 = CARTESIAN_POINT ( 'NONE',  ( 192.4380962356868281, 295.3344353383980661, 13.50754959408193656 ) ) ;
#42208 = CARTESIAN_POINT ( 'NONE',  ( 87.35192423430838460, 43.74464389095077621, 1.893651613221468688 ) ) ;
#42209 = CARTESIAN_POINT ( 'NONE',  ( 158.6799548824769772, 255.8052513312497638, -17.63511970826639441 ) ) ;
#42210 = EDGE_LOOP ( 'NONE', ( #90831, #20622, #68364, #24247, #28547 ) ) ;
#42211 = CARTESIAN_POINT ( 'NONE',  ( 92.59663213601572807, 234.2677522451419065, -5.000000000000047962 ) ) ;
#42212 = CARTESIAN_POINT ( 'NONE',  ( 22.71735025659390317, 28.51421378149919406, -9.188101187500004485 ) ) ;
#42213 = CARTESIAN_POINT ( 'NONE',  ( 205.8452707775803390, 274.1125278458945900, 11.42742867493066328 ) ) ;
#42215 = CARTESIAN_POINT ( 'NONE',  ( 205.9240884482826175, 273.9760116357041966, 10.27504561427317142 ) ) ;
#42214 = CARTESIAN_POINT ( 'NONE',  ( 166.8906917922102480, 254.4375966883865487, 14.01000126778575527 ) ) ;
#42217 = ORIENTED_EDGE ( 'NONE', *, *, #53027, .T. ) ;
#42216 = CARTESIAN_POINT ( 'NONE',  ( 159.9671766634011192, 253.5757178060795809, 16.49140845334465411 ) ) ;
#42218 = ORIENTED_EDGE ( 'NONE', *, *, #15571, .F. ) ;
#42219 = CARTESIAN_POINT ( 'NONE',  ( 146.6676967921120820, 276.6110926573920779, -3.425452920967749115 ) ) ;
#42220 = CARTESIAN_POINT ( 'NONE',  ( 69.32645819574260315, 62.94046279709883152, 13.62531992251986246 ) ) ;
#42221 = CARTESIAN_POINT ( 'NONE',  ( -62.95439910331221256, 68.06504152958493137, 60.00000000000000000 ) ) ;
#42222 = CARTESIAN_POINT ( 'NONE',  ( -71.07364842061382149, 47.42355933771584375, -10.00000000000000000 ) ) ;
#42223 = CARTESIAN_POINT ( 'NONE',  ( 198.8820006463426182, 286.1732655000252521, -17.07140226101661185 ) ) ;
#42224 = CARTESIAN_POINT ( 'NONE',  ( 190.4787930012176105, 300.7280480879330753, -0.07093684169630354308 ) ) ;
#42225 = EDGE_LOOP ( 'NONE', ( #30578, #74856, #76094, #44183 ) ) ;
#42226 = DIRECTION ( 'NONE',  ( -0.5000000000000014433, 0.8660254037844378194, -0.000000000000000000 ) ) ;
#42227 = CARTESIAN_POINT ( 'NONE',  ( 9.861089372814316079, 17.64441083166259006, -10.00000000000000533 ) ) ;
#42228 = CARTESIAN_POINT ( 'NONE',  ( 51.48077938449444702, 188.9824982072973967, 3.021315404115420679E-15 ) ) ;
#42229 = CARTESIAN_POINT ( 'NONE',  ( -5.967884128652756637, 167.3615022471902591, -10.00000000000009592 ) ) ;
#42230 = CARTESIAN_POINT ( 'NONE',  ( 33.34606076043043998, 183.3927522451418213, 10.00000000000009592 ) ) ;
#42231 = CARTESIAN_POINT ( 'NONE',  ( 91.10780387927019319, 235.6589784336661353, -6.496448406907676862E-16 ) ) ;
#42232 = DIRECTION ( 'NONE',  ( -0.9133924323370935516, 0.1624253398589796948, -0.3732723851573047091 ) ) ;
#42233 = DIRECTION ( 'NONE',  ( 0.2938926261462335709, -0.5090369604551240323, 0.8090169943749504489 ) ) ;
#42234 = CARTESIAN_POINT ( 'NONE',  ( 163.0076983195990294, 254.4055174419354159, -15.32059749880538568 ) ) ;
#42235 = CARTESIAN_POINT ( 'NONE',  ( 12.11013585174968554, 186.9869531367911293, 4.594050593750046652 ) ) ;
#42236 = EDGE_CURVE ( 'NONE', #45437, #1972, #10296, .T. ) ;
#42237 = CARTESIAN_POINT ( 'NONE',  ( 161.5056331467593225, 250.9110330116698435, 14.52719814064025528 ) ) ;
#42238 = VERTEX_POINT ( 'NONE', #55856 ) ;
#42239 = ORIENTED_EDGE ( 'NONE', *, *, #30639, .T. ) ;
#42240 = CARTESIAN_POINT ( 'NONE',  ( 185.2106478887846777, 259.7847997664600257, -5.498830920350593843 ) ) ;
#42241 = ADVANCED_FACE ( 'NONE', ( #48294 ), #96712, .T. ) ;
#42242 = CARTESIAN_POINT ( 'NONE',  ( 78.36279588851795097, 47.41043415324340771, -13.73196331463247688 ) ) ;
#42243 = CARTESIAN_POINT ( 'NONE',  ( 75.98104421109889017, 51.53574906954564483, 16.18761828508177203 ) ) ;
#42244 = CARTESIAN_POINT ( 'NONE',  ( 193.1049081091807125, 263.9287996605999638, -4.331719323007160227 ) ) ;
#42245 = CARTESIAN_POINT ( 'NONE',  ( 161.3773209892555371, 251.1332761876949746, -14.50043705923759241 ) ) ;
#42246 = CARTESIAN_POINT ( 'NONE',  ( 144.9899443387551798, 254.5170451491295296, 0.000000000000000000 ) ) ;
#42247 = CARTESIAN_POINT ( 'NONE',  ( 168.1916425577783514, 251.6829154642088895, 10.62658168803038095 ) ) ;
#42248 = CARTESIAN_POINT ( 'NONE',  ( 49.16021902710897251, 193.0643266524159856, -9.188101187500093303 ) ) ;
#42249 = CARTESIAN_POINT ( 'NONE',  ( 88.62734903533704767, 228.6427522451418781, -10.00000000000009415 ) ) ;
#42250 = ORIENTED_EDGE ( 'NONE', *, *, #87525, .F. ) ;
#42251 = EDGE_CURVE ( 'NONE', #70967, #49038, #97895, .T. ) ;
#42252 = CARTESIAN_POINT ( 'NONE',  ( 78.99848661620951873, 60.24637179098722584, -16.44349368446545867 ) ) ;
#42253 = CARTESIAN_POINT ( 'NONE',  ( 58.97569090598251762, 178.8759306620404175, 17.47570218321536473 ) ) ;
#42254 = CARTESIAN_POINT ( 'NONE',  ( -2.639098984630277922, 169.2833772461660828, -9.188101187500095079 ) ) ;
#42255 = CARTESIAN_POINT ( 'NONE',  ( -19.65312891409030271, 93.06504152958497400, 177.5919119679930134 ) ) ;
#42256 = CARTESIAN_POINT ( 'NONE',  ( 198.7357616895271804, 286.4265588032756114, -17.04018524297827497 ) ) ;
#42257 = CARTESIAN_POINT ( 'NONE',  ( 179.0080424117914220, 253.6959867325634264, -1.969551310178471404 ) ) ;
#42258 = CARTESIAN_POINT ( 'NONE',  ( 146.7944005049231180, 276.3916353892955726, -4.243051111306586520 ) ) ;
#42259 = FACE_OUTER_BOUND ( 'NONE', #24525, .T. ) ;
#42260 = DIRECTION ( 'NONE',  ( -0.000000000000000000, 0.000000000000000000, 1.000000000000000000 ) ) ;
#42261 = CARTESIAN_POINT ( 'NONE',  ( 78.03658003843786162, 205.8615022471901739, 5.000000000000051514 ) ) ;
#42262 = CARTESIAN_POINT ( 'NONE',  ( 164.9335952247126045, 244.9736285262353306, -1.661461410667423255 ) ) ;
#42263 = EDGE_CURVE ( 'NONE', #18147, #88849, #44446, .T. ) ;
#42264 = ORIENTED_EDGE ( 'NONE', *, *, #31981, .F. ) ;
#42265 = VECTOR ( 'NONE', #29253, 999.9999999999998863 ) ;
#42266 = CARTESIAN_POINT ( 'NONE',  ( 6.228640307978117185, 167.7365022471902023, 10.00000000000009592 ) ) ;
#42267 = DIRECTION ( 'NONE',  ( -0.5000000000000001110, 0.8660254037844384856, 0.000000000000000000 ) ) ;
#42268 = CARTESIAN_POINT ( 'NONE',  ( 122.5830220656496579, 232.3923013555409796, 4.594050593750050204 ) ) ;
#42269 = CARTESIAN_POINT ( 'NONE',  ( 23.51121325743158508, 19.28920272979927120, -7.433330006724141015 ) ) ;
#42270 = CARTESIAN_POINT ( 'NONE',  ( 74.84209865657220462, 67.13651163270155564, 12.97079428878455509 ) ) ;
#42271 = CARTESIAN_POINT ( 'NONE',  ( 46.28462696178780789, 185.9824982072973967, 3.021315404115420679E-15 ) ) ;
#42273 = FACE_OUTER_BOUND ( 'NONE', #61271, .T. ) ;
#42272 = CARTESIAN_POINT ( 'NONE',  ( 182.8798658535135928, 295.3622947365996083, -6.914253198550406765 ) ) ;
#42274 = CARTESIAN_POINT ( 'NONE',  ( 22.44855073024449155, 13.36477965099640208, 1.583844403245364907 ) ) ;
#42275 = ORIENTED_EDGE ( 'NONE', *, *, #78363, .F. ) ;
#42276 = CARTESIAN_POINT ( 'NONE',  ( 191.5281967176683509, 298.9104275333885994, 7.715154960566919407 ) ) ;
#42277 = CARTESIAN_POINT ( 'NONE',  ( 196.9431415128477170, 289.5314680279574304, -16.61413060656005669 ) ) ;
#42278 = CARTESIAN_POINT ( 'NONE',  ( 180.6665526851674599, 287.6815954905284798, 14.11204521094005671 ) ) ;
#42279 = CARTESIAN_POINT ( 'NONE',  ( 176.3588661899402439, 292.5224010984320557, -1.117630640333412639 ) ) ;
#42280 = CARTESIAN_POINT ( 'NONE',  ( 81.62968001876643598, 55.78593752935011452, -16.36028778889455282 ) ) ;
#42281 = ORIENTED_EDGE ( 'NONE', *, *, #58382, .F. ) ;
#42282 = CARTESIAN_POINT ( 'NONE',  ( 189.2748339612899144, 265.2827144222970333, 12.02701514401042360 ) ) ;
#42283 = CARTESIAN_POINT ( 'NONE',  ( 168.3417633411148984, 271.6681995330380346, -17.37814367259023740 ) ) ;
#42284 = EDGE_CURVE ( 'NONE', #62590, #26159, #36563, .T. ) ;
#42285 = EDGE_CURVE ( 'NONE', #56545, #66866, #97597, .T. ) ;
#42286 = CARTESIAN_POINT ( 'NONE',  ( 71.69055946895421982, 72.48590965862314306, 0.9596580914388839201 ) ) ;
#42287 = CARTESIAN_POINT ( 'NONE',  ( 71.64316818921393804, 72.05741665177616539, -3.509880912999890690 ) ) ;
#42288 = CARTESIAN_POINT ( 'NONE',  ( 196.2991918319561364, 270.8780335082191755, 12.03491514832104592 ) ) ;
#42289 = CARTESIAN_POINT ( 'NONE',  ( 185.6543263943590603, 297.1164544966914605, 5.613520220585219711 ) ) ;
#42290 = CARTESIAN_POINT ( 'NONE',  ( 71.14876058709654671, 71.77059820202033791, -0.7402833220517009982 ) ) ;
#42291 = CARTESIAN_POINT ( 'NONE',  ( 148.1700451075146532, 274.5003607289000342, 6.655253088558737318 ) ) ;
#42292 = ADVANCED_FACE ( 'NONE', ( #51790 ), #75095, .T. ) ;
#42293 = CYLINDRICAL_SURFACE ( 'NONE', #58398, 10.00000000000010658 ) ;
#42294 = CARTESIAN_POINT ( 'NONE',  ( 13.85453579343919905, 10.12755873383624206, -6.180339887498949025 ) ) ;
#42295 = CARTESIAN_POINT ( 'NONE',  ( 173.7786751825973681, 272.6665995263483637, -16.36869263761786897 ) ) ;
#42296 = ORIENTED_EDGE ( 'NONE', *, *, #37813, .F. ) ;
#42297 = DIRECTION ( 'NONE',  ( 0.000000000000000000, -1.000000000000000000, 0.000000000000000000 ) ) ;
#42298 = CARTESIAN_POINT ( 'NONE',  ( 38.08139550823666042, 22.39040679176985904, -6.890680421881970419E-14 ) ) ;
#42299 = CARTESIAN_POINT ( 'NONE',  ( 156.1849287808383338, 261.6246031306073974, -17.08462936727468673 ) ) ;
#42300 = EDGE_LOOP ( 'NONE', ( #52274, #44239, #44456, #44586 ) ) ;
#42302 = EDGE_CURVE ( 'NONE', #1644, #15777, #57377, .T. ) ;
#42301 = CARTESIAN_POINT ( 'NONE',  ( 79.06565384122613693, 60.08000270057965508, 16.12336209646970886 ) ) ;
#42303 = CARTESIAN_POINT ( 'NONE',  ( 185.5025673201750749, 291.0580338203257611, 12.15717963013472769 ) ) ;
#42304 = DIRECTION ( 'NONE',  ( -0.5634352399127592337, -0.8261602328994366307, 0.000000000000000000 ) ) ;
#42305 = ORIENTED_EDGE ( 'NONE', *, *, #57869, .T. ) ;
#42306 = DIRECTION ( 'NONE',  ( 0.5000000000000002220, -0.8660254037844384856, 0.000000000000000000 ) ) ;
#42307 = CARTESIAN_POINT ( 'NONE',  ( 73.47631802762754205, 69.90797475050369769, -9.735925655486411756 ) ) ;
#42308 = CARTESIAN_POINT ( 'NONE',  ( 84.60292230380740364, 49.80262622141071915, -13.18993139652274671 ) ) ;
#42309 = CARTESIAN_POINT ( 'NONE',  ( 185.0126953839742896, 259.9172543619729936, -5.831654218434374926 ) ) ;
#42310 = EDGE_CURVE ( 'NONE', #67514, #83087, #9950, .T. ) ;
#42311 = VERTEX_POINT ( 'NONE', #14767 ) ;
#42312 = ADVANCED_FACE ( 'NONE', ( #61357 ), #44651, .T. ) ;
#42313 = ORIENTED_EDGE ( 'NONE', *, *, #34981, .T. ) ;
#42314 = CARTESIAN_POINT ( 'NONE',  ( 178.1963635607110916, 260.9795737440591097, 12.20855421423478404 ) ) ;
#42315 = ORIENTED_EDGE ( 'NONE', *, *, #16462, .F. ) ;
#42316 = LINE ( 'NONE', #27647, #91932 ) ;
#42317 = EDGE_LOOP ( 'NONE', ( #11494, #42956, #87157, #88247, #69342 ) ) ;
#42318 = DIRECTION ( 'NONE',  ( 0.1577859398657057433, -0.9874733399847793747, 0.000000000000000000 ) ) ;
#42319 = CARTESIAN_POINT ( 'NONE',  ( 155.4661767250933622, 261.3716783840932294, -17.10192542004562810 ) ) ;
#42320 = VERTEX_POINT ( 'NONE', #45163 ) ;
#42321 = CARTESIAN_POINT ( 'NONE',  ( 182.8342258324622378, 279.9465444586228386, -16.27734326228908301 ) ) ;
#42322 = CARTESIAN_POINT ( 'NONE',  ( 81.96055694566001648, 41.06594365097284793, 3.414074282795390936 ) ) ;
#42323 = CARTESIAN_POINT ( 'NONE',  ( 80.61273461444635302, 43.38457209157425609, -9.435640752088607641 ) ) ;
#42324 = CARTESIAN_POINT ( 'NONE',  ( 160.5053574735698021, 276.1538589699120507, -12.57604534192124746 ) ) ;
#42325 = CARTESIAN_POINT ( 'NONE',  ( 192.8011239859581849, 296.7056528303708660, -11.79847971295421694 ) ) ;
#42326 = CARTESIAN_POINT ( 'NONE',  ( 200.6737073311291795, 283.0699384897140476, -17.61533935526990291 ) ) ;
#42327 = FACE_OUTER_BOUND ( 'NONE', #16259, .T. ) ;
#42328 = CARTESIAN_POINT ( 'NONE',  ( 0.07393976959879319799, 182.3967562850347406, 2.649461200531984646E-14 ) ) ;
#42329 = CARTESIAN_POINT ( 'NONE',  ( 140.9585647324944659, 258.3149278399160380, 9.188101187500093303 ) ) ;
#42330 = VERTEX_POINT ( 'NONE', #99387 ) ;
#42331 = DIRECTION ( 'NONE',  ( -0.000000000000000000, -0.000000000000000000, -1.000000000000000000 ) ) ;
#42332 = CARTESIAN_POINT ( 'NONE',  ( 9.553764119070452310, 20.91421378149917132, 9.188101187500008038 ) ) ;
#42333 = ORIENTED_EDGE ( 'NONE', *, *, #84274, .F. ) ;
#42335 = EDGE_LOOP ( 'NONE', ( #39273, #3810, #81242, #39954 ) ) ;
#42334 = CARTESIAN_POINT ( 'NONE',  ( 204.0750558719120988, 271.6231733279527703, 9.785492889829541241 ) ) ;
#42336 = LINE ( 'NONE', #10971, #30342 ) ;
#42337 = CARTESIAN_POINT ( 'NONE',  ( 122.4023397829301700, 248.1427522451419065, -10.00000000000009592 ) ) ;
#42338 = CARTESIAN_POINT ( 'NONE',  ( 153.3256299635001483, 276.8936154282524171, 7.080213329903488173 ) ) ;
#42339 = CARTESIAN_POINT ( 'NONE',  ( 70.44287837739904035, 60.93660230331288830, 14.43604447541618008 ) ) ;
#42340 = CARTESIAN_POINT ( 'NONE',  ( 171.6775608579050925, 280.0339643969739427, 13.87834783768247071 ) ) ;
#42341 = AXIS2_PLACEMENT_3D ( 'NONE', #94779, #72474, #63841 ) ;
#42342 = CARTESIAN_POINT ( 'NONE',  ( -19.65312891409030271, 93.06504152958497400, 10.00000000000000888 ) ) ;
#42343 = CARTESIAN_POINT ( 'NONE',  ( 88.23959751488011705, 43.87687695675944610, -2.120018653157903721 ) ) ;
#42344 = ORIENTED_EDGE ( 'NONE', *, *, #2059, .F. ) ;
#42345 = DIRECTION ( 'NONE',  ( -1.000000000000000000, 0.000000000000000000, 0.000000000000000000 ) ) ;
#42346 = CARTESIAN_POINT ( 'NONE',  ( 65.79394124285487067, 69.11298328710827832, 0.1263844587676525022 ) ) ;
#42347 = ORIENTED_EDGE ( 'NONE', *, *, #63578, .F. ) ;
#42348 = DIRECTION ( 'NONE',  ( -0.5242119900219359696, 0.000000000000000000, 0.8515878049368965641 ) ) ;
#42349 = CARTESIAN_POINT ( 'NONE',  ( 200.9372752118609640, 267.7768021933786144, -2.766562499730290448 ) ) ;
#42350 = DIRECTION ( 'NONE',  ( -0.9413434404457865501, 0.3374500364938337049, 0.000000000000000000 ) ) ;
#42351 = CARTESIAN_POINT ( 'NONE',  ( -31.59160691316810343, 24.09060609829247213, 177.5919119679930134 ) ) ;
#42352 = CARTESIAN_POINT ( 'NONE',  ( 203.0398866899141126, 278.9715956204779559, 16.57839218037009132 ) ) ;
#42354 = CARTESIAN_POINT ( 'NONE',  ( 87.92119597943950282, 44.20992230385985522, 2.809437090033895856 ) ) ;
#42353 = CARTESIAN_POINT ( 'NONE',  ( 170.3620333804029485, 268.1781345414723319, 17.80501103880222402 ) ) ;
#42355 = ADVANCED_FACE ( 'NONE', ( #21868 ), #98893, .F. ) ;
#42356 = CARTESIAN_POINT ( 'NONE',  ( 62.71875570545262946, 207.0177522451418497, -10.00000000000009592 ) ) ;
#42357 = ORIENTED_EDGE ( 'NONE', *, *, #96381, .F. ) ;
#42358 = B_SPLINE_CURVE_WITH_KNOTS ( 'NONE', 3,
 ( #21679, #30267, #62145, #31258, #30776, #85521, #60150, #38351, #46445, #23153, #77886, #93091, #92606, #37851, #38856, #77378, #6968, #76391, #84021, #68759, #69762, #44962, #7980, #865, #23648, #91113, #37359, #61157, #53066, #45945, #54044, #52558, #99684, #60645, #370, #75901, #16065, #54538, #22172, #92126, #83514, #76862, #85002, #6481, #22679, #68264 ),
 .UNSPECIFIED., .F., .F.,
 ( 4, 2, 2, 2, 2, 2, 2, 2, 2, 2, 2, 2, 2, 2, 2, 2, 2, 2, 2, 2, 2, 2, 4 ),
 ( 0.001386463054751980182, 0.001851836421151829490, 0.002317209787551679015, 0.002549896470751603778, 0.002666239812351530163, 0.002782583153951456983, 0.002898926495551383802, 0.003015269837151310188, 0.003247956520351133903, 0.003713329886750830339, 0.004178703253150526341, 0.005109449985949853293, 0.006040196718749181112, 0.006505570085148845889, 0.006970943451548509799, 0.007087286793148386312, 0.007145458463948324568, 0.007203630134748261957, 0.007319973476348140204, 0.007436316817948018451, 0.007901690184347711851, 0.008367063550747406986, 0.008832436917147098651 ),
 .UNSPECIFIED. ) ;
#42359 = CARTESIAN_POINT ( 'NONE',  ( 75.68423863107267380, 61.28764373785409703, -15.43813584130047367 ) ) ;
#42360 = EDGE_CURVE ( 'NONE', #71854, #7443, #52879, .T. ) ;
#42361 = CARTESIAN_POINT ( 'NONE',  ( 194.3094773688834778, 284.8302703302293253, 17.74979085435418469 ) ) ;
#42362 = CARTESIAN_POINT ( 'NONE',  ( -22.42236680055709641, 157.8615022471902591, 0.000000000000000000 ) ) ;
#42363 = CARTESIAN_POINT ( 'NONE',  ( 80.90469142059797036, 42.95404229843371979, -9.526595558722311452 ) ) ;
#42364 = DIRECTION ( 'NONE',  ( 0.8660254037844395958, 0.4999999999999985567, 0.000000000000000000 ) ) ;
#42365 = CARTESIAN_POINT ( 'NONE',  ( 5.317335864756744357, 180.0024278399160949, -9.188101187500093303 ) ) ;
#42366 = CARTESIAN_POINT ( 'NONE',  ( 111.1892885731694065, 228.8768266524159856, -9.188101187500091527 ) ) ;
#42367 = CARTESIAN_POINT ( 'NONE',  ( 202.7754741559590173, 279.4295715634463022, -15.65855077192107636 ) ) ;
#42368 = CARTESIAN_POINT ( 'NONE',  ( 87.98904372666932261, 44.25610683789894750, -4.385737539232402504 ) ) ;
#42369 = CARTESIAN_POINT ( 'NONE',  ( 186.3053879374282928, 296.7155014134779663, -7.306349104823136820 ) ) ;
#42370 = EDGE_CURVE ( 'NONE', #6973, #17025, #55776, .T. ) ;
#42371 = DIRECTION ( 'NONE',  ( -0.1344185706417024839, 0.9909246428798921258, 0.000000000000000000 ) ) ;
#42372 = VECTOR ( 'NONE', #18774, 1000.000000000000114 ) ;
#42373 = CARTESIAN_POINT ( 'NONE',  ( 49.04287251715432205, 95.72274150194785136, 10.00000000000000000 ) ) ;
#42374 = FACE_OUTER_BOUND ( 'NONE', #89028, .T. ) ;
#42375 = CARTESIAN_POINT ( 'NONE',  ( 194.3011251241114508, 294.1075746476782342, -14.76047579547631905 ) ) ;
#42376 = CARTESIAN_POINT ( 'NONE',  ( 181.7502977777323281, 291.5405758491393726, 9.349876991887354549 ) ) ;
#42377 = EDGE_CURVE ( 'NONE', #47356, #97296, #79491, .T. ) ;
#42378 = CARTESIAN_POINT ( 'NONE',  ( -48.02262176224491697, 41.70345557631966926, 59.99999999999999289 ) ) ;
#42379 = CARTESIAN_POINT ( 'NONE',  ( 164.5782759443297039, 245.5890595727670984, -5.697842221573455213 ) ) ;
#42380 = CARTESIAN_POINT ( 'NONE',  ( 74.28057495708935676, 56.36868286471138845, -16.09213986559992549 ) ) ;
#42381 = DIRECTION ( 'NONE',  ( 0.8660254037844395958, 0.4999999999999985567, 0.000000000000000000 ) ) ;
#42382 = EDGE_CURVE ( 'NONE', #88881, #71264, #13772, .T. ) ;
#42383 = CARTESIAN_POINT ( 'NONE',  ( 90.45192255479418009, 211.4824982072973683, 3.021315404115420679E-15 ) ) ;
#42384 = CIRCLE ( 'NONE', #86149, 12.50000000000000000 ) ;
#42385 = CARTESIAN_POINT ( 'NONE',  ( -19.65312891409030271, 93.06504152958497400, 177.5919119679930134 ) ) ;
#42386 = CARTESIAN_POINT ( 'NONE',  ( 84.39645409570583467, 219.5333772461660544, 9.188101187500095079 ) ) ;
#42387 = CARTESIAN_POINT ( 'NONE',  ( 161.4816992964961742, 250.9524876563463067, -12.92750327687364198 ) ) ;
#42388 = CARTESIAN_POINT ( 'NONE',  ( 163.4945121521897988, 257.9090426894093184, 15.56564318970484884 ) ) ;
#42390 = DIRECTION ( 'NONE',  ( -0.5000000000000013323, 0.8660254037844378194, 0.000000000000000000 ) ) ;
#42389 = CARTESIAN_POINT ( 'NONE',  ( 157.8763546842245376, 257.1971277035954699, 17.68444922773363004 ) ) ;
#42391 = CARTESIAN_POINT ( 'NONE',  ( 151.0013883899287066, 269.1049186256390726, -14.25461351222133466 ) ) ;
#42392 = CARTESIAN_POINT ( 'NONE',  ( 175.9975959079605161, 269.8183398160408046, -16.55671884903257407 ) ) ;
#42393 = CARTESIAN_POINT ( 'NONE',  ( 35.55378427144160014, 29.03085787977765264, 9.188101187500006262 ) ) ;
#42394 = DIRECTION ( 'NONE',  ( 1.000000000000000000, -0.000000000000000000, -1.082076799516502080E-16 ) ) ;
#42395 = CARTESIAN_POINT ( 'NONE',  ( 127.2636487221268311, 255.8297689869269504, -2.679491924311252493 ) ) ;
#42396 = VERTEX_POINT ( 'NONE', #37068 ) ;
#42397 = CARTESIAN_POINT ( 'NONE',  ( 20.11807774711229868, 23.56628583063840665, 9.188101187500006262 ) ) ;
#42398 = CARTESIAN_POINT ( 'NONE',  ( 77.03558525930309031, 203.0327760586659451, 1.948934522072302763E-15 ) ) ;
#42399 = CARTESIAN_POINT ( 'NONE',  ( 173.0455529495148141, 289.6430652088176885, -1.041919219315089906 ) ) ;
#42400 = DIRECTION ( 'NONE',  ( 0.02225111142181396273, 0.9997524133706774396, 0.000000000000000000 ) ) ;
#42401 = CARTESIAN_POINT ( 'NONE',  ( 35.14194503788360890, 114.0493334331461455, 59.99999999999999289 ) ) ;
#42402 = CARTESIAN_POINT ( 'NONE',  ( 86.72009611066519597, 47.05274629621921889, 10.38319007345879541 ) ) ;
#42403 = CARTESIAN_POINT ( 'NONE',  ( 190.1859351024625369, 286.6565765330755085, 16.32613358219952104 ) ) ;
#42404 = LINE ( 'NONE', #65710, #19410 ) ;
#42405 = CARTESIAN_POINT ( 'NONE',  ( 118.6676052326576922, 245.9865022471903444, -10.00000000000009415 ) ) ;
#42406 = FACE_OUTER_BOUND ( 'NONE', #55427, .T. ) ;
#42407 = EDGE_CURVE ( 'NONE', #8402, #20413, #68615, .T. ) ;
#42408 = CARTESIAN_POINT ( 'NONE',  ( 75.17844314609712342, 53.08451609724016151, 16.49030186085838778 ) ) ;
#42409 = ORIENTED_EDGE ( 'NONE', *, *, #95225, .T. ) ;
#42410 = CARTESIAN_POINT ( 'NONE',  ( 165.6072792903335937, 246.7937695405969976, -1.477711117505905225 ) ) ;
#42411 = ORIENTED_EDGE ( 'NONE', *, *, #47834, .T. ) ;
#42412 = CARTESIAN_POINT ( 'NONE',  ( 202.5245888501533216, 279.8641176599742266, 15.60152447840272494 ) ) ;
#42413 = CARTESIAN_POINT ( 'NONE',  ( 207.2032113364036547, 269.9913168956704794, -0.07087847770824695637 ) ) ;
#42414 = ORIENTED_EDGE ( 'NONE', *, *, #5153, .T. ) ;
#42415 = CARTESIAN_POINT ( 'NONE',  ( 74.56414817410228579, 187.8759306620403322, -17.47570218321536473 ) ) ;
#42416 = EDGE_LOOP ( 'NONE', ( #86111, #62464, #54267, #37296 ) ) ;
#42418 = ADVANCED_FACE ( 'NONE', ( #14909 ), #81349, .F. ) ;
#42417 = CARTESIAN_POINT ( 'NONE',  ( 188.8306723507383538, 290.8947323270112975, 14.73421016979825282 ) ) ;
#42419 = CARTESIAN_POINT ( 'NONE',  ( 205.8346909429602363, 274.1308526569923742, 12.31208841938360976 ) ) ;
#42420 = CARTESIAN_POINT ( 'NONE',  ( 78.92295937046175425, 204.8262482093457777, 3.021315404115420679E-15 ) ) ;
#42421 = CARTESIAN_POINT ( 'NONE',  ( 154.0923235371355986, 263.7512619077765521, -17.59436137934181232 ) ) ;
#42422 = CARTESIAN_POINT ( 'NONE',  ( -19.65312891409030271, 93.06504152958497400, -10.00000000000000888 ) ) ;
#42423 = EDGE_CURVE ( 'NONE', #28265, #67548, #33518, .T. ) ;
#42424 = CARTESIAN_POINT ( 'NONE',  ( 38.36533659613348846, 24.01110640527295104, 2.839279412974134775 ) ) ;
#42425 = CARTESIAN_POINT ( 'NONE',  ( 70.98683038387876820, 61.11472152276905234, -14.49225651734632692 ) ) ;
#42426 = CARTESIAN_POINT ( 'NONE',  ( -22.42236680055709641, 157.8615022471902591, 0.000000000000000000 ) ) ;
#42427 = CARTESIAN_POINT ( 'NONE',  ( 173.8469137325424185, 256.4471593116459189, -12.44389045026504270 ) ) ;
#42428 = ORIENTED_EDGE ( 'NONE', *, *, #87623, .F. ) ;
#42429 = ORIENTED_EDGE ( 'NONE', *, *, #95893, .F. ) ;
#42430 = CARTESIAN_POINT ( 'NONE',  ( 196.1252721995043942, 284.4712197134549001, -17.81715240067734030 ) ) ;
#42432 = CARTESIAN_POINT ( 'NONE',  ( 147.6884207308302450, 274.8431469350302336, -8.096293592099874203 ) ) ;
#42431 = CARTESIAN_POINT ( 'NONE',  ( 204.2129321040862919, 276.9398213635460024, 14.41515352680879758 ) ) ;
#42433 = CARTESIAN_POINT ( 'NONE',  ( 85.94797495143531307, 48.32083425265168586, 12.00338787116683470 ) ) ;
#42434 = CARTESIAN_POINT ( 'NONE',  ( 193.9844289374573520, 294.6561085335266625, 15.49818881749970245 ) ) ;
#42435 = CARTESIAN_POINT ( 'NONE',  ( 120.7221038307704788, 252.0530062829862743, -4.648177544792955347E-16 ) ) ;
#42436 = CARTESIAN_POINT ( 'NONE',  ( 157.8043799545718286, 257.3217915922150496, -17.97575562758749257 ) ) ;
#42437 = CARTESIAN_POINT ( 'NONE',  ( 164.1144691085127647, 246.3923965773001328, 5.648579756269943353 ) ) ;
#42438 = CARTESIAN_POINT ( 'NONE',  ( 166.3040822299595050, 265.4869683937334912, 16.55097390736193219 ) ) ;
#42439 = CARTESIAN_POINT ( 'NONE',  ( 179.3484401907847996, 256.1569968345440884, 4.890721239772626738 ) ) ;
#42440 = CARTESIAN_POINT ( 'NONE',  ( 91.10780387927019319, 235.6589784336661353, -6.496448406907675876E-16 ) ) ;
#42441 = ORIENTED_EDGE ( 'NONE', *, *, #10851, .F. ) ;
#42442 = DIRECTION ( 'NONE',  ( 0.1887253692075823441, -0.9820299053580097137, 0.000000000000000000 ) ) ;
#42443 = CARTESIAN_POINT ( 'NONE',  ( -19.65312891409030271, 93.06504152958497400, 10.00000000000000888 ) ) ;
#42444 = CARTESIAN_POINT ( 'NONE',  ( 166.8095580818603025, 278.3619912271652765, -13.27947376363879251 ) ) ;
#42445 = ORIENTED_EDGE ( 'NONE', *, *, #64757, .F. ) ;
#42446 = AXIS2_PLACEMENT_3D ( 'NONE', #81222, #66470, #27492 ) ;
#42447 = ORIENTED_EDGE ( 'NONE', *, *, #52233, .T. ) ;
#42448 = CARTESIAN_POINT ( 'NONE',  ( 87.23257741107988750, 46.04474800944700519, -8.789869334516776433 ) ) ;
#42450 = B_SPLINE_SURFACE_WITH_KNOTS ( 'NONE', 3, 1, ( 
 ( #72503, #8308 ),
 ( #39172, #95828 ),
 ( #64374, #18289 ),
 ( #92443, #46276 ),
 ( #39669, #70595 ),
 ( #49183, #61493 ),
 ( #76704, #70089 ),
 ( #69095, #7807 ),
 ( #38693, #22989 ),
 ( #1207, #7298 ),
 ( #53879, #699 ),
 ( #84840, #31582 ),
 ( #95336, #62475 ),
 ( #23994, #25894 ),
 ( #10681, #3109 ),
 ( #33997, #53397 ),
 ( #84347, #14893 ),
 ( #26878, #51673 ),
 ( #59233, #18785 ),
 ( #19786, #13185 ),
 ( #27866, #73982 ),
 ( #66367, #65856 ),
 ( #67355, #96817 ),
 ( #81607, #90209 ),
 ( #82117, #42549 ),
 ( #34469, #81122 ),
 ( #96310, #58745 ),
 ( #4566, #58259 ),
 ( #57259, #43038 ),
 ( #97786, #80621 ),
 ( #50655, #88733 ),
 ( #26381, #20279 ),
 ( #89718, #34956 ),
 ( #19303, #35462 ) ),
 .UNSPECIFIED., .T., .F., .F.,
 ( 4, 2, 2, 2, 2, 2, 2, 2, 2, 2, 2, 2, 2, 2, 2, 2, 4 ),
 ( 2, 2 ),
 ( 0.000000000000000000, 0.06250000000000000000, 0.1250000000000000000, 0.1875000000000000000, 0.2500000000000000000, 0.3125000000000000000, 0.3750000000000000000, 0.4375000000000000000, 0.5000000000000000000, 0.5625000000000000000, 0.6250000000000000000, 0.6875000000000000000, 0.7500000000000000000, 0.8125000000000000000, 0.8750000000000000000, 0.9375000000000000000, 1.000000000000000000 ),
 ( 0.000000000000000000, 1.000000000000000000 ),
 .UNSPECIFIED. ) ;
#42449 = CARTESIAN_POINT ( 'NONE',  ( 196.0760950258556363, 286.0837363073127904, -17.73048769406821279 ) ) ;
#42451 = DIRECTION ( 'NONE',  ( -0.000000000000000000, -0.000000000000000000, -1.000000000000000000 ) ) ;
#42452 = CARTESIAN_POINT ( 'NONE',  ( 7.026152882275393807, 27.55466486950697913, -1.111400068045478839E-16 ) ) ;
#42453 = CARTESIAN_POINT ( 'NONE',  ( 208.2726345668874615, 269.9082104343620472, 2.818736869262927769 ) ) ;
#42454 = CARTESIAN_POINT ( 'NONE',  ( 94.03063961704269502, 237.3464784336661637, 1.353441290958777327E-15 ) ) ;
#42455 = ORIENTED_EDGE ( 'NONE', *, *, #5206, .F. ) ;
#42456 = VERTEX_POINT ( 'NONE', #43921 ) ;
#42457 = CARTESIAN_POINT ( 'NONE',  ( 162.6425574510925003, 248.9418223522047526, -10.70838742014210077 ) ) ;
#42458 = EDGE_LOOP ( 'NONE', ( #98328, #55037, #57161, #76696, #69368, #10845 ) ) ;
#42459 = EDGE_CURVE ( 'NONE', #99984, #72868, #38337, .T. ) ;
#42460 = VECTOR ( 'NONE', #81163, 1000.000000000000227 ) ;
#42461 = CARTESIAN_POINT ( 'NONE',  ( 170.4855375986076638, 248.6613294790634541, -0.2716024841417116753 ) ) ;
#42462 = CARTESIAN_POINT ( 'NONE',  ( 41.71240375114938814, 62.05720181600818108, -10.00000000000000000 ) ) ;
#42463 = CARTESIAN_POINT ( 'NONE',  ( 165.5562080735016082, 285.3469202611815376, 0.5477150056637907216 ) ) ;
#42465 = CARTESIAN_POINT ( 'NONE',  ( 69.59544983168204624, 63.11080376311066686, -13.61608123681405758 ) ) ;
#42464 = CARTESIAN_POINT ( 'NONE',  ( 124.8827946268633298, 255.1589784336661069, -6.496448406907675876E-16 ) ) ;
#42466 = CARTESIAN_POINT ( 'NONE',  ( -12.69762320744227502, 170.1427522451419350, -10.00000000000009415 ) ) ;
#42467 = DIRECTION ( 'NONE',  ( -0.8660254037844369313, -0.5000000000000029976, 0.000000000000000000 ) ) ;
#42468 = VERTEX_POINT ( 'NONE', #74372 ) ;
#42469 = CARTESIAN_POINT ( 'NONE',  ( 156.9781162866021589, 258.7529222455866034, 16.87007551417546480 ) ) ;
#42470 = CARTESIAN_POINT ( 'NONE',  ( 81.48768738999534378, 47.92560860843236981, 13.01067380738259160 ) ) ;
#42471 = CARTESIAN_POINT ( 'NONE',  ( 81.95337945677349012, 41.00406898985013271, -3.180093734862122545 ) ) ;
#42472 = CARTESIAN_POINT ( 'NONE',  ( 188.8600501376575096, 269.6449448202791359, 14.64833052561093396 ) ) ;
#42473 = LINE ( 'NONE', #59669, #18863 ) ;
#42474 =( BOUNDED_CURVE ( )  B_SPLINE_CURVE ( 2, ( #47276, #94423, #39655, #38676, #188, #1705, #78199, #70577, #16879 ),
 .UNSPECIFIED., .F., .T. ) 
 B_SPLINE_CURVE_WITH_KNOTS ( ( 3, 2, 2, 2, 3 ),
 ( 0.6088709677419354982, 0.6102150537634408733, 0.6129032258064516236, 0.6155913978494623739, 0.6169354838709677491 ),
 .UNSPECIFIED. ) 
 CURVE ( )  GEOMETRIC_REPRESENTATION_ITEM ( )  RATIONAL_B_SPLINE_CURVE ( ( 0.9330127018922194093, 0.9330127018922194093, 1.000000000000000000, 0.8660254037844387076, 1.000000000000000000, 0.8660254037844387076, 1.000000000000000000, 0.9330127018922194093, 0.9330127018922194093 ) ) 
 REPRESENTATION_ITEM ( '' )  );
#42475 = DIRECTION ( 'NONE',  ( -0.8660254037844384856, -0.5000000000000004441, 0.000000000000000000 ) ) ;
#42476 = DIRECTION ( 'NONE',  ( -0.06442261589617466477, -0.9979227057047523886, 0.000000000000000000 ) ) ;
#42477 = DIRECTION ( 'NONE',  ( 0.000000000000000000, 0.000000000000000000, -1.000000000000000000 ) ) ;
#42478 =( BOUNDED_CURVE ( )  B_SPLINE_CURVE ( 2, ( #12147, #89689, #10652, #97269, #72970, #73453, #64849, #11166, #50138 ),
 .UNSPECIFIED., .F., .T. ) 
 B_SPLINE_CURVE_WITH_KNOTS ( ( 3, 2, 2, 2, 3 ),
 ( 0.1653225806451612823, 0.1666666666666666574, 0.1693548387096774077, 0.1720430107526881858, 0.1733870967741935609 ),
 .UNSPECIFIED. ) 
 CURVE ( )  GEOMETRIC_REPRESENTATION_ITEM ( )  RATIONAL_B_SPLINE_CURVE ( ( 0.9330127018922194093, 0.9330127018922194093, 1.000000000000000000, 0.8660254037844387076, 1.000000000000000000, 0.8660254037844387076, 1.000000000000000000, 0.9330127018922194093, 0.9330127018922194093 ) ) 
 REPRESENTATION_ITEM ( '' )  );
#42479 = CARTESIAN_POINT ( 'NONE',  ( 80.86831763631852255, 54.93583156370407039, 15.92778375911414024 ) ) ;
#42480 = CARTESIAN_POINT ( 'NONE',  ( 66.46320885748656337, 68.94986384069261476, 0.01364106734875079018 ) ) ;
#42481 = CARTESIAN_POINT ( 'NONE',  ( 23.90043047733868420, 15.92755873383626408, 6.180339887498953466 ) ) ;
#42482 = CARTESIAN_POINT ( 'NONE',  ( 78.34913526621272695, 61.55915279984171917, 16.16953766326405528 ) ) ;
#42483 = CARTESIAN_POINT ( 'NONE',  ( 178.2245750143592602, 292.8343567999519337, -5.806686789501219970 ) ) ;
#42484 = CARTESIAN_POINT ( 'NONE',  ( 89.81297465553679160, 45.16368336106900472, 0.1873032967079516220 ) ) ;
#42485 = ADVANCED_FACE ( 'NONE', ( #60108 ), #36013, .F. ) ;
#42486 = CARTESIAN_POINT ( 'NONE',  ( 70.50619853993235608, 64.86658464427489434, -12.22208435811523763 ) ) ;
#42487 = CARTESIAN_POINT ( 'NONE',  ( 185.2191211618261661, 266.4373919749868378, 13.17776240725820358 ) ) ;
#42488 = CARTESIAN_POINT ( 'NONE',  ( -13.11024591527723437, 27.99999999999999645, -25.00000000000017053 ) ) ;
#42489 = ADVANCED_FACE ( 'NONE', ( #62098 ), #31212, .F. ) ;
#42490 = CARTESIAN_POINT ( 'NONE',  ( 30.13164393277487818, 36.13478043621390157, 8.090169943749478065 ) ) ;
#42491 = CARTESIAN_POINT ( 'NONE',  ( 192.2185419806677942, 297.7147144631093170, 12.45868041609393728 ) ) ;
#42492 = FILL_AREA_STYLE_COLOUR ( '', #83209 ) ;
#42493 = CARTESIAN_POINT ( 'NONE',  ( 71.77677790152782222, 58.69870002817014409, -15.46647683744001966 ) ) ;
#42494 = CARTESIAN_POINT ( 'NONE',  ( 83.43238562051314489, 43.24558130407336876, -6.915862364849616029 ) ) ;
#42495 = ADVANCED_FACE ( 'NONE', ( #85473 ), #16019, .T. ) ;
#42496 = CARTESIAN_POINT ( 'NONE',  ( 15.70964071017000663, 186.0024278399160949, -9.188101187500093303 ) ) ;
#42497 = DIRECTION ( 'NONE',  ( 1.000000000000000000, 0.000000000000000000, 0.000000000000000000 ) ) ;
#42498 = ORIENTED_EDGE ( 'NONE', *, *, #44925, .T. ) ;
#42499 = CARTESIAN_POINT ( 'NONE',  ( 87.13013406632065028, 46.22635825882438354, 8.450982903413489566 ) ) ;
#42500 = FACE_OUTER_BOUND ( 'NONE', #73869, .T. ) ;
#42501 = CARTESIAN_POINT ( 'NONE',  ( 207.7655736232174206, 270.7864657513322300, 3.530742899761726949 ) ) ;
#42502 = CARTESIAN_POINT ( 'NONE',  ( 81.75700027247154367, 41.62903602420404070, 5.464259697822261508 ) ) ;
#42503 = CARTESIAN_POINT ( 'NONE',  ( 37.03551627836181837, 198.3149278399161233, 9.188101187500093303 ) ) ;
#42504 = VECTOR ( 'NONE', #23197, 1000.000000000000000 ) ;
#42505 = CARTESIAN_POINT ( 'NONE',  ( 87.13039101863441260, 46.06611145402069241, 8.900391155234917306 ) ) ;
#42506 = CARTESIAN_POINT ( 'NONE',  ( 147.1249913145849177, 275.8190353104462815, 3.637773609013635223 ) ) ;
#42507 = CARTESIAN_POINT ( 'NONE',  ( 36.78445495848383473, 29.43677371833804202, -10.00000000000000355 ) ) ;
#42508 = CARTESIAN_POINT ( 'NONE',  ( 199.6009500900462115, 267.6840532653818059, -6.578795037453118333 ) ) ;
#42509 = CARTESIAN_POINT ( 'NONE',  ( 178.8777897842755920, 293.7479682644459444, 2.680126103812829896 ) ) ;
#42510 = CARTESIAN_POINT ( 'NONE',  ( 179.3350525740847274, 278.4300550830843690, -16.48020194126838334 ) ) ;
#42511 = CARTESIAN_POINT ( 'NONE',  ( 73.03896240731778278, 67.55704344529559080, -11.28667427251763655 ) ) ;
#42512 = CARTESIAN_POINT ( 'NONE',  ( 82.78345634833958400, 53.69061190982763776, 15.38144188222361386 ) ) ;
#42513 = CIRCLE ( 'NONE', #18251, 70.00000000000001421 ) ;
#42514 = CARTESIAN_POINT ( 'NONE',  ( 83.48272809759448876, 51.94771123612189001, 15.01134753452855009 ) ) ;
#42515 = B_SPLINE_CURVE_WITH_KNOTS ( 'NONE', 3,
 ( #14142, #75454, #44017, #45030 ),
 .UNSPECIFIED., .F., .F.,
 ( 4, 4 ),
 ( 0.01114144257808264912, 0.01698608932288061743 ),
 .UNSPECIFIED. ) ;
#42516 = CARTESIAN_POINT ( 'NONE',  ( 192.6198018426369458, 295.4256716423112152, -13.24907985865837468 ) ) ;
#42517 = CARTESIAN_POINT ( 'NONE',  ( 77.24272341830202038, 228.7365022471903444, 2.944929066748280225E-16 ) ) ;
#42518 = CARTESIAN_POINT ( 'NONE',  ( -6.281727404287059890, 25.63055774385195917, -10.00000000000000000 ) ) ;
#42519 = ADVANCED_FACE ( 'NONE', ( #6439 ), #60603, .T. ) ;
#42520 = DIRECTION ( 'NONE',  ( 0.2168075248790211351, 0.9762143704923794685, 0.000000000000000000 ) ) ;
#42521 = VERTEX_POINT ( 'NONE', #94062 ) ;
#42522 = CARTESIAN_POINT ( 'NONE',  ( 39.63359248971512017, 199.8149278399161233, 9.188101187500093303 ) ) ;
#42523 = ORIENTED_EDGE ( 'NONE', *, *, #88365, .F. ) ;
#42524 = CARTESIAN_POINT ( 'NONE',  ( 162.5372704899184839, 263.2211447608169692, 17.50793036557484683 ) ) ;
#42525 = CARTESIAN_POINT ( 'NONE',  ( 198.5201458116119397, 286.8000164587433005, -18.30276554821096013 ) ) ;
#42526 = CARTESIAN_POINT ( 'NONE',  ( 67.00635898293039361, 66.93325455025599524, -8.753795382997793695 ) ) ;
#42527 = ORIENTED_EDGE ( 'NONE', *, *, #51096, .T. ) ;
#42529 = CARTESIAN_POINT ( 'NONE',  ( 168.1331800941538006, 285.1077698243100258, 7.621536105887456003 ) ) ;
#42528 = VECTOR ( 'NONE', #33320, 1000.000000000000000 ) ;
#42530 = CARTESIAN_POINT ( 'NONE',  ( 207.5686001603237116, 271.1276337968068333, 7.659944433763431704 ) ) ;
#42531 = DIRECTION ( 'NONE',  ( 0.5000000000000001110, -0.8660254037844384856, -0.000000000000000000 ) ) ;
#42532 = CARTESIAN_POINT ( 'NONE',  ( 29.70508255828911004, 19.01110640527293327, 2.839279412974134775 ) ) ;
#42533 = CARTESIAN_POINT ( 'NONE',  ( 186.0925163355340999, 262.9831289636886140, 11.40996487886282651 ) ) ;
#42534 = CARTESIAN_POINT ( 'NONE',  ( -13.76211276271269668, 162.8615022471902591, -10.00000000000007816 ) ) ;
#42535 = CARTESIAN_POINT ( 'NONE',  ( 171.3620354993367130, 255.7207998885352538, 11.34474888520862201 ) ) ;
#42536 = VERTEX_POINT ( 'NONE', #47900 ) ;
#42537 = CARTESIAN_POINT ( 'NONE',  ( 18.12859834787737157, 11.26216523072493736, -2.296566073217252530E-15 ) ) ;
#42538 = CARTESIAN_POINT ( 'NONE',  ( 76.03006974497249360, 60.13132759335589128, 15.77593001480065737 ) ) ;
#42539 = CARTESIAN_POINT ( 'NONE',  ( 172.3741624485570867, 252.4865239976215037, 8.880853820034850798 ) ) ;
#42540 = FACE_OUTER_BOUND ( 'NONE', #73965, .T. ) ;
#42541 = EDGE_CURVE ( 'NONE', #10181, #27077, #37988, .T. ) ;
#42542 = ORIENTED_EDGE ( 'NONE', *, *, #76116, .T. ) ;
#42543 = CARTESIAN_POINT ( 'NONE',  ( 182.5039235484258882, 284.0050300796905276, 15.07559313791482403 ) ) ;
#42544 = CARTESIAN_POINT ( 'NONE',  ( 151.0099717111976076, 269.0900518771037468, 15.84752309685681659 ) ) ;
#42545 = DIRECTION ( 'NONE',  ( 0.4999999999999998890, -0.8660254037844385966, 0.000000000000000000 ) ) ;
#42546 = ORIENTED_EDGE ( 'NONE', *, *, #25860, .F. ) ;
#42548 = DIRECTION ( 'NONE',  ( -0.6623377501714527993, 0.7492053821868994712, 0.000000000000000000 ) ) ;
#42547 = CARTESIAN_POINT ( 'NONE',  ( 161.3145230519951951, 251.2420454056404822, -14.44869077440025151 ) ) ;
#42549 = CARTESIAN_POINT ( 'NONE',  ( 148.9285945872975390, 272.6951028054104427, -12.01265727652413240 ) ) ;
#42550 = EDGE_LOOP ( 'NONE', ( #81380, #2345, #20441, #10156 ) ) ;
#42551 = CARTESIAN_POINT ( 'NONE',  ( 66.26306969915694367, 68.66842913227013412, -2.141827346873069970 ) ) ;
#42552 = CARTESIAN_POINT ( 'NONE',  ( 159.5764336135613632, 254.2525046211064819, 15.32981087583629076 ) ) ;
#42553 = CARTESIAN_POINT ( 'NONE',  ( 72.91150845015395987, 57.63568554243673248, -16.31368332975456781 ) ) ;
#42554 = CARTESIAN_POINT ( 'NONE',  ( 78.35677645844283745, 61.14921145379764056, -15.90198519767692353 ) ) ;
#42555 = CARTESIAN_POINT ( 'NONE',  ( 205.2121761402296443, 275.2090799237855094, -14.05269615702442465 ) ) ;
#42556 = CARTESIAN_POINT ( 'NONE',  ( 114.1121243109418799, 230.5643266524159856, -9.188101187500093303 ) ) ;
#42557 = FACE_OUTER_BOUND ( 'NONE', #91494, .T. ) ;
#42558 = CARTESIAN_POINT ( 'NONE',  ( 69.03518170984699509, 64.49507618471645287, 12.45339560606362284 ) ) ;
#42559 = ORIENTED_EDGE ( 'NONE', *, *, #55165, .F. ) ;
#42560 = CARTESIAN_POINT ( 'NONE',  ( 164.0179800784044915, 246.5595204798204065, -5.772998092557310557 ) ) ;
#42561 = ORIENTED_EDGE ( 'NONE', *, *, #68211, .F. ) ;
#42562 = CARTESIAN_POINT ( 'NONE',  ( 31.98863997849372254, 36.65586893147758474, -7.433330006724137462 ) ) ;
#42563 = FACE_BOUND ( 'NONE', #37684, .T. ) ;
#42564 = CARTESIAN_POINT ( 'NONE',  ( 75.32821269442784740, 66.69330675534777697, -13.02113851420497603 ) ) ;
#42565 = CARTESIAN_POINT ( 'NONE',  ( 73.73334276372742124, 219.5024278399160949, 9.188101187500095079 ) ) ;
#42566 = ORIENTED_EDGE ( 'NONE', *, *, #96113, .T. ) ;
#42567 = CARTESIAN_POINT ( 'NONE',  ( 14.20097916528452942, 190.5530062829863311, -4.648177544792955347E-16 ) ) ;
#42568 = CARTESIAN_POINT ( 'NONE',  ( 155.9200296242932495, 280.3860598674420430, -5.539708607631867565 ) ) ;
#42569 = CARTESIAN_POINT ( 'NONE',  ( 150.9950855294679570, 269.1158355001903715, 14.12809338255366320 ) ) ;
#42570 = CARTESIAN_POINT ( 'NONE',  ( 171.9138461029266409, 276.7610644589011031, 16.36093085335564723 ) ) ;
#42571 = VERTEX_POINT ( 'NONE', #78337 ) ;
#42572 = EDGE_CURVE ( 'NONE', #52414, #85874, #63119, .T. ) ;
#42573 = CARTESIAN_POINT ( 'NONE',  ( 81.10561266023913163, 56.14635974680164310, -16.08662763877836355 ) ) ;
#42574 = CARTESIAN_POINT ( 'NONE',  ( 203.4357368910538355, 278.2859629599173559, -16.45855118664066197 ) ) ;
#42575 = VERTEX_POINT ( 'NONE', #73601 ) ;
#42576 = CARTESIAN_POINT ( 'NONE',  ( 195.5097554423081760, 292.0141655289934874, 16.05747864979548112 ) ) ;
#42577 = CARTESIAN_POINT ( 'NONE',  ( 70.82877176157455779, 69.82901014346172985, -6.773049970042206880 ) ) ;
#42578 = EDGE_CURVE ( 'NONE', #7863, #79260, #83398, .T. ) ;
#42579 = CARTESIAN_POINT ( 'NONE',  ( 207.8431546909062320, 270.6520914003897360, -6.441273666418043220 ) ) ;
#42580 = CARTESIAN_POINT ( 'NONE',  ( 77.24272341830209143, 208.7365022471902023, -10.00000000000009237 ) ) ;
#42581 = CARTESIAN_POINT ( 'NONE',  ( 149.9060791885465846, 273.0020498124315509, -11.57482514211843849 ) ) ;
#42582 = CARTESIAN_POINT ( 'NONE',  ( 176.9166214895533642, 269.9654513595619960, 17.05290727745522972 ) ) ;
#42583 = VECTOR ( 'NONE', #85970, 1000.000000000000000 ) ;
#42584 = CARTESIAN_POINT ( 'NONE',  ( 151.5781362109140105, 269.4382799247086382, -14.31326077235408079 ) ) ;
#42585 = CARTESIAN_POINT ( 'NONE',  ( 47.49582885874516336, 78.29235751436857527, -10.00000000000000000 ) ) ;
#42586 = CARTESIAN_POINT ( 'NONE',  ( 164.2414282675923403, 253.9130995731632083, 14.60178471863180327 ) ) ;
#42587 = CARTESIAN_POINT ( 'NONE',  ( 163.7085541710205234, 247.0954618725873217, -6.713544974106887331 ) ) ;
#42588 = CARTESIAN_POINT ( 'NONE',  ( 131.4326323866306439, 240.5643266524160140, 9.188101187500095079 ) ) ;
#42589 = ORIENTED_EDGE ( 'NONE', *, *, #69077, .T. ) ;
#42590 = CARTESIAN_POINT ( 'NONE',  ( 85.72596786555051551, 44.18998096972852352, -6.301796949671089720 ) ) ;
#42591 = LINE ( 'NONE', #12223, #2852 ) ;
#42592 = CIRCLE ( 'NONE', #78196, 17.82106496071138935 ) ;
#42593 = CARTESIAN_POINT ( 'NONE',  ( 202.8549823380854491, 279.2918593523859272, -16.39745931995414807 ) ) ;
#42594 = FACE_OUTER_BOUND ( 'NONE', #30964, .T. ) ;
#42595 = CARTESIAN_POINT ( 'NONE',  ( 74.46953503235177152, 59.54388530620969533, 15.67556957382890559 ) ) ;
#42596 = DIRECTION ( 'NONE',  ( 0.1857746241280557598, -0.9825923819316327856, 0.000000000000000000 ) ) ;
#42597 = ORIENTED_EDGE ( 'NONE', *, *, #80108, .F. ) ;
#42598 = CARTESIAN_POINT ( 'NONE',  ( 80.29543856085656728, 57.12815561284512711, -16.23372326876640770 ) ) ;
#42599 = CIRCLE ( 'NONE', #55604, 70.00000000000001421 ) ;
#42600 = CARTESIAN_POINT ( 'NONE',  ( 167.5662050468191637, 249.1799470243284986, -5.491780700972443974 ) ) ;
#42601 = CARTESIAN_POINT ( 'NONE',  ( 164.8012313184158018, 245.2028895370295913, -2.462952685407667097 ) ) ;
#42602 = CARTESIAN_POINT ( 'NONE',  ( 144.9642793207625004, 248.3768266524159856, -9.188101187500093303 ) ) ;
#42603 = CARTESIAN_POINT ( 'NONE',  ( -48.71813016832984289, 30.75580926756359901, -10.00000000000000000 ) ) ;
#42604 = AXIS2_PLACEMENT_3D ( 'NONE', #63455, #2672, #70041 ) ;
#42605 = DIRECTION ( 'NONE',  ( -0.000000000000000000, 1.000000000000000000, -0.000000000000000000 ) ) ;
#42606 = CYLINDRICAL_SURFACE ( 'NONE', #48283, 70.00000000000002842 ) ;
#42607 = CARTESIAN_POINT ( 'NONE',  ( 157.7593757092099906, 257.3997412317380054, -18.08445832352326121 ) ) ;
#42608 = CARTESIAN_POINT ( 'NONE',  ( 173.3722461183258190, 251.8737700704222107, 3.437992158665448272 ) ) ;
#42609 = EDGE_CURVE ( 'NONE', #52564, #82653, #73117, .T. ) ;
#42610 = CARTESIAN_POINT ( 'NONE',  ( 14.52789699003380974, 30.16126292948894871, -6.180339887498951690 ) ) ;
#42611 = CARTESIAN_POINT ( 'NONE',  ( 190.7862358025146534, 300.1955415356651429, 3.573119809004446257 ) ) ;
#42612 = CARTESIAN_POINT ( 'NONE',  ( 155.3570097178104277, 279.6568258031100527, -1.565792345466651359 ) ) ;
#42613 = CARTESIAN_POINT ( 'NONE',  ( 169.3954986152665754, 285.0806455033480233, -8.523934259276524372 ) ) ;
#42614 = CARTESIAN_POINT ( 'NONE',  ( 159.4889735931715222, 254.4039898200529706, 16.88104032092801887 ) ) ;
#42615 = EDGE_CURVE ( 'NONE', #64780, #48318, #38321, .T. ) ;
#42616 = CARTESIAN_POINT ( 'NONE',  ( 187.4307896699236835, 297.8422539827560058, -7.210019786355569060 ) ) ;
#42617 = CARTESIAN_POINT ( 'NONE',  ( 137.1969404309142817, 260.0177522451418781, 5.000000000000046185 ) ) ;
#42618 = ADVANCED_FACE ( 'NONE', ( #34587 ), #95944, .T. ) ;
#42619 = CARTESIAN_POINT ( 'NONE',  ( 25.62571989635185332, 15.76426979415090202, 3.090169943749476733 ) ) ;
#42620 = ORIENTED_EDGE ( 'NONE', *, *, #30455, .F. ) ;
#42621 = ADVANCED_FACE ( 'NONE', ( #65487 ), #87811, .F. ) ;
#42622 = CARTESIAN_POINT ( 'NONE',  ( 196.3519702320103590, 290.5554067223432639, 17.39042812051341969 ) ) ;
#42623 = CARTESIAN_POINT ( 'NONE',  ( 190.5969391768923913, 300.5234129089444650, -0.7564693504096553500 ) ) ;
#42624 = CARTESIAN_POINT ( 'NONE',  ( -9.729855525997878729, 171.3149278399161233, 9.188101187500093303 ) ) ;
#42625 = CARTESIAN_POINT ( 'NONE',  ( 42.04265951369687571, 185.8923013555410080, 4.594050593750050204 ) ) ;
#42626 = CARTESIAN_POINT ( 'NONE',  ( 175.4247336203138445, 256.7083858149467233, -10.72411828751436325 ) ) ;
#42627 = CARTESIAN_POINT ( 'NONE',  ( 16.89228056887236917, 28.49103043416548786, -8.090169943749479842 ) ) ;
#42628 = CARTESIAN_POINT ( 'NONE',  ( -67.83107014231842413, 42.28230845022618922, -10.00000000000000000 ) ) ;
#42629 = CYLINDRICAL_SURFACE ( 'NONE', #91658, 10.00000000000010658 ) ;
#42630 = LINE ( 'NONE', #56841, #30630 ) ;
#42631 = CARTESIAN_POINT ( 'NONE',  ( 147.2494378675467033, 275.6034875578896504, 3.639370109197119341 ) ) ;
#42632 = CARTESIAN_POINT ( 'NONE',  ( 74.14739530845520221, 55.62984604024180868, -16.59005736389721619 ) ) ;
#42634 = CARTESIAN_POINT ( 'NONE',  ( 69.21394623383592659, 210.7677522451418497, 10.00000000000009592 ) ) ;
#42633 = CARTESIAN_POINT ( 'NONE',  ( 167.4001030851802057, 256.8364653434372258, 14.17688984365114280 ) ) ;
#42635 = CARTESIAN_POINT ( 'NONE',  ( 75.06169617786551385, 67.15492690307928569, 12.60468746697864439 ) ) ;
#42636 = CARTESIAN_POINT ( 'NONE',  ( 157.8043799545718286, 257.3217915922150496, -17.97575562758749257 ) ) ;
#42637 = DIRECTION ( 'NONE',  ( 0.8660254037844341557, 0.5000000000000082157, -0.000000000000000000 ) ) ;
#42638 = CARTESIAN_POINT ( 'NONE',  ( 40.79748767570693246, 194.3615022471902591, -10.00000000000009592 ) ) ;
#42639 = CARTESIAN_POINT ( 'NONE',  ( 66.60661563016273590, 67.77273566365288104, -7.043189648870077590 ) ) ;
#42640 = CARTESIAN_POINT ( 'NONE',  ( 163.2919429874875448, 247.8170536094679903, 9.876785378511263147 ) ) ;
#42641 = CARTESIAN_POINT ( 'NONE',  ( 13.13906166239122619, 169.2048013555410080, 4.594050593750051981 ) ) ;
#42642 = CARTESIAN_POINT ( 'NONE',  ( 168.1388510285085260, 286.2295795236503864, 4.095240327730098606 ) ) ;
#42643 = FACE_OUTER_BOUND ( 'NONE', #57235, .T. ) ;
#42644 = CARTESIAN_POINT ( 'NONE',  ( 30.44305165777243971, 40.68290643055189548, 3.479690158560446702E-15 ) ) ;
#42645 = LINE ( 'NONE', #4159, #82174 ) ;
#42646 = CARTESIAN_POINT ( 'NONE',  ( 207.6727254509676186, 270.9472835030587703, 7.315149605389819953 ) ) ;
#42647 = CARTESIAN_POINT ( 'NONE',  ( 193.7261517370125432, 295.1034577671335342, 14.97744313279139661 ) ) ;
#42648 = CARTESIAN_POINT ( 'NONE',  ( 34.71711421221060334, 41.81751292744059612, -6.180339887498951690 ) ) ;
#42649 = CARTESIAN_POINT ( 'NONE',  ( 176.5733983122591439, 260.2598607953340775, -13.59682439435957946 ) ) ;
#42650 = CARTESIAN_POINT ( 'NONE',  ( 14.11662529016922640, 10.01110640527290663, 2.839279412974134775 ) ) ;
#42651 = CARTESIAN_POINT ( 'NONE',  ( 71.69055946895423403, 72.48590965862312885, 0.9596580914388637140 ) ) ;
#42652 = CARTESIAN_POINT ( 'NONE',  ( 22.55376741186237410, 15.94754757982089544, 5.678558825948272215 ) ) ;
#42653 = CARTESIAN_POINT ( 'NONE',  ( 159.1730915527162438, 259.4008141402116507, 16.68298605874345597 ) ) ;
#42654 = AXIS2_PLACEMENT_3D ( 'NONE', #62839, #39028, #30945 ) ;
#42655 = CARTESIAN_POINT ( 'NONE',  ( 152.7657949578753289, 278.5609422129916766, -4.697314451781300804 ) ) ;
#42656 = ORIENTED_EDGE ( 'NONE', *, *, #10593, .F. ) ;
#42657 = CARTESIAN_POINT ( 'NONE',  ( 156.8398918776343294, 276.5535896746492313, 11.26052967366049806 ) ) ;
#42658 = CARTESIAN_POINT ( 'NONE',  ( 159.8946522441011382, 253.7013337850969492, -16.68230890105693121 ) ) ;
#42659 = ORIENTED_EDGE ( 'NONE', *, *, #96221, .T. ) ;
#42660 = CARTESIAN_POINT ( 'NONE',  ( 38.90713690219553200, 54.71539658304152454, 10.00000000000000000 ) ) ;
#42661 = CARTESIAN_POINT ( 'NONE',  ( 206.9377610035629118, 272.2202792677204002, 7.440532334334675646 ) ) ;
#42662 = DIRECTION ( 'NONE',  ( -0.8660254037844379305, -0.5000000000000014433, -0.000000000000000000 ) ) ;
#42663 = CARTESIAN_POINT ( 'NONE',  ( 118.6676052326576922, 245.9865022471902876, -10.00000000000009592 ) ) ;
#42664 = PRESENTATION_LAYER_ASSIGNMENT (  '', '', ( #39400 ) ) ;
#42665 = ORIENTED_EDGE ( 'NONE', *, *, #100184, .T. ) ;
#42666 = ORIENTED_EDGE ( 'NONE', *, *, #34155, .T. ) ;
#42668 = DIRECTION ( 'NONE',  ( 0.3297783986044549587, 0.8484238185761712181, -0.4140328874455618258 ) ) ;
#42667 = CARTESIAN_POINT ( 'NONE',  ( 164.1571068132817857, 246.7865404346968035, -5.088878239364682976 ) ) ;
#42669 = CARTESIAN_POINT ( 'NONE',  ( 153.4578721839791342, 264.8501638863745029, 16.85421393845643223 ) ) ;
#42670 = ORIENTED_EDGE ( 'NONE', *, *, #71711, .T. ) ;
#42671 = CARTESIAN_POINT ( 'NONE',  ( -62.83817737799399339, 37.97373922903764765, 10.00000000000000000 ) ) ;
#42672 = CARTESIAN_POINT ( 'NONE',  ( 174.6205011729852856, 262.3198158003589242, 14.36378246763594468 ) ) ;
#42673 = ORIENTED_EDGE ( 'NONE', *, *, #20368, .F. ) ;
#42674 = LINE ( 'NONE', #41181, #28080 ) ;
#42675 = CARTESIAN_POINT ( 'NONE',  ( 159.8822213732012756, 255.7228646850775533, -16.63148941946954196 ) ) ;
#42676 = CARTESIAN_POINT ( 'NONE',  ( 149.6230451358742926, 271.4922791719315001, -12.72565967355361671 ) ) ;
#42677 = EDGE_CURVE ( 'NONE', #94567, #94878, #7095, .T. ) ;
#42678 = CARTESIAN_POINT ( 'NONE',  ( 170.6178593158246315, 266.5408558992322696, -17.65857870869936974 ) ) ;
#42679 = ORIENTED_EDGE ( 'NONE', *, *, #97840, .F. ) ;
#42680 = CARTESIAN_POINT ( 'NONE',  ( 174.1176602439136332, 267.3798616381827173, 17.23308470258429992 ) ) ;
#42681 = CARTESIAN_POINT ( 'NONE',  ( 166.0506673010352472, 274.1027903476490337, -16.62009509085023851 ) ) ;
#42682 = LINE ( 'NONE', #57396, #55807 ) ;
#42683 = PRODUCT_DEFINITION_SHAPE ( 'NONE', 'NONE',  #100300 ) ;
#42684 = ORIENTED_EDGE ( 'NONE', *, *, #3882, .F. ) ;
#42685 = CARTESIAN_POINT ( 'NONE',  ( 176.8603533460532162, 279.0893642389937099, -16.89033693841190242 ) ) ;
#42686 = CARTESIAN_POINT ( 'NONE',  ( 169.0226874675672661, 261.4850206712534373, -16.08682720245705156 ) ) ;
#42687 = EDGE_LOOP ( 'NONE', ( #20177, #5436, #18820, #52293, #8910 ) ) ;
#42688 = CARTESIAN_POINT ( 'NONE',  ( 179.4037581149374034, 257.9870511612666064, -10.76565914641300736 ) ) ;
#42689 = ORIENTED_EDGE ( 'NONE', *, *, #89860, .T. ) ;
#42690 = DIRECTION ( 'NONE',  ( -0.8660254037844387076, -0.4999999999999998890, -0.000000000000000000 ) ) ;
#42691 = ORIENTED_EDGE ( 'NONE', *, *, #153, .F. ) ;
#42692 = CARTESIAN_POINT ( 'NONE',  ( 158.8103961591765767, 260.0426163253080745, 17.56740887531538675 ) ) ;
#42693 = DIRECTION ( 'NONE',  ( 0.5000000000000008882, -0.8660254037844381525, -0.000000000000000000 ) ) ;
#42694 = CARTESIAN_POINT ( 'NONE',  ( 82.74741872462533365, 53.81327073439516795, 15.79824936317409545 ) ) ;
#42695 = CARTESIAN_POINT ( 'NONE',  ( 10.64836937555893570, 29.08080186712591697, -3.090169943749475845 ) ) ;
#42696 = CARTESIAN_POINT ( 'NONE',  ( -46.74660806181546491, 29.87360136034011049, -10.00000000000000000 ) ) ;
#42697 = CARTESIAN_POINT ( 'NONE',  ( 178.4964614385565653, 291.5674140005135087, 6.117148090635161850 ) ) ;
#42698 = CARTESIAN_POINT ( 'NONE',  ( 158.3372743204232336, 256.3987914754929420, -17.01754169342242662 ) ) ;
#42699 = ORIENTED_EDGE ( 'NONE', *, *, #48738, .F. ) ;
#42700 = DIRECTION ( 'NONE',  ( -0.9263643838751194348, -0.3766285016932073293, 0.000000000000000000 ) ) ;
#42701 = CARTESIAN_POINT ( 'NONE',  ( 25.52954022263672940, 23.24335787977764411, -9.188101187500008038 ) ) ;
#42702 = PLANE ( 'NONE',  #94751 ) ;
#42703 = CARTESIAN_POINT ( 'NONE',  ( 206.5318754762992910, 272.9232936229979032, 10.63244694018452741 ) ) ;
#42705 = VERTEX_POINT ( 'NONE', #28994 ) ;
#42704 = DIRECTION ( 'NONE',  ( -1.000000000000000000, 0.000000000000000000, 0.000000000000000000 ) ) ;
#42706 = ORIENTED_EDGE ( 'NONE', *, *, #6227, .T. ) ;
#42707 = CARTESIAN_POINT ( 'NONE',  ( 190.6453198962280453, 300.4396150449484821, 6.790521636783821258 ) ) ;
#42708 = CARTESIAN_POINT ( 'NONE',  ( 171.4644772550263667, 259.7729622726477601, -14.70397530572840417 ) ) ;
#42709 = CARTESIAN_POINT ( 'NONE',  ( 16.82306525903893046, 33.21091486745860522, -1.111400068045478839E-16 ) ) ;
#42710 = CARTESIAN_POINT ( 'NONE',  ( 17.22757050757671493, 15.11029122506293554, -8.090169943749478065 ) ) ;
#42711 = CARTESIAN_POINT ( 'NONE',  ( 199.2085059260846549, 285.6077417665728149, -18.52696122218391750 ) ) ;
#42712 = CARTESIAN_POINT ( 'NONE',  ( 190.1621882522046576, 301.2764235991409123, 0.1320823580815838616 ) ) ;
#42713 = ORIENTED_EDGE ( 'NONE', *, *, #6649, .T. ) ;
#42714 = CARTESIAN_POINT ( 'NONE',  ( 167.2444082654604642, 252.9089594313395537, -12.21390469949916557 ) ) ;
#42715 = CARTESIAN_POINT ( 'NONE',  ( 205.7543183366283870, 273.7119534119829609, 10.15442286887563839 ) ) ;
#42716 = CYLINDRICAL_SURFACE ( 'NONE', #30127, 17.82106496071139645 ) ;
#42717 = CARTESIAN_POINT ( 'NONE',  ( 165.0509870607838252, 244.7702999017660375, -2.356357909806504392 ) ) ;
#42718 = CARTESIAN_POINT ( 'NONE',  ( 30.24280306353621128, 178.2677522451417929, -5.000000000000041744 ) ) ;
#42719 = CARTESIAN_POINT ( 'NONE',  ( 111.8659576938172364, 226.2048013555410080, 4.594050593750051981 ) ) ;
#42720 = CARTESIAN_POINT ( 'NONE',  ( 82.80564809348420852, 40.64392876433748825, -1.326136484287901096 ) ) ;
#42721 = CARTESIAN_POINT ( 'NONE',  ( 164.2369440024486664, 280.7661753373989768, -11.66746695687372615 ) ) ;
#42722 = CARTESIAN_POINT ( 'NONE',  ( 84.72015715327184182, 50.52193132731910197, 13.57015802400779947 ) ) ;
#42723 = CARTESIAN_POINT ( 'NONE',  ( 207.7679535393632477, 270.7823436156499497, 1.643001479255987274 ) ) ;
#42724 = CARTESIAN_POINT ( 'NONE',  ( 17.30628827445631401, 189.9869531367911293, 4.594050593750046652 ) ) ;
#42725 = CARTESIAN_POINT ( 'NONE',  ( 176.5750811079351763, 290.0661888821730372, -9.631901365267058424 ) ) ;
#42726 = VERTEX_POINT ( 'NONE', #59868 ) ;
#42727 = EDGE_LOOP ( 'NONE', ( #74736, #77061, #87874, #14178 ) ) ;
#42728 = LINE ( 'NONE', #35146, #55922 ) ;
#42729 = CARTESIAN_POINT ( 'NONE',  ( 185.4335740946144711, 259.3911566074018538, -5.299005558259515247 ) ) ;
#42730 = CARTESIAN_POINT ( 'NONE',  ( 87.27117856089937220, 44.98890866680353895, -6.231534082530021834 ) ) ;
#42731 = CARTESIAN_POINT ( 'NONE',  ( 147.4317198359019301, 275.2877659273946733, 3.797273160043843188 ) ) ;
#42732 = DIRECTION ( 'NONE',  ( -0.5696381972391160176, 0.8218955677251033043, 0.000000000000000000 ) ) ;
#42733 = AXIS2_PLACEMENT_3D ( 'NONE', #74565, #80695, #35536 ) ;
#42734 = CARTESIAN_POINT ( 'NONE',  ( 161.1232569692349443, 251.5733279787459367, -14.02750397520710557 ) ) ;
#42735 = CARTESIAN_POINT ( 'NONE',  ( 182.3344119359328488, 284.3327036968043444, 14.89823965017127172 ) ) ;
#42736 = CARTESIAN_POINT ( 'NONE',  ( -22.42236680055709641, 157.8615022471902591, 0.000000000000000000 ) ) ;
#42737 = B_SPLINE_CURVE_WITH_KNOTS ( 'NONE', 3,
 ( #85427, #31165, #53469, #22084, #54450, #69672, #47370, #8876, #70673, #77801, #62054, #76306, #61066, #61567, #39744, #6878, #7372, #77281, #15458, #84915, #278, #46356, #7891, #38258, #93005, #1288, #16475, #23558, #37768, #38768, #92035, #68671, #53958, #76779, #52980, #83929, #100103, #30178, #15975, #22582, #30687, #85947, #99596, #46876, #93518, #14968 ),
 .UNSPECIFIED., .F., .F.,
 ( 4, 1, 1, 1, 2, 2, 1, 1, 1, 2, 2, 1, 1, 2, 2, 1, 1, 2, 2, 1, 1, 2, 2, 1, 2, 2, 1, 2, 2, 4 ),
 ( 0.000000000000000000, 0.06249999999996815048, 0.09374999999995237143, 0.1093749999999444888, 0.1171874999999418798, 0.1249999999999392708, 0.1874999999999252265, 0.2187499999999161504, 0.2343749999999128752, 0.2421874999999134304, 0.2499999999999140132, 0.3124999999999193423, 0.3437499999999231726, 0.3593749999999252265, 0.3749999999999272249, 0.4374999999999390488, 0.4687499999999459321, 0.4843749999999473754, 0.4999999999999489297, 0.5624999999999630296, 0.5937499999999682476, 0.6093749999999708011, 0.6249999999999733546, 0.6874999999999765743, 0.7187499999999773515, 0.7499999999999780176, 0.8124999999999832356, 0.8437499999999856781, 0.8749999999999882316, 1.000000000000000000 ),
 .UNSPECIFIED. ) ;
#42738 = CARTESIAN_POINT ( 'NONE',  ( 38.41565749170202082, 202.1744531367911293, 4.594050593750047540 ) ) ;
#42739 = CARTESIAN_POINT ( 'NONE',  ( 100.8960422556166634, 222.3927522451418213, 10.00000000000009592 ) ) ;
#42740 = ORIENTED_EDGE ( 'NONE', *, *, #6844, .F. ) ;
#42741 = CARTESIAN_POINT ( 'NONE',  ( 83.55693731525771284, 46.16036024266245619, 10.67923881757085525 ) ) ;
#42742 = EDGE_CURVE ( 'NONE', #92439, #21055, #21386, .T. ) ;
#42743 = VECTOR ( 'NONE', #50424, 1000.000000000000000 ) ;
#42744 = CARTESIAN_POINT ( 'NONE',  ( 178.9500347670535234, 258.7740023882205378, -10.02348361398978760 ) ) ;
#42745 = CARTESIAN_POINT ( 'NONE',  ( -6.184650803196579893, 176.4244531367911293, -4.594050593750046652 ) ) ;
#42746 = CARTESIAN_POINT ( 'NONE',  ( 72.69493809724966127, 71.16443809380129437, -7.267007365939471164 ) ) ;
#42747 = CARTESIAN_POINT ( 'NONE',  ( 198.4427928769277969, 286.9339956717308837, -17.97122743692687763 ) ) ;
#42748 = DIRECTION ( 'NONE',  ( -0.000000000000000000, -0.000000000000000000, -1.000000000000000000 ) ) ;
#42749 = CARTESIAN_POINT ( 'NONE',  ( 192.5551423381268989, 297.1317055421444024, -13.20528585388119858 ) ) ;
#42750 = CARTESIAN_POINT ( 'NONE',  ( 72.38858704899024588, 72.34360798638101642, 0.000000000000000000 ) ) ;
#42751 = CARTESIAN_POINT ( 'NONE',  ( 204.1090098116124238, 275.4430282029952082, 13.26781899738782222 ) ) ;
#42752 = CARTESIAN_POINT ( 'NONE',  ( 68.80363134320050733, 67.62982772949345645, 8.378572803659114498 ) ) ;
#42753 = CARTESIAN_POINT ( 'NONE',  ( 206.8986117509267899, 272.2880877623646825, 6.975890063856878598 ) ) ;
#42754 = ORIENTED_EDGE ( 'NONE', *, *, #21470, .F. ) ;
#42755 =( BOUNDED_CURVE ( )  B_SPLINE_CURVE ( 2, ( #35132, #73651, #11859, #4752, #19952, #19478, #73166, #27560, #4232 ),
 .UNSPECIFIED., .F., .T. ) 
 B_SPLINE_CURVE_WITH_KNOTS ( ( 3, 2, 2, 2, 3 ),
 ( 0.8750000000000000000, 0.8763440860215053752, 0.8790322580645161255, 0.8817204301075268758, 0.8830645161290322509 ),
 .UNSPECIFIED. ) 
 CURVE ( )  GEOMETRIC_REPRESENTATION_ITEM ( )  RATIONAL_B_SPLINE_CURVE ( ( 0.9330127018922194093, 0.9330127018922194093, 1.000000000000000000, 0.8660254037844387076, 1.000000000000000000, 0.8660254037844387076, 1.000000000000000000, 0.9330127018922194093, 0.9330127018922194093 ) ) 
 REPRESENTATION_ITEM ( '' )  );
#42756 = CARTESIAN_POINT ( 'NONE',  ( 164.9872103004705082, 269.1319161758361247, 17.53557708690383876 ) ) ;
#42757 = CARTESIAN_POINT ( 'NONE',  ( 7.888522331898304429, 165.3615022471902023, 5.000000000000051514 ) ) ;
#42758 = LINE ( 'NONE', #20496, #69235 ) ;
#42759 = CARTESIAN_POINT ( 'NONE',  ( 127.1025053677084742, 238.0643266524160424, -9.188101187500093303 ) ) ;
#42760 = CARTESIAN_POINT ( 'NONE',  ( 24.83368966200164607, 16.19860640527292261, 2.839279412974134775 ) ) ;
#42761 = CARTESIAN_POINT ( 'NONE',  ( 74.74196695595742312, 67.08715363026114176, 12.96493619559571897 ) ) ;
#42762 = CARTESIAN_POINT ( 'NONE',  ( 150.9781172735503390, 269.9373692962728910, 13.75123450916632883 ) ) ;
#42764 = CARTESIAN_POINT ( 'NONE',  ( 189.4648164480647381, 289.7840259140004378, 14.59263643371816954 ) ) ;
#42763 = CARTESIAN_POINT ( 'NONE',  ( 196.3021893095863959, 290.6416298092292436, 17.45656988653421138 ) ) ;
#42765 = CARTESIAN_POINT ( 'NONE',  ( -63.08903959183646748, 39.77784189046417396, -10.00000000000000000 ) ) ;
#42766 = B_SPLINE_CURVE_WITH_KNOTS ( 'NONE', 3,
 ( #60927, #20981, #91891, #52342, #84291, #14838, #90904, #13851, #67544, #75662 ),
 .UNSPECIFIED., .F., .F.,
 ( 4, 2, 2, 2, 4 ),
 ( 0.000000000000000000, 0.0002622400424273148181, 0.0005244800848546296362, 0.0007867201272819444001, 0.001048960169709259272 ),
 .UNSPECIFIED. ) ;
#42767 = ORIENTED_EDGE ( 'NONE', *, *, #20259, .T. ) ;
#42768 = CARTESIAN_POINT ( 'NONE',  ( 162.5148320529283126, 285.2034568178174254, 0.5437328601018158736 ) ) ;
#42769 = CARTESIAN_POINT ( 'NONE',  ( 163.3761757142922875, 247.6711582469822019, 7.822525700913879554 ) ) ;
#42770 = CARTESIAN_POINT ( 'NONE',  ( 82.41630873631589793, 41.31828431233920895, -3.367117793111288560 ) ) ;
#42771 = CARTESIAN_POINT ( 'NONE',  ( 173.0221673524149537, 268.1772831482880974, -16.30159817659111354 ) ) ;
#42772 = CARTESIAN_POINT ( 'NONE',  ( 81.39796143918844962, 55.18843397982647758, -15.93664522424668917 ) ) ;
#42773 = VERTEX_POINT ( 'NONE', #75591 ) ;
#42774 = DIRECTION ( 'NONE',  ( -0.8660254037844387076, -0.4999999999999998890, -0.000000000000000000 ) ) ;
#42775 = CARTESIAN_POINT ( 'NONE',  ( 165.4631639692057092, 269.4820744690946981, -16.38125699399958890 ) ) ;
#42776 = CARTESIAN_POINT ( 'NONE',  ( 72.01395728112395034, 72.29389942223538412, 0.6844073223025460839 ) ) ;
#42777 = CARTESIAN_POINT ( 'NONE',  ( 149.3083371557971475, 273.7923365791965580, -10.10007029348708585 ) ) ;
#42778 = CARTESIAN_POINT ( 'NONE',  ( 79.78296747758277263, 52.56098969188083458, 15.47212231616918388 ) ) ;
#42779 = CARTESIAN_POINT ( 'NONE',  ( 181.8748162431300273, 295.1086854819222367, 4.838109536733072424 ) ) ;
#42780 = CARTESIAN_POINT ( 'NONE',  ( 71.09572938139255882, 71.74208345363453532, -0.6570354662424334746 ) ) ;
#42781 = DIRECTION ( 'NONE',  ( -0.8660254037844387076, -0.4999999999999998890, -0.000000000000000000 ) ) ;
#42782 = CARTESIAN_POINT ( 'NONE',  ( 193.4106419289095413, 282.3615967192327503, 16.94929546279620780 ) ) ;
#42783 = CARTESIAN_POINT ( 'NONE',  ( 12.10719531124914283, 12.15404122711131585, 8.090169943749479842 ) ) ;
#42784 = CARTESIAN_POINT ( 'NONE',  ( -22.42236680055709641, 157.8615022471902591, 0.000000000000000000 ) ) ;
#42785 = ORIENTED_EDGE ( 'NONE', *, *, #11096, .F. ) ;
#42786 = FACE_BOUND ( 'NONE', #5066, .T. ) ;
#42787 = CARTESIAN_POINT ( 'NONE',  ( 194.1972774922283236, 294.2874440223457100, -15.09915398317898649 ) ) ;
#42788 = CARTESIAN_POINT ( 'NONE',  ( 159.6845851668356602, 264.1119169267814186, -17.40983169896417593 ) ) ;
#42789 = ORIENTED_EDGE ( 'NONE', *, *, #15658, .T. ) ;
#42790 = CARTESIAN_POINT ( 'NONE',  ( 79.24589768621441976, 59.96875100242885992, 16.14305910152894796 ) ) ;
#42791 = DIRECTION ( 'NONE',  ( -0.000000000000000000, -0.000000000000000000, -1.000000000000000000 ) ) ;
#42792 = EDGE_CURVE ( 'NONE', #40669, #99571, #56467, .T. ) ;
#42793 = CARTESIAN_POINT ( 'NONE',  ( 42.45923888023187232, 122.5484010731363043, -10.00000000000000000 ) ) ;
#42794 = EDGE_LOOP ( 'NONE', ( #28842, #4179, #95475 ) ) ;
#42795 = CARTESIAN_POINT ( 'NONE',  ( 90.72943840876205002, 217.0643266524159856, -9.188101187500093303 ) ) ;
#42796 = CARTESIAN_POINT ( 'NONE',  ( 82.58801462665896054, 50.50509293822858581, -14.17187532088357926 ) ) ;
#42797 = CARTESIAN_POINT ( 'NONE',  ( -26.60548277334042666, 60.56602913741141947, -10.00000000000000000 ) ) ;
#42798 = CARTESIAN_POINT ( 'NONE',  ( 183.0029883054649247, 258.5817195840489262, -5.861537397372212688 ) ) ;
#42799 = ORIENTED_EDGE ( 'NONE', *, *, #21058, .F. ) ;
#42800 = CARTESIAN_POINT ( 'NONE',  ( 191.3843761966370209, 282.8631020262318430, -17.76976768207862278 ) ) ;
#42801 = VERTEX_POINT ( 'NONE', #6176 ) ;
#42802 = CARTESIAN_POINT ( 'NONE',  ( 175.4039180538638050, 286.4985578832265105, -12.71199677751706503 ) ) ;
#42803 = AXIS2_PLACEMENT_3D ( 'NONE', #42099, #96346, #88771 ) ;
#42805 = ADVANCED_FACE ( 'NONE', ( #76107 ), #6681, .T. ) ;
#42804 = ORIENTED_EDGE ( 'NONE', *, *, #41947, .F. ) ;
#42806 = CARTESIAN_POINT ( 'NONE',  ( 75.06692456002483027, 59.04669605262043319, 15.83186505758761164 ) ) ;
#42807 = CARTESIAN_POINT ( 'NONE',  ( 203.3740894404336927, 278.3927394765486838, -15.19753795879846869 ) ) ;
#42808 = VERTEX_POINT ( 'NONE', #45654 ) ;
#42809 = CARTESIAN_POINT ( 'NONE',  ( 30.68864658225822240, 104.9767549103658126, 59.99999999999999289 ) ) ;
#42810 = CARTESIAN_POINT ( 'NONE',  ( 82.19055047383055523, 40.63346341616176716, 3.399030102818711541 ) ) ;
#42811 = CARTESIAN_POINT ( 'NONE',  ( 162.6510684159478899, 255.6836685834286698, -14.96140778093960044 ) ) ;
#42812 = CARTESIAN_POINT ( 'NONE',  ( 158.6360470686486792, 274.9027906808635180, -12.66648404655886395 ) ) ;
#42814 = EDGE_CURVE ( 'NONE', #43232, #9334, #34765, .T. ) ;
#42813 = LINE ( 'NONE', #35736, #96499 ) ;
#42815 = DIRECTION ( 'NONE',  ( -0.9890802632347809320, 0.1473778574936430164, 0.000000000000000000 ) ) ;
#42816 = VECTOR ( 'NONE', #53775, 1000.000000000000000 ) ;
#42817 = LINE ( 'NONE', #11474, #92083 ) ;
#42818 = CARTESIAN_POINT ( 'NONE',  ( 147.5623555321158165, 249.8768266524159856, -9.188101187500091527 ) ) ;
#42819 = CARTESIAN_POINT ( 'NONE',  ( 168.1596581537996542, 267.1068951904059645, -17.02861468427176206 ) ) ;
#42820 = CARTESIAN_POINT ( 'NONE',  ( 70.72338235425743846, 61.42563111389683428, -14.82496901324692296 ) ) ;
#42821 = CARTESIAN_POINT ( 'NONE',  ( 7.976297994771393896, 26.64646525600388571, -2.839279412974133887 ) ) ;
#42822 = ORIENTED_EDGE ( 'NONE', *, *, #34421, .F. ) ;
#42824 = ORIENTED_EDGE ( 'NONE', *, *, #18207, .F. ) ;
#42823 = CARTESIAN_POINT ( 'NONE',  ( 204.0811171663250150, 271.5389168563704061, 9.836206406191243090 ) ) ;
#42825 = CARTESIAN_POINT ( 'NONE',  ( 203.2757866645317222, 269.5093088776978334, -7.514607224931010521 ) ) ;
#42826 = CARTESIAN_POINT ( 'NONE',  ( 163.1008115941903895, 248.1481028935802442, 11.25332017433677834 ) ) ;
#42827 = CARTESIAN_POINT ( 'NONE',  ( 76.26781202851402952, 65.13109020310881192, -14.20137929745961003 ) ) ;
#42828 = DIRECTION ( 'NONE',  ( -0.5000000000000005551, 0.8660254037844383745, 0.000000000000000000 ) ) ;
#42829 = CARTESIAN_POINT ( 'NONE',  ( 78.10439711566577614, 51.17412554839856398, -15.81061020820859575 ) ) ;
#42830 = CARTESIAN_POINT ( 'NONE',  ( 174.5324672201822409, 281.8837275374356750, 14.18752577204586274 ) ) ;
#42831 = CARTESIAN_POINT ( 'NONE',  ( 85.34255252599106711, 42.75911001269964373, 2.438663257353666403 ) ) ;
#42832 = CARTESIAN_POINT ( 'NONE',  ( 88.01997546958394025, 44.08896826132783531, -1.712360037130413737 ) ) ;
#42833 = ORIENTED_EDGE ( 'NONE', *, *, #16316, .T. ) ;
#42834 = DIRECTION ( 'NONE',  ( -1.000000000000000000, 0.000000000000000000, -0.000000000000000000 ) ) ;
#42835 = EDGE_LOOP ( 'NONE', ( #21045, #18313, #21486, #4612 ) ) ;
#42836 = CARTESIAN_POINT ( 'NONE',  ( 194.3496232524742879, 293.5687256674401056, -14.39162217157957890 ) ) ;
#42837 = CARTESIAN_POINT ( 'NONE',  ( 201.0634398150303070, 267.8636890061912368, -2.845120707021614237 ) ) ;
#42838 = CARTESIAN_POINT ( 'NONE',  ( 163.7706638094790605, 246.9878848231379038, -7.366147995746058719 ) ) ;
#42839 = CARTESIAN_POINT ( 'NONE',  ( 193.7796494901127744, 262.2143583836045764, -1.898228983734132846 ) ) ;
#42840 = CARTESIAN_POINT ( 'NONE',  ( 160.7802298691281351, 272.6907373984244032, 15.57769528675181903 ) ) ;
#42842 = CARTESIAN_POINT ( 'NONE',  ( 88.44572534255364360, 43.94768732639445830, 1.766277459783984538 ) ) ;
#42841 = CARTESIAN_POINT ( 'NONE',  ( 161.0749639472951742, 282.0180817886167688, -7.709404307391809930 ) ) ;
#42843 = VECTOR ( 'NONE', #92180, 1000.000000000000000 ) ;
#42844 = CARTESIAN_POINT ( 'NONE',  ( 168.2356071464602962, 248.8554872198452301, 6.669745218284529820 ) ) ;
#42845 = EDGE_LOOP ( 'NONE', ( #59195, #13324, #32609, #23103 ) ) ;
#42846 = EDGE_CURVE ( 'NONE', #10803, #37919, #15251, .T. ) ;
#42847 = CARTESIAN_POINT ( 'NONE',  ( 79.19548930461120051, 59.90515312544787463, -16.13566294680263624 ) ) ;
#42848 = CARTESIAN_POINT ( 'NONE',  ( 80.56202954020663753, 57.53823600680942718, 16.23110421993949259 ) ) ;
#42849 = EDGE_CURVE ( 'NONE', #27245, #27644, #38558, .T. ) ;
#42850 = CARTESIAN_POINT ( 'NONE',  ( 72.32858194273194385, 65.82052004871619033, -12.34639520340021868 ) ) ;
#42851 = CARTESIAN_POINT ( 'NONE',  ( 175.0125019719911847, 292.0719086349095051, 3.303583340955516423 ) ) ;
#42852 = CARTESIAN_POINT ( 'NONE',  ( 192.1883190596398094, 297.7670620978826150, 12.41391288785556668 ) ) ;
#42853 = CARTESIAN_POINT ( 'NONE',  ( 80.92473437028310457, 43.34290539593628466, -9.976869929326982245 ) ) ;
#42854 = DIRECTION ( 'NONE',  ( -0.5000000000000013323, 0.8660254037844378194, 0.000000000000000000 ) ) ;
#42855 = CARTESIAN_POINT ( 'NONE',  ( 11.92112666437810908, 171.5643266524160140, 9.188101187500095079 ) ) ;
#42856 = CARTESIAN_POINT ( 'NONE',  ( 101.1213961584103060, 235.3149278399160949, -9.188101187500095079 ) ) ;
#42857 = MANIFOLD_SOLID_BREP ( 'Split Line1', #96095 ) ;
#42858 = PLANE ( 'NONE',  #33741 ) ;
#42859 = CARTESIAN_POINT ( 'NONE',  ( 180.3719397577650625, 255.7858912907505271, -2.354358376422963417 ) ) ;
#42860 = LINE ( 'NONE', #72315, #91704 ) ;
#42861 = ADVANCED_FACE ( 'NONE', ( #18288 ), #53752, .F. ) ;
#42862 = CARTESIAN_POINT ( 'NONE',  ( 0.5143710859096835009, 78.77562236714182120, 59.99999999999999289 ) ) ;
#42863 = CARTESIAN_POINT ( 'NONE',  ( 163.7018558908529826, 283.5206950014648442, 5.691029027290803732 ) ) ;
#42864 = CARTESIAN_POINT ( 'NONE',  ( 194.9385458806846430, 293.0035295114944347, -15.70518692812489192 ) ) ;
#42865 = EDGE_CURVE ( 'NONE', #76712, #80425, #58258, .T. ) ;
#42866 = CARTESIAN_POINT ( 'NONE',  ( 84.47262166381923976, 50.18302823219130460, 13.87459367389479326 ) ) ;
#42867 = CARTESIAN_POINT ( 'NONE',  ( 189.2845499996045930, 259.5340837477176024, -0.8149847707460528001 ) ) ;
#42868 = CARTESIAN_POINT ( 'NONE',  ( 165.7619395286449162, 253.6454674417704780, -13.15779432277202865 ) ) ;
#42869 = AXIS2_PLACEMENT_3D ( 'NONE', #86496, #9438, #71253 ) ;
#42870 = CARTESIAN_POINT ( 'NONE',  ( 172.5158698997361171, 263.7363841177182735, -15.44335349234447108 ) ) ;
#42871 = CARTESIAN_POINT ( 'NONE',  ( 83.61187889534991768, 209.8923013555409796, 4.594050593750050204 ) ) ;
#42872 = CARTESIAN_POINT ( 'NONE',  ( 207.8984236726843164, 270.5563627158673512, -6.084369154771423815 ) ) ;
#42873 = VECTOR ( 'NONE', #70179, 1000.000000000000000 ) ;
#42874 = DIRECTION ( 'NONE',  ( -0.8660254037844387076, -0.4999999999999998890, -0.000000000000000000 ) ) ;
#42876 = CARTESIAN_POINT ( 'NONE',  ( 72.21491844529387549, 53.64441083166271085, 0.000000000000000000 ) ) ;
#42875 = CARTESIAN_POINT ( 'NONE',  ( 196.0034224882197975, 291.1591091234520263, 17.53794140922627776 ) ) ;
#42877 = CARTESIAN_POINT ( 'NONE',  ( 75.79515598915105556, 65.48576791014883725, 14.28791538466101230 ) ) ;
#42878 = CARTESIAN_POINT ( 'NONE',  ( 173.2357414004084717, 267.9835125820733310, -16.29977483448695708 ) ) ;
#42879 = CARTESIAN_POINT ( 'NONE',  ( 32.24243340009443415, 30.56628583063843152, 9.188101187500006262 ) ) ;
#42880 = CARTESIAN_POINT ( 'NONE',  ( 146.8868584395697781, 276.2314935489248455, -3.891417269505058396 ) ) ;
#42881 = CARTESIAN_POINT ( 'NONE',  ( 136.0806360202347491, 237.8262482093457493, 3.021315404115420679E-15 ) ) ;
#42882 = ORIENTED_EDGE ( 'NONE', *, *, #60365, .T. ) ;
#42883 = CARTESIAN_POINT ( 'NONE',  ( 27.74991983456899902, 18.94754757982090254, 5.678558825948272215 ) ) ;
#42884 = CARTESIAN_POINT ( 'NONE',  ( -50.66443677795496825, 105.0157659939631145, -10.00000000000000000 ) ) ;
#42885 = CARTESIAN_POINT ( 'NONE',  ( 0.005075371086064872639, 27.18819441265828019, 10.00000000000000000 ) ) ;
#42886 = CARTESIAN_POINT ( 'NONE',  ( 190.6592569510245596, 287.2925400494787027, -15.83648776903241817 ) ) ;
#42887 = EDGE_LOOP ( 'NONE', ( #100077, #45937, #55522, #20408 ) ) ;
#42888 = DIRECTION ( 'NONE',  ( -0.000000000000000000, 0.000000000000000000, -1.000000000000000000 ) ) ;
#42889 = CARTESIAN_POINT ( 'NONE',  ( 157.2276673882269051, 268.6185831692512238, 15.65931871386393226 ) ) ;
#42890 = CARTESIAN_POINT ( 'NONE',  ( 75.63268008801898645, 65.14737934564519151, -14.41129995628931404 ) ) ;
#42891 = CARTESIAN_POINT ( 'NONE',  ( 142.1224599184862711, 252.8615022471902307, -10.00000000000009592 ) ) ;
#42892 = CARTESIAN_POINT ( 'NONE',  ( -27.15312891409035601, 106.0554225863516109, 0.000000000000000000 ) ) ;
#42893 = CARTESIAN_POINT ( 'NONE',  ( 74.83655476915186000, 53.51806293172402462, 16.54630480363988809 ) ) ;
#42894 = ORIENTED_EDGE ( 'NONE', *, *, #98274, .F. ) ;
#42895 = CARTESIAN_POINT ( 'NONE',  ( 85.85265132163429769, 47.44586991713102009, 10.77177032529229450 ) ) ;
#42896 = VERTEX_POINT ( 'NONE', #2085 ) ;
#42897 = CARTESIAN_POINT ( 'NONE',  ( 162.7561251957091031, 248.7451172484279027, 11.07313294959361194 ) ) ;
#42898 = CARTESIAN_POINT ( 'NONE',  ( 82.93531674994763137, 41.19304737833027019, 0.2619559300746566732 ) ) ;
#42899 = ORIENTED_EDGE ( 'NONE', *, *, #13762, .T. ) ;
#42900 = DIRECTION ( 'NONE',  ( -0.3358313672678264750, 0.9419221266957381600, 0.000000000000000000 ) ) ;
#42901 = ORIENTED_EDGE ( 'NONE', *, *, #56716, .T. ) ;
#42902 = DIRECTION ( 'NONE',  ( -0.8279987035736640077, -0.5607300124661883656, 0.000000000000000000 ) ) ;
#42903 = CARTESIAN_POINT ( 'NONE',  ( 13.50136424336972141, 8.764269794150880699, 3.090169943749476733 ) ) ;
#42904 = CARTESIAN_POINT ( 'NONE',  ( 157.9182071844803943, 257.7446772440080736, -16.73371276857705681 ) ) ;
#42905 = CARTESIAN_POINT ( 'NONE',  ( 88.07467786089314643, 44.31731248180877714, -4.422775558719202138 ) ) ;
#42906 = FACE_OUTER_BOUND ( 'NONE', #98403, .T. ) ;
#42908 = EDGE_CURVE ( 'NONE', #94798, #77324, #29913, .T. ) ;
#42907 = AXIS2_PLACEMENT_3D ( 'NONE', #24899, #3622, #34500 ) ;
#42909 = CARTESIAN_POINT ( 'NONE',  ( 31.91767387367526609, 30.37878583063843152, 9.188101187500006262 ) ) ;
#42910 = CARTESIAN_POINT ( 'NONE',  ( 75.70354921996640485, 59.76282743397471364, -15.78267976543943085 ) ) ;
#42911 = EDGE_CURVE ( 'NONE', #71353, #12301, #100095, .T. ) ;
#42912 = CARTESIAN_POINT ( 'NONE',  ( 167.7466885841891724, 276.4027061906341487, 15.04260431868030068 ) ) ;
#42914 = VECTOR ( 'NONE', #22027, 1000.000000000000000 ) ;
#42913 = CARTESIAN_POINT ( 'NONE',  ( 82.65769392073423205, 206.9824982072973967, 3.021315404115420679E-15 ) ) ;
#42915 = ORIENTED_EDGE ( 'NONE', *, *, #25758, .F. ) ;
#42916 = ORIENTED_EDGE ( 'NONE', *, *, #78197, .T. ) ;
#42917 = CARTESIAN_POINT ( 'NONE',  ( 73.16956295238907160, 57.33411781477383329, 16.38320611710937058 ) ) ;
#42919 = CARTESIAN_POINT ( 'NONE',  ( 162.3140616334688389, 272.4534376533870841, -16.17207721611645965 ) ) ;
#42918 = CARTESIAN_POINT ( 'NONE',  ( 204.1793240545508752, 276.9980322128846524, 14.17550310845996187 ) ) ;
#42920 = B_SPLINE_CURVE_WITH_KNOTS ( 'NONE', 3,
 ( #63551, #46854, #78773, #62031, #92982, #77777, #1264, #39231, #70138, #70650, #32148, #94492, #63055, #55429, #86418, #25052, #49359, #72691, #2787, #3768, #3284, #41747, #88421, #10871, #33671, #50348, #11389, #57443, #35147, #34165, #18981, #65057, #18472, #49853, #4768, #80819, #81301, #88933, #42240, #20464, #73178, #11874, #42729, #73667, #4247, #34650, #96007, #66056, #58920, #65550 ),
 .UNSPECIFIED., .F., .F.,
 ( 4, 2, 2, 2, 2, 2, 2, 2, 2, 2, 2, 2, 2, 2, 2, 2, 2, 2, 2, 2, 2, 2, 2, 2, 4 ),
 ( 0.0001133116680782004403, 0.001133496570739383601, 0.001643589022070062779, 0.001771112134902744824, 0.001898635247735426653, 0.002026158360568108482, 0.002153681473400790528, 0.002408727699066037526, 0.002663773924731284957, 0.003173866376061861352, 0.004194051278722935212, 0.005214236181384009940, 0.005724328632714509139, 0.005979374858379796036, 0.006234421084045082932, 0.006298182640461369962, 0.006361944196877656124, 0.006425705753293943154, 0.006489467309710230183, 0.006744513535375672338, 0.006999559761041115359, 0.007254605986706557513, 0.007509652212371999667, 0.007764698438037443556, 0.008274790889368326130 ),
 .UNSPECIFIED. ) ;
#42921 = CARTESIAN_POINT ( 'NONE',  ( 85.39714985353326426, 48.29561332581459965, -11.77387981254187999 ) ) ;
#42922 = CARTESIAN_POINT ( 'NONE',  ( 194.1153812227096864, 294.4292925221022870, 15.54001482840963710 ) ) ;
#42923 = DIRECTION ( 'NONE',  ( 0.7059494278973771353, -0.7082622432767159415, 0.000000000000000000 ) ) ;
#42924 = LINE ( 'NONE', #89609, #74354 ) ;
#42926 = ADVANCED_FACE ( 'NONE', ( #89236 ), #42064, .T. ) ;
#42925 = CARTESIAN_POINT ( 'NONE',  ( 207.8721260090728720, 270.6019116053632843, -5.149293805580906991 ) ) ;
#42927 = CARTESIAN_POINT ( 'NONE',  ( 167.6797392981326595, 266.2679195731100776, 16.57304949636104752 ) ) ;
#42928 = CARTESIAN_POINT ( 'NONE',  ( 181.6314276487895540, 257.0242095793732915, 5.011107819272414332 ) ) ;
#42929 = CARTESIAN_POINT ( 'NONE',  ( 95.76303752037657091, 226.0958772461660260, -9.188101187500095079 ) ) ;
#42930 = ORIENTED_EDGE ( 'NONE', *, *, #11100, .T. ) ;
#42931 = CARTESIAN_POINT ( 'NONE',  ( 73.74866502313744832, 55.21092590717630344, -16.59690200530987170 ) ) ;
#42932 = CARTESIAN_POINT ( 'NONE',  ( 166.2700931250637666, 279.3192040119241142, -14.00315165249155669 ) ) ;
#42933 = VERTEX_POINT ( 'NONE', #80118 ) ;
#42934 = VECTOR ( 'NONE', #64869, 1000.000000000000000 ) ;
#42935 = ORIENTED_EDGE ( 'NONE', *, *, #50326, .T. ) ;
#42936 = CARTESIAN_POINT ( 'NONE',  ( 87.07436038242185816, 45.84038486297258430, -8.630882807222770126 ) ) ;
#42937 = EDGE_CURVE ( 'NONE', #23641, #32592, #72502, .T. ) ;
#42938 = CARTESIAN_POINT ( 'NONE',  ( 180.4853699739515775, 293.9068444078645825, -2.637950556201079877 ) ) ;
#42939 = CARTESIAN_POINT ( 'NONE',  ( 196.2609093297512857, 290.7131288316392670, 16.03897268885959448 ) ) ;
#42940 = CARTESIAN_POINT ( 'NONE',  ( 159.9788992190088948, 253.5554137441726255, -15.81862932303382330 ) ) ;
#42941 = CARTESIAN_POINT ( 'NONE',  ( 207.2149758913051585, 271.2477481997252085, -3.868811482646887789 ) ) ;
#42942 = EDGE_CURVE ( 'NONE', #20188, #57629, #26877, .T. ) ;
#42943 = ORIENTED_EDGE ( 'NONE', *, *, #82167, .F. ) ;
#42944 = AXIS2_PLACEMENT_3D ( 'NONE', #85477, #100149, #21640 ) ;
#42945 = ORIENTED_EDGE ( 'NONE', *, *, #85707, .T. ) ;
#42946 = CARTESIAN_POINT ( 'NONE',  ( 208.0421103033489771, 270.3074901711881353, -2.473242163239977476 ) ) ;
#42947 = EDGE_LOOP ( 'NONE', ( #12760, #89490, #21164, #89411 ) ) ;
#42948 = B_SPLINE_CURVE_WITH_KNOTS ( 'NONE', 3,
 ( #11779, #73570, #80717, #89794 ),
 .UNSPECIFIED., .F., .F.,
 ( 4, 4 ),
 ( 0.009049921839384984096, 0.01512907757492281194 ),
 .UNSPECIFIED. ) ;
#42949 = B_SPLINE_CURVE_WITH_KNOTS ( 'NONE', 3,
 ( #20161, #52041, #82980, #11566 ),
 .UNSPECIFIED., .F., .F.,
 ( 4, 4 ),
 ( 0.03276373770747892378, 0.04170172322417993460 ),
 .UNSPECIFIED. ) ;
#42950 = CARTESIAN_POINT ( 'NONE',  ( 194.5803990493530478, 266.2842781977357163, -7.755041682219012245 ) ) ;
#42951 = CARTESIAN_POINT ( 'NONE',  ( 26.29472225869274382, 23.38052372038641735, 10.00000000000000533 ) ) ;
#42952 = CARTESIAN_POINT ( 'NONE',  ( 82.68642609916942376, 45.53004534498515454, 10.54796185080066984 ) ) ;
#42954 = CARTESIAN_POINT ( 'NONE',  ( 199.7528798840209276, 284.2810620923601164, 16.93803948313987817 ) ) ;
#42953 = CARTESIAN_POINT ( 'NONE',  ( 128.2389901622930495, 244.8458772461660544, 9.188101187500095079 ) ) ;
#42955 = DIRECTION ( 'NONE',  ( 0.000000000000000000, 0.000000000000000000, 1.000000000000000000 ) ) ;
#42956 = ORIENTED_EDGE ( 'NONE', *, *, #85085, .T. ) ;
#42957 = CARTESIAN_POINT ( 'NONE',  ( 204.8109598484962532, 275.9040069258922472, 13.12942483889034762 ) ) ;
#42958 = CARTESIAN_POINT ( 'NONE',  ( 54.58172535260923297, 208.9865022471903160, 10.00000000000009415 ) ) ;
#42959 = ADVANCED_FACE ( 'NONE', ( #63870 ), #10680, .T. ) ;
#42960 = CARTESIAN_POINT ( 'NONE',  ( 82.21456097586059286, 40.60959159724548329, -3.238575740498558897 ) ) ;
#42961 = CARTESIAN_POINT ( 'NONE',  ( 191.8644938906121808, 271.7084166993448662, 14.16934409235493320 ) ) ;
#42962 = CARTESIAN_POINT ( 'NONE',  ( 123.2062803672525604, 230.3932355074535394, -2.679491924311248496 ) ) ;
#42963 = DIRECTION ( 'NONE',  ( -0.8660254037844387076, -0.4999999999999998890, -0.000000000000000000 ) ) ;
#42964 = CARTESIAN_POINT ( 'NONE',  ( 82.57296292288040718, 40.92493348698932465, -3.680003806365853336 ) ) ;
#42965 = FACE_OUTER_BOUND ( 'NONE', #4946, .T. ) ;
#42966 = ADVANCED_FACE ( 'NONE', ( #88732 ), #88233, .T. ) ;
#42967 = CARTESIAN_POINT ( 'NONE',  ( 200.7523954295751594, 282.9336467052548869, 18.23634913067694185 ) ) ;
#42968 = CARTESIAN_POINT ( 'NONE',  ( 206.6509060984486155, 272.1412184117673974, 7.097787738138362279 ) ) ;
#42969 = CARTESIAN_POINT ( 'NONE',  ( 159.8188415394622268, 253.8326417772889840, -15.43862849427313222 ) ) ;
#42970 = LINE ( 'NONE', #29793, #22434 ) ;
#42971 = CARTESIAN_POINT ( 'NONE',  ( -10.31836507581447471, 176.3967562850347406, -4.648177544792955347E-16 ) ) ;
#42972 = EDGE_CURVE ( 'NONE', #28914, #34378, #19302, .T. ) ;
#42973 = EDGE_CURVE ( 'NONE', #15205, #85879, #73481, .T. ) ;
#42975 = EDGE_CURVE ( 'NONE', #4228, #63881, #21496, .T. ) ;
#42974 = VECTOR ( 'NONE', #31518, 1000.000000000000000 ) ;
#42976 = CARTESIAN_POINT ( 'NONE',  ( 72.06748121909076588, 71.10123967445895232, -5.802816214387736871 ) ) ;
#42978 = CARTESIAN_POINT ( 'NONE',  ( 185.3757608622346709, 266.4090302586452594, 13.11668907775444204 ) ) ;
#42977 = CARTESIAN_POINT ( 'NONE',  ( 73.41259731428677071, 70.10201033320841191, -9.453773877498623079 ) ) ;
#42979 = EDGE_CURVE ( 'NONE', #89111, #47191, #97250, .T. ) ;
#42980 = CARTESIAN_POINT ( 'NONE',  ( 68.87660500748863512, 222.1199935810940929, 2.679491924311251605 ) ) ;
#42981 = CARTESIAN_POINT ( 'NONE',  ( 41.98277471387834225, 25.20801979619931998, -3.090169943749474069 ) ) ;
#42982 = CARTESIAN_POINT ( 'NONE',  ( 149.7318359886737937, 272.2261244477465993, -11.42674851380234813 ) ) ;
#42983 = LINE ( 'NONE', #4506, #83281 ) ;
#42984 = CARTESIAN_POINT ( 'NONE',  ( 157.6161041218087746, 270.9124938997304639, -14.78071789165227834 ) ) ;
#42985 = AXIS2_PLACEMENT_3D ( 'NONE', #59145, #11603, #82023 ) ;
#42986 = CARTESIAN_POINT ( 'NONE',  ( 85.26069992303990830, 43.42143465718991280, -5.099252233888901920 ) ) ;
#42987 = B_SPLINE_CURVE_WITH_KNOTS ( 'NONE', 3,
 ( #22890, #62375, #84738, #15279 ),
 .UNSPECIFIED., .F., .F.,
 ( 4, 4 ),
 ( 0.02551283278911079672, 0.03475741272028291112 ),
 .UNSPECIFIED. ) ;
#42988 = CARTESIAN_POINT ( 'NONE',  ( 7.238742955462222461, 184.1744531367911293, 4.594050593750047540 ) ) ;
#42989 = CARTESIAN_POINT ( 'NONE',  ( 41.64315915125185086, 206.3967562850347122, -4.648177544792955347E-16 ) ) ;
#42990 = ORIENTED_EDGE ( 'NONE', *, *, #9051, .T. ) ;
#42991 = CARTESIAN_POINT ( 'NONE',  ( 87.15721324309708962, 46.06501070407752252, 8.877681887861816890 ) ) ;
#42992 = CARTESIAN_POINT ( 'NONE',  ( 18.79197634579341525, 22.80066082961421614, 10.00000000000000533 ) ) ;
#42993 = CARTESIAN_POINT ( 'NONE',  ( 37.37984742713354791, 29.78052372038643369, -10.00000000000000355 ) ) ;
#42994 = CARTESIAN_POINT ( 'NONE',  ( 35.46636587765004123, 179.0327760586659736, 1.948934522072302763E-15 ) ) ;
#42995 = CARTESIAN_POINT ( 'NONE',  ( 87.25346308258933448, 46.04525953206349698, 8.773708642049088624 ) ) ;
#42996 = CARTESIAN_POINT ( 'NONE',  ( 174.6041121390431670, 289.2630556414907801, 7.804972839359269443 ) ) ;
#42997 = CARTESIAN_POINT ( 'NONE',  ( 190.3286155001717930, 300.9881631498979004, -5.624828231725103045 ) ) ;
#42998 = CARTESIAN_POINT ( 'NONE',  ( 43.01983786573178037, 33.03677371833806120, 10.00000000000000533 ) ) ;
#42999 = CARTESIAN_POINT ( 'NONE',  ( 203.1203444092346899, 269.7784739467876420, -7.400015971792329061 ) ) ;
#43000 = CARTESIAN_POINT ( 'NONE',  ( 146.5913834600193582, 276.7432712258716947, -0.4909717733184599253 ) ) ;
#43001 = AXIS2_PLACEMENT_3D ( 'NONE', #20693, #72921, #3512 ) ;
#43002 = DIRECTION ( 'NONE',  ( 0.9979227057047517224, -0.06442261589618512863, 0.000000000000000000 ) ) ;
#43003 = CARTESIAN_POINT ( 'NONE',  ( 147.8791740781505837, 276.5127524457575987, 2.771564245682613947 ) ) ;
#43004 = DIRECTION ( 'NONE',  ( 0.000000000000000000, 0.000000000000000000, 1.000000000000000000 ) ) ;
#43005 = DIRECTION ( 'NONE',  ( -0.9598361373656995044, 0.2805612043866617111, 0.000000000000000000 ) ) ;
#43006 = VECTOR ( 'NONE', #58444, 1000.000000000000114 ) ;
#43007 = CARTESIAN_POINT ( 'NONE',  ( 160.8891438268352374, 281.0495864612497599, 9.578199528566821996 ) ) ;
#43008 = CARTESIAN_POINT ( 'NONE',  ( 75.87151652897667020, 224.6115022471903160, -5.000000000000047962 ) ) ;
#43009 = CYLINDRICAL_SURFACE ( 'NONE', #53861, 16.60714546451156792 ) ;
#43010 = CARTESIAN_POINT ( 'NONE',  ( 162.0192538899617318, 268.0510789565263394, -17.53028463913764057 ) ) ;
#43011 = ORIENTED_EDGE ( 'NONE', *, *, #33898, .T. ) ;
#43012 = CARTESIAN_POINT ( 'NONE',  ( 59.93088934303040816, 217.6589784336661637, -6.496448406907675876E-16 ) ) ;
#43013 = ORIENTED_EDGE ( 'NONE', *, *, #38335, .F. ) ;
#43014 = CARTESIAN_POINT ( 'NONE',  ( 162.8839417982861448, 263.3994626277539055, 17.77684832337497767 ) ) ;
#43015 = CARTESIAN_POINT ( 'NONE',  ( 146.8358616138309571, 276.3198226421291679, 4.054088818585255716 ) ) ;
#43016 = CARTESIAN_POINT ( 'NONE',  ( 67.26473598584114200, 66.56549206475087033, -8.572050621364043721 ) ) ;
#43017 = VERTEX_POINT ( 'NONE', #44541 ) ;
#43018 = CARTESIAN_POINT ( 'NONE',  ( 167.5553568848317525, 285.0228605941855449, 7.731127579155963048 ) ) ;
#43019 = CARTESIAN_POINT ( 'NONE',  ( 164.2672861321391053, 246.1277097281173667, -2.417001679502223777 ) ) ;
#43020 = CARTESIAN_POINT ( 'NONE',  ( 188.9122134955663910, 290.7695941481946988, -15.11888497690123678 ) ) ;
#43021 = CARTESIAN_POINT ( 'NONE',  ( 30.18562306610639112, 29.37878583063842441, 9.188101187500006262 ) ) ;
#43022 = CARTESIAN_POINT ( 'NONE',  ( 189.2086094880577889, 265.3749622005305469, 10.54437259076535227 ) ) ;
#43023 = CARTESIAN_POINT ( 'NONE',  ( 86.52710474712628752, 47.22253658430707901, -10.13945441009946968 ) ) ;
#43024 = CARTESIAN_POINT ( 'NONE',  ( 171.3037854771465618, 255.8038501838435934, 11.58489188490385224 ) ) ;
#43025 = ORIENTED_EDGE ( 'NONE', *, *, #77665, .F. ) ;
#43026 = CARTESIAN_POINT ( 'NONE',  ( 9.708348802340269756, 27.64646525600388571, -2.839279412974133887 ) ) ;
#43027 = CARTESIAN_POINT ( 'NONE',  ( 31.15319227796116053, 18.39040679176984128, -6.890680421881970419E-14 ) ) ;
#43028 = CARTESIAN_POINT ( 'NONE',  ( 22.68312297988245163, 177.2365022471902023, -10.00000000000009237 ) ) ;
#43029 = CARTESIAN_POINT ( 'NONE',  ( 30.34687108590970794, 93.06504152958497400, 25.00000000000000000 ) ) ;
#43030 = VERTEX_POINT ( 'NONE', #75990 ) ;
#43031 = CARTESIAN_POINT ( 'NONE',  ( 26.96143514339544467, 174.8262482093457777, 3.021315404115420679E-15 ) ) ;
#43032 = CARTESIAN_POINT ( 'NONE',  ( 167.2952297142404632, 261.5110431333442307, 16.99354490899708381 ) ) ;
#43033 = CARTESIAN_POINT ( 'NONE',  ( 76.67567146729665239, 63.34086528488000312, -15.41964329106466103 ) ) ;
#43034 = ORIENTED_EDGE ( 'NONE', *, *, #45353, .T. ) ;
#43035 = ORIENTED_EDGE ( 'NONE', *, *, #100167, .T. ) ;
#43037 = CARTESIAN_POINT ( 'NONE',  ( -19.65312891409030271, 93.06504152958497400, 10.00000000000000888 ) ) ;
#43036 = CARTESIAN_POINT ( 'NONE',  ( 207.8996209429610360, 270.5542889829179103, -5.987818313449536411 ) ) ;
#43038 = CARTESIAN_POINT ( 'NONE',  ( 149.0203866098534888, 272.5361143586139860, -12.73049804737905255 ) ) ;
#43039 = ORIENTED_EDGE ( 'NONE', *, *, #44744, .T. ) ;
#43040 = CARTESIAN_POINT ( 'NONE',  ( 66.11215637706905568, 68.56181850691201873, -2.272870840636120882 ) ) ;
#43041 = DIRECTION ( 'NONE',  ( -0.8600446134263898257, -0.5102188382608503492, 0.000000000000000000 ) ) ;
#43042 = DIRECTION ( 'NONE',  ( -0.000000000000000000, -0.000000000000000000, -1.000000000000000000 ) ) ;
#43043 = CARTESIAN_POINT ( 'NONE',  ( 78.30529379001707468, 61.64230706715306241, -15.78713534414099051 ) ) ;
#43044 = CARTESIAN_POINT ( 'NONE',  ( 72.13964350835141204, 72.31942673879332517, -1.245071394591160674 ) ) ;
#43046 = ADVANCED_FACE ( 'NONE', ( #99275 ), #90717, .T. ) ;
#43045 = CARTESIAN_POINT ( 'NONE',  ( 112.1907172202364080, 226.3923013555410080, 4.594050593750050204 ) ) ;
#43047 = CARTESIAN_POINT ( 'NONE',  ( 204.8284483594339065, 275.8737159363993214, 14.69997973035875383 ) ) ;
#43048 = DIRECTION ( 'NONE',  ( 0.4999999999999998890, -0.8660254037844385966, 0.000000000000000000 ) ) ;
#43049 = ORIENTED_EDGE ( 'NONE', *, *, #44948, .T. ) ;
#43050 = CARTESIAN_POINT ( 'NONE',  ( 163.8111161534324935, 246.9178193081252743, -7.110480325054721717 ) ) ;
#43051 = VERTEX_POINT ( 'NONE', #5073 ) ;
#43052 = CARTESIAN_POINT ( 'NONE',  ( 34.51575008502857855, 31.87878583063843863, -9.188101187500006262 ) ) ;
#43053 = FACE_OUTER_BOUND ( 'NONE', #32757, .T. ) ;
#43054 = CARTESIAN_POINT ( 'NONE',  ( 75.23976045582850247, 66.94057334133056258, -12.81464017275781941 ) ) ;
#43055 = CARTESIAN_POINT ( 'NONE',  ( 73.24602992621615272, 225.3464784336661353, 1.353441290958777525E-15 ) ) ;
#43056 = VERTEX_POINT ( 'NONE', #51672 ) ;
#43057 = EDGE_CURVE ( 'NONE', #8187, #68859, #74980, .T. ) ;
#43058 = CARTESIAN_POINT ( 'NONE',  ( 170.5993847053230468, 287.8722104901659691, 7.679145147933459370 ) ) ;
#43059 =( BOUNDED_CURVE ( )  B_SPLINE_CURVE ( 2, ( #35832, #34823, #90589, #4433, #11560, #81478, #12051, #21635, #89113, #5440, #42903, #36323, #96680 ),
 .UNSPECIFIED., .F., .T. ) 
 B_SPLINE_CURVE_WITH_KNOTS ( ( 3, 2, 2, 2, 2, 2, 3 ),
 ( 0.01250000000000000069, 0.01499999999999999944, 0.02000000000000000042, 0.02500000000000000139, 0.02999999999999999889, 0.03500000000000000333, 0.03750000000000000555 ),
 .UNSPECIFIED. ) 
 CURVE ( )  GEOMETRIC_REPRESENTATION_ITEM ( )  RATIONAL_B_SPLINE_CURVE ( ( 0.9755282581475768211, 0.9755282581475768211, 1.000000000000000000, 0.9510565162951535312, 1.000000000000000000, 0.9510565162951535312, 1.000000000000000000, 0.9510565162951535312, 1.000000000000000000, 0.9510565162951535312, 1.000000000000000000, 0.9755282581475767101, 0.9755282581475768211 ) ) 
 REPRESENTATION_ITEM ( '' )  );
#43060 = CARTESIAN_POINT ( 'NONE',  ( 81.66071111044179531, 55.73219010195405332, 16.34934455148813370 ) ) ;
#43061 = CARTESIAN_POINT ( 'NONE',  ( 198.4688822609874137, 286.8888075330012839, 18.53129255230862071 ) ) ;
#43062 = VECTOR ( 'NONE', #84365, 1000.000000000000000 ) ;
#43063 = CARTESIAN_POINT ( 'NONE',  ( 172.1403850395635118, 276.9566470737562440, 16.52013608218327079 ) ) ;
#43064 = EDGE_CURVE ( 'NONE', #97421, #24006, #78272, .T. ) ;
#43065 = ORIENTED_EDGE ( 'NONE', *, *, #93329, .F. ) ;
#43066 = CARTESIAN_POINT ( 'NONE',  ( 75.00750624606230588, 62.98958700368800834, -14.74961995160845163 ) ) ;
#43067 = CARTESIAN_POINT ( 'NONE',  ( 66.06012914866342101, 68.52786067758134436, -4.567821539730282154 ) ) ;
#43068 = ORIENTED_EDGE ( 'NONE', *, *, #73876, .T. ) ;
#43069 = CARTESIAN_POINT ( 'NONE',  ( 195.5000684248051073, 292.0309439354826964, 16.15209601369885206 ) ) ;
#43070 = DIRECTION ( 'NONE',  ( -0.5609510170580174204, -0.8278489937552475642, 0.000000000000000000 ) ) ;
#43071 = CARTESIAN_POINT ( 'NONE',  ( 207.1432938686257046, 271.8642859028066141, -6.405155839440290322 ) ) ;
#43072 = CARTESIAN_POINT ( 'NONE',  ( -19.60980644863471412, 92.92999745296690151, 59.99999999999999289 ) ) ;
#43073 = CARTESIAN_POINT ( 'NONE',  ( 80.57137527226012708, 55.64701761767596366, 16.43878515310709787 ) ) ;
#43074 = DIRECTION ( 'NONE',  ( -0.8660254037844384856, -0.5000000000000002220, 5.782411586589354927E-17 ) ) ;
#43075 = CARTESIAN_POINT ( 'NONE',  ( 205.9642072045669465, 273.9065239114831911, 10.22128930895731536 ) ) ;
#43076 = CARTESIAN_POINT ( 'NONE',  ( 125.9182562534771677, 255.0530062829863311, -4.648177544792955347E-16 ) ) ;
#43077 = ORIENTED_EDGE ( 'NONE', *, *, #88198, .F. ) ;
#43078 = CARTESIAN_POINT ( 'NONE',  ( 207.8725590214046406, 270.6011616060040410, 1.988011721677743093 ) ) ;
#43079 = CARTESIAN_POINT ( 'NONE',  ( 126.7237928014352804, 231.7202760586659736, -5.415160957724236172E-17 ) ) ;
#43080 = ORIENTED_EDGE ( 'NONE', *, *, #77016, .T. ) ;
#43081 = AXIS2_PLACEMENT_3D ( 'NONE', #38754, #62038, #51983 ) ;
#43082 = DIRECTION ( 'NONE',  ( -0.000000000000000000, -0.000000000000000000, -1.000000000000000000 ) ) ;
#43083 = CARTESIAN_POINT ( 'NONE',  ( 81.98739982517574276, 58.71797656568649870, -0.08682408883346368067 ) ) ;
#43084 = CARTESIAN_POINT ( 'NONE',  ( 205.8889072768004951, 273.5716727396786041, -9.812782715980612025 ) ) ;
#43085 = CARTESIAN_POINT ( 'NONE',  ( 164.2712161151136172, 246.1209027979328710, 7.276091357954241445 ) ) ;
#43086 = CARTESIAN_POINT ( 'NONE',  ( 74.84842711207834043, 61.45602019284894624, 15.25606177542201536 ) ) ;
#43087 = FACE_OUTER_BOUND ( 'NONE', #99267, .T. ) ;
#43088 = VERTEX_POINT ( 'NONE', #29858 ) ;
#43089 = CARTESIAN_POINT ( 'NONE',  ( 76.99493330467112173, 57.26266963217694439, 16.17658719691544889 ) ) ;
#43090 = CARTESIAN_POINT ( 'NONE',  ( 182.2429953966146172, 275.8324561883076171, -16.43557028755543215 ) ) ;
#43091 = EDGE_CURVE ( 'NONE', #32489, #16870, #91236, .T. ) ;
#43092 = CARTESIAN_POINT ( 'NONE',  ( 166.9253229281109157, 248.7550762113961582, -5.490293681429817774 ) ) ;
#43093 = CARTESIAN_POINT ( 'NONE',  ( 0.07393976959879319799, 182.3967562850347406, 2.649461200531984646E-14 ) ) ;
#43094 = CARTESIAN_POINT ( 'NONE',  ( 30.24280306353613312, 198.2677522451419350, -5.000000000000047962 ) ) ;
#43095 = CARTESIAN_POINT ( 'NONE',  ( 73.51948839908328637, 69.73627507762921596, -9.361350578256052657 ) ) ;
#43096 = CARTESIAN_POINT ( 'NONE',  ( 190.3286155001717930, 300.9881631498979004, -5.624828231725103045 ) ) ;
#43097 = ADVANCED_FACE ( 'NONE', ( #13668 ), #91195, .T. ) ;
#43098 = CARTESIAN_POINT ( 'NONE',  ( 70.10062891805684160, 70.95873945766187774, 2.129561960066722826 ) ) ;
#43099 = CARTESIAN_POINT ( 'NONE',  ( 170.8035993136612376, 250.5442460706725569, 3.418796778386401947 ) ) ;
#43100 = EDGE_CURVE ( 'NONE', #40576, #34323, #82116, .T. ) ;
#43101 = CARTESIAN_POINT ( 'NONE',  ( 20.25339421822757302, 23.64441083166260782, -10.00000000000000533 ) ) ;
#43102 = CARTESIAN_POINT ( 'NONE',  ( 149.6071296322179194, 271.5198456328920997, 12.75640156477042453 ) ) ;
#43103 = CARTESIAN_POINT ( 'NONE',  ( -22.42236680055709641, 157.8615022471902591, 0.000000000000000000 ) ) ;
#43104 = CARTESIAN_POINT ( 'NONE',  ( 169.0232266158229208, 285.7259705221371746, -9.141046413429966933 ) ) ;
#43105 = CARTESIAN_POINT ( 'NONE',  ( 159.4574711498080433, 254.4585536525209477, 16.86100557095418395 ) ) ;
#43106 = CARTESIAN_POINT ( 'NONE',  ( 193.1232865735839539, 289.3006304592061610, 16.37785481887425476 ) ) ;
#43107 = CARTESIAN_POINT ( 'NONE',  ( 131.5677753063154682, 256.7677522451419350, -5.000000000000047962 ) ) ;
#43108 = CARTESIAN_POINT ( 'NONE',  ( 183.3171886181362140, 279.0376548180590817, 17.18391320931595345 ) ) ;
#43109 = ORIENTED_EDGE ( 'NONE', *, *, #94976, .T. ) ;
#43110 = CARTESIAN_POINT ( 'NONE',  ( 157.6286460899086137, 257.6261715744221306, 18.25526781158026779 ) ) ;
#43111 = CARTESIAN_POINT ( 'NONE',  ( 198.5970767652345899, 286.6667681383942181, -17.17073100918929640 ) ) ;
#43112 = CARTESIAN_POINT ( 'NONE',  ( -12.05712525078605069, 163.8458772461660544, 9.188101187500095079 ) ) ;
#43113 = AXIS2_PLACEMENT_3D ( 'NONE', #6581, #76960, #76003 ) ;
#43114 = CARTESIAN_POINT ( 'NONE',  ( 56.95444766116892055, 197.5643266524159856, -9.188101187500093303 ) ) ;
#43115 = CARTESIAN_POINT ( 'NONE',  ( 178.0613071443478930, 258.8060421996208902, -10.32626121482724102 ) ) ;
#43116 = CARTESIAN_POINT ( 'NONE',  ( 17.41189581114303309, 28.79103043416549212, 8.090169943749478065 ) ) ;
#43117 = CARTESIAN_POINT ( 'NONE',  ( 85.60773205244574058, 48.97959825543787105, 12.21184514131274312 ) ) ;
#43118 = CARTESIAN_POINT ( 'NONE',  ( 157.8719920515997046, 257.2046840049564480, -17.69857783492101433 ) ) ;
#43120 = VECTOR ( 'NONE', #72993, 1000.000000000000000 ) ;
#43119 = DIRECTION ( 'NONE',  ( 0.8660254037844382635, 0.5000000000000004441, 0.000000000000000000 ) ) ;
#43121 = CARTESIAN_POINT ( 'NONE',  ( -19.65312891409030271, 93.06504152958497400, 10.00000000000000000 ) ) ;
#43122 = CARTESIAN_POINT ( 'NONE',  ( 73.78934571132764120, 55.49050343092449111, -16.58731856350070899 ) ) ;
#43124 = CARTESIAN_POINT ( 'NONE',  ( 68.70876474829496772, 217.1427522451419065, 10.00000000000009237 ) ) ;
#43123 = CARTESIAN_POINT ( 'NONE',  ( 174.9671601572613326, 281.6994072225486434, -15.63500919100072473 ) ) ;
#43125 = CARTESIAN_POINT ( 'NONE',  ( 74.95743781794847393, 67.19740583228991682, 12.53491114478569912 ) ) ;
#43126 = DIRECTION ( 'NONE',  ( 0.8660254037844399289, 0.4999999999999976130, -0.000000000000000000 ) ) ;
#43127 = CARTESIAN_POINT ( 'NONE',  ( 198.4688822609874137, 286.8888075330012839, 18.53129255230862071 ) ) ;
#43128 = VECTOR ( 'NONE', #91595, 1000.000000000000000 ) ;
#43129 = CARTESIAN_POINT ( 'NONE',  ( 179.1040650366922193, 294.2007529456641919, 1.056493710678918729 ) ) ;
#43130 = CARTESIAN_POINT ( 'NONE',  ( 41.66351307949141614, 184.8615022471902023, 5.000000000000051514 ) ) ;
#43131 = CARTESIAN_POINT ( 'NONE',  ( 183.6907499062894260, 292.8494268563325136, 9.428801131153548454 ) ) ;
#43132 = CARTESIAN_POINT ( 'NONE',  ( 163.2437751800324293, 247.9004826992694461, 9.806027032984305336 ) ) ;
#43133 = CARTESIAN_POINT ( 'NONE',  ( -2.801652295722365071, 175.3149278399160949, -9.188101187500095079 ) ) ;
#43134 = CARTESIAN_POINT ( 'NONE',  ( 167.5854134468545169, 285.9299511827676383, 4.087413415166947672 ) ) ;
#43135 = ADVANCED_FACE ( 'NONE', ( #35954 ), #91690, .T. ) ;
#43136 = CARTESIAN_POINT ( 'NONE',  ( 78.98991491668435572, 60.09931805977702624, 16.11723901038370244 ) ) ;
#43137 = CARTESIAN_POINT ( 'NONE',  ( 36.57256041901661803, 33.06628583063844928, -9.188101187500006262 ) ) ;
#43138 = CARTESIAN_POINT ( 'NONE',  ( 27.35777070392073185, 16.76426979415090557, 3.090169943749476733 ) ) ;
#43139 = CARTESIAN_POINT ( 'NONE',  ( 179.9113681451759135, 276.9646501146019659, 16.30242976572636238 ) ) ;
#43140 = CARTESIAN_POINT ( 'NONE',  ( 193.7901930790854976, 294.9925349088783264, 14.24765323155741115 ) ) ;
#43141 = FACE_OUTER_BOUND ( 'NONE', #35660, .T. ) ;
#43142 = CARTESIAN_POINT ( 'NONE',  ( 141.9699493749754140, 259.7505386000626686, -7.968025677899344572 ) ) ;
#43143 = SHAPE_DEFINITION_REPRESENTATION ( #2227, #7571 ) ;
#43144 = CARTESIAN_POINT ( 'NONE',  ( 17.90851666933368236, 18.84335787977762777, 9.188101187500006262 ) ) ;
#43145 = CARTESIAN_POINT ( 'NONE',  ( 71.57943482431291216, 72.41997303871664826, 0.9858917062509064966 ) ) ;
#43146 = CARTESIAN_POINT ( 'NONE',  ( 82.33565291927013163, 54.25759526660485932, 15.62409434222757376 ) ) ;
#43147 = CARTESIAN_POINT ( 'NONE',  ( 159.1565304511513546, 259.4205487488260360, 16.68562774920905056 ) ) ;
#43148 = DIRECTION ( 'NONE',  ( 0.4827766168686586368, 0.5834231310750571664, 0.6531035050674810494 ) ) ;
#43149 = VERTEX_POINT ( 'NONE', #44040 ) ;
#43150 = VECTOR ( 'NONE', #18938, 1000.000000000000000 ) ;
#43151 = CARTESIAN_POINT ( 'NONE',  ( 156.3599523370786244, 276.2775748563693696, 10.27199958061185114 ) ) ;
#43152 = LINE ( 'NONE', #57874, #35942 ) ;
#43153 = CARTESIAN_POINT ( 'NONE',  ( 160.0166746459236435, 283.6086068001695253, 2.232576205374148248 ) ) ;
#43154 = VERTEX_POINT ( 'NONE', #60728 ) ;
#43155 = CARTESIAN_POINT ( 'NONE',  ( 192.8132846206021611, 296.6845899933152850, 11.53748932578252351 ) ) ;
#43156 = CARTESIAN_POINT ( 'NONE',  ( 70.33802287992277513, 222.9637435831424739, 2.679491924311251605 ) ) ;
#43157 = AXIS2_PLACEMENT_3D ( 'NONE', #70719, #22129, #45901 ) ;
#43158 = CARTESIAN_POINT ( 'NONE',  ( 66.61276649528306848, 68.27696284464261112, 4.555325784153476221 ) ) ;
#43159 = CARTESIAN_POINT ( 'NONE',  ( 124.0080952226617796, 235.7365022471901739, -10.00000000000009237 ) ) ;
#43160 = VERTEX_POINT ( 'NONE', #52642 ) ;
#43161 = ORIENTED_EDGE ( 'NONE', *, *, #72896, .F. ) ;
#43163 = DIRECTION ( 'NONE',  ( 0.000000000000000000, 0.000000000000000000, 1.000000000000000000 ) ) ;
#43162 = LINE ( 'NONE', #45653, #94025 ) ;
#43164 = CARTESIAN_POINT ( 'NONE',  ( 153.4242699508872647, 264.9083646613370320, 16.62000820703435267 ) ) ;
#43165 = VERTEX_POINT ( 'NONE', #66856 ) ;
#43166 = CARTESIAN_POINT ( 'NONE',  ( 190.8443993347725325, 300.0947993426467519, 8.522468760355437212 ) ) ;
#43167 = CARTESIAN_POINT ( 'NONE',  ( 80.28516836418320679, 58.07801345963574846, 16.26295356561165661 ) ) ;
#43168 = CARTESIAN_POINT ( 'NONE',  ( 174.3516257938615865, 262.5322562012714798, 15.40078459836708547 ) ) ;
#43169 = VERTEX_POINT ( 'NONE', #97785 ) ;
#43170 = CARTESIAN_POINT ( 'NONE',  ( 78.19646929978586058, 61.02229919570467587, -15.90908970393073396 ) ) ;
#43171 = CARTESIAN_POINT ( 'NONE',  ( 88.45958475239287111, 43.85926912372239883, -0.5941283661710258235 ) ) ;
#43172 = EDGE_CURVE ( 'NONE', #52670, #38281, #81554, .T. ) ;
#43173 = CARTESIAN_POINT ( 'NONE',  ( 80.77763420391843852, 43.45617620844090112, 9.404609412801525181 ) ) ;
#43174 = VERTEX_POINT ( 'NONE', #68350 ) ;
#43175 = CARTESIAN_POINT ( 'NONE',  ( 175.6563521628115438, 268.5095984484888731, 16.17594149762453171 ) ) ;
#43176 = CARTESIAN_POINT ( 'NONE',  ( 168.8056409514728102, 275.8157205250771540, -15.38912072102792905 ) ) ;
#43177 = B_SPLINE_CURVE_WITH_KNOTS ( 'NONE', 3,
 ( #70579, #17383, #63486, #85858, #16880, #24484, #94927, #17905, #16384, #26498, #32072, #39656, #1194, #62984 ),
 .UNSPECIFIED., .F., .F.,
 ( 4, 2, 2, 2, 2, 2, 4 ),
 ( 2.907926436840383405E-17, 0.0005042492132239927323, 0.001008498426447956408, 0.001260623033059940631, 0.001512747639671924637, 0.001764872246283908860, 0.002016996852895892867 ),
 .UNSPECIFIED. ) ;
#43178 = CARTESIAN_POINT ( 'NONE',  ( 73.41744195450526433, 58.55286001146748731, 15.72156431111986663 ) ) ;
#43179 = ORIENTED_EDGE ( 'NONE', *, *, #917, .T. ) ;
#43180 = CARTESIAN_POINT ( 'NONE',  ( 174.3697573357644899, 277.1653490889620457, -17.12727634137145571 ) ) ;
#43181 = CARTESIAN_POINT ( 'NONE',  ( 169.8694959362524628, 262.1277198426760151, -15.72963479151413502 ) ) ;
#43182 = VERTEX_POINT ( 'NONE', #22253 ) ;
#43183 = EDGE_CURVE ( 'NONE', #48909, #63370, #75097, .T. ) ;
#43184 = B_SPLINE_CURVE_WITH_KNOTS ( 'NONE', 3,
 ( #74972, #51660, #28860, #22243, #28344, #61234 ),
 .UNSPECIFIED., .F., .F.,
 ( 4, 2, 4 ),
 ( 0.01996523517852847110, 0.02451540668050315036, 0.02906557818247782615 ),
 .UNSPECIFIED. ) ;
#43185 = CARTESIAN_POINT ( 'NONE',  ( 160.3724000868533324, 268.8946452163862659, -16.80276685773084822 ) ) ;
#43186 = ORIENTED_EDGE ( 'NONE', *, *, #12730, .T. ) ;
#43187 = EDGE_CURVE ( 'NONE', #68818, #46791, #37818, .T. ) ;
#43188 = DIRECTION ( 'NONE',  ( -1.000000000000000000, 0.000000000000000000, 0.000000000000000000 ) ) ;
#43189 = VERTEX_POINT ( 'NONE', #20278 ) ;
#43190 = CARTESIAN_POINT ( 'NONE',  ( 73.05912352472130067, 69.60491006942920933, 9.219028434792550186 ) ) ;
#43191 = PLANE ( 'NONE',  #73577 ) ;
#43192 = CARTESIAN_POINT ( 'NONE',  ( 80.66987298107778770, 24.99999999999998579, 59.99999999999999289 ) ) ;
#43193 = CARTESIAN_POINT ( 'NONE',  ( 11.06379537489605802, 28.16126292948894161, -6.180339887498951690 ) ) ;
#43194 = CARTESIAN_POINT ( 'NONE',  ( 157.2548874775783929, 258.6822847665750942, -16.83730550228635181 ) ) ;
#43195 = CARTESIAN_POINT ( 'NONE',  ( 162.7898368507877933, 277.9903003075606875, -13.67957419982492162 ) ) ;
#43196 = CARTESIAN_POINT ( 'NONE',  ( 197.2241483131352027, 289.0447499725873399, -16.69872125311100319 ) ) ;
#43197 = ORIENTED_EDGE ( 'NONE', *, *, #89907, .T. ) ;
#43198 = CARTESIAN_POINT ( 'NONE',  ( 66.52392041426838887, 68.84470833973988135, -4.415679280545953489 ) ) ;
#43199 = VECTOR ( 'NONE', #30531, 1000.000000000000000 ) ;
#43200 = CARTESIAN_POINT ( 'NONE',  ( 206.5117639185820906, 272.9581278627833285, 11.28485531511759099 ) ) ;
#43202 = CARTESIAN_POINT ( 'NONE',  ( 206.5280879940269756, 272.9298537347264642, 11.21709153681466731 ) ) ;
#43201 = CARTESIAN_POINT ( 'NONE',  ( 149.4456112649506281, 271.7996036513546869, -12.95648166494593667 ) ) ;
#43204 = EDGE_LOOP ( 'NONE', ( #54242, #96259, #327, #82523 ) ) ;
#43203 = CARTESIAN_POINT ( 'NONE',  ( 198.2819808855875863, 287.2125302111982705, 18.53535247371401695 ) ) ;
#43205 = VECTOR ( 'NONE', #13556, 1000.000000000000000 ) ;
#43206 = EDGE_LOOP ( 'NONE', ( #83400, #47770, #1584, #61013 ) ) ;
#43207 = CARTESIAN_POINT ( 'NONE',  ( 147.2227856845451583, 275.6496504929807543, -2.633553040037199366 ) ) ;
#43208 = CARTESIAN_POINT ( 'NONE',  ( 171.5754110937450889, 259.5470102351253558, -13.93953539574996725 ) ) ;
#43209 = CARTESIAN_POINT ( 'NONE',  ( 164.2961018905060087, 247.3365041451504851, 7.253309886448856325 ) ) ;
#43210 = CARTESIAN_POINT ( 'NONE',  ( -19.65312891409030271, 93.06504152958497400, 59.99999999999999289 ) ) ;
#43211 = B_SPLINE_CURVE_WITH_KNOTS ( 'NONE', 3,
 ( #50639, #57241, #35939, #11672 ),
 .UNSPECIFIED., .F., .F.,
 ( 4, 4 ),
 ( 0.001999640796707240990, 0.007335658808800400027 ),
 .UNSPECIFIED. ) ;
#43212 = CARTESIAN_POINT ( 'NONE',  ( 160.1153909744335806, 253.3190030889627735, -14.69843286118399561 ) ) ;
#43213 = CARTESIAN_POINT ( 'NONE',  ( 148.2043552425267876, 273.9495221473935089, -8.865305688972465958 ) ) ;
#43214 = ORIENTED_EDGE ( 'NONE', *, *, #84637, .F. ) ;
#43215 = CARTESIAN_POINT ( 'NONE',  ( 170.5758582599388262, 255.6247867453906224, -12.63526933594605950 ) ) ;
#43216 = VECTOR ( 'NONE', #88765, 1000.000000000000000 ) ;
#43217 = DIRECTION ( 'NONE',  ( 0.3358313672678264750, -0.9419221266957381600, 0.000000000000000000 ) ) ;
#43218 = ADVANCED_FACE ( 'NONE', ( #51152 ), #28355, .T. ) ;
#43219 = FACE_OUTER_BOUND ( 'NONE', #18471, .T. ) ;
#43220 = CARTESIAN_POINT ( 'NONE',  ( 206.9377610035629118, 272.2202792677204002, 7.440532334334675646 ) ) ;
#43221 = ADVANCED_FACE ( 'NONE', ( #459 ), #95886, .T. ) ;
#43222 = CARTESIAN_POINT ( 'NONE',  ( 23.81978131880152816, 197.8927522451419634, 2.944929066748280225E-16 ) ) ;
#43223 = CARTESIAN_POINT ( 'NONE',  ( 105.9931361504627745, 225.8768266524159856, -9.188101187500093303 ) ) ;
#43224 = CARTESIAN_POINT ( 'NONE',  ( 184.0101390881002033, 296.9595158201846630, -2.782362052833078359 ) ) ;
#43225 = CARTESIAN_POINT ( 'NONE',  ( -1.979643831746636495, 43.07307769237275608, 59.99999999999999289 ) ) ;
#43226 = CARTESIAN_POINT ( 'NONE',  ( 157.2464636617698375, 258.2881309577184652, 18.14284729738657731 ) ) ;
#43227 = CARTESIAN_POINT ( 'NONE',  ( 13.18854085237251539, 31.24736827225017777, -10.00000000000000000 ) ) ;
#43228 = CARTESIAN_POINT ( 'NONE',  ( 28.05084980986327281, 180.8768266524160140, -9.188101187500091527 ) ) ;
#43229 = CARTESIAN_POINT ( 'NONE',  ( 175.8939073520130592, 252.7054158260212375, 5.280091837693253964 ) ) ;
#43230 = ORIENTED_EDGE ( 'NONE', *, *, #63312, .T. ) ;
#43231 = AXIS2_PLACEMENT_3D ( 'NONE', #27425, #57799, #19348 ) ;
#43232 = VERTEX_POINT ( 'NONE', #2474 ) ;
#43233 = CARTESIAN_POINT ( 'NONE',  ( 74.17419530692131957, 68.61376803465689989, 11.49684454571890591 ) ) ;
#43234 = CARTESIAN_POINT ( 'NONE',  ( 147.5539660880823192, 275.8630805544623286, -0.6031081523752792606 ) ) ;
#43235 = CARTESIAN_POINT ( 'NONE',  ( -15.31269525828471068, 104.2312461070085021, 43.89948692389422291 ) ) ;
#43236 = CARTESIAN_POINT ( 'NONE',  ( 146.8358616138309571, 276.3198226421291679, 4.054088818585255716 ) ) ;
#43237 = CARTESIAN_POINT ( 'NONE',  ( 93.96857342517718337, 15.00000000000000000, 9.212605237762133470 ) ) ;
#43238 = CARTESIAN_POINT ( 'NONE',  ( 3.606438777009930430, 25.58029201028039523, 1.583844403245363353 ) ) ;
#43239 = CARTESIAN_POINT ( 'NONE',  ( 179.3912532575458272, 287.9620500955485340, -12.67217938249804732 ) ) ;
#43240 = CARTESIAN_POINT ( 'NONE',  ( 108.5224306304829582, 221.9155109091896350, 2.679491924311254714 ) ) ;
#43241 = VECTOR ( 'NONE', #79224, 1000.000000000000114 ) ;
#43242 = CARTESIAN_POINT ( 'NONE',  ( 50.26990084964904071, 190.6423013555410080, -4.594050593750043987 ) ) ;
#43243 = CARTESIAN_POINT ( 'NONE',  ( 94.68952686182812783, 232.1427522451419065, 10.00000000000009237 ) ) ;
#43244 = VERTEX_POINT ( 'NONE', #10064 ) ;
#43245 = CARTESIAN_POINT ( 'NONE',  ( 194.7749398255589881, 266.3361531225978069, -7.673830273753635467 ) ) ;
#43246 = CARTESIAN_POINT ( 'NONE',  ( 179.3989088880254030, 257.9931946406668430, -10.60009870068524052 ) ) ;
#43247 = CARTESIAN_POINT ( 'NONE',  ( 207.8136982414359579, 270.7031114674828700, -0.9536989003868096004 ) ) ;
#43248 = EDGE_CURVE ( 'NONE', #41972, #54771, #17149, .T. ) ;
#43249 = CARTESIAN_POINT ( 'NONE',  ( 6.102605256642664067, 165.1423013555410080, -4.594050593750043987 ) ) ;
#43250 = CARTESIAN_POINT ( 'NONE',  ( 151.4376533647338476, 268.3492855237141725, -15.16853828792834236 ) ) ;
#43251 = DIRECTION ( 'NONE',  ( 0.2398044646550214765, 0.9708212084269268738, 0.000000000000000000 ) ) ;
#43252 = CARTESIAN_POINT ( 'NONE',  ( 192.6789561813392595, 296.9172536750198219, -11.84591848451790952 ) ) ;
#43253 = CARTESIAN_POINT ( 'NONE',  ( 73.67129923898167476, 69.53774399045309451, 9.705214532217949497 ) ) ;
#43254 = CARTESIAN_POINT ( 'NONE',  ( 54.51857766514267212, 202.2833772461660828, -9.188101187500095079 ) ) ;
#43255 = CARTESIAN_POINT ( 'NONE',  ( 207.5792673731680793, 271.1091576421853233, 2.359198794924813214 ) ) ;
#43256 = CARTESIAN_POINT ( 'NONE',  ( 72.48613895716145805, 57.45971281110428919, 15.82031199903085472 ) ) ;
#43257 = CARTESIAN_POINT ( 'NONE',  ( 68.85652538089030372, 67.72390236607947145, 8.290076536751538328 ) ) ;
#43258 = DIRECTION ( 'NONE',  ( -0.000000000000000000, -0.000000000000000000, -1.000000000000000000 ) ) ;
#43259 = ORIENTED_EDGE ( 'NONE', *, *, #73526, .F. ) ;
#43260 = CARTESIAN_POINT ( 'NONE',  ( 208.3152833949211526, 269.8343404973242059, 2.763633873278860342 ) ) ;
#43261 = CARTESIAN_POINT ( 'NONE',  ( 1.898513289055925979, 165.2365022471902023, -10.00000000000009059 ) ) ;
#43262 = CARTESIAN_POINT ( 'NONE',  ( 84.85648000362951393, 46.82103691607230900, 11.23615365138597788 ) ) ;
#43263 = CARTESIAN_POINT ( 'NONE',  ( 117.0346129529493311, 244.5024278399160949, -9.188101187500093303 ) ) ;
#43264 = CARTESIAN_POINT ( 'NONE',  ( 18.86656744736070124, 32.93396525600390845, 2.839279412974139660 ) ) ;
#43265 = CARTESIAN_POINT ( 'NONE',  ( 164.2866824732684279, 246.0941142798005785, 1.717120327741293195 ) ) ;
#43266 = CARTESIAN_POINT ( 'NONE',  ( -32.30932376655839988, 25.48519649537503184, -10.00000000000000000 ) ) ;
#43268 = CARTESIAN_POINT ( 'NONE',  ( 189.5210412211111191, 289.6957050120914801, 15.52021532872637266 ) ) ;
#43267 = CARTESIAN_POINT ( 'NONE',  ( 48.29091023345865352, 82.53782597618220507, -10.00000000000000000 ) ) ;
#43269 = B_SPLINE_CURVE_WITH_KNOTS ( 'NONE', 3,
 ( #77025, #84674, #67943, #67433 ),
 .UNSPECIFIED., .F., .F.,
 ( 4, 4 ),
 ( 0.008266395780886143241, 0.01413511161970297005 ),
 .UNSPECIFIED. ) ;
#43270 = CARTESIAN_POINT ( 'NONE',  ( 150.3208749327335738, 270.2836025087354415, -14.97713178109939847 ) ) ;
#43271 = ORIENTED_EDGE ( 'NONE', *, *, #72412, .T. ) ;
#43272 = CARTESIAN_POINT ( 'NONE',  ( 190.8443993347725325, 300.0947993426467519, 8.522468760355437212 ) ) ;
#43273 = CARTESIAN_POINT ( 'NONE',  ( 163.8785059224672409, 246.8010968042466118, 7.414532662353326309 ) ) ;
#43274 = AXIS2_PLACEMENT_3D ( 'NONE', #33897, #86138, #9078 ) ;
#43275 = DIRECTION ( 'NONE',  ( -0.4330127018922203530, 0.7500000000000046629, 0.4999999999999919509 ) ) ;
#43276 = DIRECTION ( 'NONE',  ( -0.4245406647209920559, -0.9054088711727195093, 0.000000000000000000 ) ) ;
#43277 = CARTESIAN_POINT ( 'NONE',  ( 81.68773053310077614, 55.22504345363421407, -15.91572386494825508 ) ) ;
#43278 = ORIENTED_EDGE ( 'NONE', *, *, #36387, .F. ) ;
#43279 = CARTESIAN_POINT ( 'NONE',  ( 22.66956910419568061, 38.88013629349136835, 10.00000000000000000 ) ) ;
#43280 = AXIS2_PLACEMENT_3D ( 'NONE', #21031, #98022, #13424 ) ;
#43281 = CARTESIAN_POINT ( 'NONE',  ( 171.2611302217239029, 284.5690204168765831, -11.47485418152970560 ) ) ;
#43282 = B_SPLINE_SURFACE_WITH_KNOTS ( 'NONE', 3, 1, ( 
 ( #41998, #89649 ),
 ( #72934, #12109 ),
 ( #51082, #3525 ),
 ( #11620, #81537 ),
 ( #34403, #65302 ),
 ( #26805, #88666 ),
 ( #19233, #50102 ),
 ( #81057, #73415 ),
 ( #65787, #42969 ),
 ( #73911, #20210 ),
 ( #52580, #68285 ),
 ( #67287, #21697 ),
 ( #66794, #83035 ),
 ( #5500, #97719 ),
 ( #68780, #29792 ),
 ( #44479, #75410 ),
 ( #45964, #5994 ),
 ( #60168, #99703 ),
 ( #60664, #21209 ),
 ( #13117, #59678 ),
 ( #74918, #75921 ),
 ( #28287, #91133 ),
 ( #36383, #98214 ),
 ( #5012, #28798 ),
 ( #30291, #84531 ),
 ( #14098, #35892 ),
 ( #61179, #92146 ),
 ( #84041, #22699 ),
 ( #43976, #90651 ),
 ( #22193, #98722 ),
 ( #36888, #13606 ),
 ( #52089, #67797 ),
 ( #83534, #29306 ),
 ( #44980, #6502 ) ),
 .UNSPECIFIED., .T., .F., .F.,
 ( 4, 2, 2, 2, 2, 2, 2, 2, 2, 2, 2, 2, 2, 2, 2, 2, 4 ),
 ( 2, 2 ),
 ( 0.000000000000000000, 0.06250000000000000000, 0.1250000000000000000, 0.1875000000000000000, 0.2500000000000000000, 0.3125000000000000000, 0.3750000000000000000, 0.4375000000000000000, 0.5000000000000000000, 0.5625000000000000000, 0.6250000000000000000, 0.6875000000000000000, 0.7500000000000000000, 0.8125000000000000000, 0.8750000000000000000, 0.9375000000000000000, 1.000000000000000000 ),
 ( 0.000000000000000000, 1.000000000000000000 ),
 .UNSPECIFIED. ) ;
#43283 = CARTESIAN_POINT ( 'NONE',  ( 84.92204705518831531, 44.20989360438028370, 7.136245731002743398 ) ) ;
#43284 = CARTESIAN_POINT ( 'NONE',  ( 196.4164021072083983, 270.5621661862001019, 13.33908636140236936 ) ) ;
#43285 = CARTESIAN_POINT ( 'NONE',  ( 185.2313369549983406, 296.3301568530737882, 4.659716315438352296 ) ) ;
#43286 = CARTESIAN_POINT ( 'NONE',  ( 69.89065256384225222, 70.96540875737194654, 1.221569532770550914 ) ) ;
#43287 = FACE_OUTER_BOUND ( 'NONE', #94521, .T. ) ;
#43288 = CIRCLE ( 'NONE', #72552, 1.449999999999993072 ) ;
#43289 = ORIENTED_EDGE ( 'NONE', *, *, #93204, .T. ) ;
#43290 = CARTESIAN_POINT ( 'NONE',  ( 1.988115337714555064, 24.08080186712590276, -3.090169943749475845 ) ) ;
#43291 = CARTESIAN_POINT ( 'NONE',  ( -40.42249077443059235, 27.53003111760058630, 10.00000000000000000 ) ) ;
#43292 = VERTEX_POINT ( 'NONE', #50055 ) ;
#43293 = LINE ( 'NONE', #36689, #96775 ) ;
#43294 = CARTESIAN_POINT ( 'NONE',  ( 86.43879872498249028, 47.50144577818752367, -11.01113278173269627 ) ) ;
#43295 = LINE ( 'NONE', #91438, #93747 ) ;
#43296 = ORIENTED_EDGE ( 'NONE', *, *, #83749, .T. ) ;
#43297 = DIRECTION ( 'NONE',  ( -0.8660254037844387076, -0.4999999999999998890, -0.000000000000000000 ) ) ;
#43298 = CARTESIAN_POINT ( 'NONE',  ( 184.8651805647570256, 291.9995124747351838, 12.23147168373134264 ) ) ;
#43299 = VECTOR ( 'NONE', #25242, 1000.000000000000000 ) ;
#43300 = CARTESIAN_POINT ( 'NONE',  ( 164.4761815919938215, 245.7658921781788592, 6.833796894895563412 ) ) ;
#43301 = CARTESIAN_POINT ( 'NONE',  ( 75.35759910184178523, 53.42226962351871578, 16.03358801198504224 ) ) ;
#43302 = ORIENTED_EDGE ( 'NONE', *, *, #35397, .T. ) ;
#43303 = CARTESIAN_POINT ( 'NONE',  ( 80.49933977867583224, 217.2833772461660544, -9.188101187500095079 ) ) ;
#43304 = CARTESIAN_POINT ( 'NONE',  ( 203.3686379427449253, 278.4021817475232297, 14.97501784957458426 ) ) ;
#43305 = AXIS2_PLACEMENT_3D ( 'NONE', #8195, #92335, #98915 ) ;
#43306 = CARTESIAN_POINT ( 'NONE',  ( 81.43089153347496278, 41.93548625179531797, -7.634709731026679158 ) ) ;
#43307 = ORIENTED_EDGE ( 'NONE', *, *, #60787, .T. ) ;
#43308 = ORIENTED_EDGE ( 'NONE', *, *, #52337, .F. ) ;
#43309 = EDGE_CURVE ( 'NONE', #99407, #63534, #95292, .T. ) ;
#43310 = DIRECTION ( 'NONE',  ( -0.8660254037844359321, -0.5000000000000051070, -0.000000000000000000 ) ) ;
#43311 = VERTEX_POINT ( 'NONE', #94690 ) ;
#43312 = DIRECTION ( 'NONE',  ( -1.000000000000000000, 0.000000000000000000, 0.000000000000000000 ) ) ;
#43313 = EDGE_LOOP ( 'NONE', ( #52259, #56003, #79386, #95557 ) ) ;
#43314 = ADVANCED_FACE ( 'NONE', ( #49063 ), #72400, .F. ) ;
#43315 = LINE ( 'NONE', #83360, #42743 ) ;
#43316 = CARTESIAN_POINT ( 'NONE',  ( 155.0453531195792038, 262.1005662498678817, -18.46987289964740953 ) ) ;
#43317 = ORIENTED_EDGE ( 'NONE', *, *, #27586, .T. ) ;
#43318 = CARTESIAN_POINT ( 'NONE',  ( 207.5409781303276588, 271.1754765561682348, -7.231270017877110767 ) ) ;
#43319 = AXIS2_PLACEMENT_3D ( 'NONE', #82942, #29207, #28194 ) ;
#43320 = CARTESIAN_POINT ( 'NONE',  ( 81.90780539245514547, 41.08307300545056506, 3.607455742197654303 ) ) ;
#43321 = CARTESIAN_POINT ( 'NONE',  ( 80.71947726780676646, 43.20949036903483176, -9.150662618319326924 ) ) ;
#43322 = ADVANCED_FACE ( 'NONE', ( #90602 ), #81494, .T. ) ;
#43323 = CARTESIAN_POINT ( 'NONE',  ( 153.0308080659177392, 265.5898606369461277, -17.74682723936668438 ) ) ;
#43324 = EDGE_CURVE ( 'NONE', #59740, #5666, #82509, .T. ) ;
#43325 = LINE ( 'NONE', #57028, #8074 ) ;
#43326 = CARTESIAN_POINT ( 'NONE',  ( 27.10026011071931151, 20.81029122506295437, 8.090169943749479842 ) ) ;
#43327 = CARTESIAN_POINT ( 'NONE',  ( 140.8778087205959650, 242.9548013555409796, -4.594050593750042211 ) ) ;
#43328 = CARTESIAN_POINT ( 'NONE',  ( 195.8767001660183951, 291.3785986239582826, -17.20508890422931003 ) ) ;
#43329 = EDGE_LOOP ( 'NONE', ( #12441, #8536, #75743, #85430 ) ) ;
#43330 = CARTESIAN_POINT ( 'NONE',  ( 76.21559454301076642, 57.26398044443746471, 16.12431043198527902 ) ) ;
#43331 = CARTESIAN_POINT ( 'NONE',  ( 4.512196379633642174, 24.64646525600387861, -2.839279412974133887 ) ) ;
#43332 = EDGE_LOOP ( 'NONE', ( #16264, #24062, #39779, #50017 ) ) ;
#43333 = CARTESIAN_POINT ( 'NONE',  ( 93.96857342517718337, 4.999999999999999112, -14.21260523776213347 ) ) ;
#43335 = ORIENTED_EDGE ( 'NONE', *, *, #92560, .F. ) ;
#43334 = CARTESIAN_POINT ( 'NONE',  ( 200.0523276869015206, 270.2207466263407696, 9.267919080221707517 ) ) ;
#43336 = DIRECTION ( 'NONE',  ( 0.000000000000000000, 0.000000000000000000, 1.000000000000000000 ) ) ;
#43337 = LINE ( 'NONE', #41845, #98128 ) ;
#43338 = CARTESIAN_POINT ( 'NONE',  ( 161.1767284389501071, 281.8257712043616152, -6.166458447416498956 ) ) ;
#43339 = CARTESIAN_POINT ( 'NONE',  ( 83.30032458682389063, 49.65944847437223331, -13.96189754096489288 ) ) ;
#43340 = CARTESIAN_POINT ( 'NONE',  ( 67.86860378221429357, 65.58690806574966814, -10.91583492536020472 ) ) ;
#43341 = CARTESIAN_POINT ( 'NONE',  ( 84.04231234028014796, 41.83853045254244307, 0.6551603079148081710 ) ) ;
#43342 = CARTESIAN_POINT ( 'NONE',  ( 88.39405946958876825, 44.08409158760228053, -2.802556091636618341 ) ) ;
#43343 = ORIENTED_EDGE ( 'NONE', *, *, #80799, .F. ) ;
#43344 = CARTESIAN_POINT ( 'NONE',  ( 184.6274781232527573, 272.9621770304452184, -16.38896422655171392 ) ) ;
#43345 = CARTESIAN_POINT ( 'NONE',  ( 66.45390109022466163, 68.94435773741150797, 0.02467235416223488229 ) ) ;
#43346 = VERTEX_POINT ( 'NONE', #43932 ) ;
#43347 = CIRCLE ( 'NONE', #19157, 70.00000000000001421 ) ;
#43348 = FACE_OUTER_BOUND ( 'NONE', #69410, .T. ) ;
#43349 = CARTESIAN_POINT ( 'NONE',  ( 171.7367047606329038, 279.7472062399093602, -14.55191673240434902 ) ) ;
#43350 = DIRECTION ( 'NONE',  ( -0.9995486091367050685, 0.03004293549036790231, 0.000000000000000000 ) ) ;
#43351 = CARTESIAN_POINT ( 'NONE',  ( 81.61276851515816588, 44.80639225569448314, -10.39255593558327462 ) ) ;
#43352 = VECTOR ( 'NONE', #46724, 1000.000000000000000 ) ;
#43353 = CARTESIAN_POINT ( 'NONE',  ( -8.406493707509316238, 25.24382671950691304, -10.00000000000000000 ) ) ;
#43355 = CARTESIAN_POINT ( 'NONE',  ( 88.26049611827410502, 43.94792280741877732, 2.484900765466349082 ) ) ;
#43354 = DIRECTION ( 'NONE',  ( 1.000000000000000000, 1.465097884282125932E-13, 0.000000000000000000 ) ) ;
#43356 = CARTESIAN_POINT ( 'NONE',  ( 203.5077069180501042, 269.8384169519572993, 5.656147133308556896 ) ) ;
#43357 = ORIENTED_EDGE ( 'NONE', *, *, #56472, .T. ) ;
#43358 = ORIENTED_EDGE ( 'NONE', *, *, #41154, .T. ) ;
#43359 = LINE ( 'NONE', #81915, #41985 ) ;
#43360 = CARTESIAN_POINT ( 'NONE',  ( 80.04426707012592601, 58.13730958922976555, 16.26787960027916569 ) ) ;
#43361 = CARTESIAN_POINT ( 'NONE',  ( 85.76519349052995267, 48.62301808087004673, -11.86379414718568093 ) ) ;
#43362 = CARTESIAN_POINT ( 'NONE',  ( 175.6384468060905988, 290.9795127648189350, 2.794533193917200453 ) ) ;
#43363 = LINE ( 'NONE', #57067, #29139 ) ;
#43364 = AXIS2_PLACEMENT_3D ( 'NONE', #35901, #75935, #99218 ) ;
#43365 =( BOUNDED_CURVE ( )  B_SPLINE_CURVE ( 2, ( #95726, #88628, #19196, #50066, #81024, #97204, #27769, #12577, #43453 ),
 .UNSPECIFIED., .F., .T. ) 
 B_SPLINE_CURVE_WITH_KNOTS ( ( 3, 2, 2, 2, 3 ),
 ( 0.7862903225806451291, 0.7876344086021505042, 0.7903225806451612545, 0.7930107526881720048, 0.7943548387096773800 ),
 .UNSPECIFIED. ) 
 CURVE ( )  GEOMETRIC_REPRESENTATION_ITEM ( )  RATIONAL_B_SPLINE_CURVE ( ( 0.9330127018922194093, 0.9330127018922194093, 1.000000000000000000, 0.8660254037844387076, 1.000000000000000000, 0.8660254037844387076, 1.000000000000000000, 0.9330127018922194093, 0.9330127018922194093 ) ) 
 REPRESENTATION_ITEM ( '' )  );
#43366 = LINE ( 'NONE', #96626, #46487 ) ;
#43367 = CARTESIAN_POINT ( 'NONE',  ( 24.55112987542764458, 40.41347472807389352, 10.00000000000000000 ) ) ;
#43368 = CARTESIAN_POINT ( 'NONE',  ( 2.557053438076354990, 172.2833772461660828, -9.188101187500095079 ) ) ;
#43369 = CARTESIAN_POINT ( 'NONE',  ( 107.1028179730028285, 223.4548013555409796, -4.594050593750042211 ) ) ;
#43370 = CARTESIAN_POINT ( 'NONE',  ( 87.66150902149263402, 44.36974732289110790, -4.043329145106127065 ) ) ;
#43371 = CARTESIAN_POINT ( 'NONE',  ( 184.9305274905498493, 294.8224435932747838, -7.698895662769760229 ) ) ;
#43372 = CARTESIAN_POINT ( 'NONE',  ( 78.76277686495221531, 54.87806250904672112, 16.03155917534425967 ) ) ;
#43373 = VECTOR ( 'NONE', #69513, 1000.000000000000000 ) ;
#43374 = EDGE_CURVE ( 'NONE', #9838, #77732, #22750, .T. ) ;
#43375 = CARTESIAN_POINT ( 'NONE',  ( 75.99421521153445269, 51.38408235280206071, 15.66610209674420062 ) ) ;
#43376 = B_SPLINE_CURVE_WITH_KNOTS ( 'NONE', 3,
 ( #85694, #40008, #70948, #15214 ),
 .UNSPECIFIED., .F., .F.,
 ( 4, 4 ),
 ( 0.01311470161809044112, 0.02170404453345711054 ),
 .UNSPECIFIED. ) ;
#43377 = CARTESIAN_POINT ( 'NONE',  ( 154.8556227199321427, 262.4291889417971788, 17.77326384500479861 ) ) ;
#43378 = CARTESIAN_POINT ( 'NONE',  ( 194.5298665426430489, 293.7113828889860656, -16.13302716640051315 ) ) ;
#43379 = CARTESIAN_POINT ( 'NONE',  ( 85.04850917506151120, 49.90949791588273143, 13.51477744872044262 ) ) ;
#43380 = CARTESIAN_POINT ( 'NONE',  ( 196.4695417320205024, 266.7097263680378205, 8.121914006708831124 ) ) ;
#43381 = CARTESIAN_POINT ( 'NONE',  ( 79.69646206235792363, 223.4865022471902591, -10.00000000000009592 ) ) ;
#43382 = CARTESIAN_POINT ( 'NONE',  ( 181.5716216444320992, 267.3631569497555915, -14.78134104179376784 ) ) ;
#43383 = VECTOR ( 'NONE', #642, 1000.000000000000000 ) ;
#43384 = DIRECTION ( 'NONE',  ( -0.8660254037844379305, -0.5000000000000014433, -0.000000000000000000 ) ) ;
#43385 = EDGE_CURVE ( 'NONE', #95480, #66118, #68732, .T. ) ;
#43386 = CARTESIAN_POINT ( 'NONE',  ( 81.52757139778736928, 224.0024278399160949, 9.188101187500095079 ) ) ;
#43387 = CARTESIAN_POINT ( 'NONE',  ( 5.211622267866312441, 23.98502408145590081, -5.678558825948271327 ) ) ;
#43388 = CARTESIAN_POINT ( 'NONE',  ( 191.4922467593309250, 298.9726946877590876, 7.604184559945784017 ) ) ;
#43389 = CARTESIAN_POINT ( 'NONE',  ( -13.90044561320711480, 103.8584542157411761, 10.83137812414022605 ) ) ;
#43391 = CARTESIAN_POINT ( 'NONE',  ( 86.44709368921655823, 43.17377345843237180, -0.6848223079830935145 ) ) ;
#43390 = CARTESIAN_POINT ( 'NONE',  ( 157.8562613713738472, 257.2319303423452652, 17.81420683562559404 ) ) ;
#43392 = CARTESIAN_POINT ( 'NONE',  ( 196.9726513669839107, 289.4803554612698235, 16.57669625517693746 ) ) ;
#43393 = CARTESIAN_POINT ( 'NONE',  ( 198.9369963555428740, 286.0780101374919013, -18.58432392708837710 ) ) ;
#43394 = CARTESIAN_POINT ( 'NONE',  ( 173.1825648917232172, 268.0947487749845095, -16.28828717342791421 ) ) ;
#43395 = CARTESIAN_POINT ( 'NONE',  ( 33.43441462842632461, 34.70171378149922248, -9.188101187500004485 ) ) ;
#43396 = CARTESIAN_POINT ( 'NONE',  ( 193.1977289678065404, 296.0187128512746995, -12.37159405312863925 ) ) ;
#43397 = CARTESIAN_POINT ( 'NONE',  ( -27.42236680055714260, 166.5217562850347406, 1.224646799147364892E-15 ) ) ;
#43398 = VERTEX_POINT ( 'NONE', #31711 ) ;
#43399 = CARTESIAN_POINT ( 'NONE',  ( 25.85429974905589745, 23.43085787977764056, -9.188101187500008038 ) ) ;
#43400 = DIRECTION ( 'NONE',  ( -0.9999990636452669168, -0.001368469433193631119, 0.000000000000000000 ) ) ;
#43401 = CARTESIAN_POINT ( 'NONE',  ( 146.8153075009282134, 276.3554234099810287, -4.113808735271278216 ) ) ;
#43402 = CARTESIAN_POINT ( 'NONE',  ( 191.7535527499152579, 287.9627823321743563, -15.84076656666959160 ) ) ;
#43403 = ORIENTED_EDGE ( 'NONE', *, *, #38266, .F. ) ;
#43404 = CARTESIAN_POINT ( 'NONE',  ( 70.95991511397710383, 61.13971250865433404, 15.00408310107609644 ) ) ;
#43405 = FACE_OUTER_BOUND ( 'NONE', #9253, .T. ) ;
#43406 = CARTESIAN_POINT ( 'NONE',  ( 157.7704454140505277, 268.4375085597957309, 16.01069904446985603 ) ) ;
#43407 = DIRECTION ( 'NONE',  ( 0.000000000000000000, 0.000000000000000000, 1.000000000000000000 ) ) ;
#43408 = CARTESIAN_POINT ( 'NONE',  ( 87.35668359673078953, 44.84080960044052233, -6.701380392922977158 ) ) ;
#43409 = CARTESIAN_POINT ( 'NONE',  ( 145.5865615336240353, 244.8615022471901739, 5.000000000000051514 ) ) ;
#43410 = CARTESIAN_POINT ( 'NONE',  ( 157.8159121039657293, 257.3018173235443555, -17.05074702406642118 ) ) ;
#43411 = CARTESIAN_POINT ( 'NONE',  ( 75.34529629774760906, 53.42024133556077459, 16.03399186784752217 ) ) ;
#43412 = ORIENTED_EDGE ( 'NONE', *, *, #90040, .F. ) ;
#43413 = CARTESIAN_POINT ( 'NONE',  ( 190.1016529815521210, 299.5590995676359967, -6.615970321355634454 ) ) ;
#43414 = AXIS2_PLACEMENT_3D ( 'NONE', #15287, #116, #21907 ) ;
#43415 = CARTESIAN_POINT ( 'NONE',  ( 167.5388416099013966, 248.0610247611899695, -1.869801589506421724 ) ) ;
#43416 = ORIENTED_EDGE ( 'NONE', *, *, #77997, .F. ) ;
#43417 = CARTESIAN_POINT ( 'NONE',  ( 196.8310340268163543, 265.3144059923225768, -4.523882790829159894 ) ) ;
#43418 = CARTESIAN_POINT ( 'NONE',  ( 86.39765121943966619, 44.20258484113508501, 5.509774257601782743 ) ) ;
#43419 = VERTEX_POINT ( 'NONE', #83989 ) ;
#43420 = CARTESIAN_POINT ( 'NONE',  ( 77.16771381044527800, 63.58369421181528480, -15.05433088148817511 ) ) ;
#43421 = ORIENTED_EDGE ( 'NONE', *, *, #19228, .T. ) ;
#43422 = VECTOR ( 'NONE', #97852, 999.9999999999998863 ) ;
#43423 = CARTESIAN_POINT ( 'NONE',  ( 192.8339539104745768, 292.5331237600439636, 15.31903378033653773 ) ) ;
#43424 = CARTESIAN_POINT ( 'NONE',  ( 158.3813060601511893, 256.3225262651385492, 16.44677913423000959 ) ) ;
#43425 = DIRECTION ( 'NONE',  ( -0.06142469166374898287, -0.9981117208278906805, 0.000000000000000000 ) ) ;
#43426 = CARTESIAN_POINT ( 'NONE',  ( 204.4652362847643303, 273.3276312005621094, 10.91026480097475293 ) ) ;
#43427 = CARTESIAN_POINT ( 'NONE',  ( 192.5395560493205949, 296.4429067975564180, -11.74828324584324868 ) ) ;
#43428 = VECTOR ( 'NONE', #52317, 1000.000000000000000 ) ;
#43429 = VECTOR ( 'NONE', #27378, 1000.000000000000227 ) ;
#43430 = CARTESIAN_POINT ( 'NONE',  ( 30.66616357392367220, 39.74646525600392977, 2.839279412974139660 ) ) ;
#43431 = CARTESIAN_POINT ( 'NONE',  ( 74.81245076906620284, 60.05495312879037328, -15.59845400761551559 ) ) ;
#43432 = EDGE_CURVE ( 'NONE', #73019, #39791, #17720, .T. ) ;
#43433 = CARTESIAN_POINT ( 'NONE',  ( 164.0653621983113339, 275.4287311911768370, 15.31700800437514864 ) ) ;
#43434 = CARTESIAN_POINT ( 'NONE',  ( 87.14368005316970311, 45.34715801825632298, 7.070389941925012245 ) ) ;
#43435 = EDGE_LOOP ( 'NONE', ( #24296, #96420, #241, #67874 ) ) ;
#43436 = EDGE_LOOP ( 'NONE', ( #45121, #45334, #30737, #57947 ) ) ;
#43437 = PLANE ( 'NONE',  #83290 ) ;
#43438 = VECTOR ( 'NONE', #96415, 1000.000000000000000 ) ;
#43440 = CARTESIAN_POINT ( 'NONE',  ( 165.9755981782961953, 274.1598679360748179, -15.15796544636562260 ) ) ;
#43439 = CARTESIAN_POINT ( 'NONE',  ( 68.34553620988224054, 65.65657992573082424, 10.39144713415675270 ) ) ;
#43441 = CARTESIAN_POINT ( 'NONE',  ( 85.54016331024442366, 48.30264805437344933, -11.71386965376238365 ) ) ;
#43442 = CARTESIAN_POINT ( 'NONE',  ( 193.9495889092963807, 294.7164532324382549, 15.46986001312306058 ) ) ;
#43443 = CARTESIAN_POINT ( 'NONE',  ( 186.6970606014003522, 295.2539764206142081, -10.47640868448896434 ) ) ;
#43444 = CARTESIAN_POINT ( 'NONE',  ( 82.08531156464800915, 40.77555587586176955, 1.302602283300562824 ) ) ;
#43445 = ADVANCED_FACE ( 'NONE', ( #76362 ), #16034, .F. ) ;
#43446 = CARTESIAN_POINT ( 'NONE',  ( 170.8091510057469691, 288.1825902081931190, -4.081328050745901770 ) ) ;
#43447 = EDGE_CURVE ( 'NONE', #11106, #30511, #30976, .T. ) ;
#43448 = CARTESIAN_POINT ( 'NONE',  ( 88.32078559155080200, 44.16791947909882765, 0.3596700509409204716 ) ) ;
#43449 = CARTESIAN_POINT ( 'NONE',  ( 180.5366697149694062, 256.7075445286905619, 4.926626485048444692 ) ) ;
#43450 = CARTESIAN_POINT ( 'NONE',  ( 92.65049840370248546, 233.4869531367911293, 4.594050593750046652 ) ) ;
#43451 = ORIENTED_EDGE ( 'NONE', *, *, #20031, .T. ) ;
#43452 = DIRECTION ( 'NONE',  ( 1.000000000000000000, 0.000000000000000000, 0.000000000000000000 ) ) ;
#43453 = CARTESIAN_POINT ( 'NONE',  ( 110.3297989853572005, 246.0530062829863311, -4.648177544792955347E-16 ) ) ;
#43454 = EDGE_LOOP ( 'NONE', ( #75287, #28424, #35120, #75449 ) ) ;
#43455 = EDGE_LOOP ( 'NONE', ( #39663, #11211, #57891, #78899, #60593 ) ) ;
#43456 = CARTESIAN_POINT ( 'NONE',  ( 86.95562746175168911, 45.78762616370607930, -8.653322509500107174 ) ) ;
#43457 = CARTESIAN_POINT ( 'NONE',  ( 179.5498935473132747, 293.3807426002626357, -2.640407830033155268 ) ) ;
#43458 = CARTESIAN_POINT ( 'NONE',  ( 157.8763546842245376, 257.1971277035954699, 17.68444922773363004 ) ) ;
#43459 = CARTESIAN_POINT ( 'NONE',  ( 160.0061168334508750, 253.5082714530983026, -16.02306982074888708 ) ) ;
#43460 = CARTESIAN_POINT ( 'NONE',  ( 162.8491774010308575, 248.5839461010540390, 10.21539626359008146 ) ) ;
#43461 = ORIENTED_EDGE ( 'NONE', *, *, #90057, .T. ) ;
#43462 = EDGE_LOOP ( 'NONE', ( #49927, #22992, #6815, #56776, #4711 ) ) ;
#43463 = CARTESIAN_POINT ( 'NONE',  ( 207.9743173328493526, 270.4249110404894054, -2.481515874287090639 ) ) ;
#43464 = VERTEX_POINT ( 'NONE', #93569 ) ;
#43465 = CARTESIAN_POINT ( 'NONE',  ( 191.3753129921931873, 263.8116507527752788, -8.027821554704329898 ) ) ;
#43466 = CARTESIAN_POINT ( 'NONE',  ( 27.69565257936902469, 21.15404122711134605, 8.090169943749479842 ) ) ;
#43467 = CARTESIAN_POINT ( 'NONE',  ( 81.82192856674927839, 43.76204572152891359, 9.071121036995474896 ) ) ;
#43469 = CARTESIAN_POINT ( 'NONE',  ( 198.7045056313791633, 284.4806958840320021, 17.79791830837532274 ) ) ;
#43468 = CARTESIAN_POINT ( 'NONE',  ( 131.6216415740022398, 255.9869531367911009, 4.594050593750046652 ) ) ;
#43470 = CARTESIAN_POINT ( 'NONE',  ( -107.5954152546897404, 65.38554960527368110, 21.50000000000000000 ) ) ;
#43471 = ORIENTED_EDGE ( 'NONE', *, *, #49308, .T. ) ;
#43472 = CARTESIAN_POINT ( 'NONE',  ( 146.8729474948188454, 276.2555880120147549, 3.934020695290606273 ) ) ;
#43473 = CARTESIAN_POINT ( 'NONE',  ( 81.92774799985024003, 49.39617170011497649, 13.74847781650752765 ) ) ;
#43474 = CARTESIAN_POINT ( 'NONE',  ( 206.6268150440956504, 272.7588534679261443, -10.76664753678610609 ) ) ;
#43475 = CARTESIAN_POINT ( 'NONE',  ( 173.2003599206826436, 251.6178260009447456, -0.2735355138943916242 ) ) ;
#43476 = CARTESIAN_POINT ( 'NONE',  ( 178.4715894149740052, 285.3467937416216955, 13.10955772305596945 ) ) ;
#43477 = CARTESIAN_POINT ( 'NONE',  ( 64.18017357788670552, 207.8615022471903728, 5.188172501216618598E-14 ) ) ;
#43478 = CARTESIAN_POINT ( 'NONE',  ( 199.0630536459244411, 281.9549554678117715, -16.62110652460417626 ) ) ;
#43479 = CARTESIAN_POINT ( 'NONE',  ( 147.4935738007826842, 244.4155109091896065, 2.679491924311254714 ) ) ;
#43480 = CARTESIAN_POINT ( 'NONE',  ( 185.9608592076092464, 288.5956984647530703, 15.36535719480430018 ) ) ;
#43481 = CARTESIAN_POINT ( 'NONE',  ( 67.38373687966300452, 69.45179799017431321, -1.105247961781016919 ) ) ;
#43482 = CIRCLE ( 'NONE', #25721, 50.00000000000000711 ) ;
#43483 = CARTESIAN_POINT ( 'NONE',  ( 57.33281313167710636, 216.1589784336661921, -6.496448406907675876E-16 ) ) ;
#43484 = CARTESIAN_POINT ( 'NONE',  ( 14.28567607145357421, 31.18080186712592550, 3.090169943749475401 ) ) ;
#43485 = CARTESIAN_POINT ( 'NONE',  ( 77.64328263671511365, 61.91708053827061065, 15.64711088792926041 ) ) ;
#43486 = CARTESIAN_POINT ( 'NONE',  ( 162.6757594134126350, 248.8843148665554281, -10.86406770146305867 ) ) ;
#43488 = CARTESIAN_POINT ( 'NONE',  ( 191.1363710586135198, 294.8022764895544583, 13.34403287223599222 ) ) ;
#43487 = VECTOR ( 'NONE', #15194, 1000.000000000000000 ) ;
#43489 = CIRCLE ( 'NONE', #85644, 70.00000000000001421 ) ;
#43490 = EDGE_CURVE ( 'NONE', #30622, #44213, #70226, .T. ) ;
#43491 = AXIS2_PLACEMENT_3D ( 'NONE', #5565, #74500, #97790 ) ;
#43492 = CARTESIAN_POINT ( 'NONE',  ( 156.6812872898450735, 261.2670451491295012, 0.000000000000000000 ) ) ;
#43493 = LINE ( 'NONE', #51606, #28552 ) ;
#43494 = CARTESIAN_POINT ( 'NONE',  ( 161.8385268298191306, 255.1149155613134951, 15.97321096069992308 ) ) ;
#43495 = ADVANCED_FACE ( 'NONE', ( #77340, #62616 ), #69729, .T. ) ;
#43496 = CARTESIAN_POINT ( 'NONE',  ( 39.83529790697233608, 25.12755873383629179, -6.180339887498949025 ) ) ;
#43497 = CARTESIAN_POINT ( 'NONE',  ( 79.77742007133535651, 56.10585682640231653, -16.52583479100570685 ) ) ;
#43498 = CARTESIAN_POINT ( 'NONE',  ( -26.08262083840154233, 139.2012482093457493, -48.95643923738973768 ) ) ;
#43499 = CARTESIAN_POINT ( 'NONE',  ( 87.27919387765231818, 43.83186819549126056, -2.650470388296021440 ) ) ;
#43500 = CARTESIAN_POINT ( 'NONE',  ( 207.1019571622349815, 271.9358831784929293, -5.989975140547304733 ) ) ;
#43501 = AXIS2_PLACEMENT_3D ( 'NONE', #16549, #42828, #20069 ) ;
#43502 = CARTESIAN_POINT ( 'NONE',  ( 15.00651571324267763, 167.2202760586659736, -5.415160957724236172E-17 ) ) ;
#43503 = B_SPLINE_CURVE_WITH_KNOTS ( 'NONE', 3,
 ( #23576, #54986, #54467, #40274 ),
 .UNSPECIFIED., .F., .F.,
 ( 4, 4 ),
 ( 0.01796415739704124506, 0.02693908509615394742 ),
 .UNSPECIFIED. ) ;
#43504 = CARTESIAN_POINT ( 'NONE',  ( 207.2586958963831023, 270.9687488091540217, 3.100303027002558665 ) ) ;
#43505 = ORIENTED_EDGE ( 'NONE', *, *, #60920, .T. ) ;
#43506 = ADVANCED_FACE ( 'NONE', ( #53529 ), #92099, .F. ) ;
#43507 = CARTESIAN_POINT ( 'NONE',  ( 87.10076192357585967, 46.06401709681040302, 8.920816893773267253 ) ) ;
#43508 = CARTESIAN_POINT ( 'NONE',  ( -69.61464189717713680, 45.83092310410447112, -10.00000000000000000 ) ) ;
#43509 = CARTESIAN_POINT ( 'NONE',  ( 164.3545367017254364, 245.9765873086048487, -5.942639963102972267 ) ) ;
#43510 = CARTESIAN_POINT ( 'NONE',  ( 71.65515660876562265, 72.43366598492664821, -1.354044368658560815 ) ) ;
#43511 = CARTESIAN_POINT ( 'NONE',  ( 59.22776434610305785, 198.8768266524159571, -9.188101187500093303 ) ) ;
#43512 = CARTESIAN_POINT ( 'NONE',  ( 161.5056331467593225, 250.9110330116698435, 14.52719814064025528 ) ) ;
#43513 = CARTESIAN_POINT ( 'NONE',  ( 151.1126408083691501, 268.9122237844355254, -15.82705194100464396 ) ) ;
#43514 = CARTESIAN_POINT ( 'NONE',  ( 147.3984236761635884, 275.3454365677582700, 5.108566646342994844 ) ) ;
#43515 = CARTESIAN_POINT ( 'NONE',  ( 5.010160986809694350, 24.93396525600388003, 2.839279412974139660 ) ) ;
#43516 = CARTESIAN_POINT ( 'NONE',  ( 202.8423703034144694, 269.9731342184576874, -6.433654896179251459 ) ) ;
#43517 = CARTESIAN_POINT ( 'NONE',  ( 146.5310397537613483, 276.8477895910274356, -0.2793038414862049068 ) ) ;
#43518 = CARTESIAN_POINT ( 'NONE',  ( 179.6700249023918730, 276.7835841873084064, 16.30426102577613534 ) ) ;
#43519 = CARTESIAN_POINT ( 'NONE',  ( 33.47037235539277589, 49.41749479597460493, -10.00000000000000000 ) ) ;
#43520 = LINE ( 'NONE', #13636, #21711 ) ;
#43521 = PRODUCT ( 'Lead Screw Acme Drive Shaft', 'Lead Screw Acme Drive Shaft', '', ( #69448 ) ) ;
#43522 = CARTESIAN_POINT ( 'NONE',  ( 167.0324277405701139, 257.7922078709543143, -15.65539679637635651 ) ) ;
#43523 = EDGE_CURVE ( 'NONE', #80622, #75397, #50362, .T. ) ;
#43524 = CARTESIAN_POINT ( 'NONE',  ( 82.93017357788667709, 175.3855496052738374, -36.50000000000000000 ) ) ;
#43525 = CARTESIAN_POINT ( 'NONE',  ( 102.3574601280508176, 223.2365022471902023, 10.00000000000009592 ) ) ;
#43526 = CARTESIAN_POINT ( 'NONE',  ( -19.65312891409030271, 93.06504152958497400, 10.00000000000000888 ) ) ;
#43527 = FACE_OUTER_BOUND ( 'NONE', #3835, .T. ) ;
#43528 = ORIENTED_EDGE ( 'NONE', *, *, #15045, .F. ) ;
#43529 = CARTESIAN_POINT ( 'NONE',  ( 52.13666070897046012, 213.1589784336661637, -6.496448406907675876E-16 ) ) ;
#43530 = ORIENTED_EDGE ( 'NONE', *, *, #34630, .F. ) ;
#43531 = CARTESIAN_POINT ( 'NONE',  ( 192.5076277540105423, 297.2140032159341558, -13.10094381206144298 ) ) ;
#43532 = CARTESIAN_POINT ( 'NONE',  ( 147.2443490232117256, 275.6123016948292275, 5.226063659459642352 ) ) ;
#43533 = CARTESIAN_POINT ( 'NONE',  ( -17.42236680055705023, 149.2012482093457777, 0.000000000000000000 ) ) ;
#43534 = VERTEX_POINT ( 'NONE', #97561 ) ;
#43535 = CARTESIAN_POINT ( 'NONE',  ( 70.24235140437789937, 201.3615022471901739, 5.000000000000051514 ) ) ;
#43536 = CARTESIAN_POINT ( 'NONE',  ( 206.9026071836525205, 272.2811674698855313, 7.240992997279449561 ) ) ;
#43537 = CARTESIAN_POINT ( 'NONE',  ( 162.0192538899617318, 268.0510789565263394, -17.53028463913764057 ) ) ;
#43538 = CARTESIAN_POINT ( 'NONE',  ( 26.79248755578709762, 33.65586893147757763, -7.433330006724137462 ) ) ;
#43539 = LINE ( 'NONE', #74480, #96718 ) ;
#43540 = CARTESIAN_POINT ( 'NONE',  ( 86.20715737948781054, 46.96926287157581470, -10.06788908585955511 ) ) ;
#43541 = CARTESIAN_POINT ( 'NONE',  ( 157.4725523017146429, 257.8965339463198916, 17.43710027717953892 ) ) ;
#43542 = ORIENTED_EDGE ( 'NONE', *, *, #48827, .T. ) ;
#43543 = CARTESIAN_POINT ( 'NONE',  ( 11.06573324809563807, 29.49540643055186351, 3.479690158560446702E-15 ) ) ;
#43544 = DIRECTION ( 'NONE',  ( 0.8560416229147678191, 0.5169068966820336009, 0.000000000000000000 ) ) ;
#43545 = CARTESIAN_POINT ( 'NONE',  ( 67.81490795777737901, 69.52803666604617661, -2.566435835120146169 ) ) ;
#43546 = CARTESIAN_POINT ( 'NONE',  ( 48.61286661847091040, 84.94359857078811160, -10.00000000000000000 ) ) ;
#43547 = EDGE_CURVE ( 'NONE', #44921, #93452, #96349, .T. ) ;
#43548 = EDGE_LOOP ( 'NONE', ( #33618, #775, #20643, #81038 ) ) ;
#43549 = CARTESIAN_POINT ( 'NONE',  ( 182.4419837166206548, 284.0818805488852377, 15.00679419155397554 ) ) ;
#43550 = CARTESIAN_POINT ( 'NONE',  ( 151.4327733764141612, 268.3577379114237829, 14.90862905801242100 ) ) ;
#43551 = CARTESIAN_POINT ( 'NONE',  ( 206.2809287719926488, 273.3579460648492159, -10.70911012174624588 ) ) ;
#43552 = ORIENTED_EDGE ( 'NONE', *, *, #72458, .F. ) ;
#43553 = VERTEX_POINT ( 'NONE', #89969 ) ;
#43554 = ADVANCED_FACE ( 'NONE', ( #74759 ), #28624, .T. ) ;
#43556 = DIRECTION ( 'NONE',  ( -0.000000000000000000, -0.000000000000000000, 1.000000000000000000 ) ) ;
#43555 = CARTESIAN_POINT ( 'NONE',  ( 161.3773209892555371, 251.1332761876949746, -14.50043705923759241 ) ) ;
#43557 = DIRECTION ( 'NONE',  ( 0.5000000000000048850, -0.8660254037844358210, 0.000000000000000000 ) ) ;
#43558 = ORIENTED_EDGE ( 'NONE', *, *, #59685, .T. ) ;
#43559 = CARTESIAN_POINT ( 'NONE',  ( 66.09459138788395194, 68.54660210817900179, -2.305970830781039815 ) ) ;
#43560 = CARTESIAN_POINT ( 'NONE',  ( 159.2303255284352304, 254.8519814094557603, 16.39103317446447150 ) ) ;
#43561 = DIRECTION ( 'NONE',  ( -0.000000000000000000, -0.000000000000000000, 1.000000000000000000 ) ) ;
#43562 = CARTESIAN_POINT ( 'NONE',  ( -6.134002256249970308, 43.13092002735066188, 59.99999999999999289 ) ) ;
#43563 = EDGE_CURVE ( 'NONE', #79622, #16754, #75247, .T. ) ;
#43564 = CARTESIAN_POINT ( 'NONE',  ( 126.2364799639240402, 237.5643266524160140, 9.188101187500095079 ) ) ;
#43565 = VECTOR ( 'NONE', #38666, 999.9999999999998863 ) ;
#43566 = EDGE_CURVE ( 'NONE', #53916, #22854, #58780, .T. ) ;
#43567 = DIRECTION ( 'NONE',  ( 0.5000000000000013323, -0.8660254037844378194, 0.000000000000000000 ) ) ;
#43568 = VERTEX_POINT ( 'NONE', #42809 ) ;
#43569 = AXIS2_PLACEMENT_3D ( 'NONE', #13484, #44356, #97600 ) ;
#43570 = CARTESIAN_POINT ( 'NONE',  ( 201.5099656766716976, 280.8415660465722112, 16.32132609628684605 ) ) ;
#43571 = EDGE_LOOP ( 'NONE', ( #5837, #89139, #37558, #7838, #89233, #48960 ) ) ;
#43572 = EDGE_LOOP ( 'NONE', ( #93678, #31383, #18507, #46381 ) ) ;
#43573 = EDGE_CURVE ( 'NONE', #18962, #6810, #5827, .T. ) ;
#43574 = FACE_BOUND ( 'NONE', #66757, .T. ) ;
#43575 = LINE ( 'NONE', #66383, #12640 ) ;
#43576 = ADVANCED_FACE ( 'NONE', ( #58519 ), #18185, .F. ) ;
#43577 = CARTESIAN_POINT ( 'NONE',  ( 76.33141897508073725, 221.0024278399160949, 9.188101187500095079 ) ) ;
#43578 = CARTESIAN_POINT ( 'NONE',  ( -75.18208942163934694, 50.44421862632483311, 10.00000000000000000 ) ) ;
#43579 = CARTESIAN_POINT ( 'NONE',  ( -19.65312891409030271, 93.06504152958497400, 10.00000000000000888 ) ) ;
#43580 = CARTESIAN_POINT ( 'NONE',  ( 198.7430995078048284, 286.4138493292020371, 18.01120443222870193 ) ) ;
#43581 = CARTESIAN_POINT ( 'NONE',  ( 173.9825871881620571, 277.6148033471986878, 15.53242809676506830 ) ) ;
#43582 = EDGE_LOOP ( 'NONE', ( #15895, #81580, #5330, #60376 ) ) ;
#43583 = AXIS2_PLACEMENT_3D ( 'NONE', #99631, #93545, #76808 ) ;
#43584 = PLANE ( 'NONE',  #88516 ) ;
#43585 = CARTESIAN_POINT ( 'NONE',  ( 152.9251141908703175, 265.7729277985770864, -16.20110192949203309 ) ) ;
#43586 = LINE ( 'NONE', #34983, #75548 ) ;
#43587 = ORIENTED_EDGE ( 'NONE', *, *, #91225, .F. ) ;
#43588 = CARTESIAN_POINT ( 'NONE',  ( 206.9395787313233939, 270.0782334019143605, 3.375702725593451969 ) ) ;
#43589 = CARTESIAN_POINT ( 'NONE',  ( 207.8232941427535536, 270.6864908788566026, -6.505149060073906142 ) ) ;
#43590 = CARTESIAN_POINT ( 'NONE',  ( 174.8967126845354869, 253.3500105558054827, -7.849478773564977807 ) ) ;
#43591 = CARTESIAN_POINT ( 'NONE',  ( 80.21278584107015774, 53.44521250575849791, 16.08036484325488757 ) ) ;
#43592 = B_SPLINE_CURVE_WITH_KNOTS ( 'NONE', 3,
 ( #570, #8668, #79, #30466, #15247, #62345, #53747, #94308, #76577, #39538, #69464, #30961, #61358, #61850, #92798, #70986, #40046, #31953, #1589, #62856, #32471, #54238, #93812, #24372, #7159, #16761, #47650, #78587, #63368, #24860, #55735, #17262, #2586, #72498, #40552, #3584, #33472, #96302, #56253, #49177, #65362, #71980, #80112, #87247, #34464, #26871, #88226, #50163, #10676, #33990, #26375, #42057, #48681, #57253 ),
 .UNSPECIFIED., .F., .F.,
 ( 4, 2, 2, 2, 2, 2, 2, 2, 2, 2, 2, 2, 2, 2, 2, 2, 2, 2, 2, 2, 2, 2, 2, 2, 2, 2, 4 ),
 ( 0.0008417762867302816879, 0.001328145691676835142, 0.001814515096623388595, 0.002057699799096665214, 0.002300884501569942266, 0.002422476852806596838, 0.002544069204043251410, 0.002665661555279905982, 0.002787253906516560555, 0.003030438608989949496, 0.003273623311463338438, 0.003759992716410036958, 0.004732731526303299123, 0.005705470336196561722, 0.006191839741143153122, 0.006435024443616449256, 0.006678209146089744523, 0.006739005321708050125, 0.006799801497326356595, 0.006860597672944663064, 0.006921393848562969534, 0.007042986199799565993, 0.007164578551036161584, 0.007407763253509473331, 0.007650947955982785945, 0.008137317360929409438, 0.008623686765876034666 ),
 .UNSPECIFIED. ) ;
#43593 = LINE ( 'NONE', #51186, #57544 ) ;
#43594 = CARTESIAN_POINT ( 'NONE',  ( 9.458193372709686741, 166.2677522451418213, -5.000000000000041744 ) ) ;
#43595 = CARTESIAN_POINT ( 'NONE',  ( 131.1618259000655371, 246.5333772461660544, 9.188101187500095079 ) ) ;
#43596 = VERTEX_POINT ( 'NONE', #97993 ) ;
#43597 = DIRECTION ( 'NONE',  ( -0.9995486091367050685, 0.03004293549036784680, 0.000000000000000000 ) ) ;
#43598 = CARTESIAN_POINT ( 'NONE',  ( 74.67000616351420206, 66.81477949400924388, -13.12245706047550797 ) ) ;
#43599 = CARTESIAN_POINT ( 'NONE',  ( 202.9490938173916561, 279.1288534886517709, -16.56031645010252973 ) ) ;
#43600 = B_SPLINE_CURVE_WITH_KNOTS ( 'NONE', 3,
 ( #1278, #77270, #39732, #46867 ),
 .UNSPECIFIED., .F., .F.,
 ( 4, 4 ),
 ( 0.000000000000000000, 0.001628043935741951614 ),
 .UNSPECIFIED. ) ;
#43601 = CARTESIAN_POINT ( 'NONE',  ( 204.2556901454867955, 276.8657622634082713, 13.61111001399713949 ) ) ;
#43602 = CARTESIAN_POINT ( 'NONE',  ( 73.71376407998293701, 56.08882236293795387, 16.08428922147598428 ) ) ;
#43603 = CARTESIAN_POINT ( 'NONE',  ( -2.073866539663252073, 26.60322154129611505, -10.00000000000000000 ) ) ;
#43604 = ORIENTED_EDGE ( 'NONE', *, *, #49962, .T. ) ;
#43605 = CARTESIAN_POINT ( 'NONE',  ( 77.54335625564391421, 61.27816323999952175, 15.77127415614125461 ) ) ;
#43606 = CARTESIAN_POINT ( 'NONE',  ( 182.3261756823741564, 275.2222332755986827, -16.67497698087158753 ) ) ;
#43607 = CARTESIAN_POINT ( 'NONE',  ( 72.53840899933517505, 71.27365409391698847, -6.036301325323600864 ) ) ;
#43608 = CARTESIAN_POINT ( 'NONE',  ( 38.49039832772786696, 181.4824982072973683, 3.021315404115420679E-15 ) ) ;
#43609 = CARTESIAN_POINT ( 'NONE',  ( 73.66740156979760457, 69.66397881967726846, -9.561189449020471187 ) ) ;
#43610 = CARTESIAN_POINT ( 'NONE',  ( 195.7820092358261093, 263.4657121749461339, 0.8738221391051791409 ) ) ;
#43611 = CARTESIAN_POINT ( 'NONE',  ( 28.67313202272483252, 177.3615022471902023, 5.000000000000051514 ) ) ;
#43612 = DIRECTION ( 'NONE',  ( -0.000000000000000000, -0.000000000000000000, -1.000000000000000000 ) ) ;
#43614 = CARTESIAN_POINT ( 'NONE',  ( 192.9666104369811990, 268.2690024003410372, 12.61864968089833638 ) ) ;
#43613 = B_SPLINE_CURVE_WITH_KNOTS ( 'NONE', 3,
 ( #39898, #14631, #45512, #69323 ),
 .UNSPECIFIED., .F., .F.,
 ( 4, 4 ),
 ( 0.000000000000000000, 0.007933777700369805050 ),
 .UNSPECIFIED. ) ;
#43615 = CARTESIAN_POINT ( 'NONE',  ( 21.61359102238895957, 12.28848085856230732, 1.475505719884397138E-15 ) ) ;
#43616 = CARTESIAN_POINT ( 'NONE',  ( 148.9498507103374152, 272.6582861203333437, 11.90061892622094852 ) ) ;
#43617 = CARTESIAN_POINT ( 'NONE',  ( 71.24263041127305485, 223.4860189848785410, -2.679491924311252493 ) ) ;
#43618 = LINE ( 'NONE', #5135, #51501 ) ;
#43619 = FACE_OUTER_BOUND ( 'NONE', #93995, .T. ) ;
#43620 = CARTESIAN_POINT ( 'NONE',  ( 72.28313422013535217, 71.96753738583048232, -3.711430182928289856 ) ) ;
#43621 = CARTESIAN_POINT ( 'NONE',  ( 140.7332108297008801, 245.3927522451417929, -10.00000000000009059 ) ) ;
#43622 = CARTESIAN_POINT ( 'NONE',  ( 175.9939695555370065, 285.4482173679398898, -11.95632612277833040 ) ) ;
#43623 = ORIENTED_EDGE ( 'NONE', *, *, #99221, .F. ) ;
#43624 = EDGE_CURVE ( 'NONE', #56647, #74262, #53930, .T. ) ;
#43625 = VECTOR ( 'NONE', #19455, 1000.000000000000114 ) ;
#43626 = CARTESIAN_POINT ( 'NONE',  ( 66.82592210189895354, 67.33918606646240335, -6.964996463769947965 ) ) ;
#43627 = CARTESIAN_POINT ( 'NONE',  ( 150.9363692955544991, 269.2175350005573478, -14.27857383982596140 ) ) ;
#43628 = CARTESIAN_POINT ( 'NONE',  ( -6.076397627723526540, 176.4869531367911293, 4.594050593750046652 ) ) ;
#43629 = CARTESIAN_POINT ( 'NONE',  ( 63.26028190641562787, 198.1423013555410080, -4.594050593750043987 ) ) ;
#43630 = CARTESIAN_POINT ( 'NONE',  ( 178.6427318236586359, 259.2647235818225226, -10.45271603834399876 ) ) ;
#43631 = CARTESIAN_POINT ( 'NONE',  ( 27.61987535298997187, 21.11029122506295508, -8.090169943749478065 ) ) ;
#43632 = CARTESIAN_POINT ( 'NONE',  ( 85.43645318413936707, 48.61927365843763482, 12.47466632846418122 ) ) ;
#43633 = CARTESIAN_POINT ( 'NONE',  ( 204.6475128369918082, 276.1871054541632020, -13.72068618491070779 ) ) ;
#43634 = CARTESIAN_POINT ( 'NONE',  ( 190.8458701802819064, 291.3353758386331833, -14.35470056613957723 ) ) ;
#43635 = CARTESIAN_POINT ( 'NONE',  ( 148.9635810001525726, 275.9368111177387846, 3.718913479852709703 ) ) ;
#43636 = CARTESIAN_POINT ( 'NONE',  ( 167.3905708005187591, 256.8461950526155988, 14.46083098827760693 ) ) ;
#43637 = CARTESIAN_POINT ( 'NONE',  ( 75.25170673533752108, 66.73598490943447814, 12.94887977284632896 ) ) ;
#43638 = EDGE_CURVE ( 'NONE', #82969, #66038, #89440, .T. ) ;
#43639 = CARTESIAN_POINT ( 'NONE',  ( 150.2494575935072874, 270.4073009688167986, 14.61449051812962985 ) ) ;
#43640 = ADVANCED_FACE ( 'NONE', ( #98502 ), #29092, .F. ) ;
#43641 = VECTOR ( 'NONE', #94509, 1000.000000000000000 ) ;
#43642 = CARTESIAN_POINT ( 'NONE',  ( 62.44812277031795134, 196.8615022471901739, 5.000000000000051514 ) ) ;
#43643 = CARTESIAN_POINT ( 'NONE',  ( 182.4321081115337222, 291.9834752246442235, 9.344615119188279806 ) ) ;
#43644 = CARTESIAN_POINT ( 'NONE',  ( 189.8480911035503880, 301.8204558191226283, -0.8992086515915015399 ) ) ;
#43645 = CARTESIAN_POINT ( 'NONE',  ( 23.01690360248371903, 184.0958772461660544, -9.188101187500095079 ) ) ;
#43646 = CARTESIAN_POINT ( 'NONE',  ( 168.2447061861834072, 286.2798532801800775, 4.135845175375446381 ) ) ;
#43647 = CARTESIAN_POINT ( 'NONE',  ( 192.4454213697443095, 297.3217478340386606, 12.58566886711101596 ) ) ;
#43648 = CARTESIAN_POINT ( 'NONE',  ( 34.56506555475243658, 38.14336893147758900, 7.433330006724141015 ) ) ;
#43649 = CARTESIAN_POINT ( 'NONE',  ( 144.1251436611898953, 244.0177522451417644, 5.000000000000051514 ) ) ;
#43650 = CARTESIAN_POINT ( 'NONE',  ( 180.4127669783307795, 277.2432443295738267, 16.31949751863770359 ) ) ;
#43651 = CARTESIAN_POINT ( 'NONE',  ( 25.38349897777161601, 16.78380873178787169, -6.180339887498949025 ) ) ;
#43652 = CARTESIAN_POINT ( 'NONE',  ( 114.3892930691446850, 248.3967562850347122, -4.648177544792955347E-16 ) ) ;
#43653 = CARTESIAN_POINT ( 'NONE',  ( -19.92236680055716391, 153.5313752282681605, 5.249404841173988696E-14 ) ) ;
#43654 = SHAPE_DEFINITION_REPRESENTATION ( #41872, #67038 ) ;
#43655 = CARTESIAN_POINT ( 'NONE',  ( 11.06573324809563807, 29.49540643055186351, 3.479690158560446702E-15 ) ) ;
#43656 = CARTESIAN_POINT ( 'NONE',  ( 71.61987371496263677, 72.44464069648768145, 0.9664813023029263928 ) ) ;
#43657 = CARTESIAN_POINT ( 'NONE',  ( 201.5232667746729760, 270.7243246684459450, 10.73244273373618718 ) ) ;
#43658 = CARTESIAN_POINT ( 'NONE',  ( 185.6872253078315964, 257.5179133167785608, -1.638249339750624589 ) ) ;
#43659 = CARTESIAN_POINT ( 'NONE',  ( 191.2663728242109187, 269.6285576558835260, -14.72094365787478232 ) ) ;
#43660 = ORIENTED_EDGE ( 'NONE', *, *, #75142, .F. ) ;
#43661 = CARTESIAN_POINT ( 'NONE',  ( 181.7743748161887822, 289.6841531283870381, 12.89587171145656974 ) ) ;
#43662 = CARTESIAN_POINT ( 'NONE',  ( 156.7717313778066455, 276.4859198570546255, 10.27056923680294354 ) ) ;
#43663 = LINE ( 'NONE', #96930, #19772 ) ;
#43664 = DIRECTION ( 'NONE',  ( -0.000000000000000000, 0.000000000000000000, 1.000000000000000000 ) ) ;
#43665 = ORIENTED_EDGE ( 'NONE', *, *, #47299, .T. ) ;
#43667 = CARTESIAN_POINT ( 'NONE',  ( 152.6364317663293946, 268.0951475544519553, 15.85731527355114778 ) ) ;
#43666 =( BOUNDED_CURVE ( )  B_SPLINE_CURVE ( 2, ( #53757, #51801, #68471, #46153, #84230, #83725, #98407, #84716, #14283 ),
 .UNSPECIFIED., .F., .T. ) 
 B_SPLINE_CURVE_WITH_KNOTS ( ( 3, 2, 2, 2, 3 ),
 ( 0.3830645161290322509, 0.3844086021505376261, 0.3870967741935483764, 0.3897849462365591267, 0.3911290322580645018 ),
 .UNSPECIFIED. ) 
 CURVE ( )  GEOMETRIC_REPRESENTATION_ITEM ( )  RATIONAL_B_SPLINE_CURVE ( ( 0.9330127018922194093, 0.9330127018922194093, 1.000000000000000000, 0.8660254037844387076, 1.000000000000000000, 0.8660254037844387076, 1.000000000000000000, 0.9330127018922194093, 0.9330127018922194093 ) ) 
 REPRESENTATION_ITEM ( '' )  );
#43668 = DIRECTION ( 'NONE',  ( 0.000000000000000000, -0.000000000000000000, -1.000000000000000000 ) ) ;
#43669 = CARTESIAN_POINT ( 'NONE',  ( 176.6558404752379090, 252.2237374370411942, -0.2705739152901737166 ) ) ;
#43670 = CARTESIAN_POINT ( 'NONE',  ( 154.9048824156581361, 262.3438686460345366, -17.40627786727128168 ) ) ;
#43671 = ORIENTED_EDGE ( 'NONE', *, *, #69535, .T. ) ;
#43672 = VERTEX_POINT ( 'NONE', #12399 ) ;
#43673 = EDGE_CURVE ( 'NONE', #4704, #35604, #76910, .T. ) ;
#43675 = CARTESIAN_POINT ( 'NONE',  ( 204.4781092559247782, 276.4805210635553863, 13.30606382016679490 ) ) ;
#43674 = LINE ( 'NONE', #4181, #81088 ) ;
#43676 = CARTESIAN_POINT ( 'NONE',  ( 152.6615646578087819, 266.2294089801508221, 16.94722993326405813 ) ) ;
#43677 = ORIENTED_EDGE ( 'NONE', *, *, #22287, .F. ) ;
#43678 = CARTESIAN_POINT ( 'NONE',  ( 194.3452430042056847, 293.4673175397701357, -14.50972866970454866 ) ) ;
#43679 = CARTESIAN_POINT ( 'NONE',  ( 80.38386138148599969, 57.79680026592914999, 16.59996232260768778 ) ) ;
#43680 = CARTESIAN_POINT ( 'NONE',  ( 174.4937798827906192, 262.3286410478639823, 14.41242922277202965 ) ) ;
#43681 = EDGE_LOOP ( 'NONE', ( #63779, #69378, #87952, #61663, #83520, #35695, #98437 ) ) ;
#43682 = DIRECTION ( 'NONE',  ( -0.8660254037844387076, -0.4999999999999998890, -0.000000000000000000 ) ) ;
#43683 = ADVANCED_FACE ( 'NONE', ( #52864 ), #45265, .T. ) ;
#43684 = EDGE_CURVE ( 'NONE', #97801, #98545, #57203, .T. ) ;
#43685 = EDGE_LOOP ( 'NONE', ( #1312, #97512, #97271, #37971, #82875 ) ) ;
#43686 = CARTESIAN_POINT ( 'NONE',  ( 165.0565241268390366, 244.7607094220335568, 2.191926263411719589 ) ) ;
#43687 = EDGE_CURVE ( 'NONE', #47416, #7762, #18996, .T. ) ;
#43688 = CARTESIAN_POINT ( 'NONE',  ( 151.1866278134736206, 275.4563625138778207, -8.238537655447901287 ) ) ;
#43689 = ORIENTED_EDGE ( 'NONE', *, *, #69842, .T. ) ;
#43690 = CARTESIAN_POINT ( 'NONE',  ( 177.6370681238493603, 279.4364947633008569, -16.61177670297263376 ) ) ;
#43691 = CARTESIAN_POINT ( 'NONE',  ( 169.0811126367664485, 261.3667313283961562, -16.44051657199686289 ) ) ;
#43692 = VERTEX_POINT ( 'NONE', #79217 ) ;
#43693 = CARTESIAN_POINT ( 'NONE',  ( 50.59379163489128928, 94.40700863652010355, -10.00000000000000000 ) ) ;
#43694 = ORIENTED_EDGE ( 'NONE', *, *, #37703, .T. ) ;
#43695 = CARTESIAN_POINT ( 'NONE',  ( 157.4694053559891529, 268.9764842683514985, 15.59267564261065431 ) ) ;
#43696 = ORIENTED_EDGE ( 'NONE', *, *, #48827, .F. ) ;
#43697 = CARTESIAN_POINT ( 'NONE',  ( 156.6075427607332244, 266.5381846890032875, -16.22512947928903415 ) ) ;
#43698 = CARTESIAN_POINT ( 'NONE',  ( 190.1752790837055045, 301.2537496138681945, -5.177773110520776711 ) ) ;
#43699 = CARTESIAN_POINT ( 'NONE',  ( 82.98423510826575011, 53.52344736239029288, 15.67380116644083721 ) ) ;
#43700 = CARTESIAN_POINT ( 'NONE',  ( 148.9230895364621574, 272.7046378331555161, 12.20434325797056019 ) ) ;
#43701 = CARTESIAN_POINT ( 'NONE',  ( 192.8323852661406761, 296.6515067047851062, 11.86505947732313615 ) ) ;
#43703 = LINE ( 'NONE', #87895, #27314 ) ;
#43702 = VECTOR ( 'NONE', #14992, 1000.000000000000000 ) ;
#43704 = CARTESIAN_POINT ( 'NONE',  ( 158.8123895076641077, 255.5758678317443469, -17.62141936352351479 ) ) ;
#43705 = ORIENTED_EDGE ( 'NONE', *, *, #2043, .T. ) ;
#43706 = CARTESIAN_POINT ( 'NONE',  ( 81.37674444193763179, 55.19836804271280783, -15.94010240901345199 ) ) ;
#43707 = CARTESIAN_POINT ( 'NONE',  ( 38.01218019840322881, 27.11029122506296929, -8.090169943749478065 ) ) ;
#43708 = CARTESIAN_POINT ( 'NONE',  ( 206.2456893945931142, 273.4189824569319285, 10.13882547285618152 ) ) ;
#43709 = CARTESIAN_POINT ( 'NONE',  ( 159.8655504377736918, 253.7517395922482706, 15.51368179719542262 ) ) ;
#43710 = CARTESIAN_POINT ( 'NONE',  ( 206.3023480738090996, 271.3208467458289874, 7.632938913807082670 ) ) ;
#43711 = CARTESIAN_POINT ( 'NONE',  ( 176.8206666507760474, 289.6423215265738804, -9.013642675727712827 ) ) ;
#43712 = ORIENTED_EDGE ( 'NONE', *, *, #40470, .T. ) ;
#43713 = CARTESIAN_POINT ( 'NONE',  ( 76.98069296933027772, 53.91054578136119346, -16.01903993249421632 ) ) ;
#43714 = DIRECTION ( 'NONE',  ( -0.000000000000000000, -0.000000000000000000, -1.000000000000000000 ) ) ;
#43715 = CARTESIAN_POINT ( 'NONE',  ( 198.6774775476553714, 286.5275098982731379, -17.42299212369177752 ) ) ;
#43716 = CARTESIAN_POINT ( 'NONE',  ( 99.75938391669748739, 221.7365022471902023, 10.00000000000009948 ) ) ;
#43717 = VECTOR ( 'NONE', #42233, 1000.000000000000114 ) ;
#43718 = EDGE_LOOP ( 'NONE', ( #65056, #29176, #19054, #76539 ) ) ;
#43719 = CARTESIAN_POINT ( 'NONE',  ( -11.40312891409031693, 78.77562236714182120, 52.49999999999999289 ) ) ;
#43720 = CARTESIAN_POINT ( 'NONE',  ( 205.6720057621449484, 274.0264657029327964, 10.42642860073514299 ) ) ;
#43721 = CARTESIAN_POINT ( 'NONE',  ( 200.9521687275011175, 282.5876292032514243, -18.16013154125647944 ) ) ;
#43723 = ADVANCED_FACE ( 'NONE', ( #18380 ), #48271, .F. ) ;
#43722 = CARTESIAN_POINT ( 'NONE',  ( 164.3524132573224392, 245.9802652221976587, -2.749586949851067441 ) ) ;
#43724 = CARTESIAN_POINT ( 'NONE',  ( 41.86197723097744472, 181.6427522451417644, 1.119607411625061291E-15 ) ) ;
#43725 = CARTESIAN_POINT ( 'NONE',  ( 106.6962611473900893, 244.6589784336661069, -6.496448406907676862E-16 ) ) ;
#43726 = CARTESIAN_POINT ( 'NONE',  ( 180.8261506122944979, 294.1084290502871568, -2.669056545970062810 ) ) ;
#43727 = CARTESIAN_POINT ( 'NONE',  ( 167.9232164608807807, 282.0145233034614876, -10.83756476677490710 ) ) ;
#43728 = CARTESIAN_POINT ( 'NONE',  ( 84.56517416216006211, 50.64586678990350777, 13.69612687457570033 ) ) ;
#43729 = CARTESIAN_POINT ( 'NONE',  ( 208.3490404761574553, 269.7758715175073689, 2.423947743236856578 ) ) ;
#43730 = CARTESIAN_POINT ( 'NONE',  ( 32.46173284068399312, 198.7369531367911293, -4.594050593750048428 ) ) ;
#43731 = DIRECTION ( 'NONE',  ( -0.000000000000000000, -0.000000000000000000, -1.000000000000000000 ) ) ;
#43732 = VERTEX_POINT ( 'NONE', #94405 ) ;
#43733 = ORIENTED_EDGE ( 'NONE', *, *, #77679, .F. ) ;
#43734 = CARTESIAN_POINT ( 'NONE',  ( 191.3941823605357229, 298.7337486089482468, 7.883234235473491225 ) ) ;
#43735 = CARTESIAN_POINT ( 'NONE',  ( 74.41897651308048012, 68.01641561303326000, -11.65844777088098461 ) ) ;
#43736 = CYLINDRICAL_SURFACE ( 'NONE', #15812, 10.00000000000010658 ) ;
#43737 = CARTESIAN_POINT ( 'NONE',  ( 190.3791419447713906, 300.9006487807255326, -5.688668718458480988 ) ) ;
#43738 = CARTESIAN_POINT ( 'NONE',  ( 106.0403798229140477, 220.4824982072973683, 3.021315404115420679E-15 ) ) ;
#43739 = CARTESIAN_POINT ( 'NONE',  ( 161.8839333999304415, 250.2557977526613229, -13.90128376743482441 ) ) ;
#43740 = CARTESIAN_POINT ( 'NONE',  ( 49.06003799288187395, 95.45573527953635562, -10.00000000000000000 ) ) ;
#43741 = CARTESIAN_POINT ( 'NONE',  ( 164.2609264239344213, 250.0470742514019378, 10.21728485584155699 ) ) ;
#43742 = CARTESIAN_POINT ( 'NONE',  ( 92.59663213601572807, 234.2677522451419065, -5.000000000000047962 ) ) ;
#43743 = ORIENTED_EDGE ( 'NONE', *, *, #99241, .T. ) ;
#43744 = CARTESIAN_POINT ( 'NONE',  ( 197.6218578199255376, 267.6909935936381544, -7.901084308168314863 ) ) ;
#43745 = EDGE_CURVE ( 'NONE', #58927, #53652, #2347, .T. ) ;
#43746 = CARTESIAN_POINT ( 'NONE',  ( 162.8042930031641049, 248.6616881586264469, 11.14389129512055554 ) ) ;
#43747 = CARTESIAN_POINT ( 'NONE',  ( 207.5959034698703078, 271.0803430774575418, -1.830000129038042544 ) ) ;
#43748 = CARTESIAN_POINT ( 'NONE',  ( 19.71535529843806245, 176.0643266524160424, 9.188101187500095079 ) ) ;
#43749 = CARTESIAN_POINT ( 'NONE',  ( 13.50136424336972141, 8.764269794150880699, 3.090169943749476733 ) ) ;
#43750 = CARTESIAN_POINT ( 'NONE',  ( 79.11275361910446691, 46.11146926033848104, 13.27945046499836579 ) ) ;
#43751 = CARTESIAN_POINT ( 'NONE',  ( 71.64977493859507263, 59.13526382602540821, -15.32350604844225295 ) ) ;
#43752 = CARTESIAN_POINT ( 'NONE',  ( 73.67278091869266632, 69.61283722901053750, 9.621970401190987232 ) ) ;
#43753 = CARTESIAN_POINT ( 'NONE',  ( 207.5195222358739784, 271.2126392554839640, 2.810970398613041432 ) ) ;
#43754 = CARTESIAN_POINT ( 'NONE',  ( 203.6857291523390074, 276.2442838610515423, 13.33094155839203587 ) ) ;
#43755 = EDGE_CURVE ( 'NONE', #41607, #17175, #15248, .T. ) ;
#43756 = CARTESIAN_POINT ( 'NONE',  ( 70.86977990947116268, 70.80167083835577557, 4.702927032916670136 ) ) ;
#43757 = CARTESIAN_POINT ( 'NONE',  ( 207.4764081617721843, 271.2873150223495600, 6.359972247200924578 ) ) ;
#43758 = ORIENTED_EDGE ( 'NONE', *, *, #8741, .F. ) ;
#43759 = B_SPLINE_CURVE_WITH_KNOTS ( 'NONE', 3,
 ( #20724, #19731, #12627, #43497, #66801, #74927, #67299, #74439, #82058, #58686, #91143, #37391, #97728, #75420, #35405, #5509 ),
 .UNSPECIFIED., .F., .F.,
 ( 4, 1, 2, 2, 2, 1, 2, 2, 4 ),
 ( 0.000000000000000000, 0.1249999999999976685, 0.1874999999999985012, 0.2499999999999993339, 0.5000000000000033307, 0.6250000000000053291, 0.6875000000000044409, 0.7500000000000035527, 1.000000000000000000 ),
 .UNSPECIFIED. ) ;
#43760 = EDGE_CURVE ( 'NONE', #58606, #35725, #48782, .T. ) ;
#43761 = CARTESIAN_POINT ( 'NONE',  ( 164.4989226152910646, 245.7265035704120351, -6.575810094723514965 ) ) ;
#43762 = CARTESIAN_POINT ( 'NONE',  ( 12.21864935082045456, 177.8615022471902591, -10.00000000000009592 ) ) ;
#43763 = CARTESIAN_POINT ( 'NONE',  ( 80.07812099633126479, 57.44764983040322903, -16.59488970948942921 ) ) ;
#43764 = CARTESIAN_POINT ( 'NONE',  ( 130.8910194135003735, 252.5024278399160949, 9.188101187500095079 ) ) ;
#43765 = CARTESIAN_POINT ( 'NONE',  ( 27.91230638117223606, 28.06628583063842797, -9.188101187500006262 ) ) ;
#43766 = CARTESIAN_POINT ( 'NONE',  ( 164.2980263007286226, 246.0744661942869982, 1.511195434064211529 ) ) ;
#43767 = CARTESIAN_POINT ( 'NONE',  ( 83.82065378329919270, 51.84410121092205515, -14.88618515114630370 ) ) ;
#43768 = CARTESIAN_POINT ( 'NONE',  ( 177.7634369230092091, 252.8608366103077856, -4.270187854574569275E-12 ) ) ;
#43770 = CARTESIAN_POINT ( 'NONE',  ( 75.27726335905293809, 66.87231400452490959, 13.31561030640130738 ) ) ;
#43769 = CARTESIAN_POINT ( 'NONE',  ( 180.6665526851674599, 287.6815954905284798, 14.11204521094005671 ) ) ;
#43771 = CARTESIAN_POINT ( 'NONE',  ( 68.53512761445865920, 64.30306519794643805, 11.73731604961160180 ) ) ;
#43772 = VERTEX_POINT ( 'NONE', #18886 ) ;
#43773 = CARTESIAN_POINT ( 'NONE',  ( 151.2648146047323507, 268.6486510375538614, 15.71323890031163550 ) ) ;
#43774 = CARTESIAN_POINT ( 'NONE',  ( 163.6887036115909666, 247.1298440500783613, 7.368436217261104204 ) ) ;
#43775 = CARTESIAN_POINT ( 'NONE',  ( 70.93378986505813089, 67.06125297378586936, -11.22077736235704926 ) ) ;
#43776 = CARTESIAN_POINT ( 'NONE',  ( 170.3310799939524429, 266.5390996155348944, -16.61713687241611836 ) ) ;
#43777 = CARTESIAN_POINT ( 'NONE',  ( 9.573022157908470220, 14.03085787977760823, 9.188101187500006262 ) ) ;
#43778 = ORIENTED_EDGE ( 'NONE', *, *, #25483, .F. ) ;
#43779 = PLANE ( 'NONE',  #81345 ) ;
#43780 = CARTESIAN_POINT ( 'NONE',  ( 168.8507326547640162, 282.4667480612920372, -10.92933487478789445 ) ) ;
#43781 = B_SPLINE_CURVE_WITH_KNOTS ( 'NONE', 3,
 ( #89936, #34694, #66101, #73710, #65595, #36182, #96545, #97049, #27617, #20014, #50891, #81839, #88980, #88469, #12416, #43782, #27116, #94667, #19534, #20514, #57999, #12923, #74727, #49903, #80861, #67087, #50396, #43283, #35699, #74228, #11434, #4293, #98010, #97525, #28095, #58966, #73220, #81350, #28588, #51390, #3813, #82355, #86589, #48020, #9551, #11920 ),
 .UNSPECIFIED., .F., .F.,
 ( 4, 1, 1, 1, 2, 2, 1, 1, 1, 2, 2, 1, 1, 2, 2, 1, 1, 2, 2, 1, 1, 2, 2, 1, 2, 2, 1, 2, 2, 4 ),
 ( 0.000000000000000000, 0.06249999999999292233, 0.09374999999998942513, 0.1093749999999886896, 0.1171874999999882455, 0.1249999999999877875, 0.1874999999999923672, 0.2187499999999937550, 0.2343749999999936162, 0.2421874999999925615, 0.2499999999999915068, 0.3124999999999931721, 0.3437499999999940603, 0.3593749999999954481, 0.3749999999999968359, 0.4374999999999996114, 0.4687499999999996114, 0.4843749999999998335, 0.5000000000000000000, 0.5624999999999985567, 0.5937499999999972244, 0.6093749999999973355, 0.6249999999999974465, 0.6874999999999983347, 0.7187499999999987788, 0.7499999999999992228, 0.8125000000000003331, 0.8437500000000008882, 0.8750000000000014433, 1.000000000000000000 ),
 .UNSPECIFIED. ) ;
#43782 = CARTESIAN_POINT ( 'NONE',  ( 83.81822528977980369, 42.74170432803968112, 5.348213412007799761 ) ) ;
#43783 = LINE ( 'NONE', #5306, #90924 ) ;
#43784 = CARTESIAN_POINT ( 'NONE',  ( 185.4867332780130766, 297.4061142773095412, 5.671143563000668131 ) ) ;
#43785 = CARTESIAN_POINT ( 'NONE',  ( 138.6583583033484786, 260.8615022471902876, 5.000000000000046185 ) ) ;
#43786 = AXIS2_PLACEMENT_3D ( 'NONE', #92482, #63542, #15941 ) ;
#43787 = CARTESIAN_POINT ( 'NONE',  ( 148.8081469520198539, 276.3561860483582109, -0.0002503201696655007265 ) ) ;
#43788 = CARTESIAN_POINT ( 'NONE',  ( 74.23555041547365363, 68.49601928387087924, -11.11897725275786719 ) ) ;
#43789 = EDGE_CURVE ( 'NONE', #20199, #17038, #27421, .T. ) ;
#43790 = CARTESIAN_POINT ( 'NONE',  ( 15.11407551230992219, 32.30945333909093620, -10.00000000000000000 ) ) ;
#43791 = CARTESIAN_POINT ( 'NONE',  ( 19.29290913472606661, 12.10801979619928126, 3.090169943749476733 ) ) ;
#43792 = CARTESIAN_POINT ( 'NONE',  ( 84.31969329757113485, 49.65246679347950476, 13.61885025447953979 ) ) ;
#43793 = ORIENTED_EDGE ( 'NONE', *, *, #15702, .T. ) ;
#43794 = FACE_OUTER_BOUND ( 'NONE', #39555, .T. ) ;
#43795 = CARTESIAN_POINT ( 'NONE',  ( 86.37995054896607883, 46.98508828575033647, -10.52062608394495591 ) ) ;
#43796 = CARTESIAN_POINT ( 'NONE',  ( 156.0331829292964017, 261.8985861856509700, -16.97186308071531258 ) ) ;
#43798 = ORIENTED_EDGE ( 'NONE', *, *, #27210, .T. ) ;
#43797 = B_SPLINE_CURVE_WITH_KNOTS ( 'NONE', 3,
 ( #55578, #16100, #85035, #47003 ),
 .UNSPECIFIED., .F., .F.,
 ( 4, 4 ),
 ( 0.04853013625147470367, 0.04887120950165269734 ),
 .UNSPECIFIED. ) ;
#43799 = CARTESIAN_POINT ( 'NONE',  ( 191.7741832257749195, 298.4843664033717801, -8.615487418695501276 ) ) ;
#43800 = CARTESIAN_POINT ( 'NONE',  ( 185.7027875752530406, 291.1743587175776611, 12.16933810580360387 ) ) ;
#43801 = B_SPLINE_CURVE_WITH_KNOTS ( 'NONE', 3,
 ( #8404, #45395, #39275, #38283, #62577, #54991, #70185, #793, #39766, #94041, #84444, #14989, #24592, #24095, #47392, #14513, #76325, #45876, #68690, #30201, #7393, #61588, #2320, #41282, #79352, #10412, #72737, #33200, #3328, #16988, #65100, #33719, #48912, #64101, #32696, #87971, #71727, #95047, #55970, #82216, #25610, #34208, #2829, #94536, #72224, #18515, #47879, #79846, #64609, #12788, #56497, #20377 ),
 .UNSPECIFIED., .F., .F.,
 ( 4, 2, 2, 2, 2, 2, 2, 2, 2, 2, 2, 2, 2, 2, 2, 2, 2, 2, 2, 2, 2, 2, 2, 2, 2, 4 ),
 ( 9.788385118261326871E-05, 0.001114237024482954202, 0.001368325317808037796, 0.001622413611133120956, 0.001749457757795665463, 0.001876501904458209753, 0.002003546051120754044, 0.002130590197783298334, 0.002384678491108393854, 0.002638766784433488506, 0.003146943371083746766, 0.004163296544384260250, 0.005179649717684773301, 0.005687826304335072761, 0.005941914597660264558, 0.006068958744322860456, 0.006196002890985456354, 0.006259524964316822392, 0.006323047037648188429, 0.006450091184311090506, 0.006704179477637036040, 0.006958267770962981574, 0.007212356064288926241, 0.007466444357614864837, 0.007720532650940801697, 0.008228709237592696235 ),
 .UNSPECIFIED. ) ;
#43802 = CARTESIAN_POINT ( 'NONE',  ( 166.0742539356187706, 262.7740412608126803, -17.50261138965781527 ) ) ;
#43803 = DIRECTION ( 'NONE',  ( 0.8660254037844383745, 0.5000000000000003331, -0.000000000000000000 ) ) ;
#43804 = ORIENTED_EDGE ( 'NONE', *, *, #21458, .T. ) ;
#43805 = CARTESIAN_POINT ( 'NONE',  ( 84.74801659416949917, 228.9244531367911293, -4.594050593750046652 ) ) ;
#43806 = CARTESIAN_POINT ( 'NONE',  ( 155.2775459039818315, 261.6983965501318039, 17.03612935257831040 ) ) ;
#43807 = CARTESIAN_POINT ( 'NONE',  ( 73.34867049892106650, 70.14346970443526175, -9.354907352444854496 ) ) ;
#43808 = CARTESIAN_POINT ( 'NONE',  ( 181.3346534254663140, 271.3440730695800767, -17.45372068697093226 ) ) ;
#43809 = CARTESIAN_POINT ( 'NONE',  ( 184.9070598923041473, 259.8481512251225354, -5.813936190556519890 ) ) ;
#43810 = B_SPLINE_CURVE_WITH_KNOTS ( 'NONE', 3,
 ( #56040, #17565, #33793, #79414, #80925, #3393, #88034, #48473, #26175, #95626, #34267, #19091, #2385, #64167, #27176, #33265, #58064, #88530, #25680, #49970, #65162, #57052, #18582, #11495, #58547, #4879, #50457, #89999, #59533, #51961, #12987, #74296, #60033, #5858, #97111, #13956, #90512, #51454, #27680, #89520, #73773, #44837, #13473, #90998, #81903, #82901, #43847, #74786, #12480, #44342, #20080, #35760 ),
 .UNSPECIFIED., .F., .F.,
 ( 4, 2, 2, 2, 2, 2, 2, 2, 2, 2, 2, 2, 2, 2, 2, 2, 2, 2, 2, 2, 2, 2, 2, 2, 2, 4 ),
 ( 0.001584306797643239388, 0.002043180208590379687, 0.002502053619537519553, 0.002731490325011090570, 0.002846208677747904918, 0.002960927030484718833, 0.003075645383221533181, 0.003190363735958347095, 0.003419800441431977527, 0.003878673852379238389, 0.004337547263326498384, 0.005255294085221049599, 0.006173040907115600814, 0.006631914318062911984, 0.007090787729010222286, 0.007205506081747125972, 0.007262865258115577816, 0.007320224434484028792, 0.007434942787220981918, 0.007549661139957934176, 0.007779097845431880327, 0.008008534550905825611, 0.008237971256379771762, 0.008467407961853717913, 0.008696844667327664063, 0.008926281372801610214 ),
 .UNSPECIFIED. ) ;
#43811 = ORIENTED_EDGE ( 'NONE', *, *, #64237, .F. ) ;
#43812 = EDGE_CURVE ( 'NONE', #64017, #99390, #44245, .T. ) ;
#43813 = ORIENTED_EDGE ( 'NONE', *, *, #45583, .F. ) ;
#43814 = CARTESIAN_POINT ( 'NONE',  ( -11.83159780365783398, 170.6427522451419065, 10.00000000000009415 ) ) ;
#43815 = ORIENTED_EDGE ( 'NONE', *, *, #67126, .T. ) ;
#43816 = CARTESIAN_POINT ( 'NONE',  ( 81.94787918575768515, 52.94560862287604408, 15.29677040454687642 ) ) ;
#43817 = ORIENTED_EDGE ( 'NONE', *, *, #41544, .T. ) ;
#43818 = CARTESIAN_POINT ( 'NONE',  ( 205.4228510824199248, 268.8300068208707785, 0.2998358105646597993 ) ) ;
#43819 = CARTESIAN_POINT ( 'NONE',  ( 155.3250150347760723, 261.6161776038049425, -18.57420904020362684 ) ) ;
#43820 = ORIENTED_EDGE ( 'NONE', *, *, #4708, .T. ) ;
#43821 = CARTESIAN_POINT ( 'NONE',  ( 206.8268337557409211, 272.4124108968919131, -7.200219557041771523 ) ) ;
#43822 = CARTESIAN_POINT ( 'NONE',  ( 87.62133583293774564, 45.31115884160843876, -7.293173845241961217 ) ) ;
#43823 = DIRECTION ( 'NONE',  ( 0.4972609476841349796, -0.8612812260087746585, 0.1045284632676570652 ) ) ;
#43824 = CARTESIAN_POINT ( 'NONE',  ( 19.28323191311993057, 170.3932355074535678, -2.679491924311248496 ) ) ;
#43825 = CARTESIAN_POINT ( 'NONE',  ( 72.02695394113958116, 68.29673134482877117, -9.986728363011483367 ) ) ;
#43826 = CARTESIAN_POINT ( 'NONE',  ( 157.1282499545302755, 258.4928831048084135, -18.43070736571433699 ) ) ;
#43827 = VERTEX_POINT ( 'NONE', #88835 ) ;
#43828 = CARTESIAN_POINT ( 'NONE',  ( 76.46110298587262832, 58.51621405362541850, 16.04222249715220983 ) ) ;
#43829 = CARTESIAN_POINT ( 'NONE',  ( 4.886862741447147940, 23.79752408145590081, -5.678558825948271327 ) ) ;
#43830 = ADVANCED_FACE ( 'NONE', ( #73089 ), #3683, .T. ) ;
#43831 = ORIENTED_EDGE ( 'NONE', *, *, #67764, .F. ) ;
#43832 = CARTESIAN_POINT ( 'NONE',  ( 41.35966550219792737, 207.3877816888192172, 4.672379723982937232E-14 ) ) ;
#43834 = ORIENTED_EDGE ( 'NONE', *, *, #8899, .T. ) ;
#43833 = CARTESIAN_POINT ( 'NONE',  ( 204.0830486605019871, 271.5957195856256590, 9.804030348223873759 ) ) ;
#43835 = CARTESIAN_POINT ( 'NONE',  ( -15.58608437336083696, 105.6654254483952826, 11.33858688303593709 ) ) ;
#43836 = CARTESIAN_POINT ( 'NONE',  ( 78.12823040285628906, 47.68785961753161473, -13.94170588958538026 ) ) ;
#43837 = PLANE ( 'NONE',  #4244 ) ;
#43838 = CARTESIAN_POINT ( 'NONE',  ( 161.3490137394416877, 281.4934520396691369, -6.492417838214519676 ) ) ;
#43839 = DIRECTION ( 'NONE',  ( -0.8660254037844387076, -0.4999999999999998890, -0.000000000000000000 ) ) ;
#43840 = CARTESIAN_POINT ( 'NONE',  ( 158.4533830096545159, 257.7614088891019719, 17.16045812922167002 ) ) ;
#43841 = CARTESIAN_POINT ( 'NONE',  ( 168.0428203547336921, 252.9999441337117503, 11.78450787674390199 ) ) ;
#43842 = CARTESIAN_POINT ( 'NONE',  ( 88.44266034405603705, 44.03949081389492903, -2.406584733330055847 ) ) ;
#43843 = VERTEX_POINT ( 'NONE', #40148 ) ;
#43844 = CARTESIAN_POINT ( 'NONE',  ( 27.53018959221258655, 41.35687530090520880, 177.5919119679930134 ) ) ;
#43845 = CARTESIAN_POINT ( 'NONE',  ( 71.04498658471177919, 63.38740358822698795, -13.40332908134212175 ) ) ;
#43846 = ORIENTED_EDGE ( 'NONE', *, *, #2048, .F. ) ;
#43847 = CARTESIAN_POINT ( 'NONE',  ( 160.1046313666135177, 276.6195463108357444, 12.87142096350444120 ) ) ;
#43848 = CARTESIAN_POINT ( 'NONE',  ( 86.81641918289878390, 45.77657501471897916, -8.750901752256119437 ) ) ;
#43849 = CARTESIAN_POINT ( 'NONE',  ( -23.47208873469913115, 24.42380372261332155, -10.00000000000000000 ) ) ;
#43850 = CARTESIAN_POINT ( 'NONE',  ( 190.1519139143167081, 301.2942192743771557, 4.481136594690903863 ) ) ;
#43851 = CARTESIAN_POINT ( 'NONE',  ( 164.8351683237598024, 274.0798523170363410, 15.21690876053529706 ) ) ;
#43853 = CARTESIAN_POINT ( 'NONE',  ( 88.27656095359526489, 44.31834822599916635, 2.178649859666209387 ) ) ;
#43852 = CARTESIAN_POINT ( 'NONE',  ( -4.533703103291247594, 174.3149278399161233, 9.188101187500093303 ) ) ;
#43854 = CARTESIAN_POINT ( 'NONE',  ( 203.1946125585645859, 269.9679951457329139, 6.014315348829343044 ) ) ;
#43855 = ORIENTED_EDGE ( 'NONE', *, *, #55293, .F. ) ;
#43856 = ORIENTED_EDGE ( 'NONE', *, *, #19358, .F. ) ;
#43857 = CARTESIAN_POINT ( 'NONE',  ( 30.80155721116056355, 46.36891074996812989, 10.00000000000000000 ) ) ;
#43858 = CARTESIAN_POINT ( 'NONE',  ( 80.56229873119019658, 57.64365382000625715, 16.23737920899276688 ) ) ;
#43859 = DIRECTION ( 'NONE',  ( -0.1039558454088829048, 0.1800568059919617214, 0.9781476007338041345 ) ) ;
#43860 = CARTESIAN_POINT ( 'NONE',  ( 175.5246756310037028, 290.9156563365580723, 2.576511661195814540 ) ) ;
#43861 = CARTESIAN_POINT ( 'NONE',  ( 153.3920560952016956, 264.9641606960921649, 16.50453917291963535 ) ) ;
#43862 = AXIS2_PLACEMENT_3D ( 'NONE', #62973, #25993, #46774 ) ;
#43863 = CARTESIAN_POINT ( 'NONE',  ( 84.52717288222906689, 47.01816712101242501, 11.03627013421178304 ) ) ;
#43864 = CARTESIAN_POINT ( 'NONE',  ( 46.22371820283660782, 112.7232458147606451, -10.00000000000000000 ) ) ;
#43865 = CARTESIAN_POINT ( 'NONE',  ( -3.586574591843265658, 177.9244531367911577, -4.594050593750046652 ) ) ;
#43866 = CARTESIAN_POINT ( 'NONE',  ( 99.66015183740654493, 228.3458772461660544, 9.188101187500095079 ) ) ;
#43867 = CARTESIAN_POINT ( 'NONE',  ( 47.20246722098146108, 191.3927522451417929, -10.00000000000009237 ) ) ;
#43868 = CARTESIAN_POINT ( 'NONE',  ( 181.1221284655866270, 256.4354403611804969, -2.327941025046529777 ) ) ;
#43869 = CARTESIAN_POINT ( 'NONE',  ( 78.17977472700404462, 52.13989681908228135, 15.57239507869588913 ) ) ;
#43870 = CARTESIAN_POINT ( 'NONE',  ( 177.8561250001070846, 283.2065401683831283, -14.44526047890849796 ) ) ;
#43871 = CARTESIAN_POINT ( 'NONE',  ( 190.6839247239546751, 299.7689920197724973, -5.111333485343316774 ) ) ;
#43872 = CARTESIAN_POINT ( 'NONE',  ( 69.81582973455006425, 63.14295414310246457, -13.67321376818634882 ) ) ;
#43873 = CARTESIAN_POINT ( 'NONE',  ( 182.6908602801013899, 274.3648995712160286, 16.39508407896753539 ) ) ;
#43874 = CARTESIAN_POINT ( 'NONE',  ( 148.1004780136491377, 274.1294427855589788, -7.811560775291159331 ) ) ;
#43875 = PLANE ( 'NONE',  #53009 ) ;
#43876 = CARTESIAN_POINT ( 'NONE',  ( 84.39448865303761238, 50.06170295690048988, 13.83095091856771219 ) ) ;
#43877 = CARTESIAN_POINT ( 'NONE',  ( 193.2553405396020025, 265.5685525206544639, 7.793004429795182375 ) ) ;
#43878 = EDGE_CURVE ( 'NONE', #59778, #6177, #46782, .T. ) ;
#43879 = CARTESIAN_POINT ( 'NONE',  ( 184.7157775894015117, 297.3647472220100099, -4.497232409310948142 ) ) ;
#43880 = CARTESIAN_POINT ( 'NONE',  ( 183.4233717680499467, 267.7550803107557158, -15.99514032604573011 ) ) ;
#43881 = DIRECTION ( 'NONE',  ( 0.000000000000000000, -0.000000000000000000, 1.000000000000000000 ) ) ;
#43882 = EDGE_CURVE ( 'NONE', #89109, #15864, #8763, .T. ) ;
#43884 = EDGE_CURVE ( 'NONE', #42705, #6582, #46868, .T. ) ;
#43883 = CARTESIAN_POINT ( 'NONE',  ( 81.85856577761916242, 58.94112368179924033, 0.4414737964294648265 ) ) ;
#43885 = EDGE_CURVE ( 'NONE', #97093, #34316, #31649, .T. ) ;
#43886 = CARTESIAN_POINT ( 'NONE',  ( 85.69549220138247847, 220.2833772461660544, -9.188101187500095079 ) ) ;
#43887 = CARTESIAN_POINT ( 'NONE',  ( 9.725772901699041739, 17.56628583063838889, 9.188101187500006262 ) ) ;
#43888 = CARTESIAN_POINT ( 'NONE',  ( 191.2056514706806070, 299.4690922889112699, 7.290007621276087590 ) ) ;
#43889 = CARTESIAN_POINT ( 'NONE',  ( 158.7250054796891732, 259.1391378321184220, -17.13534898805800211 ) ) ;
#43891 = CARTESIAN_POINT ( 'NONE',  ( 152.4944416537803988, 266.5188745142414746, 15.96416334701886086 ) ) ;
#43890 = CARTESIAN_POINT ( 'NONE',  ( 195.8627871995700502, 291.4026965887302936, 17.41145040657729481 ) ) ;
#43892 = CARTESIAN_POINT ( 'NONE',  ( 199.1216527653377000, 285.7581758537840528, -18.37739894744384728 ) ) ;
#43893 = CARTESIAN_POINT ( 'NONE',  ( 173.2161758961336488, 268.0191514601266931, -16.29353906404126562 ) ) ;
#43894 = CARTESIAN_POINT ( 'NONE',  ( 40.31210609084968866, 28.98920272979929535, 7.433330006724137462 ) ) ;
#43895 = CARTESIAN_POINT ( 'NONE',  ( 147.4271219180435253, 275.2957297547342819, -3.800519706258907782 ) ) ;
#43896 = CARTESIAN_POINT ( 'NONE',  ( 86.47331868612941719, 47.35852300529328573, 10.29769560459374667 ) ) ;
#43897 = ORIENTED_EDGE ( 'NONE', *, *, #83804, .T. ) ;
#43898 = CARTESIAN_POINT ( 'NONE',  ( 26.73894555032740783, 17.29860640527292759, -2.839279412974138328 ) ) ;
#43899 = CARTESIAN_POINT ( 'NONE',  ( 49.07419501245632176, 91.40403951869188859, -10.00000000000000000 ) ) ;
#43900 = LINE ( 'NONE', #67206, #73305 ) ;
#43901 = CARTESIAN_POINT ( 'NONE',  ( 188.0102668379925035, 285.9726363770864168, -16.35593525032086148 ) ) ;
#43902 = ORIENTED_EDGE ( 'NONE', *, *, #4660, .F. ) ;
#43903 = CARTESIAN_POINT ( 'NONE',  ( 70.35832557788559427, 61.08735884527625615, 14.88019646618581149 ) ) ;
#43904 = CARTESIAN_POINT ( 'NONE',  ( 160.0105735053945182, 253.5005522708592594, 16.10371386499367929 ) ) ;
#43905 = CARTESIAN_POINT ( 'NONE',  ( 157.3351601172205676, 268.6802943510268733, 15.65239677815443287 ) ) ;
#43906 = CARTESIAN_POINT ( 'NONE',  ( 72.57482212583268222, 71.55826866971187883, 5.407793347878283363 ) ) ;
#43907 = CARTESIAN_POINT ( 'NONE',  ( 87.37223321024185907, 44.84069173413745091, -6.683519980512460101 ) ) ;
#43908 = CARTESIAN_POINT ( 'NONE',  ( 146.5247557210571756, 248.7365022471902023, 10.00000000000009592 ) ) ;
#43909 = CARTESIAN_POINT ( 'NONE',  ( 69.40201478176561523, 62.74293981228880313, 13.19403646481873338 ) ) ;
#43910 = ORIENTED_EDGE ( 'NONE', *, *, #55892, .T. ) ;
#43911 = CARTESIAN_POINT ( 'NONE',  ( 17.60357497223980516, 35.28838536716091312, -10.00000000000000000 ) ) ;
#43912 = VERTEX_POINT ( 'NONE', #14960 ) ;
#43913 = CARTESIAN_POINT ( 'NONE',  ( 196.9914202414729232, 265.2248154332262970, -4.566998097189091332 ) ) ;
#43914 = CARTESIAN_POINT ( 'NONE',  ( 86.17717080636731453, 43.91654295222171811, 5.091268916963881175 ) ) ;
#43915 = ORIENTED_EDGE ( 'NONE', *, *, #98914, .T. ) ;
#43916 = CARTESIAN_POINT ( 'NONE',  ( 181.4406354472745591, 291.0628233767851043, -11.23432871412726541 ) ) ;
#43917 = EDGE_LOOP ( 'NONE', ( #71652, #51401, #73288 ) ) ;
#43918 = CARTESIAN_POINT ( 'NONE',  ( 201.9316232165379859, 267.4154334901691072, 4.302177643393134687 ) ) ;
#43919 = CARTESIAN_POINT ( 'NONE',  ( 158.9201382803563547, 255.3892414829881261, 16.13706509051041138 ) ) ;
#43920 = CARTESIAN_POINT ( 'NONE',  ( 144.1522069568320887, 254.0333772461660260, 9.188101187500095079 ) ) ;
#43921 = CARTESIAN_POINT ( 'NONE',  ( 86.54822389131679472, 42.74345947012793090, -2.172736160200603931E-06 ) ) ;
#43922 = CARTESIAN_POINT ( 'NONE',  ( 17.26055046206296950, 33.28368158147418399, 10.00000000000000000 ) ) ;
#43923 = CARTESIAN_POINT ( 'NONE',  ( 40.27059248445925732, 25.11110640527295601, -2.839279412974138328 ) ) ;
#43924 = DIRECTION ( 'NONE',  ( 0.000000000000000000, 0.000000000000000000, -1.000000000000000000 ) ) ;
#43925 = CARTESIAN_POINT ( 'NONE',  ( 164.4315604333902172, 274.7944110612714894, 14.66686579097542875 ) ) ;
#43926 = CARTESIAN_POINT ( 'NONE',  ( 171.7726240267592175, 270.5206136648362190, -17.82399101355076709 ) ) ;
#43927 = ORIENTED_EDGE ( 'NONE', *, *, #32161, .F. ) ;
#43928 = VECTOR ( 'NONE', #7398, 1000.000000000000114 ) ;
#43929 = ORIENTED_EDGE ( 'NONE', *, *, #61883, .T. ) ;
#43930 = CARTESIAN_POINT ( 'NONE',  ( 5.530962353892124206, 15.14441083166257584, 0.000000000000000000 ) ) ;
#43932 = CARTESIAN_POINT ( 'NONE',  ( 105.0000000000000000, 10.00000000000003197, -54.99999999999999289 ) ) ;
#43931 = CARTESIAN_POINT ( 'NONE',  ( 204.8189571845487080, 275.8901551335242175, 13.43702398685204358 ) ) ;
#43933 = CARTESIAN_POINT ( 'NONE',  ( 164.6359882590319899, 245.4890989114802551, -0.8957991669032092652 ) ) ;
#43934 = DIRECTION ( 'NONE',  ( 0.7694697644498922351, -0.6386832404231594928, 0.000000000000000000 ) ) ;
#43935 = CARTESIAN_POINT ( 'NONE',  ( 155.4618104034866235, 280.5061703920193281, 4.424633671028313842 ) ) ;
#43936 = CARTESIAN_POINT ( 'NONE',  ( 82.14221379916808985, 40.79694460358976471, 1.153306960283028149 ) ) ;
#43937 = CARTESIAN_POINT ( 'NONE',  ( 171.0227729602065665, 287.7541690653450814, -4.552090657951240793 ) ) ;
#43938 = CARTESIAN_POINT ( 'NONE',  ( 77.30329167060655493, 63.33344332055067127, -15.17436694516359097 ) ) ;
#43939 = CARTESIAN_POINT ( 'NONE',  ( 178.4848498230702489, 255.6885313391786951, 4.886089711317160855 ) ) ;
#43940 = CARTESIAN_POINT ( 'NONE',  ( 104.5047417616495125, 221.9548013555409511, -4.594050593750042211 ) ) ;
#43941 = ORIENTED_EDGE ( 'NONE', *, *, #84717, .F. ) ;
#43942 = CARTESIAN_POINT ( 'NONE',  ( 148.3835077007541088, 274.9253393602572260, -7.051312147027137378 ) ) ;
#43943 = CARTESIAN_POINT ( 'NONE',  ( 179.7302837102534738, 291.4774734579422102, -10.05131855248582795 ) ) ;
#43944 = EDGE_CURVE ( 'NONE', #83615, #59645, #35837, .T. ) ;
#43945 = VERTEX_POINT ( 'NONE', #69164 ) ;
#43946 = ORIENTED_EDGE ( 'NONE', *, *, #45220, .F. ) ;
#43947 = CARTESIAN_POINT ( 'NONE',  ( 183.4553195968295256, 297.0403188216897661, -2.838562726794640056 ) ) ;
#43948 = CARTESIAN_POINT ( 'NONE',  ( 71.55103965959418133, 59.07988815573101959, 15.32428709606925921 ) ) ;
#43949 = CARTESIAN_POINT ( 'NONE',  ( 195.7578697689113199, 291.5844189092309193, 17.18796537138345215 ) ) ;
#43950 = CARTESIAN_POINT ( 'NONE',  ( 159.3451320108506764, 254.6531307488737355, -16.72997986213134425 ) ) ;
#43951 = CARTESIAN_POINT ( 'NONE',  ( 197.4075646047015482, 273.1427705089788560, -14.69744958829762815 ) ) ;
#43952 = ORIENTED_EDGE ( 'NONE', *, *, #83954, .T. ) ;
#43953 =( BOUNDED_CURVE ( )  B_SPLINE_CURVE ( 2, ( #74340, #64726, #87596, #18631, #49509, #30198, #14509, #67708, #38280 ),
 .UNSPECIFIED., .F., .T. ) 
 B_SPLINE_CURVE_WITH_KNOTS ( ( 3, 2, 2, 2, 3 ),
 ( 0.08467741935483871774, 0.08602150537634409289, 0.08870967741935484319, 0.09139784946236559349, 0.09274193548387096864 ),
 .UNSPECIFIED. ) 
 CURVE ( )  GEOMETRIC_REPRESENTATION_ITEM ( )  RATIONAL_B_SPLINE_CURVE ( ( 0.9330127018922192983, 0.9330127018922196314, 1.000000000000000000, 0.8660254037844387076, 1.000000000000000000, 0.8660254037844387076, 1.000000000000000000, 0.9330127018922194093, 0.9330127018922194093 ) ) 
 REPRESENTATION_ITEM ( '' )  );
#43954 = ORIENTED_EDGE ( 'NONE', *, *, #4583, .F. ) ;
#43955 = CARTESIAN_POINT ( 'NONE',  ( 162.6257765080958677, 248.9708877980734485, -10.42859054881151160 ) ) ;
#43956 = VERTEX_POINT ( 'NONE', #100094 ) ;
#43957 = ADVANCED_FACE ( 'NONE', ( #24067 ), #68664, .T. ) ;
#43958 = CARTESIAN_POINT ( 'NONE',  ( 191.8042499109635060, 263.6573267499654207, -8.212264930826352227 ) ) ;
#43959 = CYLINDRICAL_SURFACE ( 'NONE', #42985, 17.82106496071139645 ) ;
#43960 = CARTESIAN_POINT ( 'NONE',  ( 83.55986682201206861, 47.94177803495283996, 12.26456158152270071 ) ) ;
#43962 = CARTESIAN_POINT ( 'NONE',  ( 69.59273039108451542, 62.48764762269725992, -13.40792685205324908 ) ) ;
#43961 = CARTESIAN_POINT ( 'NONE',  ( 132.6505673846437503, 238.2048013555409796, 4.594050593750051981 ) ) ;
#43963 = DIRECTION ( 'NONE',  ( 0.3077152132536229434, 0.9514785060800257099, 0.000000000000000000 ) ) ;
#43964 = ORIENTED_EDGE ( 'NONE', *, *, #6634, .F. ) ;
#43965 = CARTESIAN_POINT ( 'NONE',  ( 157.3094609834150788, 258.1790163958882545, 18.30007615310968916 ) ) ;
#43966 = CARTESIAN_POINT ( 'NONE',  ( 57.68498304950349365, 204.1115022471902591, 10.00000000000009592 ) ) ;
#43967 = CARTESIAN_POINT ( 'NONE',  ( 190.3403783070287432, 264.3467331185190119, -9.331392502024449698 ) ) ;
#43968 = CARTESIAN_POINT ( 'NONE',  ( 170.5500411757033419, 249.6187539556079855, -0.2597110160622304043 ) ) ;
#43969 = CARTESIAN_POINT ( 'NONE',  ( 123.0902549634681407, 230.3262482093458061, 3.021315404115420679E-15 ) ) ;
#43970 = CARTESIAN_POINT ( 'NONE',  ( -22.20871200244593879, 23.11170711957622004, -10.00000000000000000 ) ) ;
#43971 = DIRECTION ( 'NONE',  ( 0.5864613938488599798, -0.8099771808667527440, 0.000000000000000000 ) ) ;
#43972 = CARTESIAN_POINT ( 'NONE',  ( 138.8568224548344858, 257.6427522451418781, 10.00000000000009415 ) ) ;
#43973 = CARTESIAN_POINT ( 'NONE',  ( 161.5056331467593225, 250.9110330116698435, 14.52719814064025528 ) ) ;
#43974 = CARTESIAN_POINT ( 'NONE',  ( 68.79206230443567449, 70.05501897347022577, -2.776141514423435375 ) ) ;
#43975 = CARTESIAN_POINT ( 'NONE',  ( 56.27743144475606130, 212.4869531367911009, 4.594050593750046652 ) ) ;
#43976 = CARTESIAN_POINT ( 'NONE',  ( 206.5237403681858552, 272.9373840435757188, -10.81420335655575116 ) ) ;
#43977 = DIRECTION ( 'NONE',  ( -0.8660254037844387076, -0.4999999999999998890, -0.000000000000000000 ) ) ;
#43978 = CARTESIAN_POINT ( 'NONE',  ( 163.4178923001155681, 247.5989030008181260, -10.38047187240561442 ) ) ;
#43979 = FACE_OUTER_BOUND ( 'NONE', #34624, .T. ) ;
#43980 = DIRECTION ( 'NONE',  ( 0.8660254037844395958, 0.4999999999999985567, 0.000000000000000000 ) ) ;
#43982 = DIRECTION ( 'NONE',  ( -0.5000000000000013323, 0.8660254037844379305, 0.000000000000000000 ) ) ;
#43981 = LINE ( 'NONE', #27317, #74271 ) ;
#43983 = CARTESIAN_POINT ( 'NONE',  ( 13.83924611881801958, 13.15404122711132118, 8.090169943749479842 ) ) ;
#43984 = CARTESIAN_POINT ( 'NONE',  ( 33.16502987395432456, 42.08080186712595605, -3.090169943749475845 ) ) ;
#43985 = CARTESIAN_POINT ( 'NONE',  ( 149.8100742315740774, 272.7067330206335782, -11.46274738871846566 ) ) ;
#43986 = PLANE ( 'NONE',  #96449 ) ;
#43987 = CARTESIAN_POINT ( 'NONE',  ( 72.14066163544119092, 72.07444104301772825, 2.939506046423011831 ) ) ;
#43988 = CARTESIAN_POINT ( 'NONE',  ( 18.68642948779652002, 193.8464784336661637, 1.353441290958777327E-15 ) ) ;
#43989 = CARTESIAN_POINT ( 'NONE',  ( 207.1829395897571260, 270.7610514960755381, 3.262445449933754293 ) ) ;
#43990 = ADVANCED_FACE ( 'NONE', ( #92029 ), #83005, .F. ) ;
#43991 = CARTESIAN_POINT ( 'NONE',  ( 157.2744851780909414, 258.2395962677452985, 18.17792129701959070 ) ) ;
#43992 = CARTESIAN_POINT ( 'NONE',  ( 200.6957962653111167, 278.2105254787464901, 15.28271896800693952 ) ) ;
#43993 = CARTESIAN_POINT ( 'NONE',  ( 77.68426462998779414, 51.26866757787253448, -15.41241789615859936 ) ) ;
#43994 = DIRECTION ( 'NONE',  ( -0.000000000000000000, -0.000000000000000000, -1.000000000000000000 ) ) ;
#43995 = CARTESIAN_POINT ( 'NONE',  ( 40.25596147474394826, 203.2369531367911293, -4.594050593750048428 ) ) ;
#43996 = CARTESIAN_POINT ( 'NONE',  ( 17.33597792084844258, 30.98502408145592213, -5.678558825948271327 ) ) ;
#43997 = CARTESIAN_POINT ( 'NONE',  ( 170.8906340425221799, 287.3599720229358923, 7.052392840008895547 ) ) ;
#43998 = CARTESIAN_POINT ( 'NONE',  ( -18.11259370987442452, 171.8967562850347690, 9.296355089585912665E-16 ) ) ;
#43999 = CARTESIAN_POINT ( 'NONE',  ( 36.44916501977947831, 42.81751292744058901, -6.180339887498951690 ) ) ;
#44000 = CARTESIAN_POINT ( 'NONE',  ( 203.2757866645317222, 269.5093088776978334, -7.514607224931010521 ) ) ;
#44001 = CARTESIAN_POINT ( 'NONE',  ( 76.32091777638089525, 59.04525850092294093, -16.41165238920815383 ) ) ;
#44002 = CARTESIAN_POINT ( 'NONE',  ( 176.4077479315872665, 274.9858714345624549, 16.74632039004189465 ) ) ;
#44003 = CARTESIAN_POINT ( 'NONE',  ( 155.0568450317760494, 264.0806616740677555, 17.52241723436104337 ) ) ;
#44004 = CARTESIAN_POINT ( 'NONE',  ( 71.84119047025625093, 67.74597162956264640, -10.41150127685602911 ) ) ;
#44005 = CARTESIAN_POINT ( 'NONE',  ( 193.0433938349725338, 267.1203275631486349, 11.31873111441719182 ) ) ;
#44006 = CARTESIAN_POINT ( 'NONE',  ( 82.07091975778192250, 41.09839960039168005, 3.280828371301158342 ) ) ;
#44007 = CARTESIAN_POINT ( 'NONE',  ( 108.2753003872445134, 219.9865022471901739, 1.119607411625061291E-15 ) ) ;
#44008 = FACE_OUTER_BOUND ( 'NONE', #18541, .T. ) ;
#44009 = CARTESIAN_POINT ( 'NONE',  ( 80.51198428680065433, 43.68793065238016737, 9.861687463089015893 ) ) ;
#44010 = EDGE_LOOP ( 'NONE', ( #9110, #22758, #91929, #40311 ) ) ;
#44011 = CARTESIAN_POINT ( 'NONE',  ( 51.08127902204942927, 209.4869531367911009, 4.594050593750046652 ) ) ;
#44012 = VERTEX_POINT ( 'NONE', #59307 ) ;
#44013 = DIRECTION ( 'NONE',  ( 1.000000000000000000, 0.000000000000000000, 0.000000000000000000 ) ) ;
#44014 = DIRECTION ( 'NONE',  ( 1.000000000000000000, 0.000000000000000000, 0.000000000000000000 ) ) ;
#44015 = DIRECTION ( 'NONE',  ( 0.2633726137851623572, 0.9634420117996734811, -0.04913609882122786654 ) ) ;
#44016 = VERTEX_POINT ( 'NONE', #81680 ) ;
#44017 = CARTESIAN_POINT ( 'NONE',  ( 177.1052724318428773, 289.8048150823444757, 10.36495476014435901 ) ) ;
#44018 = CARTESIAN_POINT ( 'NONE',  ( 204.0604753336787667, 271.4817813032398703, 9.862283393711939183 ) ) ;
#44019 = B_SPLINE_CURVE_WITH_KNOTS ( 'NONE', 3,
 ( #58185, #59156, #3994, #90126, #20701, #65780 ),
 .UNSPECIFIED., .F., .F.,
 ( 4, 2, 4 ),
 ( 0.01962962394112050674, 0.02417033321900810550, 0.02871104249689570426 ),
 .UNSPECIFIED. ) ;
#44020 = FACE_OUTER_BOUND ( 'NONE', #71041, .T. ) ;
#44021 = B_SPLINE_CURVE_WITH_KNOTS ( 'NONE', 3,
 ( #91241, #49106, #41486, #70914 ),
 .UNSPECIFIED., .F., .F.,
 ( 4, 4 ),
 ( 0.02844990342440924941, 0.03762721602985887731 ),
 .UNSPECIFIED. ) ;
#44022 = CARTESIAN_POINT ( 'NONE',  ( 31.05164846989082506, 29.87878583063843507, -9.188101187500006262 ) ) ;
#44023 = CARTESIAN_POINT ( 'NONE',  ( 188.6489399924155066, 265.3460165191049214, 10.74106153545168318 ) ) ;
#44024 = CARTESIAN_POINT ( 'NONE',  ( 149.2593905435863348, 272.1221474021800759, -12.98626158366800176 ) ) ;
#44025 = CARTESIAN_POINT ( 'NONE',  ( 157.3812306876618266, 258.0547076216885785, 17.10114491953027027 ) ) ;
#44027 = ORIENTED_EDGE ( 'NONE', *, *, #31217, .T. ) ;
#44026 = VECTOR ( 'NONE', #33986, 1000.000000000000000 ) ;
#44028 = PRODUCT_RELATED_PRODUCT_CATEGORY ( 'part', '', ( #26520 ) ) ;
#44029 = CARTESIAN_POINT ( 'NONE',  ( 19.94606896448370392, 26.91421378149918908, 9.188101187500008038 ) ) ;
#44030 = CARTESIAN_POINT ( 'NONE',  ( 76.42898847865113510, 62.85965002459411011, 15.15259878098221691 ) ) ;
#44031 = CARTESIAN_POINT ( 'NONE',  ( 175.6063544791335573, 254.0105997054014040, 8.344378697908656051 ) ) ;
#44032 = LINE ( 'NONE', #3579, #56986 ) ;
#44033 = ORIENTED_EDGE ( 'NONE', *, *, #84494, .T. ) ;
#44034 = CARTESIAN_POINT ( 'NONE',  ( -22.42236680055709641, 157.8615022471902591, 0.000000000000000000 ) ) ;
#44035 = CARTESIAN_POINT ( 'NONE',  ( 166.9027035012226463, 261.4283233817405971, 16.57751465251748257 ) ) ;
#44036 = CARTESIAN_POINT ( 'NONE',  ( 159.9997000813754084, 253.5193855937126841, -16.28798248637880519 ) ) ;
#44037 = ORIENTED_EDGE ( 'NONE', *, *, #67667, .F. ) ;
#44038 = ORIENTED_EDGE ( 'NONE', *, *, #27553, .T. ) ;
#44040 = CARTESIAN_POINT ( 'NONE',  ( 28.66479899236089679, 61.08171380020798580, 59.99999999999999289 ) ) ;
#44039 = CARTESIAN_POINT ( 'NONE',  ( 159.2607205968722042, 282.5689587104361635, -3.306452599273326243 ) ) ;
#44041 = CARTESIAN_POINT ( 'NONE',  ( 70.65128213755779996, 71.32262211326366241, -4.112991392911065525 ) ) ;
#44042 = CARTESIAN_POINT ( 'NONE',  ( 65.83005313167186046, 68.93055679263270008, -2.414931814313005631 ) ) ;
#44043 = CARTESIAN_POINT ( 'NONE',  ( 159.3528137482544196, 254.6398255893999476, 16.73628156321660398 ) ) ;
#44044 = DIRECTION ( 'NONE',  ( -0.4996954135095461047, 0.8654978445076770832, -0.03489949670251103753 ) ) ;
#44045 = CARTESIAN_POINT ( 'NONE',  ( 164.5705541677141923, 265.2993310360931787, -16.66072161617881164 ) ) ;
#44046 = CARTESIAN_POINT ( 'NONE',  ( 132.9753269110629503, 238.3923013555409796, 4.594050593750050204 ) ) ;
#44047 = CARTESIAN_POINT ( 'NONE',  ( -19.65312891409030271, 93.06504152958497400, 60.00000000000000000 ) ) ;
#44048 = VERTEX_POINT ( 'NONE', #97855 ) ;
#44049 = CARTESIAN_POINT ( 'NONE',  ( 170.3043206595384902, 263.9273437261221602, 15.94611219504030508 ) ) ;
#44050 = LINE ( 'NONE', #26390, #46412 ) ;
#44051 = CARTESIAN_POINT ( 'NONE',  ( 183.6331817901053682, 289.8384269728442177, -13.45033778474055808 ) ) ;
#44052 = ADVANCED_FACE ( 'NONE', ( #20352 ), #4643, .F. ) ;
#44053 = ORIENTED_EDGE ( 'NONE', *, *, #22537, .T. ) ;
#44054 = DIRECTION ( 'NONE',  ( 0.000000000000000000, 1.000000000000000000, 0.000000000000000000 ) ) ;
#44055 = ORIENTED_EDGE ( 'NONE', *, *, #50427, .F. ) ;
#44056 = ORIENTED_EDGE ( 'NONE', *, *, #86935, .F. ) ;
#44057 = CARTESIAN_POINT ( 'NONE',  ( 198.2819808855875863, 287.2125302111982705, 18.53535247371401695 ) ) ;
#44058 = CARTESIAN_POINT ( 'NONE',  ( 75.32733312582141139, 66.71342752998261005, -13.00712609038388479 ) ) ;
#44059 = CARTESIAN_POINT ( 'NONE',  ( 75.81765026128996965, 205.3923013555409796, 4.594050593750050204 ) ) ;
#44060 = CARTESIAN_POINT ( 'NONE',  ( -22.42236680055709641, 157.8615022471902591, 0.000000000000000000 ) ) ;
#44061 = DIRECTION ( 'NONE',  ( 0.4174706225611763410, 0.9086904199442095154, 0.000000000000000000 ) ) ;
#44062 = CARTESIAN_POINT ( 'NONE',  ( 194.1011995340913074, 294.4538559273262877, 13.93949783759920713 ) ) ;
#44063 = CARTESIAN_POINT ( 'NONE',  ( 175.3207465333977950, 278.3523610338168623, 15.46700679219081209 ) ) ;
#44064 = CARTESIAN_POINT ( 'NONE',  ( 87.65336964024139377, 45.10687245489101116, 6.884500160062612117 ) ) ;
#44065 = EDGE_LOOP ( 'NONE', ( #13442, #71222, #50385, #53407 ) ) ;
#44066 = ADVANCED_FACE ( 'NONE', ( #66439 ), #34372, .T. ) ;
#44067 = CARTESIAN_POINT ( 'NONE',  ( 49.06003799288187395, 95.45573527953635562, -10.00000000000000000 ) ) ;
#44068 = CARTESIAN_POINT ( 'NONE',  ( 153.2906404175950854, 265.1398178023911782, -17.60231834963988007 ) ) ;
#44069 = CARTESIAN_POINT ( 'NONE',  ( 88.22000632671873177, 44.27423112938744509, 4.003506518527982116 ) ) ;
#44070 = EDGE_LOOP ( 'NONE', ( #84735, #60377, #41705, #71884 ) ) ;
#44071 = CARTESIAN_POINT ( 'NONE',  ( 72.58391486703608564, 69.83303746380133248, -8.484543846056432415 ) ) ;
#44072 = ADVANCED_FACE ( 'NONE', ( #21337 ), #84874, .T. ) ;
#44073 = CARTESIAN_POINT ( 'NONE',  ( 76.15417792458961799, 51.07502231937492354, -16.06867589080808401 ) ) ;
#44074 = CARTESIAN_POINT ( 'NONE',  ( 174.2670700365113134, 253.8381489143473004, -7.486906580229475416 ) ) ;
#44075 = DIRECTION ( 'NONE',  ( -0.8660254037844378194, -0.5000000000000014433, -0.000000000000000000 ) ) ;
#44076 = CARTESIAN_POINT ( 'NONE',  ( 164.3939401533646958, 245.9083385283718712, 2.844462461176849200 ) ) ;
#44077 = LINE ( 'NONE', #75016, #14443 ) ;
#44078 = CARTESIAN_POINT ( 'NONE',  ( 195.7846125890239364, 279.4931724946097233, 16.34764129634911711 ) ) ;
#44079 = CARTESIAN_POINT ( 'NONE',  ( 163.8111161534324935, 246.9178193081252743, -7.110480325054721717 ) ) ;
#44080 = CARTESIAN_POINT ( 'NONE',  ( 138.9560545341254851, 251.0333772461660260, 9.188101187500095079 ) ) ;
#44081 = EDGE_LOOP ( 'NONE', ( #40452, #60017, #14816, #34980 ) ) ;
#44082 = CARTESIAN_POINT ( 'NONE',  ( 81.21903618153429250, 44.31068850558377648, -10.11524766067121384 ) ) ;
#44083 = CARTESIAN_POINT ( 'NONE',  ( 85.08339545359741862, 43.17538514247008408, 4.622258380740561279 ) ) ;
#44084 = CARTESIAN_POINT ( 'NONE',  ( 181.7383033065034112, 289.1381347789208007, -13.52584881963807284 ) ) ;
#44085 = CARTESIAN_POINT ( 'NONE',  ( 73.05937878676877517, 70.59762130387636603, 7.796525793287967687 ) ) ;
#44086 = CARTESIAN_POINT ( 'NONE',  ( -27.42236680055714260, 166.5217562850347406, 1.224646799147364892E-15 ) ) ;
#44087 = CARTESIAN_POINT ( 'NONE',  ( 178.3148920459139788, 254.9549173854477999, 4.342301552106668794 ) ) ;
#44088 = EDGE_LOOP ( 'NONE', ( #23720, #29133, #95805, #36304 ) ) ;
#44089 = CARTESIAN_POINT ( 'NONE',  ( 77.24725012743233776, 58.87555087126124675, 16.09217688641884081 ) ) ;
#44090 = CARTESIAN_POINT ( 'NONE',  ( 182.3761579831538313, 275.1398338757759348, -16.79997168648350936 ) ) ;
#44091 = CARTESIAN_POINT ( 'NONE',  ( 164.5641499066685469, 246.8022252770303169, -5.664862832761055955 ) ) ;
#44092 = CARTESIAN_POINT ( 'NONE',  ( 81.23969665105722981, 52.59010616956271633, 15.26830288788405987 ) ) ;
#44093 = CARTESIAN_POINT ( 'NONE',  ( 186.2798660816079632, 264.0713031700501006, -12.82791401631097550 ) ) ;
#44094 = B_SPLINE_CURVE_WITH_KNOTS ( 'NONE', 3,
 ( #66110, #89946, #20523, #4303, #59480, #67098, #74737, #5316, #97058, #97534 ),
 .UNSPECIFIED., .F., .F.,
 ( 4, 2, 2, 2, 4 ),
 ( 0.000000000000000000, 0.0002622400424273354179, 0.0005244800848546708359, 0.0007867201272820061996, 0.001048960169709341672 ),
 .UNSPECIFIED. ) ;
#44095 = CARTESIAN_POINT ( 'NONE',  ( 146.8358616138309571, 276.3198226421291679, 4.054088818585255716 ) ) ;
#44096 = CARTESIAN_POINT ( 'NONE',  ( 70.61771366156216345, 71.37294255471428528, 1.331711565741383385 ) ) ;
#44097 = AXIS2_PLACEMENT_3D ( 'NONE', #25080, #95555, #1802 ) ;
#44098 = VECTOR ( 'NONE', #87483, 1000.000000000000114 ) ;
#44099 = CARTESIAN_POINT ( 'NONE',  ( -19.65312891409030271, 93.06504152958497400, 10.00000000000000888 ) ) ;
#44100 = EDGE_CURVE ( 'NONE', #34942, #33130, #64919, .T. ) ;
#44101 = ADVANCED_FACE ( 'NONE', ( #69912 ), #23311, .T. ) ;
#44102 = VECTOR ( 'NONE', #38917, 1000.000000000000000 ) ;
#44103 = B_SPLINE_SURFACE_WITH_KNOTS ( 'NONE', 3, 1, ( 
 ( #11751, #42614 ),
 ( #27448, #43105 ),
 ( #58322, #36017 ),
 ( #89297, #74048 ),
 ( #35530, #97849 ),
 ( #41625, #57327 ),
 ( #28420, #66431 ),
 ( #59298, #90279 ),
 ( #97359, #49246 ),
 ( #10749, #98346 ),
 ( #44108, #15202 ),
 ( #83161, #22319 ),
 ( #59814, #76536 ),
 ( #68912, #90780 ),
 ( #13726, #29922 ),
 ( #29426, #28937 ),
 ( #61310, #5623 ),
 ( #6122, #14230 ),
 ( #67926, #75537 ),
 ( #45117, #36517 ),
 ( #67418, #76051 ),
 ( #46098, #21331 ),
 ( #37018, #82684 ),
 ( #7617, #52215 ),
 ( #30420, #6631 ),
 ( #44603, #98849 ),
 ( #60300, #91259 ),
 ( #21822, #92272 ),
 ( #53222, #60794 ),
 ( #20851, #22820 ),
 ( #13251, #52708 ),
 ( #83667, #84173 ),
 ( #37508, #53701 ),
 ( #99836, #68415 ) ),
 .UNSPECIFIED., .T., .F., .F.,
 ( 4, 2, 2, 2, 2, 2, 2, 2, 2, 2, 2, 2, 2, 2, 2, 2, 4 ),
 ( 2, 2 ),
 ( 0.000000000000000000, 0.06250000000000000000, 0.1250000000000000000, 0.1875000000000000000, 0.2500000000000000000, 0.3125000000000000000, 0.3750000000000000000, 0.4375000000000000000, 0.5000000000000000000, 0.5625000000000000000, 0.6250000000000000000, 0.6875000000000000000, 0.7500000000000000000, 0.8125000000000000000, 0.8750000000000000000, 0.9375000000000000000, 1.000000000000000000 ),
 ( 0.000000000000000000, 1.000000000000000000 ),
 .UNSPECIFIED. ) ;
#44104 = CARTESIAN_POINT ( 'NONE',  ( 25.63248128490755562, 16.92755873383626763, 6.180339887498953466 ) ) ;
#44105 = CARTESIAN_POINT ( 'NONE',  ( 148.9230895364621574, 272.7046378331555161, 12.20434325797056019 ) ) ;
#44106 = CARTESIAN_POINT ( 'NONE',  ( 73.03889176721716581, 219.6427522451419065, -10.00000000000009592 ) ) ;
#44107 = LINE ( 'NONE', #45116, #6443 ) ;
#44108 = CARTESIAN_POINT ( 'NONE',  ( 197.8977219949227049, 287.8780861330898801, 17.48564646125164046 ) ) ;
#44109 = CARTESIAN_POINT ( 'NONE',  ( 161.4317887380794900, 251.0389352793577871, 14.14184562255241318 ) ) ;
#44110 = EDGE_CURVE ( 'NONE', #68650, #79972, #32244, .T. ) ;
#44111 = CARTESIAN_POINT ( 'NONE',  ( 143.3312870410541677, 246.8927522451417929, -10.00000000000009059 ) ) ;
#44112 = CARTESIAN_POINT ( 'NONE',  ( 175.5934154519829633, 286.1723408421822228, -11.93597657450535188 ) ) ;
#44113 = EDGE_LOOP ( 'NONE', ( #67999, #77687 ) ) ;
#44114 = ADVANCED_FACE ( 'NONE', ( #32428 ), #49731, .T. ) ;
#44116 = CARTESIAN_POINT ( 'NONE',  ( 66.72164201642236492, 67.46051856063240848, -6.617423282627738601 ) ) ;
#44115 = AXIS2_PLACEMENT_3D ( 'NONE', #20323, #96355, #33523 ) ;
#44117 = CARTESIAN_POINT ( 'NONE',  ( 150.8168331730346949, 269.4245776381016526, -15.71017957295074652 ) ) ;
#44118 = CARTESIAN_POINT ( 'NONE',  ( 7.942909239684589728, 166.2048013555410080, 4.594050593750051981 ) ) ;
#44119 = CARTESIAN_POINT ( 'NONE',  ( 178.7548933528066470, 273.8195275360004075, -17.51453903275912793 ) ) ;
#44120 = CARTESIAN_POINT ( 'NONE',  ( 29.16343140518078414, 25.03677371833803278, 10.00000000000000533 ) ) ;
#44121 = CARTESIAN_POINT ( 'NONE',  ( 71.96639307748559133, 71.49757472301890004, -5.734781593071435424 ) ) ;
#44122 = CARTESIAN_POINT ( 'NONE',  ( 157.6036818288543486, 257.6694109429415107, -16.73826488331764395 ) ) ;
#44123 = CARTESIAN_POINT ( 'NONE',  ( 20.94669640352213236, 37.57748520232516398, -10.00000000000000000 ) ) ;
#44124 = DIRECTION ( 'NONE',  ( 0.4999999999999998890, -0.8660254037844385966, 0.000000000000000000 ) ) ;
#44125 = ADVANCED_FACE ( 'NONE', ( #96764 ), #3059, .T. ) ;
#44126 = B_SPLINE_SURFACE_WITH_KNOTS ( 'NONE', 3, 1, ( 
 ( #63890, #25913 ),
 ( #79639, #55269 ),
 ( #17287, #86249 ),
 ( #69978, #71013 ),
 ( #16787, #94332 ),
 ( #9195, #592 ),
 ( #79138, #9719 ),
 ( #40070, #24885 ),
 ( #86753, #48191 ),
 ( #17806, #93326 ),
 ( #71515, #2105 ),
 ( #94826, #41069 ),
 ( #2611, #31477 ),
 ( #64395, #33499 ),
 ( #56785, #62368 ),
 ( #58766, #50189 ),
 ( #97317, #35974 ),
 ( #27884, #34016 ),
 ( #42085, #51696 ),
 ( #35484, #42569 ),
 ( #73017, #34977 ),
 ( #57280, #96330 ),
 ( #43580, #66876 ),
 ( #10703, #41581 ),
 ( #82139, #12200 ),
 ( #74004, #3609 ),
 ( #43061, #18803 ),
 ( #88256, #64901 ),
 ( #5093, #11708 ),
 ( #59255, #49686 ),
 ( #80641, #12709 ),
 ( #3131, #4590 ),
 ( #66388, #51174 ),
 ( #89736, #97809 ) ),
 .UNSPECIFIED., .T., .F., .F.,
 ( 4, 2, 2, 2, 2, 2, 2, 2, 2, 2, 2, 2, 2, 2, 2, 2, 4 ),
 ( 2, 2 ),
 ( 0.000000000000000000, 0.06250000000000000000, 0.1250000000000000000, 0.1875000000000000000, 0.2500000000000000000, 0.3125000000000000000, 0.3750000000000000000, 0.4375000000000000000, 0.5000000000000000000, 0.5625000000000000000, 0.6250000000000000000, 0.6875000000000000000, 0.7500000000000000000, 0.8125000000000000000, 0.8750000000000000000, 0.9375000000000000000, 1.000000000000000000 ),
 ( 0.000000000000000000, 1.000000000000000000 ),
 .UNSPECIFIED. ) ;
#44128 = CARTESIAN_POINT ( 'NONE',  ( 73.18322933451463541, 206.3927522451418213, -10.00000000000009059 ) ) ;
#44127 = CARTESIAN_POINT ( 'NONE',  ( 18.55146011244625370, 181.5177522451418497, -10.00000000000009592 ) ) ;
#44129 = ADVANCED_FACE ( 'NONE', ( #67816 ), #92165, .F. ) ;
#44130 = CARTESIAN_POINT ( 'NONE',  ( 75.11332179147987631, 67.11795023670394755, 12.64955091210966742 ) ) ;
#44131 = CARTESIAN_POINT ( 'NONE',  ( 198.5328126748496516, 286.7780768080430676, 18.48542741931266775 ) ) ;
#44132 = B_SPLINE_CURVE_WITH_KNOTS ( 'NONE', 3,
 ( #10795, #25999, #69699, #18395, #22611, #38290, #76804, #55850, #33591, #40666, #307, #80227, #84940, #61091, #69200, #53497, #30209, #56373, #87371, #63977, #100126, #86845, #9806, #72100, #56870, #92062, #84451, #61594, #49289, #92545, #17900 ),
 .UNSPECIFIED., .F., .F.,
 ( 4, 3, 3, 3, 3, 3, 3, 3, 3, 3, 4 ),
 ( 0.000000000000000000, 0.1333490885032359574, 0.3007194338854340954, 0.4699862290245186980, 0.5844252810809413834, 0.6686540514502794519, 0.7354980260655689106, 0.8028463152565833427, 0.8633854507757432462, 0.9437142632667659958, 1.000000000000000000 ),
 .UNSPECIFIED. ) ;
#44133 = CARTESIAN_POINT ( 'NONE',  ( 55.08690683815012790, 212.6115022471903444, -5.000000000000047962 ) ) ;
#44134 = CARTESIAN_POINT ( 'NONE',  ( 181.9135216713392538, 291.6657426544036298, 9.319931514330358269 ) ) ;
#44135 = CARTESIAN_POINT ( 'NONE',  ( 189.8533352240220893, 301.8113727360248504, -0.2033756396389863053 ) ) ;
#44136 = CARTESIAN_POINT ( 'NONE',  ( 16.52171307410043255, 180.3458772461660544, 9.188101187500095079 ) ) ;
#44137 = CARTESIAN_POINT ( 'NONE',  ( 168.2555426073723481, 286.2821508661389771, 4.155022024279104720 ) ) ;
#44138 = CARTESIAN_POINT ( 'NONE',  ( 192.3401793061076717, 297.5040324353506094, 12.56432540404525611 ) ) ;
#44139 = CARTESIAN_POINT ( 'NONE',  ( 43.68478726420265446, 28.14754757982094802, -5.678558825948276656 ) ) ;
#44140 = DIRECTION ( 'NONE',  ( 1.000000000000000000, 0.000000000000000000, 0.000000000000000000 ) ) ;
#44141 = CARTESIAN_POINT ( 'NONE',  ( 207.6209998424140792, 271.0368748851258260, 6.610167240481342965 ) ) ;
#44142 = LINE ( 'NONE', #38538, #81542 ) ;
#44143 = CARTESIAN_POINT ( 'NONE',  ( 123.1420698188773315, 235.2365022471902023, 10.00000000000009948 ) ) ;
#44144 = CARTESIAN_POINT ( 'NONE',  ( 160.6358730764160612, 280.0761735822365495, 9.121476281160894928 ) ) ;
#44145 = APPLICATION_PROTOCOL_DEFINITION ( 'draft international standard', 'automotive_design', 1998, #13922 ) ;
#44146 = CARTESIAN_POINT ( 'NONE',  ( 21.21803360120161486, 14.11110640527291871, -2.839279412974138328 ) ) ;
#44147 = CARTESIAN_POINT ( 'NONE',  ( 121.1754704609022468, 240.7677522451418497, 10.00000000000009592 ) ) ;
#44148 = CARTESIAN_POINT ( 'NONE',  ( 82.53276180672601470, 53.86864964727561755, 15.84768121842077271 ) ) ;
#44149 = CARTESIAN_POINT ( 'NONE',  ( 159.4515169353164197, 258.9283067265839122, 16.83560305343668517 ) ) ;
#44150 = CARTESIAN_POINT ( 'NONE',  ( 155.6126298223767890, 261.1180141786725244, 18.15400560664037855 ) ) ;
#44151 = ORIENTED_EDGE ( 'NONE', *, *, #80813, .T. ) ;
#44152 = CARTESIAN_POINT ( 'NONE',  ( 181.8673996824255710, 289.2482696471543022, 12.44316705411579882 ) ) ;
#44153 = CARTESIAN_POINT ( 'NONE',  ( 84.30322693489105745, 45.55207041838918514, -10.27315936618584047 ) ) ;
#44154 = CARTESIAN_POINT ( 'NONE',  ( 81.37151302304147293, 42.01189121629286660, 7.817116131920905708 ) ) ;
#44155 = LINE ( 'NONE', #95935, #51266 ) ;
#44156 = ORIENTED_EDGE ( 'NONE', *, *, #76416, .T. ) ;
#44157 = CARTESIAN_POINT ( 'NONE',  ( 196.4830298217786435, 289.2019227521179232, -16.84636831274811897 ) ) ;
#44158 = CARTESIAN_POINT ( 'NONE',  ( 67.97811056134003138, 69.84350333162846880, 0.3721567129542452390 ) ) ;
#44159 = B_SPLINE_CURVE_WITH_KNOTS ( 'NONE', 3,
 ( #9396, #32687, #63588, #63087 ),
 .UNSPECIFIED., .F., .F.,
 ( 4, 4 ),
 ( 0.000000000000000000, 0.005356180736718595299 ),
 .UNSPECIFIED. ) ;
#44160 = CARTESIAN_POINT ( 'NONE',  ( 81.38228331512368641, 42.18052851754683275, 8.075145019496558163 ) ) ;
#44161 = CARTESIAN_POINT ( 'NONE',  ( 202.8874463667715133, 279.2356300052831557, -15.29930322226033468 ) ) ;
#44162 = ORIENTED_EDGE ( 'NONE', *, *, #94508, .F. ) ;
#44163 = ORIENTED_EDGE ( 'NONE', *, *, #83384, .T. ) ;
#44165 = CARTESIAN_POINT ( 'NONE',  ( 204.9780665305064531, 275.6145696623662502, 14.10615427165218883 ) ) ;
#44164 = CARTESIAN_POINT ( 'NONE',  ( 159.2788173922416775, 279.4644734097240644, -9.612199085998382131 ) ) ;
#44166 = CARTESIAN_POINT ( 'NONE',  ( 192.4202172926039793, 297.3654025762033370, 10.98569444949570872 ) ) ;
#44167 = ORIENTED_EDGE ( 'NONE', *, *, #93249, .F. ) ;
#44168 = CARTESIAN_POINT ( 'NONE',  ( 151.3589047706063582, 268.4856820897672378, 14.56544807350869419 ) ) ;
#44169 = CARTESIAN_POINT ( 'NONE',  ( 80.17693862949111860, 57.41387879531588112, -16.59169664258510224 ) ) ;
#44170 = CARTESIAN_POINT ( 'NONE',  ( 76.92873890057782660, 49.89429371730488327, 15.13083596839045519 ) ) ;
#44171 = VERTEX_POINT ( 'NONE', #22715 ) ;
#44172 = CARTESIAN_POINT ( 'NONE',  ( 87.70375725421425273, 45.31067632575319237, -6.371254654310869014 ) ) ;
#44173 = CARTESIAN_POINT ( 'NONE',  ( 80.87722779131914308, 43.49871416137424518, 9.386169728457165462 ) ) ;
#44174 = EDGE_CURVE ( 'NONE', #56928, #72976, #83552, .T. ) ;
#44175 = VERTEX_POINT ( 'NONE', #68301 ) ;
#44176 = CARTESIAN_POINT ( 'NONE',  ( 164.6241018286200699, 245.5096868128744632, 3.031483545445131433 ) ) ;
#44177 = CARTESIAN_POINT ( 'NONE',  ( 158.2296914707421820, 265.1721668954002666, 17.20786077318715712 ) ) ;
#44178 = EDGE_LOOP ( 'NONE', ( #59980, #70982 ) ) ;
#44179 = CARTESIAN_POINT ( 'NONE',  ( 174.5677109544117229, 276.8219974751209520, -15.95664790871851757 ) ) ;
#44180 = CARTESIAN_POINT ( 'NONE',  ( -22.42236680055709641, 157.8615022471902591, 0.000000000000000000 ) ) ;
#44181 = CIRCLE ( 'NONE', #79821, 16.82106496071157764 ) ;
#44182 = EDGE_CURVE ( 'NONE', #10482, #67335, #26157, .T. ) ;
#44183 = ORIENTED_EDGE ( 'NONE', *, *, #25022, .T. ) ;
#44184 = CARTESIAN_POINT ( 'NONE',  ( 38.41907791167486153, 30.38052372038644577, 10.00000000000000533 ) ) ;
#44185 = CARTESIAN_POINT ( 'NONE',  ( 146.9700173529739970, 276.0874580858064746, -5.099093031535578469 ) ) ;
#44186 = ORIENTED_EDGE ( 'NONE', *, *, #100057, .T. ) ;
#44187 = ORIENTED_EDGE ( 'NONE', *, *, #98839, .F. ) ;
#44188 = CARTESIAN_POINT ( 'NONE',  ( 75.15191903148871688, 52.97183600646508239, -16.48001256418180915 ) ) ;
#44189 = CARTESIAN_POINT ( 'NONE',  ( 147.5813496936708020, 275.0285994114094592, 4.516581957185684004 ) ) ;
#44190 = CARTESIAN_POINT ( 'NONE',  ( 82.70618072881376293, 53.83593579450209177, 15.81121719814037796 ) ) ;
#44191 = CARTESIAN_POINT ( 'NONE',  ( 17.82296297622643166, 15.45404122711132544, -8.090169943749478065 ) ) ;
#44192 = CARTESIAN_POINT ( 'NONE',  ( 157.0719585813440062, 259.1361147967522243, -16.97184851174986164 ) ) ;
#44193 = EDGE_CURVE ( 'NONE', #39676, #72634, #5517, .T. ) ;
#44194 = CARTESIAN_POINT ( 'NONE',  ( 191.7916824445696591, 298.4540568673266421, 9.471960810989466850 ) ) ;
#44195 = CARTESIAN_POINT ( 'NONE',  ( 146.7373254022577100, 276.4904923669593586, -0.7242168585908188572 ) ) ;
#44196 = VECTOR ( 'NONE', #26723, 1000.000000000000227 ) ;
#44197 = EDGE_LOOP ( 'NONE', ( #36242, #304, #83377, #37326 ) ) ;
#44198 = CARTESIAN_POINT ( 'NONE',  ( 76.62092529291432186, 57.15656925429084367, -16.16476570274940983 ) ) ;
#44199 = DIRECTION ( 'NONE',  ( 0.000000000000000000, 0.000000000000000000, 1.000000000000000000 ) ) ;
#44201 = CARTESIAN_POINT ( 'NONE',  ( 206.0627831668701901, 273.7357853363691902, 10.14454147593459687 ) ) ;
#44200 = CARTESIAN_POINT ( 'NONE',  ( 149.5390997184345281, 271.6376768999995761, -11.52989534384373016 ) ) ;
#44202 = LINE ( 'NONE', #59903, #54156 ) ;
#44203 = CARTESIAN_POINT ( 'NONE',  ( 189.3832291599495079, 300.6256203239445313, 1.753828516883770838 ) ) ;
#44204 = ORIENTED_EDGE ( 'NONE', *, *, #52570, .F. ) ;
#44205 = CARTESIAN_POINT ( 'NONE',  ( 149.6097189538088230, 271.5153607963395075, -12.93833707350289330 ) ) ;
#44206 = CARTESIAN_POINT ( 'NONE',  ( 80.33594858597078314, 52.74141113690976113, -15.46677329171331650 ) ) ;
#44207 = DIRECTION ( 'NONE',  ( 0.5000000000000003331, -0.8660254037844384856, 0.000000000000000000 ) ) ;
#44208 = EDGE_CURVE ( 'NONE', #64640, #82637, #51345, .T. ) ;
#44209 = CARTESIAN_POINT ( 'NONE',  ( 79.66724985528871628, 45.93439818594649182, 12.94489230522013301 ) ) ;
#44210 = EDGE_CURVE ( 'NONE', #9334, #83096, #28660, .T. ) ;
#44211 = CARTESIAN_POINT ( 'NONE',  ( 198.8190325544414634, 286.2823294344537999, -18.51269608589847948 ) ) ;
#44212 = DIRECTION ( 'NONE',  ( 0.000000000000000000, 0.000000000000000000, 1.000000000000000000 ) ) ;
#44213 = VERTEX_POINT ( 'NONE', #84552 ) ;
#44214 = CARTESIAN_POINT ( 'NONE',  ( 167.7412147458803133, 253.5458412874411636, -11.91840095923254417 ) ) ;
#44215 = DIRECTION ( 'NONE',  ( -0.1032265479692960342, 0.9946578707245736783, 0.000000000000000000 ) ) ;
#44216 = FACE_OUTER_BOUND ( 'NONE', #9417, .T. ) ;
#44217 = CARTESIAN_POINT ( 'NONE',  ( 32.33569778934854355, 196.1427522451419065, 10.00000000000009237 ) ) ;
#44218 = CARTESIAN_POINT ( 'NONE',  ( 118.6312605172356598, 248.4869531367911293, 4.594050593750046652 ) ) ;
#44219 = CARTESIAN_POINT ( 'NONE',  ( 151.1811967613751335, 268.7934813906678642, -15.79361349403328418 ) ) ;
#44220 = CARTESIAN_POINT ( 'NONE',  ( 41.85954357502990320, 126.4744881464662001, 10.00000000000000000 ) ) ;
#44221 = CARTESIAN_POINT ( 'NONE',  ( 84.25609682182033566, 50.63756641705167283, 13.79401547250049909 ) ) ;
#44222 = CARTESIAN_POINT ( 'NONE',  ( 37.40852414342580801, 106.7320921514703826, 59.99999999999999289 ) ) ;
#44223 = B_SPLINE_CURVE_WITH_KNOTS ( 'NONE', 3,
 ( #96278, #57723, #18255, #19273 ),
 .UNSPECIFIED., .F., .F.,
 ( 4, 4 ),
 ( 0.008754644785881138605, 0.01505839894353219049 ),
 .UNSPECIFIED. ) ;
#44224 = CARTESIAN_POINT ( 'NONE',  ( 37.65788526339063225, 201.7369531367911293, -4.594050593750048428 ) ) ;
#44225 = DIRECTION ( 'NONE',  ( -0.5000000000000014433, 0.8660254037844378194, -0.000000000000000000 ) ) ;
#44226 = VERTEX_POINT ( 'NONE', #15092 ) ;
#44227 = LINE ( 'NONE', #51855, #83539 ) ;
#44228 = DIRECTION ( 'NONE',  ( -0.8116583814955280474, -0.01378320505840839941, 0.5839697723396116702 ) ) ;
#44229 = ADVANCED_FACE ( 'NONE', ( #24211 ), #63709, .T. ) ;
#44230 = CARTESIAN_POINT ( 'NONE',  ( 48.98810889288134263, 89.24608170897542436, -10.00000000000000000 ) ) ;
#44231 = CARTESIAN_POINT ( 'NONE',  ( 76.29269770996508271, 51.10466816460979089, 16.05732426857825246 ) ) ;
#44232 = CARTESIAN_POINT ( 'NONE',  ( 81.90994132515743331, 41.13720830924725647, -5.473952179386033734 ) ) ;
#44233 = CARTESIAN_POINT ( 'NONE',  ( -63.39619785071779035, 38.08345695496143435, -10.00000000000000000 ) ) ;
#44234 =( BOUNDED_CURVE ( )  B_SPLINE_CURVE ( 2, ( #33133, #15413, #46308, #57422, #95986, #4224, #95500, #25542, #65528, #79785, #48851, #49834, #87910 ),
 .UNSPECIFIED., .F., .T. ) 
 B_SPLINE_CURVE_WITH_KNOTS ( ( 3, 2, 2, 2, 2, 2, 3 ),
 ( 0.9375000000000000000, 0.9399999999999999467, 0.9449999999999999512, 0.9499999999999999556, 0.9549999999999999600, 0.9599999999999999645, 0.9625000000000000222 ),
 .UNSPECIFIED. ) 
 CURVE ( )  GEOMETRIC_REPRESENTATION_ITEM ( )  RATIONAL_B_SPLINE_CURVE ( ( 0.9755282581475768211, 0.9755282581475768211, 1.000000000000000000, 0.9510565162951535312, 1.000000000000000000, 0.9510565162951535312, 1.000000000000000000, 0.9510565162951535312, 1.000000000000000000, 0.9510565162951535312, 1.000000000000000000, 0.9755282581475761550, 0.9755282581475767101 ) ) 
 REPRESENTATION_ITEM ( '' )  );
#44235 = CARTESIAN_POINT ( 'NONE',  ( 178.0385697874355060, 286.6247767869483596, -12.15384962285411952 ) ) ;
#44236 = CARTESIAN_POINT ( 'NONE',  ( 181.2921530440871720, 261.7463096819169550, 13.20693057592762010 ) ) ;
#44237 = ADVANCED_FACE ( 'NONE', ( #32304 ), #29593, .T. ) ;
#44238 = CARTESIAN_POINT ( 'NONE',  ( 87.40047971330908183, 231.2677522451419065, -5.000000000000047962 ) ) ;
#44239 = ORIENTED_EDGE ( 'NONE', *, *, #30144, .T. ) ;
#44240 = CARTESIAN_POINT ( 'NONE',  ( 198.5188009505039872, 267.2797725955071542, -8.327816907216345044 ) ) ;
#44241 = EDGE_CURVE ( 'NONE', #63156, #31137, #9287, .T. ) ;
#44242 = CARTESIAN_POINT ( 'NONE',  ( 155.2811537424576329, 279.9766836497481108, -2.298807824649978571 ) ) ;
#44243 = CARTESIAN_POINT ( 'NONE',  ( 79.00863916493514694, 47.82580172363768156, -14.30855080123139800 ) ) ;
#44244 = CARTESIAN_POINT ( 'NONE',  ( 10.18907585680922878, 170.5643266524159571, -9.188101187500093303 ) ) ;
#44245 = B_SPLINE_CURVE_WITH_KNOTS ( 'NONE', 3,
 ( #33577, #95919, #25466, #41655, #65462, #17884, #32573, #64472, #26479, #57355, #49766, #80722, #11295, #42155 ),
 .UNSPECIFIED., .F., .F.,
 ( 4, 2, 2, 2, 2, 2, 4 ),
 ( 0.0004313387020570975386, 0.001079531987292708202, 0.001403628629910513587, 0.001727725272528318756, 0.002051821915146123925, 0.002375918557763929528, 0.003024111842999565019 ),
 .UNSPECIFIED. ) ;
#44246 = ADVANCED_FACE ( 'NONE', ( #95156 ), #73319, .T. ) ;
#44247 = CARTESIAN_POINT ( 'NONE',  ( 5.030029564959478172, 25.83705186507751606, 3.090169943749475401 ) ) ;
#44248 = CARTESIAN_POINT ( 'NONE',  ( 195.8823446862052151, 273.2863346474129003, 15.24343364205054208 ) ) ;
#44249 = CARTESIAN_POINT ( 'NONE',  ( 71.82174548183152751, 58.68616614677867460, -15.47660959074812403 ) ) ;
#44250 = CARTESIAN_POINT ( 'NONE',  ( 66.32523131455108967, 68.13125372015736048, -4.501321185133645209 ) ) ;
#44251 = EDGE_CURVE ( 'NONE', #14427, #11056, #18547, .T. ) ;
#44252 = CARTESIAN_POINT ( 'NONE',  ( 60.22919299317007358, 196.3923013555409796, 4.594050593750050204 ) ) ;
#44253 = CARTESIAN_POINT ( 'NONE',  ( 208.1415148974628266, 270.1353163636768500, 3.453641150550738725 ) ) ;
#44254 = CARTESIAN_POINT ( 'NONE',  ( 72.48465836905157289, 57.53796734512142308, 15.80717508320729792 ) ) ;
#44255 = CARTESIAN_POINT ( 'NONE',  ( 68.70128421410518627, 67.44681517729620168, 8.549379373129788462 ) ) ;
#44256 = CARTESIAN_POINT ( 'NONE',  ( 151.3511865740561007, 278.6745403919405248, -1.693856907688049862 ) ) ;
#44257 =( BOUNDED_CURVE ( )  B_SPLINE_CURVE ( 2, ( #95922, #26483, #88334, #58351, #81214, #12277, #65962, #56360, #11300, #34565, #43138, #49769, #74080 ),
 .UNSPECIFIED., .F., .T. ) 
 B_SPLINE_CURVE_WITH_KNOTS ( ( 3, 2, 2, 2, 2, 2, 3 ),
 ( 0.4124999999999999778, 0.4149999999999999800, 0.4199999999999999845, 0.4249999999999999889, 0.4299999999999999933, 0.4349999999999999978, 0.4375000000000000000 ),
 .UNSPECIFIED. ) 
 CURVE ( )  GEOMETRIC_REPRESENTATION_ITEM ( )  RATIONAL_B_SPLINE_CURVE ( ( 0.9755282581475768211, 0.9755282581475768211, 1.000000000000000000, 0.9510565162951535312, 1.000000000000000000, 0.9510565162951535312, 1.000000000000000000, 0.9510565162951535312, 1.000000000000000000, 0.9510565162951535312, 1.000000000000000000, 0.9755282581475768211, 0.9755282581475768211 ) ) 
 REPRESENTATION_ITEM ( '' )  );
#44258 = ORIENTED_EDGE ( 'NONE', *, *, #84447, .T. ) ;
#44259 = VECTOR ( 'NONE', #83213, 1000.000000000000000 ) ;
#44260 = B_SPLINE_CURVE_WITH_KNOTS ( 'NONE', 3,
 ( #3363, #87001, #10442, #17529, #56527, #87515, #72769, #70731, #41315, #65132, #57521, #11462, #19059, #49933, #63130, #94074, #24626, #35228, #42806, #74756, #5336, #97558, #73247, #82874, #3841, #81381, #75245, #36217, #36713, #73739, #58031, #98549, #97078, #4330, #82387, #67119, #98043, #34726, #35730, #11948, #12447, #81870, #89488, #28621, #67620, #52415 ),
 .UNSPECIFIED., .F., .F.,
 ( 4, 1, 1, 1, 2, 2, 1, 1, 1, 2, 2, 1, 1, 2, 2, 1, 1, 2, 2, 1, 1, 2, 2, 1, 2, 2, 1, 2, 2, 4 ),
 ( 0.000000000000000000, 0.06249999999999474032, 0.09374999999999351907, 0.1093749999999934081, 0.1171874999999933387, 0.1249999999999932832, 0.1874999999999907296, 0.2187499999999880373, 0.2343749999999852340, 0.2421874999999834299, 0.2499999999999815703, 0.3124999999999802935, 0.3437499999999796829, 0.3593749999999787947, 0.3749999999999779066, 0.4374999999999760747, 0.4687499999999755751, 0.4843749999999764633, 0.4999999999999773515, 0.5624999999999864553, 0.5937499999999923395, 0.6093749999999942268, 0.6249999999999961142, 0.6874999999999993339, 0.7187500000000019984, 0.7500000000000025535, 0.8125000000000031086, 0.8437500000000033307, 0.8750000000000036637, 1.000000000000000000 ),
 .UNSPECIFIED. ) ;
#44261 = CARTESIAN_POINT ( 'NONE',  ( 14.74455677852512636, 165.9865022471901739, 1.119607411625061291E-15 ) ) ;
#44262 = CARTESIAN_POINT ( 'NONE',  ( 207.5408646414791178, 271.1756731246201753, 3.050859480894625886 ) ) ;
#44263 = AXIS2_PLACEMENT_3D ( 'NONE', #29703, #59078, #60580 ) ;
#44264 = CARTESIAN_POINT ( 'NONE',  ( 134.0307085979840167, 242.0643266524160140, 9.188101187500095079 ) ) ;
#44265 = CARTESIAN_POINT ( 'NONE',  ( 30.57771352727866443, 18.44966523072494979, -2.296566073217252530E-15 ) ) ;
#44266 = CARTESIAN_POINT ( 'NONE',  ( 191.2557879401978198, 261.3776189723048446, -4.694998167070893125 ) ) ;
#44267 = CARTESIAN_POINT ( 'NONE',  ( -15.31269525828471068, 104.2312461070085021, 45.19948692389422717 ) ) ;
#44268 = DIRECTION ( 'NONE',  ( 1.000000000000000000, 0.000000000000000000, 0.000000000000000000 ) ) ;
#44269 = VECTOR ( 'NONE', #89358, 1000.000000000000000 ) ;
#44271 = CARTESIAN_POINT ( 'NONE',  ( 189.2663724790391200, 289.8708104362821700, 14.44557331680590195 ) ) ;
#44270 = CARTESIAN_POINT ( 'NONE',  ( 157.5710319558766344, 257.7259621817996162, 18.28704422422941533 ) ) ;
#44272 = CARTESIAN_POINT ( 'NONE',  ( 68.53468829871430046, 64.27236547913501852, 11.76169348210352972 ) ) ;
#44273 = VERTEX_POINT ( 'NONE', #56603 ) ;
#44274 = CARTESIAN_POINT ( 'NONE',  ( 155.5494399783600272, 273.4016498944568525, 13.96529472218679224 ) ) ;
#44275 = CARTESIAN_POINT ( 'NONE',  ( 163.5327758489833059, 247.3999188572254013, 7.475710045443520357 ) ) ;
#44276 = CARTESIAN_POINT ( 'NONE',  ( 180.8098011652053003, 287.7440423659127191, 14.08944922001110633 ) ) ;
#44277 = CARTESIAN_POINT ( 'NONE',  ( 173.0248719821516090, 268.2920160064722950, -16.32364012504238460 ) ) ;
#44278 = CARTESIAN_POINT ( 'NONE',  ( 194.2215157464497111, 270.7474829811882273, -14.13497883233823416 ) ) ;
#44279 = ORIENTED_EDGE ( 'NONE', *, *, #45944, .T. ) ;
#44280 = CARTESIAN_POINT ( 'NONE',  ( 70.21329603614420023, 69.13614683806369499, 7.337258324027051692 ) ) ;
#44281 = CARTESIAN_POINT ( 'NONE',  ( 168.2714446481795960, 282.1153207652979518, -10.92340985837064338 ) ) ;
#44282 = CARTESIAN_POINT ( 'NONE',  ( 72.04176329605472517, 72.30724862116409213, 0.7207730510373432375 ) ) ;
#44283 = DIRECTION ( 'NONE',  ( -0.4554470513245730823, -0.8902628732232696906, 0.000000000000000000 ) ) ;
#44284 = CARTESIAN_POINT ( 'NONE',  ( 196.2975913249615587, 270.7692368477389664, 13.22270430323884938 ) ) ;
#44285 = CARTESIAN_POINT ( 'NONE',  ( 175.1183745746886871, 267.9007702990796247, 17.47926410801357022 ) ) ;
#44286 = FACE_OUTER_BOUND ( 'NONE', #15695, .T. ) ;
#44287 = CARTESIAN_POINT ( 'NONE',  ( 150.0209462876923396, 271.4416770187968382, -12.09856010893388678 ) ) ;
#44288 = CARTESIAN_POINT ( 'NONE',  ( 194.3931393306973234, 282.9231816806054098, 17.79127136852465441 ) ) ;
#44289 = CARTESIAN_POINT ( 'NONE',  ( 15.24017643949430401, 10.92755873383624454, 6.180339887498953466 ) ) ;
#44290 = CARTESIAN_POINT ( 'NONE',  ( 45.66470909604093720, 114.5311720768849995, 10.00000000000000000 ) ) ;
#44291 = ORIENTED_EDGE ( 'NONE', *, *, #72061, .T. ) ;
#44292 = CARTESIAN_POINT ( 'NONE',  ( 167.5680495833038322, 281.2627909971289455, 12.96205408629257150 ) ) ;
#44293 = B_SPLINE_CURVE_WITH_KNOTS ( 'NONE', 3,
 ( #25183, #93624, #55074, #78406, #56063, #1403, #87056, #17591, #94129, #24684, #97135, #59557, #50477, #96135, #35784, #65187, #4383, #49992, #43371, #20595, #80439, #73794, #35283, #66677, #74318, #20104, #80947, #5388, #11515, #13008, #72823, #36274, #66190, #67173, #19116, #50974, #27703, #98096, #97612, #42369, #27198, #21104, #81430, #58569 ),
 .UNSPECIFIED., .F., .F.,
 ( 4, 2, 2, 2, 2, 2, 2, 2, 2, 2, 2, 2, 2, 2, 2, 2, 2, 2, 2, 2, 2, 4 ),
 ( 0.002656945797708354200, 0.003073439877435233704, 0.003281686917298652639, 0.003385810437230362107, 0.003489933957162071575, 0.003698180997025623216, 0.003906428036889175726, 0.004322922116616358806, 0.005155910276070672059, 0.005988898435524985311, 0.006821886594979298564, 0.007654874754433611816, 0.007758998274365423199, 0.007811060034331282487, 0.007863121794297142642, 0.007967245314228861217, 0.008071368834160581526, 0.008487862913887627564, 0.008696109953751200022, 0.008904356993614772481, 0.009112604033478348409, 0.009320851073341920867 ),
 .UNSPECIFIED. ) ;
#44294 = CARTESIAN_POINT ( 'NONE',  ( 86.22341231051544241, 46.94107917315361078, -10.56950783746432698 ) ) ;
#44295 = CARTESIAN_POINT ( 'NONE',  ( 156.0396634953594628, 261.8849338628862711, -16.97419079234479611 ) ) ;
#44296 = VERTEX_POINT ( 'NONE', #3431 ) ;
#44297 = CARTESIAN_POINT ( 'NONE',  ( 147.0721334091522294, 275.9105878882373304, 0.7242168585908188572 ) ) ;
#44298 = CARTESIAN_POINT ( 'NONE',  ( 204.8067230205685689, 273.0357175708630848, -9.758814814642425617 ) ) ;
#44299 = CARTESIAN_POINT ( 'NONE',  ( 163.9149533033796047, 246.7379680887036670, 7.273005089308705706 ) ) ;
#44300 = CYLINDRICAL_SURFACE ( 'NONE', #78665, 10.00000000000010658 ) ;
#44301 = ORIENTED_EDGE ( 'NONE', *, *, #59037, .T. ) ;
#44302 = CARTESIAN_POINT ( 'NONE',  ( 92.19068272976576850, 224.0333772461660544, 9.188101187500095079 ) ) ;
#44303 = CARTESIAN_POINT ( 'NONE',  ( 199.0624198797852955, 283.1069319285825827, 17.22852181067409916 ) ) ;
#44304 = CARTESIAN_POINT ( 'NONE',  ( 69.13511649644314616, 71.04256955909853843, 2.869324681485878275E-06 ) ) ;
#44305 = CARTESIAN_POINT ( 'NONE',  ( 81.32775793644282203, 42.22126959800928603, -7.181039397308548011 ) ) ;
#44306 = EDGE_LOOP ( 'NONE', ( #45301, #32221, #84353, #59372 ) ) ;
#44307 = ORIENTED_EDGE ( 'NONE', *, *, #11761, .F. ) ;
#44308 = CARTESIAN_POINT ( 'NONE',  ( 88.42339661562220954, 43.82656006556687345, 0.1181016345699155146 ) ) ;
#44309 = VERTEX_POINT ( 'NONE', #89082 ) ;
#44310 = CARTESIAN_POINT ( 'NONE',  ( 71.90400658755810070, 72.53437165389429708, 1.750395423964758557 ) ) ;
#44311 = VERTEX_POINT ( 'NONE', #50490 ) ;
#44312 = CARTESIAN_POINT ( 'NONE',  ( 159.4780960521576674, 258.5615967792256811, 17.42390817850915141 ) ) ;
#44313 = CARTESIAN_POINT ( 'NONE',  ( 87.87588256303088485, 45.05834245088315981, 6.537532970176371805 ) ) ;
#44314 = ORIENTED_EDGE ( 'NONE', *, *, #20988, .F. ) ;
#44315 = CARTESIAN_POINT ( 'NONE',  ( 164.3663504224794565, 247.9561253440330972, -9.019399920391260039 ) ) ;
#44316 = CARTESIAN_POINT ( 'NONE',  ( 71.41016749218992743, 59.45273978182970609, 15.69346469599747174 ) ) ;
#44317 = CARTESIAN_POINT ( 'NONE',  ( 152.7729059155601021, 266.0365602647466972, -17.50667083025758686 ) ) ;
#44318 = FACE_OUTER_BOUND ( 'NONE', #8190, .T. ) ;
#44319 = ADVANCED_FACE ( 'NONE', ( #87589 ), #18114, .F. ) ;
#44320 = CARTESIAN_POINT ( 'NONE',  ( 82.71327011143105779, 53.60354310397067934, -15.74390733313335922 ) ) ;
#44321 = CARTESIAN_POINT ( 'NONE',  ( 195.8418359169588427, 291.4389852746969041, -17.23329826360656014 ) ) ;
#44322 = VERTEX_POINT ( 'NONE', #72838 ) ;
#44323 = DIRECTION ( 'NONE',  ( -0.9599109957006544125, -0.2803049773603353279, 0.000000000000000000 ) ) ;
#44324 = CARTESIAN_POINT ( 'NONE',  ( 11.13306418284875576, 18.37878583063839244, 9.188101187500006262 ) ) ;
#44325 = ORIENTED_EDGE ( 'NONE', *, *, #20805, .T. ) ;
#44326 = CARTESIAN_POINT ( 'NONE',  ( 166.5387429586460257, 283.1419806720085148, 8.930908821604470305 ) ) ;
#44328 = ORIENTED_EDGE ( 'NONE', *, *, #41263, .F. ) ;
#44327 = CARTESIAN_POINT ( 'NONE',  ( 17.75760349231054391, 174.3927522451418213, 10.00000000000009948 ) ) ;
#44329 = CARTESIAN_POINT ( 'NONE',  ( 202.9093905060991005, 279.1976216410395182, 16.97070083370504179 ) ) ;
#44330 = CARTESIAN_POINT ( 'NONE',  ( 185.3339162672891973, 258.7583632471134933, 2.918957613551585339 ) ) ;
#44331 = CARTESIAN_POINT ( 'NONE',  ( 151.3711344188577925, 276.7819027391564077, -5.262085087660871352 ) ) ;
#44332 = EDGE_CURVE ( 'NONE', #5374, #22952, #4437, .T. ) ;
#44333 = CYLINDRICAL_SURFACE ( 'NONE', #3661, 10.00000000000010658 ) ;
#44334 = DIRECTION ( 'NONE',  ( -0.8660254037844303809, -0.5000000000000144329, 0.000000000000000000 ) ) ;
#44335 = EDGE_CURVE ( 'NONE', #46799, #98986, #80963, .T. ) ;
#44336 = VECTOR ( 'NONE', #6985, 1000.000000000000000 ) ;
#44337 = CARTESIAN_POINT ( 'NONE',  ( 86.93970924122183419, 44.33811398603066323, 5.029826232848033207 ) ) ;
#44338 = CARTESIAN_POINT ( 'NONE',  ( 193.8212943487757514, 292.9386659295947197, 15.46346239154970625 ) ) ;
#44339 = VERTEX_POINT ( 'NONE', #6887 ) ;
#44340 = CARTESIAN_POINT ( 'NONE',  ( 181.8761527141526813, 271.4782540734216809, -15.98508151632294094 ) ) ;
#44341 = ORIENTED_EDGE ( 'NONE', *, *, #12345, .T. ) ;
#44342 = CARTESIAN_POINT ( 'NONE',  ( 160.0078452925083354, 276.7889099177259595, 13.19893458269325670 ) ) ;
#44343 = CARTESIAN_POINT ( 'NONE',  ( -4.831225789733595732, 168.0177522451418781, -10.00000000000009592 ) ) ;
#44344 = AXIS2_PLACEMENT_3D ( 'NONE', #45032, #27847, #81589 ) ;
#44345 = CARTESIAN_POINT ( 'NONE',  ( 194.7112710368652131, 268.6419340635496837, -10.81822129561431822 ) ) ;
#44346 = CARTESIAN_POINT ( 'NONE',  ( 175.0303541417597160, 281.4344200042963280, -14.16194463650028901 ) ) ;
#44347 = CARTESIAN_POINT ( 'NONE',  ( 28.46864935082047410, 149.7156766241961350, 37.50000000000000000 ) ) ;
#44348 = CARTESIAN_POINT ( 'NONE',  ( 85.38005290443321371, 44.62545188726001300, -7.421218069141172435 ) ) ;
#44349 = CARTESIAN_POINT ( 'NONE',  ( 164.6715181915554069, 274.3332101388145361, 14.81878660653080892 ) ) ;
#44351 = CARTESIAN_POINT ( 'NONE',  ( 75.99079911453461023, 65.46731794264749738, 14.35477091480207967 ) ) ;
#44350 = CARTESIAN_POINT ( 'NONE',  ( -14.92600794870451253, 168.3149278399160664, 9.188101187500093303 ) ) ;
#44352 = CARTESIAN_POINT ( 'NONE',  ( 163.9407385976260798, 248.4868885448184415, 9.894533935068681174 ) ) ;
#44353 = ORIENTED_EDGE ( 'NONE', *, *, #37903, .F. ) ;
#44354 = B_SPLINE_SURFACE_WITH_KNOTS ( 'NONE', 3, 1, ( 
 ( #81444, #95666 ),
 ( #89554, #64206 ),
 ( #80962, #4399 ),
 ( #42872, #95155 ),
 ( #11526, #19133 ),
 ( #57590, #20117 ),
 ( #26709, #88074 ),
 ( #18113, #89081 ),
 ( #34305, #49016 ),
 ( #79949, #42387 ),
 ( #79454, #34789 ),
 ( #35296, #73318 ),
 ( #73805, #10019 ),
 ( #66207, #40881 ),
 ( #88571, #97148 ),
 ( #11026, #3908 ),
 ( #71830, #41392 ),
 ( #26214, #65692 ),
 ( #2427, #96646 ),
 ( #50006, #27714 ),
 ( #27216, #56602 ),
 ( #58098, #33828 ),
 ( #80455, #33304 ),
 ( #87588, #10515 ),
 ( #72335, #19631 ),
 ( #2940, #57091 ),
 ( #18622, #49500 ),
 ( #41898, #72837 ),
 ( #3430, #65205 ),
 ( #96146, #37776 ),
 ( #76312, #21604 ),
 ( #44383, #90038 ),
 ( #61073, #59068 ),
 ( #14499, #52484 ) ),
 .UNSPECIFIED., .T., .F., .F.,
 ( 4, 2, 2, 2, 2, 2, 2, 2, 2, 2, 2, 2, 2, 2, 2, 2, 4 ),
 ( 2, 2 ),
 ( 0.000000000000000000, 0.06250000000000000000, 0.1250000000000000000, 0.1875000000000000000, 0.2500000000000000000, 0.3125000000000000000, 0.3750000000000000000, 0.4375000000000000000, 0.5000000000000000000, 0.5625000000000000000, 0.6250000000000000000, 0.6875000000000000000, 0.7500000000000000000, 0.8125000000000000000, 0.8750000000000000000, 0.9375000000000000000, 1.000000000000000000 ),
 ( 0.000000000000000000, 1.000000000000000000 ),
 .UNSPECIFIED. ) ;
#44355 = ORIENTED_EDGE ( 'NONE', *, *, #50440, .F. ) ;
#44356 = DIRECTION ( 'NONE',  ( 0.8660254037844395958, 0.4999999999999985567, 0.000000000000000000 ) ) ;
#44357 = PLANE ( 'NONE',  #7585 ) ;
#44358 = CARTESIAN_POINT ( 'NONE',  ( 69.56932906937804262, 66.26470779536496991, -10.53527169505675509 ) ) ;
#44359 = CARTESIAN_POINT ( 'NONE',  ( 175.6186723166894126, 290.9646728346197619, 2.631908926450905017 ) ) ;
#44360 = CARTESIAN_POINT ( 'NONE',  ( 85.24872127118341325, 42.51433283568908195, 1.035734531770441169 ) ) ;
#44361 = CARTESIAN_POINT ( 'NONE',  ( 202.7395715537438150, 279.4917566946068064, -16.55506732176026219 ) ) ;
#44362 = CARTESIAN_POINT ( 'NONE',  ( 84.25611980550206681, 46.28114692587162438, 10.44557183192605265 ) ) ;
#44363 = CARTESIAN_POINT ( 'NONE',  ( 153.1852539850606547, 279.2954070424707993, 3.897478566824396307 ) ) ;
#44364 = EDGE_CURVE ( 'NONE', #24743, #59656, #12892, .T. ) ;
#44365 = CARTESIAN_POINT ( 'NONE',  ( 24.64070123457955219, 185.0333772461660544, 9.188101187500095079 ) ) ;
#44366 = CARTESIAN_POINT ( 'NONE',  ( 120.7155680147981940, 234.3768266524159856, 9.188101187500098632 ) ) ;
#44367 = CARTESIAN_POINT ( 'NONE',  ( 45.14796862286864609, 185.3262482093457209, 3.021315404115420679E-15 ) ) ;
#44368 = DIRECTION ( 'NONE',  ( -0.9922852870422786964, 0.1239754375649568807, 0.000000000000000000 ) ) ;
#44369 = CARTESIAN_POINT ( 'NONE',  ( 79.28644739073136805, 58.22391059449252282, 16.22396175955610786 ) ) ;
#44370 = EDGE_CURVE ( 'NONE', #53564, #38420, #75671, .T. ) ;
#44371 = CARTESIAN_POINT ( 'NONE',  ( 177.1851337456532178, 282.7301262368820858, -14.31388644062017690 ) ) ;
#44372 = CARTESIAN_POINT ( 'NONE',  ( 154.9344967692067598, 262.2925750810547356, 17.30210568643136781 ) ) ;
#44373 = CARTESIAN_POINT ( 'NONE',  ( 207.2707369601997982, 271.6435479931266173, -5.381413637561199614 ) ) ;
#44374 = CARTESIAN_POINT ( 'NONE',  ( 148.0637215040603394, 274.1931069276759558, -7.795633835291665648 ) ) ;
#44375 = EDGE_CURVE ( 'NONE', #93452, #35100, #12035, .T. ) ;
#44376 = CARTESIAN_POINT ( 'NONE',  ( 85.03805233423882726, 49.96613157754471501, 13.55353664355913956 ) ) ;
#44377 = CARTESIAN_POINT ( 'NONE',  ( 188.2332182273270291, 299.2236753513818712, -0.5858898820902108673 ) ) ;
#44378 = CARTESIAN_POINT ( 'NONE',  ( -89.11465314115665137, 93.37593066204027537, 37.50000000000002132 ) ) ;
#44379 = CARTESIAN_POINT ( 'NONE',  ( 165.4117122400764401, 253.5151701492806069, -13.08392429282121050 ) ) ;
#44380 = CARTESIAN_POINT ( 'NONE',  ( -19.65312891409030271, 93.06504152958497400, 45.00000000000000711 ) ) ;
#44381 = CARTESIAN_POINT ( 'NONE',  ( 175.4548110154385938, 265.3612680696711550, -15.70463155788832310 ) ) ;
#44382 = CARTESIAN_POINT ( 'NONE',  ( 91.91987624320061911, 230.0024278399160949, 9.188101187500095079 ) ) ;
#44383 = CARTESIAN_POINT ( 'NONE',  ( 207.8232941427535536, 270.6864908788566026, -6.505149060073906142 ) ) ;
#44384 = LINE ( 'NONE', #91528, #20708 ) ;
#44386 = CARTESIAN_POINT ( 'NONE',  ( 84.27014134724090866, 42.34832866126101436, -3.331555649036015865 ) ) ;
#44385 = CARTESIAN_POINT ( 'NONE',  ( 196.4982648257524147, 290.3020170531091821, 16.69353242256149628 ) ) ;
#44387 = CARTESIAN_POINT ( 'NONE',  ( 192.3589614934448946, 289.7923222231842715, -16.44823055510686771 ) ) ;
#44388 = CARTESIAN_POINT ( 'NONE',  ( 75.88363445057348144, 65.49265179502715739, 14.31053417012051376 ) ) ;
#44389 = CARTESIAN_POINT ( 'NONE',  ( 38.65784837781280459, 56.65029301956751340, -10.00000000000000000 ) ) ;
#44390 = CARTESIAN_POINT ( 'NONE',  ( 36.73494696561986217, 42.18502408145594984, 5.678558825948276656 ) ) ;
#44391 = CARTESIAN_POINT ( 'NONE',  ( 193.1028332910263998, 296.1830769848763225, -12.04975758233223893 ) ) ;
#44392 = FACE_BOUND ( 'NONE', #13035, .T. ) ;
#44393 = ORIENTED_EDGE ( 'NONE', *, *, #32855, .T. ) ;
#44394 = CARTESIAN_POINT ( 'NONE',  ( 28.18775043786755319, 21.98920272979927759, 7.433330006724137462 ) ) ;
#44395 = DIRECTION ( 'NONE',  ( 0.1696015684586875405, 0.9855127132494806430, 0.000000000000000000 ) ) ;
#44396 = CARTESIAN_POINT ( 'NONE',  ( 197.0600256462842026, 267.5279731586389858, 9.811020786235678415 ) ) ;
#44397 = CARTESIAN_POINT ( 'NONE',  ( 187.9898463188184223, 285.9731239514064214, -16.38654393692524991 ) ) ;
#44398 = ORIENTED_EDGE ( 'NONE', *, *, #78927, .T. ) ;
#44399 = CARTESIAN_POINT ( 'NONE',  ( 37.67364948790085322, 52.89489741671174272, -10.00000000000000000 ) ) ;
#44400 = CARTESIAN_POINT ( 'NONE',  ( 75.95690509902382814, 65.20561023377018728, -14.47468716891346219 ) ) ;
#44401 = VECTOR ( 'NONE', #85777, 1000.000000000000114 ) ;
#44403 = ADVANCED_FACE ( 'NONE', ( #20613 ), #21499, .F. ) ;
#44402 = CARTESIAN_POINT ( 'NONE',  ( 73.27399602445112237, 57.75849500631026245, 16.33089542203346767 ) ) ;
#44404 = CARTESIAN_POINT ( 'NONE',  ( 173.1900044977692232, 253.8258194800205274, -9.054949657387052042 ) ) ;
#44405 = CARTESIAN_POINT ( 'NONE',  ( 75.09903334936105068, 52.93404696900269357, -16.00280056458343836 ) ) ;
#44406 = CARTESIAN_POINT ( 'NONE',  ( 144.7205361298395871, 254.3615022471902307, -10.00000000000009592 ) ) ;
#44407 = CARTESIAN_POINT ( 'NONE',  ( 157.4893260420801653, 257.8674809757739013, -18.30842125257398223 ) ) ;
#44408 = VERTEX_POINT ( 'NONE', #8885 ) ;
#44409 = CARTESIAN_POINT ( 'NONE',  ( 95.64807497750081211, 214.4824982072973683, 3.021315404115420679E-15 ) ) ;
#44410 = B_SPLINE_SURFACE_WITH_KNOTS ( 'NONE', 3, 1, ( 
 ( #87236, #63356 ),
 ( #79096, #33459 ),
 ( #56751, #63852 ),
 ( #94295, #47640 ),
 ( #70451, #40541 ),
 ( #62844, #24849 ),
 ( #48153, #56243 ),
 ( #93799, #79604 ),
 ( #17248, #25350 ),
 ( #70974, #17770 ),
 ( #95812, #41034 ),
 ( #64355, #9680 ),
 ( #71475, #1576 ),
 ( #55724, #24360 ),
 ( #55231, #86214 ),
 ( #86712, #16752 ),
 ( #32459, #78574 ),
 ( #87733, #18271 ),
 ( #9158, #94791 ),
 ( #2575, #71971 ),
 ( #49165, #2068 ),
 ( #32948, #80101 ),
 ( #48671, #10667 ),
 ( #72488, #3090 ),
 ( #33981, #64865 ),
 ( #26366, #85718 ),
 ( #28339, #12672 ),
 ( #82604, #13170 ),
 ( #34454, #80603 ),
 ( #96801, #5059 ),
 ( #96291, #73962 ),
 ( #3573, #67340 ),
 ( #89222, #44024 ),
 ( #19285, #59217 ) ),
 .UNSPECIFIED., .T., .F., .F.,
 ( 4, 2, 2, 2, 2, 2, 2, 2, 2, 2, 2, 2, 2, 2, 2, 2, 4 ),
 ( 2, 2 ),
 ( 0.000000000000000000, 0.06250000000000000000, 0.1250000000000000000, 0.1875000000000000000, 0.2500000000000000000, 0.3125000000000000000, 0.3750000000000000000, 0.4375000000000000000, 0.5000000000000000000, 0.5625000000000000000, 0.6250000000000000000, 0.6875000000000000000, 0.7500000000000000000, 0.8125000000000000000, 0.8750000000000000000, 0.9375000000000000000, 1.000000000000000000 ),
 ( 0.000000000000000000, 1.000000000000000000 ),
 .UNSPECIFIED. ) ;
#44411 = ORIENTED_EDGE ( 'NONE', *, *, #31583, .F. ) ;
#44412 = CARTESIAN_POINT ( 'NONE',  ( 202.8499463704053198, 279.3005819042728604, 17.04674939340617001 ) ) ;
#44413 = CARTESIAN_POINT ( 'NONE',  ( 66.10228174255657052, 68.64626758096548542, 4.271897712742703135 ) ) ;
#44414 = EDGE_CURVE ( 'NONE', #18565, #10368, #62279, .T. ) ;
#44415 = ORIENTED_EDGE ( 'NONE', *, *, #65194, .F. ) ;
#44416 = CARTESIAN_POINT ( 'NONE',  ( 87.07963357598215737, 43.74386682785180369, 2.609826112548035759 ) ) ;
#44418 = ORIENTED_EDGE ( 'NONE', *, *, #47040, .F. ) ;
#44417 = VECTOR ( 'NONE', #55390, 1000.000000000000114 ) ;
#44419 = DIRECTION ( 'NONE',  ( 0.4999999999999998890, -0.8660254037844385966, 0.000000000000000000 ) ) ;
#44420 = CARTESIAN_POINT ( 'NONE',  ( 205.5942821894498422, 274.5472528326565680, 11.03599490385640003 ) ) ;
#44421 = CARTESIAN_POINT ( 'NONE',  ( 190.5112993737188560, 278.7663833916702174, -16.51125563584619726 ) ) ;
#44422 = B_SPLINE_CURVE_WITH_KNOTS ( 'NONE', 3,
 ( #54396, #93967, #24520, #31111, #78739, #84863, #99543, #16917, #78240, #30632, #8821, #93466, #23504, #85372, #23010, #39197 ),
 .UNSPECIFIED., .F., .F.,
 ( 4, 2, 2, 2, 2, 2, 2, 4 ),
 ( 0.002922212478766483476, 0.003107388242815427911, 0.003199976124839900345, 0.003292564006864372780, 0.003477739770913328490, 0.003662915534962284635, 0.004403618591158125692, 0.005885024703549807806 ),
 .UNSPECIFIED. ) ;
#44423 = CARTESIAN_POINT ( 'NONE',  ( 153.6416917630915862, 264.5317790359255810, -18.09859318578890708 ) ) ;
#44424 = CARTESIAN_POINT ( 'NONE',  ( 200.8147387322574957, 282.8256649374973790, -18.02438097732020239 ) ) ;
#44425 = FACE_OUTER_BOUND ( 'NONE', #73131, .T. ) ;
#44426 = CARTESIAN_POINT ( 'NONE',  ( 38.69312636016019269, 30.84335787977765975, 9.188101187500006262 ) ) ;
#44427 = CARTESIAN_POINT ( 'NONE',  ( 77.46076174113461832, 59.13541342898363240, -16.06266701479841785 ) ) ;
#44428 = DIRECTION ( 'NONE',  ( 0.5102188382608533468, -0.8600446134263880493, 0.000000000000000000 ) ) ;
#44429 = CARTESIAN_POINT ( 'NONE',  ( 62.54379424586281289, 218.4637435831424739, 2.679491924311251605 ) ) ;
#44430 = ORIENTED_EDGE ( 'NONE', *, *, #52211, .T. ) ;
#44431 = ORIENTED_EDGE ( 'NONE', *, *, #9240, .F. ) ;
#44432 = CARTESIAN_POINT ( 'NONE',  ( 81.54798657518921345, 42.52537976816986287, 7.469856817513908176 ) ) ;
#44434 = CARTESIAN_POINT ( 'NONE',  ( 164.1635987429686736, 273.1024144199500370, -15.31708653229989814 ) ) ;
#44433 = CARTESIAN_POINT ( 'NONE',  ( 164.4272222519600746, 245.8506922426221593, 7.021336339662529902 ) ) ;
#44435 = CARTESIAN_POINT ( 'NONE',  ( 204.1633547645365638, 275.3510256380408237, 13.36249479004741580 ) ) ;
#44436 = CARTESIAN_POINT ( 'NONE',  ( 200.7780343897620980, 274.8121090555061983, -13.81066045772921314 ) ) ;
#44437 = CARTESIAN_POINT ( 'NONE',  ( 74.11595357172687670, 61.08279995983697575, -15.22303157954070940 ) ) ;
#44438 = DIRECTION ( 'NONE',  ( 1.000000000000000000, 3.568574007723717001E-15, 0.000000000000000000 ) ) ;
#44439 = CARTESIAN_POINT ( 'NONE',  ( 167.0623087134214302, 286.3931234802170707, -4.864607199251016922 ) ) ;
#44440 = CARTESIAN_POINT ( 'NONE',  ( 165.8284142803885857, 265.9971752285911180, 17.07883704590099327 ) ) ;
#44441 = CARTESIAN_POINT ( 'NONE',  ( 178.1291671650300543, 255.4875147564563065, 4.904221248299380775 ) ) ;
#44442 = CARTESIAN_POINT ( 'NONE',  ( 113.9495709998497688, 236.5958772461660544, -9.188101187500095079 ) ) ;
#44443 = CARTESIAN_POINT ( 'NONE',  ( 148.0510481135471252, 274.9194765995500802, -5.872114088031683110 ) ) ;
#44444 = CARTESIAN_POINT ( 'NONE',  ( 188.3599285997746051, 273.5439987038621439, 15.65562976607134260 ) ) ;
#44445 = ORIENTED_EDGE ( 'NONE', *, *, #32593, .T. ) ;
#44446 = B_SPLINE_CURVE_WITH_KNOTS ( 'NONE', 3,
 ( #43669, #13301, #11806, #28470 ),
 .UNSPECIFIED., .F., .F.,
 ( 4, 4 ),
 ( 0.01303476720425170501, 0.02161825251906693626 ),
 .UNSPECIFIED. ) ;
#44447 = CARTESIAN_POINT ( 'NONE',  ( 73.82480279627529285, 68.30552952313148296, -11.59219441058860589 ) ) ;
#44448 = CARTESIAN_POINT ( 'NONE',  ( 164.4286791602839912, 246.2317698387275300, -2.006671165488138175 ) ) ;
#44449 = CARTESIAN_POINT ( 'NONE',  ( 157.3988263959001870, 258.0242309610243865, 16.72376558639979294 ) ) ;
#44450 = CARTESIAN_POINT ( 'NONE',  ( 67.70744425388356547, 69.01537731644371831, 5.819509745403966150 ) ) ;
#44451 = EDGE_CURVE ( 'NONE', #92910, #47283, #1296, .T. ) ;
#44452 = B_SPLINE_CURVE_WITH_KNOTS ( 'NONE', 3,
 ( #83589, #90706, #67856, #13661, #6049, #83090, #5553, #82609, #52141, #53144, #20772, #51142, #82106, #36438, #84100, #21748, #13175, #45039, #67345, #75982, #6557, #36943, #29849, #98777, #44532, #14652, #37430, #99263, #75464, #45530, #68339, #29358, #43545, #60224, #76461, #74486, #37921, #99758, #30348, #5064, #91186, #35946, #66847, #32342, #8551, #47044 ),
 .UNSPECIFIED., .F., .F.,
 ( 4, 1, 2, 2, 1, 2, 2, 1, 1, 2, 2, 1, 1, 2, 2, 1, 1, 2, 2, 1, 1, 1, 2, 2, 1, 1, 1, 2, 2, 4 ),
 ( 0.000000000000000000, 0.06250000000000141553, 0.09375000000000073552, 0.1250000000000000555, 0.1874999999999985012, 0.2187499999999978073, 0.2499999999999971412, 0.3124999999999955036, 0.3437499999999950040, 0.3593749999999945599, 0.3749999999999940603, 0.4374999999999884537, 0.4687499999999856781, 0.4843749999999853451, 0.4999999999999849565, 0.5624999999999893419, 0.5937499999999898970, 0.6093749999999897859, 0.6249999999999896749, 0.6874999999999938938, 0.7187499999999972244, 0.7343749999999993339, 0.7421875000000008882, 0.7500000000000025535, 0.8125000000000000000, 0.8437499999999998890, 0.8593749999999997780, 0.8671875000000003331, 0.8750000000000007772, 1.000000000000000000 ),
 .UNSPECIFIED. ) ;
#44453 = CARTESIAN_POINT ( 'NONE',  ( -17.42236680055705023, 149.2012482093457777, 0.000000000000000000 ) ) ;
#44454 = ORIENTED_EDGE ( 'NONE', *, *, #12401, .T. ) ;
#44455 = EDGE_CURVE ( 'NONE', #63624, #57758, #32181, .T. ) ;
#44456 = ORIENTED_EDGE ( 'NONE', *, *, #10755, .T. ) ;
#44457 = CARTESIAN_POINT ( 'NONE',  ( -19.65312891409030271, 93.06504152958497400, -10.00000000000000888 ) ) ;
#44458 = EDGE_LOOP ( 'NONE', ( #8194, #8915, #71080, #75447 ) ) ;
#44459 = CARTESIAN_POINT ( 'NONE',  ( 44.44844410339183582, 68.22168590943847732, 10.00000000000000000 ) ) ;
#44460 = CARTESIAN_POINT ( 'NONE',  ( 158.0966096247271366, 263.1875288115938929, 17.28628307208229842 ) ) ;
#44461 = CYLINDRICAL_SURFACE ( 'NONE', #59686, 10.00000000000010658 ) ;
#44463 = CARTESIAN_POINT ( 'NONE',  ( 29.30989995549245464, 44.80713248141895377, -10.00000000000000000 ) ) ;
#44462 = CARTESIAN_POINT ( 'NONE',  ( 185.1766543017484139, 289.3992658934859037, -13.22389641140907024 ) ) ;
#44464 = DIRECTION ( 'NONE',  ( -0.7300871660154473197, -0.6833540297821711906, 0.000000000000000000 ) ) ;
#44465 = ORIENTED_EDGE ( 'NONE', *, *, #71824, .F. ) ;
#44466 = CARTESIAN_POINT ( 'NONE',  ( 190.2236813008869660, 301.1699145145108218, -5.401374690107298093 ) ) ;
#44467 = CARTESIAN_POINT ( 'NONE',  ( 71.33560860404993775, 62.23091869455711134, 14.08802979949528655 ) ) ;
#44468 = CARTESIAN_POINT ( 'NONE',  ( 82.63281508735799719, 40.94328431217294195, -3.617117793222135447 ) ) ;
#44469 = CARTESIAN_POINT ( 'NONE',  ( 170.0428130633470687, 248.7678227811192926, -0.2667965012368537780 ) ) ;
#44470 = CARTESIAN_POINT ( 'NONE',  ( 44.44844410339183582, 68.22168590943847732, -10.00000000000000000 ) ) ;
#44471 = CARTESIAN_POINT ( 'NONE',  ( 41.37327796571899796, 124.7191351846657028, -10.00000000000000000 ) ) ;
#44472 = VECTOR ( 'NONE', #8101, 1000.000000000000000 ) ;
#44473 = CARTESIAN_POINT ( 'NONE',  ( 83.88636183630472942, 44.33847814200196069, 8.266257927242135040 ) ) ;
#44474 = CYLINDRICAL_SURFACE ( 'NONE', #21951, 16.60714546451156792 ) ;
#44475 = CARTESIAN_POINT ( 'NONE',  ( 70.43138298049650814, 61.25676307520114250, -14.82522626399372889 ) ) ;
#44476 = EDGE_CURVE ( 'NONE', #24132, #69830, #78194, .T. ) ;
#44477 = CARTESIAN_POINT ( 'NONE',  ( 70.02137158282522478, 70.42997685080844406, -4.196993381856343852 ) ) ;
#44478 = CARTESIAN_POINT ( 'NONE',  ( 74.46396492422927338, 222.9869531367911293, 4.594050593750046652 ) ) ;
#44479 = CARTESIAN_POINT ( 'NONE',  ( 206.2313482792274328, 273.4438219973828268, -9.403385562213845361 ) ) ;
#44480 = DIRECTION ( 'NONE',  ( -0.8660254037844387076, -0.4999999999999998890, -0.000000000000000000 ) ) ;
#44481 = CARTESIAN_POINT ( 'NONE',  ( 162.6541320028305506, 248.9217746405196294, -10.16950121496441817 ) ) ;
#44482 = B_SPLINE_CURVE_WITH_KNOTS ( 'NONE', 3,
 ( #48984, #63170, #87040, #94114 ),
 .UNSPECIFIED., .F., .F.,
 ( 4, 4 ),
 ( 0.01172131844875056762, 0.02019504072144193141 ),
 .UNSPECIFIED. ) ;
#44483 = CARTESIAN_POINT ( 'NONE',  ( 196.6222993919940905, 288.9791602159129411, -16.90160481779407320 ) ) ;
#44484 = CARTESIAN_POINT ( 'NONE',  ( 207.3646600298985447, 271.4808684644054324, -5.284084612275558257 ) ) ;
#44485 = CARTESIAN_POINT ( 'NONE',  ( 165.0179060354396370, 286.2867116390483488, 3.417988829560836272 ) ) ;
#44487 = CARTESIAN_POINT ( 'NONE',  ( 185.9406580756425171, 265.4572926502605128, 14.02042132963198817 ) ) ;
#44486 = CARTESIAN_POINT ( 'NONE',  ( 73.71929281187129845, 69.57097904280846024, -9.712794511546583465 ) ) ;
#44488 = CARTESIAN_POINT ( 'NONE',  ( 27.82114452072190147, 69.44848197715137417, 59.99999999999999289 ) ) ;
#44489 = CARTESIAN_POINT ( 'NONE',  ( 33.58045587329145576, 41.16126292948898424, -6.180339887498951690 ) ) ;
#44490 = LINE ( 'NONE', #60179, #7795 ) ;
#44491 = CARTESIAN_POINT ( 'NONE',  ( 157.2744851780909414, 258.2395962677452985, 18.17792129701959070 ) ) ;
#44492 = CARTESIAN_POINT ( 'NONE',  ( 72.11830045305705994, 72.06781504142615802, 2.913192023061343949 ) ) ;
#44493 = CARTESIAN_POINT ( 'NONE',  ( 23.34166312890287998, 184.2833772461660544, -9.188101187500095079 ) ) ;
#44494 = ADVANCED_FACE ( 'NONE', ( #40764 ), #18502, .F. ) ;
#44495 = CARTESIAN_POINT ( 'NONE',  ( 187.4171132689631634, 261.5282790321019206, -9.397869408254909018 ) ) ;
#44496 = CARTESIAN_POINT ( 'NONE',  ( 81.57843032188139887, 42.64747388495735692, -7.641580732431849654 ) ) ;
#44497 = CARTESIAN_POINT ( 'NONE',  ( 194.2900850603946310, 294.1266965989547657, -15.88613936555681505 ) ) ;
#44498 = CARTESIAN_POINT ( 'NONE',  ( 72.12583136055069133, 72.30106763173874640, -1.396970068680259969 ) ) ;
#44499 = CARTESIAN_POINT ( 'NONE',  ( 43.96371950863733247, 202.3149278399160949, -9.188101187500095079 ) ) ;
#44500 = EDGE_CURVE ( 'NONE', #90241, #30665, #33704, .T. ) ;
#44501 = VECTOR ( 'NONE', #75585, 1000.000000000000000 ) ;
#44502 = CARTESIAN_POINT ( 'NONE',  ( 18.45699304436188015, 28.84336893147756342, -7.433330006724137462 ) ) ;
#44503 = CARTESIAN_POINT ( 'NONE',  ( 31.27486418823966119, 41.55466486950703597, 7.012934429366973338E-14 ) ) ;
#44504 = FACE_OUTER_BOUND ( 'NONE', #37095, .T. ) ;
#44505 = CARTESIAN_POINT ( 'NONE',  ( 34.47489329363036603, 42.83705186507756935, 3.090169943749475401 ) ) ;
#44506 = CARTESIAN_POINT ( 'NONE',  ( 202.5450565896906596, 269.8107279373824099, -6.424806493487884573 ) ) ;
#44507 = CARTESIAN_POINT ( 'NONE',  ( 175.7185668582631592, 291.0393361692799772, 2.533717797835123964 ) ) ;
#44508 = CARTESIAN_POINT ( 'NONE',  ( 176.2779124731408444, 274.9878774502150236, 17.29739640835781245 ) ) ;
#44509 = CARTESIAN_POINT ( 'NONE',  ( 73.35233208022572171, 64.24922777283234154, 13.69859057857681250 ) ) ;
#44510 = CARTESIAN_POINT ( 'NONE',  ( 73.94193992219132383, 67.36277748690798717, -11.91547202175585340 ) ) ;
#44511 = LINE ( 'NONE', #24094, #8547 ) ;
#44512 = CARTESIAN_POINT ( 'NONE',  ( -59.82327302696292293, 35.73826312759339174, -10.00000000000000000 ) ) ;
#44513 = CARTESIAN_POINT ( 'NONE',  ( 87.63502826371527021, 234.7365022471903444, 2.944929066748280225E-16 ) ) ;
#44514 = CARTESIAN_POINT ( 'NONE',  ( 161.6673510627899191, 250.6309293646106653, 13.01175935005004192 ) ) ;
#44515 = CARTESIAN_POINT ( 'NONE',  ( 165.1836928371452018, 269.6304300936849359, -16.29016501675020123 ) ) ;
#44516 = ORIENTED_EDGE ( 'NONE', *, *, #93241, .F. ) ;
#44517 = CARTESIAN_POINT ( 'NONE',  ( 49.53858449761714411, 211.6589784336661637, -6.496448406907675876E-16 ) ) ;
#44518 = EDGE_LOOP ( 'NONE', ( #54182, #30922, #55240 ) ) ;
#44519 = CARTESIAN_POINT ( 'NONE',  ( 88.92874521539408761, 44.69521367694441949, 1.972556413651489717E-15 ) ) ;
#44520 = CARTESIAN_POINT ( 'NONE',  ( 146.8881680668833951, 276.2292252078784145, 4.973452195244782104 ) ) ;
#44521 = CYLINDRICAL_SURFACE ( 'NONE', #75852, 17.82106496071139645 ) ;
#44522 = ORIENTED_EDGE ( 'NONE', *, *, #50435, .F. ) ;
#44523 = DIRECTION ( 'NONE',  ( -0.6384778167143362326, 0.7696402260561061581, 0.000000000000000000 ) ) ;
#44524 = CARTESIAN_POINT ( 'NONE',  ( 79.12983535314947403, 46.24050403399365194, -12.75843083597309402 ) ) ;
#44525 = DIRECTION ( 'NONE',  ( 0.000000000000000000, 0.000000000000000000, 1.000000000000000000 ) ) ;
#44526 = CARTESIAN_POINT ( 'NONE',  ( 176.9245165359646990, 274.6851866283708432, -17.45875439271293317 ) ) ;
#44527 = CARTESIAN_POINT ( 'NONE',  ( -19.65312891409030271, 93.06504152958497400, 60.00000000000000000 ) ) ;
#44528 = CARTESIAN_POINT ( 'NONE',  ( 204.6163864379986705, 276.2410179586759682, 14.66911174422491726 ) ) ;
#44529 = ORIENTED_EDGE ( 'NONE', *, *, #97601, .F. ) ;
#44530 = CARTESIAN_POINT ( 'NONE',  ( 27.97303175072023151, 18.01110640527293327, 2.839279412974134775 ) ) ;
#44531 = CARTESIAN_POINT ( 'NONE',  ( 68.55211899962544919, 64.27634076875820313, 12.40740400025066670 ) ) ;
#44532 = CARTESIAN_POINT ( 'NONE',  ( 69.01602661498650093, 69.91613256616328442, -3.960103623913056037 ) ) ;
#44533 = CARTESIAN_POINT ( 'NONE',  ( 154.2194984598485519, 265.5309884801890234, 17.12742652472672944 ) ) ;
#44534 = ORIENTED_EDGE ( 'NONE', *, *, #42382, .T. ) ;
#44535 = CARTESIAN_POINT ( 'NONE',  ( 77.33932581937109774, 58.33597099166552624, 16.55227366965920766 ) ) ;
#44536 = FACE_OUTER_BOUND ( 'NONE', #18425, .T. ) ;
#44537 = VECTOR ( 'NONE', #32977, 1000.000000000000227 ) ;
#44538 = VERTEX_POINT ( 'NONE', #96036 ) ;
#44539 =( BOUNDED_CURVE ( )  B_SPLINE_CURVE ( 2, ( #26207, #18613, #65199, #49490, #26701, #88561, #19126, #14492, #83928 ),
 .UNSPECIFIED., .F., .T. ) 
 B_SPLINE_CURVE_WITH_KNOTS ( ( 3, 2, 2, 2, 3 ),
 ( 0.09274193548387096864, 0.09408602150537634379, 0.09677419354838709409, 0.09946236559139784439, 0.1008064516129032334 ),
 .UNSPECIFIED. ) 
 CURVE ( )  GEOMETRIC_REPRESENTATION_ITEM ( )  RATIONAL_B_SPLINE_CURVE ( ( 0.9330127018922194093, 0.9330127018922194093, 1.000000000000000000, 0.8660254037844387076, 1.000000000000000000, 0.8660254037844387076, 1.000000000000000000, 0.9330127018922189652, 0.9330127018922192983 ) ) 
 REPRESENTATION_ITEM ( '' )  );
#44541 = CARTESIAN_POINT ( 'NONE',  ( 20.85854946042532276, 194.3967562850347122, -4.648177544792955347E-16 ) ) ;
#44540 = CARTESIAN_POINT ( 'NONE',  ( 170.4623819437503016, 288.8056674672355939, -5.476885062779371260 ) ) ;
#44542 = CARTESIAN_POINT ( 'NONE',  ( 162.8223739550644211, 248.6303710312858186, -11.16939803179192658 ) ) ;
#44543 = CARTESIAN_POINT ( 'NONE',  ( 65.95699843562651665, 69.05652685496262677, -2.081137445023961252 ) ) ;
#44544 = CARTESIAN_POINT ( 'NONE',  ( 188.0431710233438309, 294.4895058550014824, -10.95648900967039197 ) ) ;
#44545 = CARTESIAN_POINT ( 'NONE',  ( 81.89485588203808675, 55.22971306509116829, 16.24120679747551677 ) ) ;
#44546 = CARTESIAN_POINT ( 'NONE',  ( 205.5791761573774181, 272.5734172477073116, 10.13670412909801044 ) ) ;
#44548 = CARTESIAN_POINT ( 'NONE',  ( 120.0114017305758267, 252.3464784336661353, 1.353441290958777525E-15 ) ) ;
#44547 = AXIS2_PLACEMENT_3D ( 'NONE', #20886, #58356, #51775 ) ;
#44549 = CARTESIAN_POINT ( 'NONE',  ( 76.00665944866153723, 220.8149278399160664, 9.188101187500093303 ) ) ;
#44550 = EDGE_LOOP ( 'NONE', ( #88976, #67263, #35747, #55180 ) ) ;
#44551 = CARTESIAN_POINT ( 'NONE',  ( 170.4098397670617828, 263.7867033673382480, 15.85021430837907630 ) ) ;
#44552 = CARTESIAN_POINT ( 'NONE',  ( 79.09182929055386069, 45.95956795106130244, 13.18793794369859818 ) ) ;
#44553 = VERTEX_POINT ( 'NONE', #3798 ) ;
#44554 = CARTESIAN_POINT ( 'NONE',  ( 200.5237418414733384, 281.6908991433180631, 17.12490243155320613 ) ) ;
#44555 = ORIENTED_EDGE ( 'NONE', *, *, #32346, .F. ) ;
#44556 = ORIENTED_EDGE ( 'NONE', *, *, #94262, .T. ) ;
#44557 = CARTESIAN_POINT ( 'NONE',  ( 76.27486002672000609, 65.07516076971148777, 14.62441312286923534 ) ) ;
#44558 = CARTESIAN_POINT ( 'NONE',  ( -19.65312891409030271, 93.06504152958497400, 10.00000000000000888 ) ) ;
#44559 = CARTESIAN_POINT ( 'NONE',  ( -6.699655929326435277, 178.4860189848785410, -2.679491924311252493 ) ) ;
#44560 = CARTESIAN_POINT ( 'NONE',  ( 84.51277906370384585, 42.32962709305126481, -4.653106241441020252 ) ) ;
#44561 = CARTESIAN_POINT ( 'NONE',  ( 81.29647558948052222, 56.17074938437520615, 16.09536513502975552 ) ) ;
#44562 = CARTESIAN_POINT ( 'NONE',  ( 194.3252252352508265, 294.0658320307167628, 14.07225870721148731 ) ) ;
#44563 = ADVANCED_FACE ( 'NONE', ( #11904 ), #58649, .T. ) ;
#44564 = CARTESIAN_POINT ( 'NONE',  ( 71.07161859112099478, 65.75594004187888686, 11.78334260209157236 ) ) ;
#44565 = ORIENTED_EDGE ( 'NONE', *, *, #55315, .F. ) ;
#44566 = EDGE_CURVE ( 'NONE', #70676, #22043, #55303, .T. ) ;
#44567 = CARTESIAN_POINT ( 'NONE',  ( 200.6583719735737645, 283.0965001081523269, -17.35266956530146132 ) ) ;
#44568 = CARTESIAN_POINT ( 'NONE',  ( 189.4308808934198680, 289.8491723414206831, 15.72891001903047048 ) ) ;
#44569 = EDGE_LOOP ( 'NONE', ( #59358, #59970, #45593, #65247 ) ) ;
#44570 = CARTESIAN_POINT ( 'NONE',  ( 0.1404396296823678947, 45.26966602009034801, 59.99999999999999289 ) ) ;
#44571 = CARTESIAN_POINT ( 'NONE',  ( 76.19538127100192071, 51.60791020780316529, -16.17731679098115549 ) ) ;
#44572 = EDGE_CURVE ( 'NONE', #26627, #5926, #72040, .T. ) ;
#44573 = CARTESIAN_POINT ( 'NONE',  ( 81.05763270389509501, 43.67158023151814916, 9.470390458390101074 ) ) ;
#44574 = CARTESIAN_POINT ( 'NONE',  ( 164.9171241593586217, 245.0021572482830550, 1.622680932994367220 ) ) ;
#44575 = CIRCLE ( 'NONE', #42907, 70.00000000000001421 ) ;
#44576 = CARTESIAN_POINT ( 'NONE',  ( 46.85966550219804816, 187.8615022471902023, 5.000000000000051514 ) ) ;
#44577 = CARTESIAN_POINT ( 'NONE',  ( 163.9354095869165633, 246.7025367662834014, -7.289870401565430313 ) ) ;
#44578 = CARTESIAN_POINT ( 'NONE',  ( 136.6287848093373043, 243.5643266524160140, 9.188101187500095079 ) ) ;
#44579 = VERTEX_POINT ( 'NONE', #79172 ) ;
#44580 = LINE ( 'NONE', #37972, #27107 ) ;
#44581 = CARTESIAN_POINT ( 'NONE',  ( 182.4211569912797586, 258.2722588617187967, 6.464551942522600569 ) ) ;
#44582 = CARTESIAN_POINT ( 'NONE',  ( 179.8841377953208109, 288.3657013325343428, -13.30019851817003307 ) ) ;
#44583 = VECTOR ( 'NONE', #56044, 1000.000000000000227 ) ;
#44584 = CARTESIAN_POINT ( 'NONE',  ( 79.51536559218330069, 59.45954251456831230, -16.20368373865058231 ) ) ;
#44585 = CARTESIAN_POINT ( 'NONE',  ( 68.00997593938822661, 67.42022595953058328, -7.990198427795091263 ) ) ;
#44586 = ORIENTED_EDGE ( 'NONE', *, *, #2141, .T. ) ;
#44587 = LINE ( 'NONE', #13235, #88343 ) ;
#44588 = CARTESIAN_POINT ( 'NONE',  ( 184.3179147726750386, 277.0395465893940354, -16.62992345926578253 ) ) ;
#44589 = CARTESIAN_POINT ( 'NONE',  ( 167.9496373820661290, 248.6204696539478789, -6.517719931589019744 ) ) ;
#44590 = CARTESIAN_POINT ( 'NONE',  ( 79.49951204047911801, 46.37032438487753438, 12.70281872619212926 ) ) ;
#44591 = CARTESIAN_POINT ( 'NONE',  ( 73.59092698701640245, 69.71842387940506569, -9.437048835751642883 ) ) ;
#44592 = CARTESIAN_POINT ( 'NONE',  ( 195.9531395617315752, 264.6018537701219202, 0.8289104891173008083 ) ) ;
#44593 = CARTESIAN_POINT ( 'NONE',  ( 146.8058449195592061, 276.3718130816831149, 4.181814292810413392 ) ) ;
#44594 = CARTESIAN_POINT ( 'NONE',  ( 71.38700058129320780, 71.90615381975096909, 0.1362715070751574220 ) ) ;
#44595 = VECTOR ( 'NONE', #34647, 1000.000000000000000 ) ;
#44596 = CARTESIAN_POINT ( 'NONE',  ( 204.6149525604204769, 276.2435015074934199, -13.22810747389629960 ) ) ;
#44597 = CARTESIAN_POINT ( 'NONE',  ( 196.2612106832813481, 270.7781520464870937, 11.97022677330632412 ) ) ;
#44598 = CARTESIAN_POINT ( 'NONE',  ( 25.25549177415141955, 22.78052372038641238, -10.00000000000000355 ) ) ;
#44599 = LINE ( 'NONE', #6119, #15964 ) ;
#44600 = DIRECTION ( 'NONE',  ( 0.2701803667135113662, 0.9628097264997651505, 0.000000000000000000 ) ) ;
#44601 = CARTESIAN_POINT ( 'NONE',  ( -22.42236680055709641, 157.8615022471902591, 0.000000000000000000 ) ) ;
#44602 = VECTOR ( 'NONE', #45066, 1000.000000000000114 ) ;
#44603 = CARTESIAN_POINT ( 'NONE',  ( 198.6755293322981117, 286.5308843062557571, 17.86676876308990103 ) ) ;
#44604 = CARTESIAN_POINT ( 'NONE',  ( 207.5570812576139303, 271.1475851215477064, 6.450149787450828676 ) ) ;
#44605 = CARTESIAN_POINT ( 'NONE',  ( -11.38080322590321281, 173.4244531367911293, -4.594050593750046652 ) ) ;
#44606 = CARTESIAN_POINT ( 'NONE',  ( 176.0078709123280589, 285.3975443765536397, -11.99210929984988816 ) ) ;
#44607 = ORIENTED_EDGE ( 'NONE', *, *, #21213, .T. ) ;
#44608 = CARTESIAN_POINT ( 'NONE',  ( 66.86791019689516702, 67.62081465971216687, -6.465500182084312542 ) ) ;
#44609 = PLANE ( 'NONE',  #58071 ) ;
#44610 = CARTESIAN_POINT ( 'NONE',  ( 150.9584389135710865, 269.1793093008492406, -15.82751450793727699 ) ) ;
#44611 = CARTESIAN_POINT ( 'NONE',  ( -2.422939729449180124, 181.6589784336661637, -6.496448406907676862E-16 ) ) ;
#44612 = EDGE_CURVE ( 'NONE', #62907, #99632, #64832, .T. ) ;
#44613 = CARTESIAN_POINT ( 'NONE',  ( 178.4187001493748426, 273.6290048830982755, -17.20285326387372038 ) ) ;
#44614 = CARTESIAN_POINT ( 'NONE',  ( 29.35192616055884685, 22.11029122506295863, -8.090169943749478065 ) ) ;
#44615 = CARTESIAN_POINT ( 'NONE',  ( 85.38233340156565987, 49.09383606134155542, 12.40279396366186404 ) ) ;
#44616 = CARTESIAN_POINT ( 'NONE',  ( 67.91490812815924016, 210.0177522451418497, -10.00000000000009592 ) ) ;
#44617 = CARTESIAN_POINT ( 'NONE',  ( 71.94697066620052794, 72.20377774097838142, -3.624262489285473343 ) ) ;
#44618 = DIRECTION ( 'NONE',  ( 0.03277852384265245167, -0.9994626398093610087, 0.000000000000000000 ) ) ;
#44620 = CARTESIAN_POINT ( 'NONE',  ( 69.21394623383588396, 220.7677522451419065, -5.000000000000047962 ) ) ;
#44619 = CARTESIAN_POINT ( 'NONE',  ( 198.6654679441890892, 270.7080073051427007, -10.97714029729529983 ) ) ;
#44621 = CARTESIAN_POINT ( 'NONE',  ( 175.9315981478186472, 252.7514783800165503, -3.278135643623982354 ) ) ;
#44622 = CARTESIAN_POINT ( 'NONE',  ( 150.2761558193201381, 270.3610582852369930, 14.81920478290713028 ) ) ;
#44623 = ADVANCED_FACE ( 'NONE', ( #9752 ), #83831, .F. ) ;
#44624 = CARTESIAN_POINT ( 'NONE',  ( 61.58209736653347477, 206.3615022471902307, -10.00000000000009592 ) ) ;
#44625 = CARTESIAN_POINT ( 'NONE',  ( 39.57658603661993624, 34.80066082961425877, 10.00000000000000533 ) ) ;
#44626 = CARTESIAN_POINT ( 'NONE',  ( 148.4049257185216106, 273.6021238924720365, 8.639190357831699529 ) ) ;
#44627 = CARTESIAN_POINT ( 'NONE',  ( 23.96437920969670898, 175.4548013555409796, -4.594050593750042211 ) ) ;
#44628 = CARTESIAN_POINT ( 'NONE',  ( 72.78963790118945099, 71.14248580567580404, -7.401817665068024077 ) ) ;
#44629 = EDGE_CURVE ( 'NONE', #92184, #43912, #76738, .T. ) ;
#44630 = CARTESIAN_POINT ( 'NONE',  ( 153.3127735718713609, 265.1014820546527631, 17.57722645152040641 ) ) ;
#44631 = CARTESIAN_POINT ( 'NONE',  ( 35.00289615805098009, 41.18502408145595695, 5.678558825948277544 ) ) ;
#44632 = CARTESIAN_POINT ( 'NONE',  ( -19.65312891409030271, 93.06504152958497400, -10.00000000000000888 ) ) ;
#44633 = LINE ( 'NONE', #83697, #53107 ) ;
#44634 = CARTESIAN_POINT ( 'NONE',  ( 185.2853394675401830, 266.6322772215058876, 13.29842321144261774 ) ) ;
#44635 = CARTESIAN_POINT ( 'NONE',  ( 39.64431452495995245, 58.26521502737223557, -10.00000000000000000 ) ) ;
#44636 = DIRECTION ( 'NONE',  ( -0.9055221650797476984, -0.4242989612870696758, 0.000000000000000000 ) ) ;
#44637 = CARTESIAN_POINT ( 'NONE',  ( 19.72235211587467063, 17.10170272979926764, -7.433330006724141015 ) ) ;
#44638 = CARTESIAN_POINT ( 'NONE',  ( 147.8503508990560533, 274.5626756563852950, 7.845851077393495743 ) ) ;
#44639 = CARTESIAN_POINT ( 'NONE',  ( -50.24117156905492720, 92.72553494444620981, 36.50000000000000000 ) ) ;
#44640 = CARTESIAN_POINT ( 'NONE',  ( 71.46833469722506038, 59.16469923302185663, 15.78718056386504642 ) ) ;
#44641 = AXIS2_PLACEMENT_3D ( 'NONE', #44457, #53555, #76859 ) ;
#44642 = CARTESIAN_POINT ( 'NONE',  ( 155.2419697281468416, 261.7600162942170527, 18.58580762350309357 ) ) ;
#44643 = ORIENTED_EDGE ( 'NONE', *, *, #63101, .T. ) ;
#44644 = CARTESIAN_POINT ( 'NONE',  ( 181.6645495853941839, 289.2224369541009992, 12.52750095734821123 ) ) ;
#44645 = CARTESIAN_POINT ( 'NONE',  ( 84.80046560730060889, 45.49911806156455185, -9.891506693440607734 ) ) ;
#44646 = CARTESIAN_POINT ( 'NONE',  ( 81.77267345883888083, 42.08915124187546297, 7.561132706673316939 ) ) ;
#44647 = ORIENTED_EDGE ( 'NONE', *, *, #58580, .T. ) ;
#44648 = LINE ( 'NONE', #68458, #48988 ) ;
#44649 = CARTESIAN_POINT ( 'NONE',  ( 67.15811240557331985, 69.28574695336774880, 1.445375503756383795 ) ) ;
#44650 = VECTOR ( 'NONE', #31716, 1000.000000000000114 ) ;
#44651 = CYLINDRICAL_SURFACE ( 'NONE', #5687, 70.00000000000002842 ) ;
#44652 = CARTESIAN_POINT ( 'NONE',  ( 203.0026270830780675, 279.0361311525880978, -16.61345826058821373 ) ) ;
#44653 = VERTEX_POINT ( 'NONE', #89287 ) ;
#44654 = ORIENTED_EDGE ( 'NONE', *, *, #70279, .T. ) ;
#44656 = CARTESIAN_POINT ( 'NONE',  ( 164.2851776226980860, 246.0967207574460929, 5.847738044744511754 ) ) ;
#44655 = LINE ( 'NONE', #77064, #6632 ) ;
#44657 = VERTEX_POINT ( 'NONE', #19835 ) ;
#44658 = CARTESIAN_POINT ( 'NONE',  ( 150.8757650385446993, 269.3225046528533539, 14.31332712971473953 ) ) ;
#44659 = FACE_OUTER_BOUND ( 'NONE', #93676, .T. ) ;
#44660 = CARTESIAN_POINT ( 'NONE',  ( 80.46516936217979321, 57.89407423507869055, 16.25250200478403428 ) ) ;
#44661 = DIRECTION ( 'NONE',  ( 1.000000000000000000, 0.000000000000000000, 0.000000000000000000 ) ) ;
#44662 = ORIENTED_EDGE ( 'NONE', *, *, #93701, .F. ) ;
#44663 = CARTESIAN_POINT ( 'NONE',  ( 156.0916382163451601, 277.5285333452508212, -10.52960063827285886 ) ) ;
#44664 = ORIENTED_EDGE ( 'NONE', *, *, #26998, .T. ) ;
#44665 = CARTESIAN_POINT ( 'NONE',  ( 164.3022921857394749, 246.0670774647090582, 1.862798784958315856 ) ) ;
#44666 = VECTOR ( 'NONE', #13814, 1000.000000000000114 ) ;
#44667 = DIRECTION ( 'NONE',  ( 0.000000000000000000, -0.000000000000000000, 1.000000000000000000 ) ) ;
#44668 = B_SPLINE_CURVE_WITH_KNOTS ( 'NONE', 3,
 ( #56191, #32408, #8120, #94247 ),
 .UNSPECIFIED., .F., .F.,
 ( 4, 4 ),
 ( 0.008701075091435968994, 0.01503270840399712274 ),
 .UNSPECIFIED. ) ;
#44669 = ORIENTED_EDGE ( 'NONE', *, *, #6967, .T. ) ;
#44670 = EDGE_CURVE ( 'NONE', #82029, #3452, #89576, .T. ) ;
#44671 = CARTESIAN_POINT ( 'NONE',  ( 190.6661865267473104, 300.4034729807058852, 4.523489664447863490 ) ) ;
#44672 = CARTESIAN_POINT ( 'NONE',  ( 172.2817675467364609, 263.9987076400973933, -16.71829096631468659 ) ) ;
#44673 = ORIENTED_EDGE ( 'NONE', *, *, #68143, .T. ) ;
#44674 = CARTESIAN_POINT ( 'NONE',  ( 158.6532002544261104, 274.8663221026905603, -12.72708391612727574 ) ) ;
#44675 = CARTESIAN_POINT ( 'NONE',  ( 187.4061870533930971, 294.1816329134088619, 12.04041381263369814 ) ) ;
#44676 = DIRECTION ( 'NONE',  ( 0.000000000000000000, 0.000000000000000000, 1.000000000000000000 ) ) ;
#44678 = VECTOR ( 'NONE', #69299, 1000.000000000000000 ) ;
#44677 = CARTESIAN_POINT ( 'NONE',  ( 170.5993847053230468, 287.8722104901659691, 7.679145147933459370 ) ) ;
#44679 = ORIENTED_EDGE ( 'NONE', *, *, #81177, .T. ) ;
#44680 = EDGE_LOOP ( 'NONE', ( #60118, #50775, #6637, #88033 ) ) ;
#44681 = CARTESIAN_POINT ( 'NONE',  ( 73.67010975928342020, 69.53433136659224090, 9.708230610803601834 ) ) ;
#44682 = FACE_OUTER_BOUND ( 'NONE', #79379, .T. ) ;
#44683 = CARTESIAN_POINT ( 'NONE',  ( 82.45129306854981621, 53.84777233740991420, 15.85475489262521620 ) ) ;
#44684 = CARTESIAN_POINT ( 'NONE',  ( 149.0323968763055689, 272.5153119669064949, 11.64231532207353403 ) ) ;
#44685 = CARTESIAN_POINT ( 'NONE',  ( 152.7531861616124615, 266.0707158804971186, 17.45453282433162556 ) ) ;
#44686 = EDGE_CURVE ( 'NONE', #52414, #65850, #5124, .T. ) ;
#44687 = CARTESIAN_POINT ( 'NONE',  ( 146.8175579285427546, 276.3515255550140068, 0.7851837772504086654 ) ) ;
#44688 = EDGE_CURVE ( 'NONE', #36928, #71064, #38246, .T. ) ;
#44689 = CARTESIAN_POINT ( 'NONE',  ( 191.1687199697037443, 299.5330595250031820, -8.491751560014430211 ) ) ;
#44690 = ORIENTED_EDGE ( 'NONE', *, *, #37574, .F. ) ;
#44691 = CARTESIAN_POINT ( 'NONE',  ( 79.26668090384839616, 56.12960650164554011, -16.16769687457144755 ) ) ;
#44692 = CARTESIAN_POINT ( 'NONE',  ( 30.63508420971764679, 41.18528772668520332, -1.583844403245363575 ) ) ;
#44694 = CARTESIAN_POINT ( 'NONE',  ( 66.62671586282783665, 69.45108170673691461, 2.068076428306299785 ) ) ;
#44693 = CARTESIAN_POINT ( 'NONE',  ( 196.9976074755333286, 289.4371302133026802, -16.79549473444794216 ) ) ;
#44695 = CARTESIAN_POINT ( 'NONE',  ( 169.5742172260261214, 287.1141421671970875, 4.090594757681383697 ) ) ;
#44696 = CARTESIAN_POINT ( 'NONE',  ( 86.51086010412997496, 43.19054546371415171, 3.687685646923426930 ) ) ;
#44697 = CARTESIAN_POINT ( 'NONE',  ( 104.8295012880686699, 222.1423013555409796, -4.594050593750043987 ) ) ;
#44698 = VERTEX_POINT ( 'NONE', #20333 ) ;
#44699 = CARTESIAN_POINT ( 'NONE',  ( 149.3744903853108212, 271.9227886283697444, -13.09816371469833740 ) ) ;
#44700 = CARTESIAN_POINT ( 'NONE',  ( 79.16171021146236342, 53.16507682567369386, -15.71592495584207150 ) ) ;
#44701 = CARTESIAN_POINT ( 'NONE',  ( 149.1694037875916194, 273.2954204789498363, 9.972691433298622954 ) ) ;
#44702 = CARTESIAN_POINT ( 'NONE',  ( 79.05185236193558751, 46.14960762662803972, 12.72882390507626127 ) ) ;
#44703 = CARTESIAN_POINT ( 'NONE',  ( 38.92905753611409381, 204.8297689869269220, -2.679491924311252493 ) ) ;
#44704 = CARTESIAN_POINT ( 'NONE',  ( 83.71005568810697639, 52.19702411997352698, -14.66788051681769822 ) ) ;
#44705 = VERTEX_POINT ( 'NONE', #5613 ) ;
#44706 = CARTESIAN_POINT ( 'NONE',  ( 169.0084691738961737, 254.5285646557595669, -11.70697648969032301 ) ) ;
#44707 = CARTESIAN_POINT ( 'NONE',  ( 83.43812176953721860, 42.81150887395778426, 7.143380295109257538 ) ) ;
#44708 = CARTESIAN_POINT ( 'NONE',  ( 206.9059968923335475, 272.2752963222270068, 6.902135944297345560 ) ) ;
#44709 = CARTESIAN_POINT ( 'NONE',  ( 47.13029843733273339, 198.0177522451418781, -10.00000000000009592 ) ) ;
#44710 = CARTESIAN_POINT ( 'NONE',  ( 114.4904897814500373, 249.1589784336661069, -6.496448406907676862E-16 ) ) ;
#44711 = CARTESIAN_POINT ( 'NONE',  ( -14.83262083840144996, 124.7156766241961208, 37.49999999999998579 ) ) ;
#44712 = CARTESIAN_POINT ( 'NONE',  ( 84.14312167556933275, 48.98415679381830756, 0.000000000000000000 ) ) ;
#44713 = DIRECTION ( 'NONE',  ( 0.4999999999999998890, -0.8660254037844385966, 0.000000000000000000 ) ) ;
#44714 = CARTESIAN_POINT ( 'NONE',  ( 172.9698904924519240, 250.6642211707864476, -4.168778760986519671 ) ) ;
#44715 = CARTESIAN_POINT ( 'NONE',  ( 36.16949087457737733, 197.8149278399160949, -9.188101187500095079 ) ) ;
#44716 = CIRCLE ( 'NONE', #14006, 17.82106496071138224 ) ;
#44717 = CARTESIAN_POINT ( 'NONE',  ( -19.69645137954583802, 93.20008560620287597, 59.99999999999999289 ) ) ;
#44718 = AXIS2_PLACEMENT_3D ( 'NONE', #58418, #88907, #19470 ) ;
#44719 = ORIENTED_EDGE ( 'NONE', *, *, #9126, .F. ) ;
#44720 = CARTESIAN_POINT ( 'NONE',  ( 73.05912352472130067, 69.60491006942920933, 9.219028434792550186 ) ) ;
#44721 = DIRECTION ( 'NONE',  ( 0.5840252505817135065, 0.000000000000000000, 0.8117354905897405937 ) ) ;
#44722 = DIRECTION ( 'NONE',  ( 0.000000000000000000, 0.000000000000000000, 1.000000000000000000 ) ) ;
#44723 = AXIS2_PLACEMENT_3D ( 'NONE', #91475, #5851, #36735 ) ;
#44724 = CARTESIAN_POINT ( 'NONE',  ( 190.7403173041394950, 300.2750747078583800, -4.254144485856557800 ) ) ;
#44725 = CARTESIAN_POINT ( 'NONE',  ( 81.71293863666839741, 41.47842697493793196, -5.166121441586708052 ) ) ;
#44726 = DIRECTION ( 'NONE',  ( -0.000000000000000000, -0.000000000000000000, -1.000000000000000000 ) ) ;
#44727 = CARTESIAN_POINT ( 'NONE',  ( 179.3575481875710693, 287.7525672830279291, -12.49454744750270585 ) ) ;
#44728 = CARTESIAN_POINT ( 'NONE',  ( 164.3438181478333036, 250.0973453384040113, 10.21369496864028292 ) ) ;
#44729 = CARTESIAN_POINT ( 'NONE',  ( 112.9482291249501174, 226.0177522451418213, 5.000000000000051514 ) ) ;
#44730 = VERTEX_POINT ( 'NONE', #21320 ) ;
#44731 = CARTESIAN_POINT ( 'NONE',  ( 79.18684305567127524, 59.44391592844133498, -16.53590917749600919 ) ) ;
#44732 = CARTESIAN_POINT ( 'NONE',  ( 202.7041331321765938, 279.5531378413010657, 17.14708438049711248 ) ) ;
#44733 = DIRECTION ( 'NONE',  ( -0.9981117208278914577, 0.06142469166373826922, 0.000000000000000000 ) ) ;
#44734 = EDGE_CURVE ( 'NONE', #57136, #54902, #41861, .T. ) ;
#44735 = AXIS2_PLACEMENT_3D ( 'NONE', #63450, #93894, #62424 ) ;
#44736 = CARTESIAN_POINT ( 'NONE',  ( 4.207654042216683266, 182.4244531367911293, -4.594050593750046652 ) ) ;
#44737 = CARTESIAN_POINT ( 'NONE',  ( 69.20949672380906748, 68.87578926811286806, -7.751714074739255445 ) ) ;
#44738 = VECTOR ( 'NONE', #17432, 1000.000000000000000 ) ;
#44739 = CARTESIAN_POINT ( 'NONE',  ( 192.2315437480665992, 272.1294165976894988, 14.32756029153346056 ) ) ;
#44740 = CARTESIAN_POINT ( 'NONE',  ( 71.78644915716171226, 58.70311003640473757, -15.46670377541668273 ) ) ;
#44741 = FACE_OUTER_BOUND ( 'NONE', #58960, .T. ) ;
#44743 = CARTESIAN_POINT ( 'NONE',  ( 59.17381130624904273, 192.7202760586659736, -5.415160957724236172E-17 ) ) ;
#44742 = CARTESIAN_POINT ( 'NONE',  ( 195.2495212664957194, 275.1290853193528392, -16.26662379558266380 ) ) ;
#44744 = EDGE_CURVE ( 'NONE', #20065, #39184, #11740, .T. ) ;
#44745 = CARTESIAN_POINT ( 'NONE',  ( 207.5215400641004351, 271.2091442744748520, 2.886080616848571534 ) ) ;
#44746 = CARTESIAN_POINT ( 'NONE',  ( 73.93007176995158147, 55.19876193233204020, 16.12294130170896622 ) ) ;
#44747 = CARTESIAN_POINT ( 'NONE',  ( -32.97666635132488011, 94.88921800892812541, 43.93259070532314325 ) ) ;
#44748 = CARTESIAN_POINT ( 'NONE',  ( 66.32312229954955285, 68.11665519946647862, -4.542135202938414551 ) ) ;
#44749 = EDGE_LOOP ( 'NONE', ( #40187, #92186, #88876, #93289 ) ) ;
#44750 = AXIS2_PLACEMENT_3D ( 'NONE', #88627, #89137, #19688 ) ;
#44751 = CARTESIAN_POINT ( 'NONE',  ( 16.62094515339138212, 173.7365022471902307, 10.00000000000009592 ) ) ;
#44752 = B_SPLINE_CURVE_WITH_KNOTS ( 'NONE', 3,
 ( #41512, #73929, #34424, #65324 ),
 .UNSPECIFIED., .F., .F.,
 ( 4, 4 ),
 ( 0.01189126407362384348, 0.01800151522966263185 ),
 .UNSPECIFIED. ) ;
#44753 = CARTESIAN_POINT ( 'NONE',  ( 164.0179800784044915, 246.5595204798204065, -5.772998092557310557 ) ) ;
#44754 = CARTESIAN_POINT ( 'NONE',  ( 131.5133883985292016, 255.9244531367911293, -4.594050593750046652 ) ) ;
#44755 = CARTESIAN_POINT ( 'NONE',  ( 23.58217936225004863, 25.56628583063841376, 9.188101187500006262 ) ) ;
#44757 = ADVANCED_FACE ( 'NONE', ( #40489 ), #62282, .T. ) ;
#44756 = CARTESIAN_POINT ( 'NONE',  ( 165.0728006432024699, 244.7325176687217549, 1.503174307937145793 ) ) ;
#44758 = CARTESIAN_POINT ( 'NONE',  ( -17.42236680055705023, 149.2012482093457777, 0.000000000000000000 ) ) ;
#44759 = CARTESIAN_POINT ( 'NONE',  ( 203.3946109532447224, 276.3571951737117729, -14.55139583984842133 ) ) ;
#44761 = CARTESIAN_POINT ( 'NONE',  ( 75.07027850253338386, 67.11046765588916685, 13.07895222455245055 ) ) ;
#44760 = CARTESIAN_POINT ( 'NONE',  ( 88.07864672190808619, 43.84249974723677923, 2.482382391715419523 ) ) ;
#44762 = CARTESIAN_POINT ( 'NONE',  ( 69.09645378865941723, 64.24355404979770867, 12.03626827164885604 ) ) ;
#44763 = ORIENTED_EDGE ( 'NONE', *, *, #65679, .F. ) ;
#44764 = DIRECTION ( 'NONE',  ( -0.7162481363636782339, 0.000000000000000000, 0.6978456900745019231 ) ) ;
#44765 = CARTESIAN_POINT ( 'NONE',  ( 207.8229629847965612, 270.6870644612629917, -0.3253519274997035415 ) ) ;
#44766 = CARTESIAN_POINT ( 'NONE',  ( 69.17795686453304427, 67.22120498262539456, -9.978070790114912825 ) ) ;
#44767 = CARTESIAN_POINT ( 'NONE',  ( 34.97213163436671124, 51.32435524152968753, -10.00000000000000000 ) ) ;
#44768 = CARTESIAN_POINT ( 'NONE',  ( 197.3243759857185182, 273.2497805167799356, -13.42310424059574636 ) ) ;
#44769 = ORIENTED_EDGE ( 'NONE', *, *, #9594, .F. ) ;
#44770 = CARTESIAN_POINT ( 'NONE',  ( 70.76518571626657206, 70.00280625673043744, 6.363910008508249838 ) ) ;
#44771 = CARTESIAN_POINT ( 'NONE',  ( 48.53010236944518851, 101.9116055364396090, 10.00000000000000000 ) ) ;
#44772 = EDGE_CURVE ( 'NONE', #33315, #71254, #69660, .T. ) ;
#44773 = EDGE_CURVE ( 'NONE', #39921, #25006, #35080, .T. ) ;
#44774 = CARTESIAN_POINT ( 'NONE',  ( -21.58168810074490551, 24.33735145887882112, -10.00000000000000000 ) ) ;
#44775 = CARTESIAN_POINT ( 'NONE',  ( 172.4831635826484444, 290.8796410925290843, -1.652085212636280609 ) ) ;
#44776 = CARTESIAN_POINT ( 'NONE',  ( 81.87359138893998534, 41.32955797152818889, 5.976920566253458134 ) ) ;
#44777 = DIRECTION ( 'NONE',  ( -0.9086904199442051855, 0.4174706225611858335, 0.000000000000000000 ) ) ;
#44778 = CARTESIAN_POINT ( 'NONE',  ( 153.0790963368640689, 265.5062228982576471, -17.74594954892339160 ) ) ;
#44779 = ORIENTED_EDGE ( 'NONE', *, *, #53702, .F. ) ;
#44780 = DIRECTION ( 'NONE',  ( -0.7082622432767082810, -0.7059494278973847958, 0.000000000000000000 ) ) ;
#44781 = CARTESIAN_POINT ( 'NONE',  ( 11.59314018038319283, 18.64441083166259361, -10.00000000000000533 ) ) ;
#44782 = DIRECTION ( 'NONE',  ( 0.2347357813929421555, -0.4065742997269585213, 0.8829475928589297640 ) ) ;
#44783 = ORIENTED_EDGE ( 'NONE', *, *, #69873, .T. ) ;
#44784 = CARTESIAN_POINT ( 'NONE',  ( 190.5477107455830321, 300.6086790531491033, 3.126266616601216963 ) ) ;
#44785 = FACE_OUTER_BOUND ( 'NONE', #97971, .T. ) ;
#44786 = CARTESIAN_POINT ( 'NONE',  ( 189.1342855833499925, 297.0966903347303969, 8.133747755478912822 ) ) ;
#44787 = ORIENTED_EDGE ( 'NONE', *, *, #4754, .F. ) ;
#44788 = CARTESIAN_POINT ( 'NONE',  ( 191.4852287632733123, 298.9848502134979071, -9.870565261052552941 ) ) ;
#44789 = CARTESIAN_POINT ( 'NONE',  ( 50.30020549591841927, 90.50945844122861672, 10.00000000000000000 ) ) ;
#44790 = B_SPLINE_CURVE_WITH_KNOTS ( 'NONE', 3,
 ( #46467, #84529, #69779, #30794, #15073, #45962, #61673, #92623, #23173, #31276, #62164, #93113, #23665, #85541, #16082, #1896 ),
 .UNSPECIFIED., .F., .F.,
 ( 4, 1, 2, 2, 2, 1, 2, 2, 4 ),
 ( 0.000000000000000000, 0.1250000000000054956, 0.1875000000000070499, 0.2500000000000086042, 0.5000000000000109912, 0.6250000000000103251, 0.6875000000000102141, 0.7500000000000101030, 1.000000000000000000 ),
 .UNSPECIFIED. ) ;
#44791 = CARTESIAN_POINT ( 'NONE',  ( 204.2129321040862919, 276.9398213635460024, 14.41515352680879758 ) ) ;
#44792 = CARTESIAN_POINT ( 'NONE',  ( 46.83931157395847578, 209.3967562850346837, 1.101618078115930403E-13 ) ) ;
#44793 = ORIENTED_EDGE ( 'NONE', *, *, #35071, .F. ) ;
#44794 = CARTESIAN_POINT ( 'NONE',  ( 82.14994038281616895, 227.4244531367911293, -4.594050593750046652 ) ) ;
#44795 = CARTESIAN_POINT ( 'NONE',  ( 203.5644143473884071, 278.0630870677574649, 15.19023846038192183 ) ) ;
#44796 = AXIS2_PLACEMENT_3D ( 'NONE', #79624, #10187, #70994 ) ;
#44797 = CARTESIAN_POINT ( 'NONE',  ( 181.2813888893848571, 271.4291121770711470, -16.07812310781979548 ) ) ;
#44798 = CARTESIAN_POINT ( 'NONE',  ( 81.64801244726884022, 42.30507044763769642, -8.030039233986487446 ) ) ;
#44799 = ORIENTED_EDGE ( 'NONE', *, *, #67248, .T. ) ;
#44800 = EDGE_CURVE ( 'NONE', #13224, #86658, #62474, .T. ) ;
#44801 = ORIENTED_EDGE ( 'NONE', *, *, #29347, .T. ) ;
#44802 = ORIENTED_EDGE ( 'NONE', *, *, #49958, .F. ) ;
#44803 = DIRECTION ( 'NONE',  ( 0.000000000000000000, 0.000000000000000000, 1.000000000000000000 ) ) ;
#44804 = ORIENTED_EDGE ( 'NONE', *, *, #20350, .F. ) ;
#44805 = CARTESIAN_POINT ( 'NONE',  ( 69.48788112159641628, 70.05884240972372368, 4.410909553017925866 ) ) ;
#44806 = EDGE_LOOP ( 'NONE', ( #5183, #34108, #76943, #87866 ) ) ;
#44807 = ADVANCED_FACE ( 'NONE', ( #11127 ), #43282, .F. ) ;
#44808 = DIRECTION ( 'NONE',  ( -0.7909930170786233505, 0.6118251767726273771, 0.000000000000000000 ) ) ;
#44809 = VECTOR ( 'NONE', #35881, 1000.000000000000227 ) ;
#44810 = DIRECTION ( 'NONE',  ( -0.000000000000000000, -0.000000000000000000, -1.000000000000000000 ) ) ;
#44811 = CARTESIAN_POINT ( 'NONE',  ( -23.54859545362356243, 99.76679586987334858, 45.19948259297560611 ) ) ;
#44812 = CARTESIAN_POINT ( 'NONE',  ( 82.74895235971042950, 53.70034252712168410, -15.76590362002541390 ) ) ;
#44813 = EDGE_CURVE ( 'NONE', #63549, #79661, #82552, .T. ) ;
#44814 = CARTESIAN_POINT ( 'NONE',  ( 165.0528804069804494, 264.4852527057752241, -17.76608744198970768 ) ) ;
#44815 = VERTEX_POINT ( 'NONE', #99206 ) ;
#44816 = CARTESIAN_POINT ( 'NONE',  ( -22.42236680055709641, 157.8615022471902591, 0.000000000000000000 ) ) ;
#44817 = CARTESIAN_POINT ( 'NONE',  ( 19.72235211587467063, 17.10170272979926764, -7.433330006724141015 ) ) ;
#44818 = ORIENTED_EDGE ( 'NONE', *, *, #6479, .T. ) ;
#44819 = EDGE_CURVE ( 'NONE', #6345, #12659, #91623, .T. ) ;
#44820 = CARTESIAN_POINT ( 'NONE',  ( 166.8217491802902259, 284.2403532778428712, 9.447065769108251132 ) ) ;
#44821 = CARTESIAN_POINT ( 'NONE',  ( 49.28760614098965220, 105.1966139777580338, 10.00000000000000000 ) ) ;
#44823 = ORIENTED_EDGE ( 'NONE', *, *, #49010, .F. ) ;
#44822 = CARTESIAN_POINT ( 'NONE',  ( 119.8764323552255604, 240.0177522451418497, -10.00000000000009592 ) ) ;
#44824 = EDGE_CURVE ( 'NONE', #40677, #91721, #45478, .T. ) ;
#44825 = CARTESIAN_POINT ( 'NONE',  ( 163.0171530587457767, 248.2930037274571191, 9.677214176418313940 ) ) ;
#44826 = APPLICATION_CONTEXT ( 'automotive_design' ) ;
#44827 = ADVANCED_FACE ( 'NONE', ( #37870 ), #76412, .F. ) ;
#44828 = CARTESIAN_POINT ( 'NONE',  ( 185.8333456925277289, 259.2190590162801982, 2.892714555682415867 ) ) ;
#44829 = CARTESIAN_POINT ( 'NONE',  ( 157.6030016657039994, 279.9469238675063139, -6.853747175795008140 ) ) ;
#44830 = CARTESIAN_POINT ( 'NONE',  ( -22.85267942241863182, 23.13820207187276168, 10.00000000000000000 ) ) ;
#44831 = DIRECTION ( 'NONE',  ( -0.000000000000000000, 0.000000000000000000, -1.000000000000000000 ) ) ;
#44832 = CARTESIAN_POINT ( 'NONE',  ( 161.1611771195837548, 251.5076483517112536, 14.17749514252127163 ) ) ;
#44833 = CARTESIAN_POINT ( 'NONE',  ( 160.2158583160598653, 282.4101726736743672, 2.089109771773170365 ) ) ;
#44834 =( BOUNDED_CURVE ( )  B_SPLINE_CURVE ( 2, ( #10540, #73342, #27734, #80477, #41925, #58121, #18644, #35318, #3451, #50030, #41414, #11047, #40903 ),
 .UNSPECIFIED., .F., .T. ) 
 B_SPLINE_CURVE_WITH_KNOTS ( ( 3, 2, 2, 2, 2, 2, 3 ),
 ( 0.4874999999999999889, 0.4899999999999999911, 0.4949999999999999956, 0.5000000000000000000, 0.5050000000000000044, 0.5100000000000000089, 0.5125000000000000666 ),
 .UNSPECIFIED. ) 
 CURVE ( )  GEOMETRIC_REPRESENTATION_ITEM ( )  RATIONAL_B_SPLINE_CURVE ( ( 0.9755282581475768211, 0.9755282581475768211, 1.000000000000000000, 0.9510565162951535312, 1.000000000000000000, 0.9510565162951535312, 1.000000000000000000, 0.9510565162951535312, 1.000000000000000000, 0.9510565162951535312, 1.000000000000000000, 0.9755282581475761550, 0.9755282581475767101 ) ) 
 REPRESENTATION_ITEM ( '' )  );
#44835 = ORIENTED_EDGE ( 'NONE', *, *, #4562, .T. ) ;
#44836 = CARTESIAN_POINT ( 'NONE',  ( 194.5990735076113936, 293.5915129094234430, -15.16177817946606865 ) ) ;
#44837 = CARTESIAN_POINT ( 'NONE',  ( 160.3456795905085812, 276.2092357212747515, 12.64195674795301727 ) ) ;
#44838 = CARTESIAN_POINT ( 'NONE',  ( 3.829028248110833754, 163.0177522451418213, 5.000000000000051514 ) ) ;
#44839 = CARTESIAN_POINT ( 'NONE',  ( 192.9426967849980485, 267.3039850408317193, -11.05276717515422114 ) ) ;
#44840 = CARTESIAN_POINT ( 'NONE',  ( 172.0926279537021344, 280.4607217264099290, -15.30784906875749840 ) ) ;
#44841 = CARTESIAN_POINT ( 'NONE',  ( 203.4577257922414333, 278.2478770658579492, -15.05669205718196402 ) ) ;
#44842 = CARTESIAN_POINT ( 'NONE',  ( 83.48498291495343437, 44.67303044464677697, -9.033275216153651144 ) ) ;
#44843 = CARTESIAN_POINT ( 'NONE',  ( 164.6063343576543048, 274.4739709976624908, 16.17759516952312637 ) ) ;
#44845 = CARTESIAN_POINT ( 'NONE',  ( 33.29424590502123493, 178.4824982072973683, 3.021315404115420679E-15 ) ) ;
#44844 = CARTESIAN_POINT ( 'NONE',  ( -2.801652295722365071, 175.3149278399160949, -9.188101187500095079 ) ) ;
#44846 = CARTESIAN_POINT ( 'NONE',  ( 189.0285275759924559, 297.0242660314676755, 8.140054971467193923 ) ) ;
#44847 = EDGE_LOOP ( 'NONE', ( #73757, #92572, #99055 ) ) ;
#44848 = ORIENTED_EDGE ( 'NONE', *, *, #10359, .T. ) ;
#44849 = FACE_OUTER_BOUND ( 'NONE', #18524, .T. ) ;
#44850 = FACE_OUTER_BOUND ( 'NONE', #10723, .T. ) ;
#44851 = DIRECTION ( 'NONE',  ( -0.6857383512133925496, -0.7278481391575704063, 0.000000000000000000 ) ) ;
#44852 = CARTESIAN_POINT ( 'NONE',  ( 63.33450210234187239, 195.8262482093458061, 3.021315404115420679E-15 ) ) ;
#44853 = CARTESIAN_POINT ( 'NONE',  ( 85.04377965201177858, 48.84687674572034410, 12.36303725827022149 ) ) ;
#44854 = CARTESIAN_POINT ( 'NONE',  ( 150.0982468106783472, 276.6106350970345034, 3.452134251224849404 ) ) ;
#44855 = CARTESIAN_POINT ( 'NONE',  ( 21.25804982287034406, 173.8923013555409796, 4.594050593750050204 ) ) ;
#44856 = CARTESIAN_POINT ( 'NONE',  ( 117.0885659928033817, 250.6589784336661637, -6.496448406907675876E-16 ) ) ;
#44857 = CARTESIAN_POINT ( 'NONE',  ( 87.72832916959468719, 44.38926273554258728, -3.984038184195087595 ) ) ;
#44858 = CARTESIAN_POINT ( 'NONE',  ( 66.31795133325435643, 69.20145725284447735, 2.477662600225432055 ) ) ;
#44859 = CARTESIAN_POINT ( 'NONE',  ( 206.5228006916347852, 272.3196060122579070, -7.607667339345448809 ) ) ;
#44860 = PLANE ( 'NONE',  #35551 ) ;
#44861 = VECTOR ( 'NONE', #52480, 1000.000000000000000 ) ;
#44862 = CARTESIAN_POINT ( 'NONE',  ( 77.25811804238409763, 54.54226996051674803, -16.06399464395360255 ) ) ;
#44863 = VECTOR ( 'NONE', #48127, 1000.000000000000000 ) ;
#44864 = CARTESIAN_POINT ( 'NONE',  ( 154.9226727788713731, 262.3130548330639726, 18.22497199616848818 ) ) ;
#44865 = CARTESIAN_POINT ( 'NONE',  ( 161.4816992964961742, 250.9524876563463067, -12.92750327687364198 ) ) ;
#44866 = CARTESIAN_POINT ( 'NONE',  ( 189.7876278749425580, 284.7637188201192089, 17.36559644418266757 ) ) ;
#44867 = CARTESIAN_POINT ( 'NONE',  ( -78.57153713424663977, 57.64153020465174393, -10.00000000000000000 ) ) ;
#44868 = B_SPLINE_CURVE_WITH_KNOTS ( 'NONE', 3,
 ( #85975, #46387, #47396, #77312 ),
 .UNSPECIFIED., .F., .F.,
 ( 4, 4 ),
 ( 7.858125020761361721E-17, 0.007288700693340222428 ),
 .UNSPECIFIED. ) ;
#44869 = CARTESIAN_POINT ( 'NONE',  ( 84.56695678370634539, 50.23807730109928826, 13.87492620287773804 ) ) ;
#44870 = CARTESIAN_POINT ( 'NONE',  ( -19.65312891409030271, 93.06504152958497400, 10.00000000000000888 ) ) ;
#44871 = FACE_OUTER_BOUND ( 'NONE', #18806, .T. ) ;
#44872 = CARTESIAN_POINT ( 'NONE',  ( 55.77019854693759271, 214.5530062829863311, -4.648177544792955347E-16 ) ) ;
#44873 = CARTESIAN_POINT ( 'NONE',  ( 48.91227514082039107, 78.96591507484178862, 10.00000000000000000 ) ) ;
#44874 = VECTOR ( 'NONE', #44782, 999.9999999999998863 ) ;
#44875 = CARTESIAN_POINT ( 'NONE',  ( 181.6437473107036169, 268.0140057806834761, 15.00620755021360964 ) ) ;
#44876 = CARTESIAN_POINT ( 'NONE',  ( 95.92559083146868204, 220.0643266524159856, -9.188101187500093303 ) ) ;
#44877 = CARTESIAN_POINT ( 'NONE',  ( 12.88253908977640094, 9.298606405272902720, -2.839279412974138328 ) ) ;
#44879 = ADVANCED_FACE ( 'NONE', ( #51598 ), #16084, .T. ) ;
#44878 = CARTESIAN_POINT ( 'NONE',  ( 67.68582956716421961, 65.71206495485193955, 10.68281714332846555 ) ) ;
#44881 = CARTESIAN_POINT ( 'NONE',  ( 83.06579348197817581, 42.04301930353511807, -4.596628070075716721 ) ) ;
#44880 = CARTESIAN_POINT ( 'NONE',  ( 9.678154728840961951, 27.36126292948894090, 6.180339887498949913 ) ) ;
#44882 = DIRECTION ( 'NONE',  ( -0.1889875038809470387, -0.9819794923402672682, 0.000000000000000000 ) ) ;
#44883 = CARTESIAN_POINT ( 'NONE',  ( 150.8247211172754589, 269.4109153179094278, -14.37608026040300402 ) ) ;
#44884 = PLANE ( 'NONE',  #12185 ) ;
#44885 = CARTESIAN_POINT ( 'NONE',  ( 41.60632629512001301, 26.94754757982093096, 5.678558825948272215 ) ) ;
#44886 = CARTESIAN_POINT ( 'NONE',  ( 192.5551423381268989, 297.1317055421444024, -13.20528585388119858 ) ) ;
#44887 = FACE_BOUND ( 'NONE', #99690, .T. ) ;
#44888 = VERTEX_POINT ( 'NONE', #38372 ) ;
#44889 = CARTESIAN_POINT ( 'NONE',  ( 29.48197064213787044, 19.94754757982090609, 5.678558825948272215 ) ) ;
#44890 = VECTOR ( 'NONE', #51937, 999.9999999999998863 ) ;
#44891 = CARTESIAN_POINT ( 'NONE',  ( 16.37683477841346047, 11.58380873178785642, 6.180339887498953466 ) ) ;
#44892 = CARTESIAN_POINT ( 'NONE',  ( 146.7842303614460207, 276.4092505945183689, -4.491116827832889236 ) ) ;
#44893 = CARTESIAN_POINT ( 'NONE',  ( 149.7109319212262051, 271.3400547943878109, -12.38605961032017433 ) ) ;
#44895 = VERTEX_POINT ( 'NONE', #94624 ) ;
#44894 = EDGE_CURVE ( 'NONE', #33624, #56899, #63687, .T. ) ;
#44896 = EDGE_CURVE ( 'NONE', #32075, #19304, #56393, .T. ) ;
#44897 = CARTESIAN_POINT ( 'NONE',  ( 70.73225150608038803, 60.85528942256977558, 14.53863242546318446 ) ) ;
#44898 = CARTESIAN_POINT ( 'NONE',  ( 159.5204760365350012, 254.3494259875849082, 16.90107507090185379 ) ) ;
#44899 = CARTESIAN_POINT ( 'NONE',  ( 171.9881733610453978, 253.5440279410006781, -8.835078667792725327 ) ) ;
#44900 = CARTESIAN_POINT ( 'NONE',  ( 136.0602820919951341, 259.3615022471902876, 5.000000000000046185 ) ) ;
#44901=STYLED_ITEM('',(#100338),#9388);
#44902 = ORIENTED_EDGE ( 'NONE', *, *, #96675, .F. ) ;
#44903 = CARTESIAN_POINT ( 'NONE',  ( 28.09809348231459936, 175.4824982072973967, 3.021315404115420679E-15 ) ) ;
#44904 = ORIENTED_EDGE ( 'NONE', *, *, #27524, .F. ) ;
#44905 = DIRECTION ( 'NONE',  ( -0.1550826972584531394, -0.9879014915521905360, 0.000000000000000000 ) ) ;
#44906 = CARTESIAN_POINT ( 'NONE',  ( 66.10335034196877757, 68.51773249980182356, 4.672338372422939479 ) ) ;
#44907 = EDGE_LOOP ( 'NONE', ( #36926, #74275, #16682, #1826 ) ) ;
#44908 = CARTESIAN_POINT ( 'NONE',  ( 181.9468416852762971, 290.8932940152133142, -10.89979107759946153 ) ) ;
#44909 = ORIENTED_EDGE ( 'NONE', *, *, #26473, .T. ) ;
#44910 = DIRECTION ( 'NONE',  ( 1.000000000000000000, 0.000000000000000000, 0.000000000000000000 ) ) ;
#44911 = CARTESIAN_POINT ( 'NONE',  ( 206.3088856847695922, 273.3095232714966869, 11.40914494729949880 ) ) ;
#44912 = CARTESIAN_POINT ( 'NONE',  ( 85.03805233423882726, 49.96613157754471501, 13.55353664355913956 ) ) ;
#44913 = CARTESIAN_POINT ( 'NONE',  ( 153.3548908812967966, 265.0285327348495912, -17.67588370404063625 ) ) ;
#44914 = CARTESIAN_POINT ( 'NONE',  ( 200.6583719735737645, 283.0965001081523269, -17.35266956530146132 ) ) ;
#44915 = DIRECTION ( 'NONE',  ( 0.3473291852294957405, -0.6015917957689906892, 0.7193398003386545225 ) ) ;
#44916 = CARTESIAN_POINT ( 'NONE',  ( 37.11382629638189457, 33.37878583063844218, 9.188101187500006262 ) ) ;
#44917 = CARTESIAN_POINT ( 'NONE',  ( 192.1943038168404314, 277.1473907896511264, 17.36549850453357635 ) ) ;
#44918 = CARTESIAN_POINT ( 'NONE',  ( 75.97978661270015266, 62.19592087238390121, -15.66257012141549687 ) ) ;
#44919 = CARTESIAN_POINT ( 'NONE',  ( 62.42776884207837895, 218.3967562850346837, -4.648177544792955347E-16 ) ) ;
#44920 = VERTEX_POINT ( 'NONE', #23667 ) ;
#44921 = VERTEX_POINT ( 'NONE', #25181 ) ;
#44922 = CARTESIAN_POINT ( 'NONE',  ( 205.1793861064249711, 275.2658739283173759, -14.08953480709093675 ) ) ;
#44923 = DIRECTION ( 'NONE',  ( 0.4552093898365224267, -0.8903844177683372108, 0.000000000000000000 ) ) ;
#44924 = CARTESIAN_POINT ( 'NONE',  ( 84.37825102736907468, 49.99960613749294680, 13.80049582259581520 ) ) ;
#44925 = EDGE_CURVE ( 'NONE', #17810, #69750, #98767, .T. ) ;
#44927 = CARTESIAN_POINT ( 'NONE',  ( 165.9766573681747559, 274.1408043494670892, -15.16394994857281020 ) ) ;
#44926 = CARTESIAN_POINT ( 'NONE',  ( 174.5179243658558335, 257.1845942475917468, -12.14858670780875904 ) ) ;
#44928 = CARTESIAN_POINT ( 'NONE',  ( 206.0061733044583434, 273.8338364942757153, -9.988470584493322590 ) ) ;
#44929 = CARTESIAN_POINT ( 'NONE',  ( 197.5903643141157886, 272.8324856170032149, -13.22247203134994997 ) ) ;
#44930 = CARTESIAN_POINT ( 'NONE',  ( 156.3551087084618700, 261.3239775484371989, -17.56576820129662053 ) ) ;
#44931 = CARTESIAN_POINT ( 'NONE',  ( 82.37522948072516726, 40.40699566382964036, 1.446055329426206848 ) ) ;
#44932 = VECTOR ( 'NONE', #49102, 1000.000000000000000 ) ;
#44933 = CARTESIAN_POINT ( 'NONE',  ( 170.3352017334123047, 289.0068553437270111, -4.481107825698984470 ) ) ;
#44934 = CARTESIAN_POINT ( 'NONE',  ( 77.06427544118604089, 63.50113506902185634, -15.44174958657458951 ) ) ;
#44935 = EDGE_CURVE ( 'NONE', #19698, #33352, #30796, .T. ) ;
#44936 = CARTESIAN_POINT ( 'NONE',  ( 184.0013592068560229, 285.0434840400766348, -15.03075733970070083 ) ) ;
#44937 = EDGE_CURVE ( 'NONE', #511, #96562, #92625, .T. ) ;
#44938 = CARTESIAN_POINT ( 'NONE',  ( 109.2943373587434053, 246.1589784336661069, -6.496448406907675876E-16 ) ) ;
#44939 = ORIENTED_EDGE ( 'NONE', *, *, #50862, .T. ) ;
#44940 = CARTESIAN_POINT ( 'NONE',  ( 183.4673376644933853, 260.0777518357641611, -9.504335236147220201 ) ) ;
#44941 = CARTESIAN_POINT ( 'NONE',  ( 28.93411276635479368, 38.74646525600392266, 2.839279412974139660 ) ) ;
#44942 = DIRECTION ( 'NONE',  ( 0.8660254037844395958, 0.4999999999999985567, 0.000000000000000000 ) ) ;
#44943 = VECTOR ( 'NONE', #46967, 1000.000000000000000 ) ;
#44944 = ORIENTED_EDGE ( 'NONE', *, *, #2733, .F. ) ;
#44945 = VECTOR ( 'NONE', #31432, 1000.000000000000000 ) ;
#44946 = CARTESIAN_POINT ( 'NONE',  ( 74.21927401529055146, 68.62113723208385352, -11.51360559050239374 ) ) ;
#44947 = EDGE_CURVE ( 'NONE', #36501, #75140, #63184, .T. ) ;
#44948 = EDGE_CURVE ( 'NONE', #68820, #46298, #85543, .T. ) ;
#44950 = CARTESIAN_POINT ( 'NONE',  ( 180.1752864420345475, 295.1175617866244920, -2.097363342680641729 ) ) ;
#44949 = B_SPLINE_SURFACE_WITH_KNOTS ( 'NONE', 3, 1, ( 
 ( #82616, #99762 ),
 ( #35951, #37434 ),
 ( #74977, #44036 ),
 ( #97781, #60722 ),
 ( #14657, #68345 ),
 ( #36948, #98781 ),
 ( #90203, #7047 ),
 ( #98278, #74491 ),
 ( #29364, #91685 ),
 ( #60230, #52637 ),
 ( #13665, #58738 ),
 ( #66852, #83593 ),
 ( #5558, #36444 ),
 ( #14157, #5069 ),
 ( #6561, #45044 ),
 ( #20777, #75987 ),
 ( #99269, #22247 ),
 ( #67349, #28865 ),
 ( #59743, #20274 ),
 ( #53149, #90713 ),
 ( #51148, #37927 ),
 ( #21268, #84104 ),
 ( #52146, #45534 ),
 ( #82111, #83095 ),
 ( #28349, #12684 ),
 ( #43551, #59228 ),
 ( #86610, #9571 ),
 ( #7543, #955 ),
 ( #32349, #69841 ),
 ( #94191, #31832 ),
 ( #78984, #85609 ),
 ( #93691, #38434 ),
 ( #454, #77469 ),
 ( #46026, #24254 ) ),
 .UNSPECIFIED., .T., .F., .F.,
 ( 4, 2, 2, 2, 2, 2, 2, 2, 2, 2, 2, 2, 2, 2, 2, 2, 4 ),
 ( 2, 2 ),
 ( 0.000000000000000000, 0.06250000000000000000, 0.1250000000000000000, 0.1875000000000000000, 0.2500000000000000000, 0.3125000000000000000, 0.3750000000000000000, 0.4375000000000000000, 0.5000000000000000000, 0.5625000000000000000, 0.6250000000000000000, 0.6875000000000000000, 0.7500000000000000000, 0.8125000000000000000, 0.8750000000000000000, 0.9375000000000000000, 1.000000000000000000 ),
 ( 0.000000000000000000, 1.000000000000000000 ),
 .UNSPECIFIED. ) ;
#44951 = CARTESIAN_POINT ( 'NONE',  ( 164.6675328809421330, 249.1567145543851325, 9.967022399947358835 ) ) ;
#44952 = CARTESIAN_POINT ( 'NONE',  ( 159.8946522441011382, 253.7013337850969492, -16.68230890105693121 ) ) ;
#44953 = DIRECTION ( 'NONE',  ( -0.8660254037844387076, -0.4999999999999998890, -0.000000000000000000 ) ) ;
#44954 = ORIENTED_EDGE ( 'NONE', *, *, #23190, .T. ) ;
#44955 = CARTESIAN_POINT ( 'NONE',  ( 148.7061709727940979, 273.0803518065333151, 9.839166884367505972 ) ) ;
#44956 = AXIS2_PLACEMENT_3D ( 'NONE', #45488, #53098, #77915 ) ;
#44957 = ORIENTED_EDGE ( 'NONE', *, *, #39206, .F. ) ;
#44958 = LINE ( 'NONE', #98698, #72173 ) ;
#44959 = ORIENTED_EDGE ( 'NONE', *, *, #15891, .F. ) ;
#44960 = CARTESIAN_POINT ( 'NONE',  ( 164.5348324038273518, 245.6643059921780718, 1.473102934610569958 ) ) ;
#44961 = AXIS2_PLACEMENT_3D ( 'NONE', #13555, #28742, #75357 ) ;
#44962 = CARTESIAN_POINT ( 'NONE',  ( 193.4228679857477005, 263.9407716114525897, 4.448677965214572261 ) ) ;
#44963 = CARTESIAN_POINT ( 'NONE',  ( 35.89232211637455094, 179.9824982072973683, 3.021315404115420679E-15 ) ) ;
#44964 = CARTESIAN_POINT ( 'NONE',  ( 192.6946760137320780, 261.4813915186712165, 3.932628284434791966E-12 ) ) ;
#44966 = CARTESIAN_POINT ( 'NONE',  ( 156.9403576227286976, 280.1547494552592070, 5.860362588905387859 ) ) ;
#44965 = DIRECTION ( 'NONE',  ( -0.8660254037844387076, -0.4999999999999998890, -0.000000000000000000 ) ) ;
#44967 = CARTESIAN_POINT ( 'NONE',  ( 201.4463813434794019, 281.7316278426353620, -17.16864527463587820 ) ) ;
#44968 = VERTEX_POINT ( 'NONE', #46990 ) ;
#44969 = CARTESIAN_POINT ( 'NONE',  ( 69.66731286396763778, 199.4824982072973967, 3.021315404115420679E-15 ) ) ;
#44971 = CARTESIAN_POINT ( 'NONE',  ( -44.26501565779586400, 27.25709555612339230, -10.00000000000000000 ) ) ;
#44970 = B_SPLINE_SURFACE_WITH_KNOTS ( 'NONE', 3, 1, ( 
 ( #64254, #87634 ),
 ( #95205, #12062 ),
 ( #19676, #95714 ),
 ( #50537, #72380 ),
 ( #10565, #18162 ),
 ( #58629, #65249 ),
 ( #49062, #26262 ),
 ( #57138, #27757 ),
 ( #65738, #79996 ),
 ( #26756, #81493 ),
 ( #42431, #89603 ),
 ( #42918, #41440 ),
 ( #88119, #20167 ),
 ( #73860, #18668 ),
 ( #49548, #51034 ),
 ( #19183, #80501 ),
 ( #11075, #81991 ),
 ( #41951, #72886 ),
 ( #3478, #34353 ),
 ( #96195, #57639 ),
 ( #11573, #88615 ),
 ( #50054, #81011 ),
 ( #73365, #28241 ),
 ( #45427, #36337 ),
 ( #43931, #21649 ),
 ( #6451, #20657 ),
 ( #84479, #53032 ),
 ( #74870, #60615 ),
 ( #51546, #53528 ),
 ( #99154, #44433 ),
 ( #21166, #52532 ),
 ( #82508, #29743 ),
 ( #14048, #67239 ),
 ( #92098, #91570 ) ),
 .UNSPECIFIED., .T., .F., .F.,
 ( 4, 2, 2, 2, 2, 2, 2, 2, 2, 2, 2, 2, 2, 2, 2, 2, 4 ),
 ( 2, 2 ),
 ( 0.000000000000000000, 0.06250000000000000000, 0.1250000000000000000, 0.1875000000000000000, 0.2500000000000000000, 0.3125000000000000000, 0.3750000000000000000, 0.4375000000000000000, 0.5000000000000000000, 0.5625000000000000000, 0.6250000000000000000, 0.6875000000000000000, 0.7500000000000000000, 0.8125000000000000000, 0.8750000000000000000, 0.9375000000000000000, 1.000000000000000000 ),
 ( 0.000000000000000000, 1.000000000000000000 ),
 .UNSPECIFIED. ) ;
#44972 = CARTESIAN_POINT ( 'NONE',  ( 190.4293642567297411, 263.8188777254847537, -9.661471042078789040 ) ) ;
#44973 = CARTESIAN_POINT ( 'NONE',  ( 170.4554201786903889, 249.5219033123342172, -0.2601445000210800274 ) ) ;
#44974 = CARTESIAN_POINT ( 'NONE',  ( 189.0767298292155942, 269.8417627541793991, -13.98674968934414409 ) ) ;
#44975 = CARTESIAN_POINT ( 'NONE',  ( 153.5028723857075761, 272.7411571805866970, -13.59438242947847719 ) ) ;
#44976 = CARTESIAN_POINT ( 'NONE',  ( 31.27486418823966119, 41.55466486950703597, 7.012934429366973338E-14 ) ) ;
#44977 = CARTESIAN_POINT ( 'NONE',  ( -35.82302091652844922, 24.69132351629776423, 10.00000000000000000 ) ) ;
#44978 = CARTESIAN_POINT ( 'NONE',  ( 26.00288702772274263, 192.4865022471903160, 10.00000000000009415 ) ) ;
#44979 = CARTESIAN_POINT ( 'NONE',  ( 86.31820828217628616, 211.4548013555409796, -4.594050593750042211 ) ) ;
#44980 = CARTESIAN_POINT ( 'NONE',  ( 206.7893622945242385, 272.4773133715531230, -10.52881283832460291 ) ) ;
#44981 = DIRECTION ( 'NONE',  ( -0.4999999999999974465, 0.8660254037844402619, 0.000000000000000000 ) ) ;
#44982 = CARTESIAN_POINT ( 'NONE',  ( 163.2000388741132895, 247.9762362032568035, -11.19676374274550312 ) ) ;
#44983 = EDGE_CURVE ( 'NONE', #34461, #63662, #79210, .T. ) ;
#44984 = CARTESIAN_POINT ( 'NONE',  ( 66.62014279665129379, 67.58845556211061023, 6.252763347840865293 ) ) ;
#44985 = CARTESIAN_POINT ( 'NONE',  ( 207.5462191418491500, 271.1663988579299485, -5.239401497773396699 ) ) ;
#44986 = CARTESIAN_POINT ( 'NONE',  ( 5.783292089056025098, 27.85010085989870277, -10.00000000000000000 ) ) ;
#44988 = CARTESIAN_POINT ( 'NONE',  ( 70.70420039156243774, 71.94848598797803163, 6.061257734329015641E-06 ) ) ;
#44987 = CARTESIAN_POINT ( 'NONE',  ( 73.51766844768523868, 69.20770085021928253, -10.00626470679032387 ) ) ;
#44989 = LINE ( 'NONE', #21219, #68562 ) ;
#44990 = FACE_OUTER_BOUND ( 'NONE', #91350, .T. ) ;
#44991 = CARTESIAN_POINT ( 'NONE',  ( 82.26031953026701160, 54.24911196204305242, 15.63359092428133401 ) ) ;
#44992 = CARTESIAN_POINT ( 'NONE',  ( 71.81276634784433099, 72.21619144530795609, 3.256612196116196234 ) ) ;
#44993 = CIRCLE ( 'NONE', #74108, 70.00000000000001421 ) ;
#44994 = CARTESIAN_POINT ( 'NONE',  ( 196.4677418905696129, 290.3548843276421394, 17.08610552292358520 ) ) ;
#44996 = ADVANCED_FACE ( 'NONE', ( #46469 ), #75709, .F. ) ;
#44995 = CARTESIAN_POINT ( 'NONE',  ( 81.19911097159209135, 42.30626095209706961, -7.446220821091688258 ) ) ;
#44997 = CIRCLE ( 'NONE', #77575, 12.50000000000000000 ) ;
#44998 = CARTESIAN_POINT ( 'NONE',  ( 165.9251183996210557, 249.1081943271603052, -9.381642927290494427 ) ) ;
#44999 = CARTESIAN_POINT ( 'NONE',  ( 71.77363275119753894, 72.50400781664164640, -1.333432854898964681 ) ) ;
#45000 = CARTESIAN_POINT ( 'NONE',  ( 48.05019010880389629, 207.7369531367911293, -4.594050593750048428 ) ) ;
#45001 = CIRCLE ( 'NONE', #95190, 15.10714546451156792 ) ;
#45002 = CARTESIAN_POINT ( 'NONE',  ( 16.96131155903493593, 31.83396525600390348, -2.839279412974133887 ) ) ;
#45003 = CARTESIAN_POINT ( 'NONE',  ( 171.2930143073555485, 286.6872321052386496, 7.314772950087515824 ) ) ;
#45004 = CARTESIAN_POINT ( 'NONE',  ( 149.3253462891332219, 272.0079086998416074, -12.99539319630191336 ) ) ;
#45005 = CARTESIAN_POINT ( 'NONE',  ( 46.16810866859812990, 28.78380873178791077, -6.180339887498949025 ) ) ;
#45006 = CARTESIAN_POINT ( 'NONE',  ( 157.1002372043759010, 258.5414026113353430, -17.73553732786789539 ) ) ;
#45007 = CARTESIAN_POINT ( 'NONE',  ( 202.8866346594412846, 269.9979106734580228, -6.436829395617527538 ) ) ;
#45008 = CARTESIAN_POINT ( 'NONE',  ( 175.9514560434575401, 291.1772476316439793, 2.554599904375252528 ) ) ;
#45009 = AXIS2_PLACEMENT_3D ( 'NONE', #43579, #74513, #13688 ) ;
#45010 = CARTESIAN_POINT ( 'NONE',  ( 176.1283921439560061, 274.8553815178914306, 16.96726162417416717 ) ) ;
#45011 = CARTESIAN_POINT ( 'NONE',  ( 72.09886792114333787, 59.49856892740179148, 15.29648596422838658 ) ) ;
#45012 = CARTESIAN_POINT ( 'NONE',  ( 152.7176750937324812, 276.5233964160840969, 7.187293814298707062 ) ) ;
#45013 = EDGE_CURVE ( 'NONE', #32492, #72476, #65315, .T. ) ;
#45014 = ADVANCED_FACE ( 'NONE', ( #72944 ), #42011, .F. ) ;
#45015 = CARTESIAN_POINT ( 'NONE',  ( -19.52224708177258705, 93.11966464384923370, 59.99999999999999289 ) ) ;
#45017 = EDGE_CURVE ( 'NONE', #16029, #57256, #51092, .T. ) ;
#45016 = CIRCLE ( 'NONE', #95279, 7.500000000000000000 ) ;
#45018 = CARTESIAN_POINT ( 'NONE',  ( 96.65612621980322672, 226.6115022471902307, 10.00000000000009592 ) ) ;
#45019 = CARTESIAN_POINT ( 'NONE',  ( 200.1103929410127762, 284.0456276340304953, 17.67835211026828901 ) ) ;
#45020 = CARTESIAN_POINT ( 'NONE',  ( 194.6617293356793539, 285.5289016145630399, -17.32716204712188102 ) ) ;
#45021 = VERTEX_POINT ( 'NONE', #88676 ) ;
#45022 = CARTESIAN_POINT ( 'NONE',  ( 48.48320281069610616, 207.9869531367911009, 4.594050593750046652 ) ) ;
#45023 = BREP_WITH_VOIDS ( 'NONE', #52348, ( #52172 ) );
#45024 = VERTEX_POINT ( 'NONE', #81550 ) ;
#45025 = CARTESIAN_POINT ( 'NONE',  ( 156.6812872898450735, 261.2670451491295012, 0.000000000000000000 ) ) ;
#45026 = CARTESIAN_POINT ( 'NONE',  ( -19.42194755839791753, 24.31068691715149299, -10.00000000000000000 ) ) ;
#45027 = CARTESIAN_POINT ( 'NONE',  ( 170.3127733705114224, 263.9010670580030364, 17.23448983536806622 ) ) ;
#45028 = ORIENTED_EDGE ( 'NONE', *, *, #93908, .F. ) ;
#45029 = AXIS2_PLACEMENT_3D ( 'NONE', #17959, #733, #2257 ) ;
#45030 = CARTESIAN_POINT ( 'NONE',  ( 178.6423073663378602, 290.9544255387157818, 10.03153667033594765 ) ) ;
#45031 = CARTESIAN_POINT ( 'NONE',  ( 79.33488432162613435, 46.38139623303920445, -12.77319259312810118 ) ) ;
#45032 = CARTESIAN_POINT ( 'NONE',  ( -19.65312891409030271, 93.06504152958497400, -10.00000000000000888 ) ) ;
#45033 = CARTESIAN_POINT ( 'NONE',  ( 176.0559032325554085, 274.2081378810889305, -17.70795040911156804 ) ) ;
#45034 = CARTESIAN_POINT ( 'NONE',  ( 206.9514768121390489, 271.8153902181765034, -5.779928228329159978 ) ) ;
#45035 = CARTESIAN_POINT ( 'NONE',  ( 204.9620549308181694, 275.6423025665365572, 14.49661402992083481 ) ) ;
#45036 = ORIENTED_EDGE ( 'NONE', *, *, #99722, .T. ) ;
#45037 = CARTESIAN_POINT ( 'NONE',  ( 21.52536902826200915, 24.37878583063841376, 9.188101187500006262 ) ) ;
#45038 = CARTESIAN_POINT ( 'NONE',  ( 75.81630083228941430, 58.88796208816045663, 15.95549709212262535 ) ) ;
#45039 = CARTESIAN_POINT ( 'NONE',  ( 70.06226729709648282, 70.14289581699462417, -5.146418532987001804 ) ) ;
#45040 = CARTESIAN_POINT ( 'NONE',  ( 75.06185269395857063, 67.24559711482957880, -12.98328508234621026 ) ) ;
#45041 = ORIENTED_EDGE ( 'NONE', *, *, #28321, .F. ) ;
#45042 = DIRECTION ( 'NONE',  ( -0.8660254037844361541, -0.5000000000000042188, -0.000000000000000000 ) ) ;
#45043 = B_SPLINE_CURVE_WITH_KNOTS ( 'NONE', 3,
 ( #35682, #21006, #20499, #45267, #76200, #6776, #75199, #66584, #52369, #74211, #68069, #91407, #43767, #51372, #98503, #13396, #83314, #97994, #98993, #13876, #75690, #6277, #90931, #37171, #60454, #5775, #12908, #21972, #99491, #82828, #74711 ),
 .UNSPECIFIED., .F., .F.,
 ( 4, 3, 3, 3, 3, 3, 3, 3, 3, 3, 4 ),
 ( 0.000000000000000000, 0.1333490885032327655, 0.3007194338854324855, 0.4699862290245073182, 0.5844252810809297261, 0.6686540514502762322, 0.7354980260655518132, 0.8028463152565620264, 0.8633854507757146024, 0.9437142632667205877, 1.000000000000000000 ),
 .UNSPECIFIED. ) ;
#45044 = CARTESIAN_POINT ( 'NONE',  ( 159.3237119419271437, 254.6902313965507858, -15.56765445935501191 ) ) ;
#45045 = ORIENTED_EDGE ( 'NONE', *, *, #66044, .T. ) ;
#45046 = CARTESIAN_POINT ( 'NONE',  ( 80.33776826693566875, 49.81241265353616399, -14.39611721561766799 ) ) ;
#45047 = CIRCLE ( 'NONE', #40195, 14.21260523776213347 ) ;
#45048 = EDGE_CURVE ( 'NONE', #35725, #58503, #34897, .T. ) ;
#45050 = CARTESIAN_POINT ( 'NONE',  ( 53.17212233558426959, 213.0530062829863311, -4.648177544792955347E-16 ) ) ;
#45049 = CARTESIAN_POINT ( 'NONE',  ( -13.11024591527723615, 4.999999999999999112, -32.50000000000017053 ) ) ;
#45051 = CARTESIAN_POINT ( 'NONE',  ( -105.0000000000000000, 4.999999999999999112, 54.99999999999999289 ) ) ;
#45052 = CARTESIAN_POINT ( 'NONE',  ( 204.7235752877335244, 276.0553614249301972, 14.82397698933823271 ) ) ;
#45053 = PLANE ( 'NONE',  #20536 ) ;
#45054 = CARTESIAN_POINT ( 'NONE',  ( 77.18288558774111152, 49.26002351683675329, -15.37362206159445144 ) ) ;
#45055 = CARTESIAN_POINT ( 'NONE',  ( 77.99518601148065500, 61.05539905302716619, -15.87786080876372985 ) ) ;
#45056 = CARTESIAN_POINT ( 'NONE',  ( 131.1618259000655371, 246.5333772461660544, 9.188101187500095079 ) ) ;
#45057 = CARTESIAN_POINT ( 'NONE',  ( 175.9407212156297078, 268.6798998318777194, 16.14890207857037652 ) ) ;
#45058 = CARTESIAN_POINT ( 'NONE',  ( 179.9705885308941902, 259.1087249338424954, 9.582984254543152502 ) ) ;
#45059 = CARTESIAN_POINT ( 'NONE',  ( 75.49289073487081225, 205.2048013555409796, 4.594050593750051981 ) ) ;
#45060 = ORIENTED_EDGE ( 'NONE', *, *, #11296, .F. ) ;
#45061 = CARTESIAN_POINT ( 'NONE',  ( 174.1167577371777782, 265.6544076377189185, 16.40429495823174832 ) ) ;
#45062 = CARTESIAN_POINT ( 'NONE',  ( 73.29685492166123595, 60.06436106922850371, -15.83144761987708549 ) ) ;
#45063 = CARTESIAN_POINT ( 'NONE',  ( 149.0807665407234026, 276.4376266709116408, -5.539133476438467873 ) ) ;
#45064 = AXIS2_PLACEMENT_3D ( 'NONE', #85023, #99704, #54068 ) ;
#45065 = ORIENTED_EDGE ( 'NONE', *, *, #47664, .T. ) ;
#45066 = DIRECTION ( 'NONE',  ( -0.2433040867433108045, -0.9699500612784162090, 0.000000000000000000 ) ) ;
#45067 = ORIENTED_EDGE ( 'NONE', *, *, #73547, .T. ) ;
#45068 = ORIENTED_EDGE ( 'NONE', *, *, #65872, .F. ) ;
#45069 = FACE_BOUND ( 'NONE', #32693, .T. ) ;
#45070 = FACE_OUTER_BOUND ( 'NONE', #8807, .T. ) ;
#45071 = CARTESIAN_POINT ( 'NONE',  ( -6.130263895410292818, 177.2677522451419350, -5.000000000000047962 ) ) ;
#45072 = CARTESIAN_POINT ( 'NONE',  ( 88.02796755599807454, 43.59779901362369259, -1.172627947537940913E-07 ) ) ;
#45073 = CARTESIAN_POINT ( 'NONE',  ( 109.1931406464380530, 245.3967562850346837, -4.648177544792955347E-16 ) ) ;
#45074 = CARTESIAN_POINT ( 'NONE',  ( 155.4917600441137324, 261.3273667757233056, 17.14261720787171939 ) ) ;
#45075 = CARTESIAN_POINT ( 'NONE',  ( 71.63128215215617445, 67.23017368855626330, 10.79322251376788877 ) ) ;
#45076 = CARTESIAN_POINT ( 'NONE',  ( 87.41847558182290356, 44.98594970355500777, 6.912341091792677084 ) ) ;
#45077 = ORIENTED_EDGE ( 'NONE', *, *, #93770, .F. ) ;
#45078 = CARTESIAN_POINT ( 'NONE',  ( 20.25339421822757302, 23.64441083166260782, -10.00000000000000533 ) ) ;
#45079 = CARTESIAN_POINT ( 'NONE',  ( 201.0973175254986245, 282.3362241104620125, -17.32135558411286524 ) ) ;
#45080 = AXIS2_PLACEMENT_3D ( 'NONE', #82918, #51979, #52964 ) ;
#45081 = VERTEX_POINT ( 'NONE', #50599 ) ;
#45082 = CARTESIAN_POINT ( 'NONE',  ( 76.28872632189685987, 51.00282802106350744, -16.03419075290740636 ) ) ;
#45083 = CARTESIAN_POINT ( 'NONE',  ( 175.2131407122271298, 254.6897258708467007, -7.357366922857768721 ) ) ;
#45084 = AXIS2_PLACEMENT_3D ( 'NONE', #8649, #25868, #41025 ) ;
#45085 = CARTESIAN_POINT ( 'NONE',  ( 66.18968672761215544, 68.49487770601442094, -4.881532527435788360 ) ) ;
#45087 = EDGE_CURVE ( 'NONE', #23902, #81619, #42983, .T. ) ;
#45086 = VECTOR ( 'NONE', #10337, 1000.000000000000000 ) ;
#45088 = CARTESIAN_POINT ( 'NONE',  ( 206.5571822944673670, 272.8794609281530938, 10.95833005210827515 ) ) ;
#45089 = CARTESIAN_POINT ( 'NONE',  ( 148.9831146496684084, 272.6006712873522133, -12.63706091291043343 ) ) ;
#45090 = CARTESIAN_POINT ( 'NONE',  ( -66.34925969370661392, 42.61035540433362456, 10.00000000000000000 ) ) ;
#45091 = DIRECTION ( 'NONE',  ( -1.000000000000000000, 0.000000000000000000, 0.000000000000000000 ) ) ;
#45092 = CIRCLE ( 'NONE', #92084, 70.00000000000001421 ) ;
#45093 = CARTESIAN_POINT ( 'NONE',  ( 143.3676317564762144, 244.3923013555409511, 4.594050593750050204 ) ) ;
#45094 = EDGE_LOOP ( 'NONE', ( #18756, #53749, #80279 ) ) ;
#45095 = CARTESIAN_POINT ( 'NONE',  ( 80.47590545208809942, 44.37644993918018343, -10.62012430727854806 ) ) ;
#45096 = CARTESIAN_POINT ( 'NONE',  ( 86.59400028779953118, 45.20624741140364478, 7.285646471211377317 ) ) ;
#45097 = CARTESIAN_POINT ( 'NONE',  ( 88.05069107734583156, 43.77613950941169918, -2.175448891271404506 ) ) ;
#45098 = CARTESIAN_POINT ( 'NONE',  ( 9.476883925432959543, 29.12856466152289414, 10.00000000000000000 ) ) ;
#45099 = CARTESIAN_POINT ( 'NONE',  ( 73.28493474805527796, 66.86745001568056068, -12.01134084813802438 ) ) ;
#45100 = ORIENTED_EDGE ( 'NONE', *, *, #30655, .T. ) ;
#45101 = LINE ( 'NONE', #27910, #63975 ) ;
#45102 = AXIS2_PLACEMENT_3D ( 'NONE', #90840, #7168, #99891 ) ;
#45103 = DIRECTION ( 'NONE',  ( 1.000000000000000000, 0.000000000000000000, 0.000000000000000000 ) ) ;
#45104 = PLANE ( 'NONE',  #2612 ) ;
#45105 = CARTESIAN_POINT ( 'NONE',  ( 81.29352784059901182, 52.88188998950131747, 15.35000877273065889 ) ) ;
#45106 = CARTESIAN_POINT ( 'NONE',  ( 73.68745215720861097, 69.36524252693955361, -9.936694521456994167 ) ) ;
#45107 = DIRECTION ( 'NONE',  ( -1.000000000000000000, 0.000000000000000000, 0.000000000000000000 ) ) ;
#45108 = CARTESIAN_POINT ( 'NONE',  ( 182.9443896863899113, 280.6423201065871353, 16.69554559524186743 ) ) ;
#45109 = B_SPLINE_CURVE_WITH_KNOTS ( 'NONE', 3,
 ( #71411, #55176, #79027, #61783, #63790, #47585, #86160, #9098, #16694, #87170, #85656, #93740, #54672, #46076, #85136, #86654 ),
 .UNSPECIFIED., .F., .F.,
 ( 4, 2, 2, 2, 2, 2, 2, 4 ),
 ( 3.002691588427585642E-15, 0.0005721413298776353764, 0.0008582119948149507941, 0.001144282659752266429, 0.001430353324689581738, 0.001716423989626897264, 0.002002494654564213224, 0.002288565319501528750 ),
 .UNSPECIFIED. ) ;
#45110 = VECTOR ( 'NONE', #70942, 1000.000000000000000 ) ;
#45111 = CARTESIAN_POINT ( 'NONE',  ( 159.7068082092014265, 262.5164536406643379, -17.81808555889180923 ) ) ;
#45112 = CARTESIAN_POINT ( 'NONE',  ( 170.6844402143995012, 263.2133925425807206, -17.01386034520750812 ) ) ;
#45113 = CARTESIAN_POINT ( 'NONE',  ( 19.48182849416020090, 34.18080186712593616, 3.090169943749475401 ) ) ;
#45114 = CARTESIAN_POINT ( 'NONE',  ( 30.68386671255119325, 44.42157463747831514, -10.00000000000000000 ) ) ;
#45115 = DIRECTION ( 'NONE',  ( -0.5000000000000001110, 0.8660254037844384856, 0.000000000000000000 ) ) ;
#45116 = CARTESIAN_POINT ( 'NONE',  ( 80.44297273216872668, 44.73620253192707708, -11.65665792466250927 ) ) ;
#45117 = CARTESIAN_POINT ( 'NONE',  ( 198.4264492142971221, 286.9623037257889564, 17.00126466006521397 ) ) ;
#45118 = CARTESIAN_POINT ( 'NONE',  ( 72.00136543793328769, 71.75253384267894319, -3.919387538446478025 ) ) ;
#45119 = CARTESIAN_POINT ( 'NONE',  ( 145.8571944687587632, 255.0177522451418497, -10.00000000000009592 ) ) ;
#45120 = FACE_OUTER_BOUND ( 'NONE', #98697, .T. ) ;
#45121 = ORIENTED_EDGE ( 'NONE', *, *, #70203, .T. ) ;
#45122 = CARTESIAN_POINT ( 'NONE',  ( 66.72975355781689188, 67.37222994295811418, -6.798010804002465157 ) ) ;
#45123 = CARTESIAN_POINT ( 'NONE',  ( 72.87252120309179304, 71.00776288696198435, -7.711505026642224259 ) ) ;
#45124 = CARTESIAN_POINT ( 'NONE',  ( 151.4428545556028780, 268.3402767968688067, -15.03309903163500749 ) ) ;
#45125 = CARTESIAN_POINT ( 'NONE',  ( 11.59636713795893925, 171.3768266524160424, 9.188101187500096856 ) ) ;
#45126 = CARTESIAN_POINT ( 'NONE',  ( 25.72017957606892580, 26.80066082961422680, 10.00000000000000533 ) ) ;
#45127 = CARTESIAN_POINT ( 'NONE',  ( 85.16413976203500624, 49.03542080487202526, 12.45445162886715451 ) ) ;
#45128 = CARTESIAN_POINT ( 'NONE',  ( 63.44840177721309971, 218.9860189848785126, -2.679491924311252493 ) ) ;
#45129 = CARTESIAN_POINT ( 'NONE',  ( 71.85042758235270810, 71.69843285251393183, -3.789477364735267084 ) ) ;
#45130 = CARTESIAN_POINT ( 'NONE',  ( 122.2995471069890812, 252.9637435831425023, 2.679491924311251605 ) ) ;
#45131 = CARTESIAN_POINT ( 'NONE',  ( 82.78613357252183391, 43.65115152597518033, 9.027654786050977265 ) ) ;
#45132 = CARTESIAN_POINT ( 'NONE',  ( 151.0480362197490933, 269.0241222143274626, 14.53796507407317762 ) ) ;
#45133 = EDGE_CURVE ( 'NONE', #47298, #59964, #82059, .T. ) ;
#45134 = EDGE_CURVE ( 'NONE', #60500, #51335, #39495, .T. ) ;
#45135 = CARTESIAN_POINT ( 'NONE',  ( 53.78786873247351252, 201.8615022471902307, -10.00000000000009592 ) ) ;
#45136 = FACE_OUTER_BOUND ( 'NONE', #55164, .T. ) ;
#45137 = CARTESIAN_POINT ( 'NONE',  ( 190.0515794655415789, 301.4680036374047063, -1.296825456579539626 ) ) ;
#45138 = EDGE_CURVE ( 'NONE', #91866, #56834, #94639, .T. ) ;
#45139 = CARTESIAN_POINT ( 'NONE',  ( 17.30628827445631401, 189.9869531367911293, 4.594050593750046652 ) ) ;
#45140 = CARTESIAN_POINT ( 'NONE',  ( 66.57727237866471626, 69.35756060501768161, -2.461574745472292935 ) ) ;
#45141 = EDGE_CURVE ( 'NONE', #15749, #84837, #55036, .T. ) ;
#45142 = CARTESIAN_POINT ( 'NONE',  ( 78.77203581278492095, 60.02538875188410827, 16.11206551482094795 ) ) ;
#45143 = CARTESIAN_POINT ( 'NONE',  ( 42.32740281844729680, 26.29860640527295601, -2.839279412974138328 ) ) ;
#45144 = PLANE ( 'NONE',  #98338 ) ;
#45146 = CARTESIAN_POINT ( 'NONE',  ( -22.42236680055709641, 157.8615022471902591, 0.000000000000000000 ) ) ;
#45145 = VECTOR ( 'NONE', #41381, 1000.000000000000000 ) ;
#45147 = CARTESIAN_POINT ( 'NONE',  ( 189.1267433986236597, 268.0052114195003128, 14.01527934077552473 ) ) ;
#45148 = DIRECTION ( 'NONE',  ( -0.8660254037844387076, -0.4999999999999998890, -0.000000000000000000 ) ) ;
#45149 = CARTESIAN_POINT ( 'NONE',  ( 160.3357114222172868, 280.0449195850608248, 9.200148331950654068 ) ) ;
#45150 = CONTEXT_DEPENDENT_SHAPE_REPRESENTATION ( #86923, #56401 ) ;
#45151 = CARTESIAN_POINT ( 'NONE',  ( 11.20403028766721398, 24.65586893147754921, -7.433330006724137462 ) ) ;
#45152 = CARTESIAN_POINT ( 'NONE',  ( 190.5674408456512765, 300.5745055173924811, -0.9151048603553563199 ) ) ;
#45153 = CARTESIAN_POINT ( 'NONE',  ( 71.94031269653281413, 59.11929964053626918, 15.37436981742643738 ) ) ;
#45154 = CARTESIAN_POINT ( 'NONE',  ( 147.4771028564622100, 275.6046161191591182, 9.141179566768406735E-14 ) ) ;
#45155 = ORIENTED_EDGE ( 'NONE', *, *, #53279, .F. ) ;
#45156 = AXIS2_PLACEMENT_3D ( 'NONE', #73986, #43042, #66371 ) ;
#45157 = CARTESIAN_POINT ( 'NONE',  ( 181.7992873095532786, 289.2334549628592981, 12.46585778909335929 ) ) ;
#45158 = CARTESIAN_POINT ( 'NONE',  ( 83.28414321500220296, 45.66981348057217360, -11.01983884672045910 ) ) ;
#45159 = CARTESIAN_POINT ( 'NONE',  ( 81.64255549193633499, 42.62546693999003367, 7.546458374570336858 ) ) ;
#45160 = EDGE_LOOP ( 'NONE', ( #3821, #51172, #82256, #47027 ) ) ;
#45161 = DIRECTION ( 'NONE',  ( 0.5000000000000014433, -0.8660254037844378194, 0.000000000000000000 ) ) ;
#45162 = DIRECTION ( 'NONE',  ( -1.000000000000000000, 0.000000000000000000, 0.000000000000000000 ) ) ;
#45163 = CARTESIAN_POINT ( 'NONE',  ( 165.3118168859175796, 246.3185293925050701, -4.432402497422931020 ) ) ;
#45164 = CARTESIAN_POINT ( 'NONE',  ( 203.2732885619977026, 278.5673317194472247, -16.64305493556850024 ) ) ;
#45165 = ORIENTED_EDGE ( 'NONE', *, *, #54153, .T. ) ;
#45166 = VECTOR ( 'NONE', #96697, 1000.000000000000114 ) ;
#45167 = VERTEX_POINT ( 'NONE', #48456 ) ;
#45169 = CARTESIAN_POINT ( 'NONE',  ( 152.8593402092683959, 275.2840601128194749, 10.96293945604634068 ) ) ;
#45168 = CARTESIAN_POINT ( 'NONE',  ( 201.6710194064352208, 279.8704541772306129, 16.35544272301150670 ) ) ;
#45170 = VERTEX_POINT ( 'NONE', #1859 ) ;
#45171 = CARTESIAN_POINT ( 'NONE',  ( 201.0844796915553161, 282.3584598911111812, -16.59562674965125950 ) ) ;
#45172 = CARTESIAN_POINT ( 'NONE',  ( 110.0000000000000000, 15.00000000000003908, -59.99999999999999289 ) ) ;
#45173 = CARTESIAN_POINT ( 'NONE',  ( 80.46882139176624094, 57.60428850591405592, -16.59250918983046574 ) ) ;
#45174 = CARTESIAN_POINT ( 'NONE',  ( 72.76796725029400648, 69.66064322242992546, -9.545088302685920567 ) ) ;
#45175 = EDGE_LOOP ( 'NONE', ( #75695, #68838, #7557, #72645 ) ) ;
#45176 = LINE ( 'NONE', #98905, #76610 ) ;
#45177 = VECTOR ( 'NONE', #88966, 1000.000000000000000 ) ;
#45178 = ORIENTED_EDGE ( 'NONE', *, *, #18879, .F. ) ;
#45179 = CARTESIAN_POINT ( 'NONE',  ( 205.7829192689729325, 274.2205238267313234, 11.21202327925415254 ) ) ;
#45180 = CARTESIAN_POINT ( 'NONE',  ( 75.18426732535230883, 66.40243072218130749, 13.13391322278640239 ) ) ;
#45181 = EDGE_LOOP ( 'NONE', ( #1324, #32663, #5972, #75340 ) ) ;
#45182 = CARTESIAN_POINT ( 'NONE',  ( 149.1903793729515257, 272.2416782560088677, 12.95958987445043675 ) ) ;
#45183 = DIRECTION ( 'NONE',  ( 0.5000000000000014433, -0.8660254037844378194, 0.000000000000000000 ) ) ;
#45184 = VERTEX_POINT ( 'NONE', #79893 ) ;
#45185 = CARTESIAN_POINT ( 'NONE',  ( -14.94286098042907440, 73.02398837676157939, 13.77360950052949917 ) ) ;
#45186 = CARTESIAN_POINT ( 'NONE',  ( 85.75863988884901801, 226.9865022471903160, 10.00000000000009415 ) ) ;
#45187 = CARTESIAN_POINT ( 'NONE',  ( 183.2707082818002107, 282.3109398786273800, 17.13350622414966296 ) ) ;
#45188 = CARTESIAN_POINT ( 'NONE',  ( 83.54910681719562149, 52.38058030375331242, 14.79278836691776533 ) ) ;
#45189 = ORIENTED_EDGE ( 'NONE', *, *, #3991, .F. ) ;
#45190 = ORIENTED_EDGE ( 'NONE', *, *, #78225, .F. ) ;
#45191 = CARTESIAN_POINT ( 'NONE',  ( 156.6433882741441721, 266.7315762886727271, -16.19180110469071465 ) ) ;
#45192 = CARTESIAN_POINT ( 'NONE',  ( 190.7908437487391780, 300.1875603386860689, -4.317984972589949955 ) ) ;
#45193 = CARTESIAN_POINT ( 'NONE',  ( 189.8314329296643450, 301.8493086226544619, -0.8085564604676659384 ) ) ;
#45194 = CARTESIAN_POINT ( 'NONE',  ( 190.7705347155322499, 300.2227366160529414, 3.504769718465625239 ) ) ;
#45195 = CARTESIAN_POINT ( 'NONE',  ( 192.2185419806677942, 297.7147144631093170, 12.45868041609393728 ) ) ;
#45196 = CARTESIAN_POINT ( 'NONE',  ( 191.5201351928026270, 298.9243905040425489, 8.280408090104206309 ) ) ;
#45197 = CARTESIAN_POINT ( 'NONE',  ( 147.2180753513904961, 275.6578090293250511, 0.4909717733184589261 ) ) ;
#45198 = CARTESIAN_POINT ( 'NONE',  ( 163.7500375660153793, 257.3530331621871028, 15.54842262632091909 ) ) ;
#45199 = EDGE_CURVE ( 'NONE', #15352, #12202, #16562, .T. ) ;
#45200 = CARTESIAN_POINT ( 'NONE',  ( 70.78197494834935810, 69.22129442327373283, 7.798897796936612004 ) ) ;
#45202 = CARTESIAN_POINT ( 'NONE',  ( 97.10949284993499475, 215.3262482093457493, 3.021315404115420679E-15 ) ) ;
#45201 = CARTESIAN_POINT ( 'NONE',  ( 149.5796913320911870, 271.5673701627850960, -12.80793412251569841 ) ) ;
#45203 = PLANE ( 'NONE',  #58997 ) ;
#45204 = CARTESIAN_POINT ( 'NONE',  ( 168.3419904543532937, 286.3602298079341040, 4.048007086931957765 ) ) ;
#45205 = CARTESIAN_POINT ( 'NONE',  ( 78.33405375115705738, 47.76087145685212931, 13.91665194331178768 ) ) ;
#45206 = CARTESIAN_POINT ( 'NONE',  ( 96.62871582839601103, 238.8464784336661637, 1.353441290958777327E-15 ) ) ;
#45207 = VERTEX_POINT ( 'NONE', #26158 ) ;
#45208 = CARTESIAN_POINT ( 'NONE',  ( 149.1483424966081657, 272.3144882616274458, -12.96605911529412403 ) ) ;
#45209 = CARTESIAN_POINT ( 'NONE',  ( 76.66452470125624075, 54.01436104093935597, -16.04660053521852703 ) ) ;
#45210 = CARTESIAN_POINT ( 'NONE',  ( 148.8371570812549294, 273.9697221964345886, 8.907495186123728814 ) ) ;
#45211 = LINE ( 'NONE', #78635, #5322 ) ;
#45212 = B_SPLINE_CURVE_WITH_KNOTS ( 'NONE', 3,
 ( #99258, #46015, #36939, #90700, #1323, #84582, #91675, #37918, #6551, #40290, #14145, #32205, #24607, #68830 ),
 .UNSPECIFIED., .F., .F.,
 ( 4, 2, 2, 2, 2, 2, 4 ),
 ( 0.000000000000000000, 0.2231112372999934090, 0.3346668559499891837, 0.4462224745999849307, 0.6693337118999764801, 0.7808893305499718940, 0.8924449491999673079 ),
 .UNSPECIFIED. ) ;
#45213 = DIRECTION ( 'NONE',  ( -1.000000000000000000, 0.000000000000000000, 1.082076799516502204E-16 ) ) ;
#45214 = CARTESIAN_POINT ( 'NONE',  ( 83.58053473790808141, 52.37444464214736684, -15.15899823554475212 ) ) ;
#45215 = CARTESIAN_POINT ( 'NONE',  ( 165.4103701307380163, 283.8590981551407708, -8.431619659680563927 ) ) ;
#45216 = ORIENTED_EDGE ( 'NONE', *, *, #86987, .F. ) ;
#45217 = CARTESIAN_POINT ( 'NONE',  ( 167.3001686924326918, 253.0705894573350179, -12.10497857386071985 ) ) ;
#45218 = CARTESIAN_POINT ( 'NONE',  ( 206.4484807199597753, 273.0677375780628608, -9.220527398138528952 ) ) ;
#45220 = EDGE_CURVE ( 'NONE', #83087, #24162, #48711, .T. ) ;
#45219 = CARTESIAN_POINT ( 'NONE',  ( 72.48454840684568978, 71.59325672763723958, 6.192859277029571174 ) ) ;
#45221 = CARTESIAN_POINT ( 'NONE',  ( 48.42933654300943402, 188.7677522451417929, -5.000000000000041744 ) ) ;
#45222 = CARTESIAN_POINT ( 'NONE',  ( 105.2078667585768557, 240.7369531367911009, -4.594050593750048428 ) ) ;
#45223 = FACE_OUTER_BOUND ( 'NONE', #77254, .T. ) ;
#45224 = VECTOR ( 'NONE', #23941, 1000.000000000000114 ) ;
#45225 = CYLINDRICAL_SURFACE ( 'NONE', #51301, 10.00000000000001066 ) ;
#45226 = CARTESIAN_POINT ( 'NONE',  ( 84.13204908911603752, 50.42604040346916605, 13.71367173376234838 ) ) ;
#45227 = CARTESIAN_POINT ( 'NONE',  ( 172.2247897617710066, 250.7459979994374066, -4.062067949591432914 ) ) ;
#45228 = CARTESIAN_POINT ( 'NONE',  ( 26.15589859543730000, 198.1589784336661637, -6.496448406907675876E-16 ) ) ;
#45229 = CARTESIAN_POINT ( 'NONE',  ( 147.7917198021585534, 275.6304213403500398, -3.790807063116589770 ) ) ;
#45230 = AXIS2_PLACEMENT_3D ( 'NONE', #65802, #81556, #34902 ) ;
#45231 = ORIENTED_EDGE ( 'NONE', *, *, #72191, .F. ) ;
#45232 = CARTESIAN_POINT ( 'NONE',  ( 75.06695094285400671, 67.05599132900850634, -12.66018568268392208 ) ) ;
#45233 = CARTESIAN_POINT ( 'NONE',  ( 177.9867648153962989, 265.4645870862016181, 15.84164618472818198 ) ) ;
#45234 = PLANE ( 'NONE',  #33628 ) ;
#45235 = CARTESIAN_POINT ( 'NONE',  ( -53.68831936616818723, 31.89637462494507858, 177.5919119679930134 ) ) ;
#45236 = CARTESIAN_POINT ( 'NONE',  ( 81.73784743073348125, 41.66220971920373017, -5.569503698209836706 ) ) ;
#45237 = CARTESIAN_POINT ( 'NONE',  ( 105.0000000000000000, 4.999999999999999112, 59.99999999999999289 ) ) ;
#45238 = AXIS2_PLACEMENT_3D ( 'NONE', #38005, #39498, #70425 ) ;
#45239 = CARTESIAN_POINT ( 'NONE',  ( 165.9669116182938353, 251.0260590123588145, 10.21599650959468519 ) ) ;
#45240 = CARTESIAN_POINT ( 'NONE',  ( 113.8864233123832577, 229.8927522451418213, 10.00000000000009592 ) ) ;
#45241 = ORIENTED_EDGE ( 'NONE', *, *, #7646, .T. ) ;
#45242 = LINE ( 'NONE', #28053, #98266 ) ;
#45243 = B_SPLINE_CURVE_WITH_KNOTS ( 'NONE', 3,
 ( #95350, #12700, #57769, #65870, #41573, #43570, #81134, #64386, #11700, #25905, #21286, #28884, #52162, #67879, #44554, #45555 ),
 .UNSPECIFIED., .F., .F.,
 ( 4, 2, 2, 2, 2, 2, 2, 4 ),
 ( 1.040834085586084257E-17, 0.0003787177898466214700, 0.0007574355796932325316, 0.001136153369539843593, 0.001514871159386454655, 0.001893588949233065716, 0.002272306739079676778, 0.003029742318772891529 ),
 .UNSPECIFIED. ) ;
#45244 = CARTESIAN_POINT ( 'NONE',  ( 154.9032082715209810, 280.6326124547101699, -2.389722542998433230 ) ) ;
#45245 = CARTESIAN_POINT ( 'NONE',  ( 154.0193023235302689, 265.1638567325853728, 16.81819982589781048 ) ) ;
#45246 = VECTOR ( 'NONE', #21624, 999.9999999999998863 ) ;
#45247 = CARTESIAN_POINT ( 'NONE',  ( 21.25804982287034406, 173.8923013555409796, 4.594050593750050204 ) ) ;
#45248 = CARTESIAN_POINT ( 'NONE',  ( 14.99119413235835729, 10.78380873178785393, -6.180339887498949025 ) ) ;
#45249 = CARTESIAN_POINT ( 'NONE',  ( 196.0356377417433862, 273.4210236615080589, 15.17726198895217493 ) ) ;
#45250 = CARTESIAN_POINT ( 'NONE',  ( 71.67621869789168443, 58.80470100248025034, -15.42187440688404010 ) ) ;
#45251 = CARTESIAN_POINT ( 'NONE',  ( -62.95439910331221256, 68.06504152958493137, 45.00000000000000711 ) ) ;
#45252 = ADVANCED_FACE ( 'NONE', ( #32743 ), #56023, .T. ) ;
#45254 = CARTESIAN_POINT ( 'NONE',  ( 64.39641960523518094, 217.1744531367911293, 4.594050593750047540 ) ) ;
#45253 = CARTESIAN_POINT ( 'NONE',  ( 194.7629524071031426, 274.9938599527168890, -15.98506956286481895 ) ) ;
#45255 = CARTESIAN_POINT ( 'NONE',  ( 207.6172352878830907, 271.0433952848413810, 3.316653249540578496 ) ) ;
#45256 = VECTOR ( 'NONE', #62807, 1000.000000000000114 ) ;
#45257 = CARTESIAN_POINT ( 'NONE',  ( 72.71764745495315196, 57.12077235107377504, 16.37631838998483857 ) ) ;
#45258 = CARTESIAN_POINT ( 'NONE',  ( 66.21002856626215305, 68.68800931748855021, -4.337945611540375168 ) ) ;
#45259 = ORIENTED_EDGE ( 'NONE', *, *, #80889, .F. ) ;
#45260 = CARTESIAN_POINT ( 'NONE',  ( 17.34263298987844237, 167.4865022471901739, 1.119607411625061291E-15 ) ) ;
#45261 = B_SPLINE_CURVE_WITH_KNOTS ( 'NONE', 3,
 ( #39002, #94256, #522, #39488 ),
 .UNSPECIFIED., .F., .F.,
 ( 4, 4 ),
 ( 0.009195655101482617944, 0.01511765829135664103 ),
 .UNSPECIFIED. ) ;
#45262 = CARTESIAN_POINT ( 'NONE',  ( 207.8302079587528794, 270.6745157982714431, 3.572475529330238153 ) ) ;
#45263 = CARTESIAN_POINT ( 'NONE',  ( 140.7695555451228984, 242.8923013555409796, 4.594050593750050204 ) ) ;
#45264 = CARTESIAN_POINT ( 'NONE',  ( 25.31423016981892715, 26.56628583063841731, 9.188101187500006262 ) ) ;
#45265 = CYLINDRICAL_SURFACE ( 'NONE', #26500, 16.60714546451156792 ) ;
#45266 = EDGE_CURVE ( 'NONE', #19562, #10543, #70940, .T. ) ;
#45267 = CARTESIAN_POINT ( 'NONE',  ( 83.66208585045004043, 52.31085355490836264, -15.11568120807085336 ) ) ;
#45268 = CARTESIAN_POINT ( 'NONE',  ( 206.1585898378126274, 271.5698433145930721, 8.212139725584252758 ) ) ;
#45270 = CARTESIAN_POINT ( 'NONE',  ( 189.2726224819945458, 299.8637631263580943, 4.914554397034637923 ) ) ;
#45269 = CARTESIAN_POINT ( 'NONE',  ( 88.09744597521934395, 43.85530739230785713, 2.493575494356681688 ) ) ;
#45271 = CARTESIAN_POINT ( 'NONE',  ( 68.69116047246832579, 64.25973440136523607, 12.48137981580948441 ) ) ;
#45272 = ORIENTED_EDGE ( 'NONE', *, *, #9843, .F. ) ;
#45273 = DIRECTION ( 'NONE',  ( -0.000000000000000000, -0.000000000000000000, -1.000000000000000000 ) ) ;
#45274 = CARTESIAN_POINT ( 'NONE',  ( 75.75493378409400691, 65.86437009324527025, -14.07593894684413804 ) ) ;
#45275 = CARTESIAN_POINT ( 'NONE',  ( 156.6772434156269753, 280.3381848834534935, -5.402216236100986890 ) ) ;
#45276 = CARTESIAN_POINT ( 'NONE',  ( 3.278110179240818045, 23.93396525600387648, 2.839279412974139660 ) ) ;
#45277 = EDGE_LOOP ( 'NONE', ( #89043, #11870, #38432, #14638 ) ) ;
#45278 = DIRECTION ( 'NONE',  ( -0.8845109580947931871, 0.1124011590738229760, -0.4527762631246169400 ) ) ;
#45279 = CARTESIAN_POINT ( 'NONE',  ( 170.1203493898869397, 283.3057450205278087, -11.00909384804022473 ) ) ;
#45280 = CARTESIAN_POINT ( 'NONE',  ( 71.69150499680799271, 72.11108097137680772, 0.6386526183549271485 ) ) ;
#45281 = CARTESIAN_POINT ( 'NONE',  ( 148.7749086576190791, 273.3915829829758195, -9.018907845894478470 ) ) ;
#45282 = CARTESIAN_POINT ( 'NONE',  ( 196.1574275305892741, 271.0118636216350865, 12.32861447576741298 ) ) ;
#45283 = CARTESIAN_POINT ( 'NONE',  ( 107.5017976953482446, 221.3262482093458061, 3.021315404115420679E-15 ) ) ;
#45284 = CARTESIAN_POINT ( 'NONE',  ( 69.33671394560225565, 70.52709464844167542, 2.076833668242843434 ) ) ;
#45285 = CARTESIAN_POINT ( 'NONE',  ( 200.9521687275011175, 282.5876292032514243, -18.16013154125647944 ) ) ;
#45286 = VERTEX_POINT ( 'NONE', #82407 ) ;
#45287 = CARTESIAN_POINT ( 'NONE',  ( 190.5050603160280787, 281.5143243275973077, 17.11203965365400492 ) ) ;
#45288 = CARTESIAN_POINT ( 'NONE',  ( 13.83924611881801958, 13.15404122711132118, 8.090169943749479842 ) ) ;
#45289 = CARTESIAN_POINT ( 'NONE',  ( 164.6077667029246925, 248.8717717204749817, 10.07792378446523607 ) ) ;
#45290 = ORIENTED_EDGE ( 'NONE', *, *, #82639, .T. ) ;
#45291 = CARTESIAN_POINT ( 'NONE',  ( 149.7166446726674565, 271.3301600186404698, 12.26048591517335495 ) ) ;
#45292 = DIRECTION ( 'NONE',  ( 0.8718556560469403749, 0.4897629171537585813, 0.000000000000000000 ) ) ;
#45293 = CARTESIAN_POINT ( 'NONE',  ( 189.0786975680280477, 297.0699590293599499, 8.119915869620735194 ) ) ;
#45294 = ORIENTED_EDGE ( 'NONE', *, *, #10391, .F. ) ;
#45295 = VECTOR ( 'NONE', #71261, 1000.000000000000000 ) ;
#45296 = CARTESIAN_POINT ( 'NONE',  ( 146.7373254022577100, 276.4904923669593586, -0.7242168585908188572 ) ) ;
#45297 = CARTESIAN_POINT ( 'NONE',  ( 165.9013214703126948, 280.3534790633716511, 13.25418706671784541 ) ) ;
#45298 = B_SPLINE_CURVE_WITH_KNOTS ( 'NONE', 3,
 ( #93881, #53168, #37451, #51683, #36462, #36962, #84606, #82632, #83107, #52656, #91204, #60245, #45061, #29868, #91701, #60739, #76958, #5570, #92221, #38450, #53650, #21765, #67363, #13193, #29377, #52159, #28366, #59242, #75485, #98291, #90222, #44551, #22773, #6068, #98796, #44049, #45551, #83608, #14176, #28880, #20791, #74990, #76002, #13678, #90726, #67875, #6579, #22264 ),
 .UNSPECIFIED., .F., .F.,
 ( 4, 2, 2, 2, 2, 2, 2, 2, 2, 2, 2, 2, 2, 2, 2, 2, 2, 2, 2, 2, 2, 2, 2, 4 ),
 ( 0.001171907001705587087, 0.001643730509668527798, 0.002115554017631468726, 0.002351465771612907749, 0.002587377525594346771, 0.002705333402585056307, 0.002823289279575765410, 0.003059201033557106420, 0.003531024541519774129, 0.004002848049482442272, 0.004946495065407923407, 0.005890142081333404542, 0.006361965589296181105, 0.006833789097258956800, 0.006951744974249671541, 0.007010722912745051896, 0.007069700851240433119, 0.007187656728231248474, 0.007305612605222063828, 0.007541524359203702343, 0.007777436113185339991, 0.008013347867166977639, 0.008249259621148617022, 0.008721083129111881910 ),
 .UNSPECIFIED. ) ;
#45299 = CARTESIAN_POINT ( 'NONE',  ( 164.2297246530060875, 246.1927681183832988, 5.803160395959773510 ) ) ;
#45300 = CARTESIAN_POINT ( 'NONE',  ( 69.40990849430419019, 62.86359034874993057, 13.12394659649692841 ) ) ;
#45301 = ORIENTED_EDGE ( 'NONE', *, *, #48612, .F. ) ;
#45302 = CARTESIAN_POINT ( 'NONE',  ( 101.4461556848294492, 235.5024278399160949, -9.188101187500093303 ) ) ;
#45303 = DIRECTION ( 'NONE',  ( 0.000000000000000000, 0.000000000000000000, 1.000000000000000000 ) ) ;
#45304 = CARTESIAN_POINT ( 'NONE',  ( 190.0601721553029222, 300.2863949309033842, 3.228815124723532382 ) ) ;
#45305 = CARTESIAN_POINT ( 'NONE',  ( 81.20826322331814140, 42.31471022520455705, -7.450868512929636367 ) ) ;
#45306 = VERTEX_POINT ( 'NONE', #4866 ) ;
#45307 = VERTEX_POINT ( 'NONE', #28141 ) ;
#45308 = ORIENTED_EDGE ( 'NONE', *, *, #93638, .T. ) ;
#45309 = CARTESIAN_POINT ( 'NONE',  ( 80.64008363966095772, 47.31418076955320373, 12.92985048805446802 ) ) ;
#45310 = ORIENTED_EDGE ( 'NONE', *, *, #12922, .T. ) ;
#45311 = CARTESIAN_POINT ( 'NONE',  ( 69.72532707139153274, 70.32948975208321940, 4.014237884418147218 ) ) ;
#45312 = VECTOR ( 'NONE', #68168, 1000.000000000000114 ) ;
#45313 = ORIENTED_EDGE ( 'NONE', *, *, #59808, .T. ) ;
#45314 = CARTESIAN_POINT ( 'NONE',  ( 207.5230514910949182, 271.2065264061283756, 2.678931747975364708 ) ) ;
#45315 = CARTESIAN_POINT ( 'NONE',  ( -22.42236680055709641, 157.8615022471902591, 0.000000000000000000 ) ) ;
#45316 = CARTESIAN_POINT ( 'NONE',  ( 168.4414336168281636, 281.4392610354049680, 11.65181175857584428 ) ) ;
#45317 = CARTESIAN_POINT ( 'NONE',  ( -23.50969410143729377, 99.78871212707066718, 45.19948159324908943 ) ) ;
#45318 = CARTESIAN_POINT ( 'NONE',  ( 67.66304282922978075, 68.28595519557160287, -6.094803320878922293 ) ) ;
#45319 = ORIENTED_EDGE ( 'NONE', *, *, #18143, .T. ) ;
#45320 = CARTESIAN_POINT ( 'NONE',  ( 194.3589246629463787, 272.8122030992582836, -15.48160684239839568 ) ) ;
#45321 = CARTESIAN_POINT ( 'NONE',  ( 12.86511499041763074, 19.37878583063839244, 9.188101187500006262 ) ) ;
#45322 = EDGE_CURVE ( 'NONE', #84457, #34967, #52503, .T. ) ;
#45323 = CARTESIAN_POINT ( 'NONE',  ( 198.4820782953651133, 277.0876319724349628, -15.27341537592363707 ) ) ;
#45324 = CARTESIAN_POINT ( 'NONE',  ( 80.42870892512175374, 57.78063267130220027, 16.59889063300756007 ) ) ;
#45326 = ORIENTED_EDGE ( 'NONE', *, *, #68501, .F. ) ;
#45325 = CARTESIAN_POINT ( 'NONE',  ( 182.4004271739244700, 284.1903799708203451, 16.39187655311515002 ) ) ;
#45327 = CARTESIAN_POINT ( 'NONE',  ( 163.4216610345155800, 247.5923753613567442, 10.58669027323842826 ) ) ;
#45328 = EDGE_CURVE ( 'NONE', #94086, #22165, #52792, .T. ) ;
#45329 = CARTESIAN_POINT ( 'NONE',  ( 185.0221735844220063, 258.3581008124040181, 2.953144405170906595 ) ) ;
#45330 = CARTESIAN_POINT ( 'NONE',  ( 79.76359975193354046, 44.98417069036879923, 11.54310746654911846 ) ) ;
#45331 = CARTESIAN_POINT ( 'NONE',  ( 60.86586985908987657, 190.3595308348468791, 0.000000000000000000 ) ) ;
#45332 = CARTESIAN_POINT ( 'NONE',  ( 171.4141472835499940, 255.5714509828059136, 11.16434605878179021 ) ) ;
#45333 = CARTESIAN_POINT ( 'NONE',  ( 193.1345686763260971, 263.1208943439388577, -0.7594564661863862920 ) ) ;
#45334 = ORIENTED_EDGE ( 'NONE', *, *, #10382, .F. ) ;
#45336 = DIRECTION ( 'NONE',  ( 3.755686162884237478E-16, -5.590926415426495573E-32, -1.000000000000000000 ) ) ;
#45335 = B_SPLINE_CURVE_WITH_KNOTS ( 'NONE', 3,
 ( #21725, #53121, #93152, #69322, #60698, #85056, #22222, #54100, #68810, #38408, #84567, #99739, #92659, #47022, #22729, #45012, #91657, #100243, #91159, #52609, #69814, #31804, #99238, #15604, #84077, #46503, #6534, #14630, #424, #45996, #8037, #38910, #8528, #45510, #77440, #37409, #76914, #83567 ),
 .UNSPECIFIED., .F., .F.,
 ( 4, 2, 2, 2, 2, 2, 2, 2, 2, 2, 2, 2, 2, 2, 2, 2, 2, 2, 4 ),
 ( 0.0009380411731141725462, 0.001032228557793670462, 0.001126415942473168270, 0.001314790711832097315, 0.001691540250549881247, 0.002445039327985399670, 0.003952037482856488558, 0.004705536560292067697, 0.005082286099009856832, 0.005270660868368789130, 0.005364848253048254412, 0.005459035637727720561, 0.005506129330067452768, 0.005553223022407186710, 0.005647410407086621634, 0.005835785176445533115, 0.006212534715163351741, 0.006589284253881176438, 0.006966033792599000268 ),
 .UNSPECIFIED. ) ;
#45337 = CARTESIAN_POINT ( 'NONE',  ( 71.58048890525513741, 63.26397358144141236, -13.65483747980514728 ) ) ;
#45339 = EDGE_CURVE ( 'NONE', #35809, #30665, #50918, .T. ) ;
#45338 = DIRECTION ( 'NONE',  ( -0.8660254037844387076, -0.4999999999999998890, -0.000000000000000000 ) ) ;
#45340 = CARTESIAN_POINT ( 'NONE',  ( 9.025180670817464446, 166.0177522451418213, 5.000000000000051514 ) ) ;
#45341 = CARTESIAN_POINT ( 'NONE',  ( 192.9924223820390239, 267.3565088504736877, -11.03506825955556536 ) ) ;
#45342 = CARTESIAN_POINT ( 'NONE',  ( 171.2938825197189487, 279.7153930126568184, -14.88499062438163101 ) ) ;
#45343 = CARTESIAN_POINT ( 'NONE',  ( 204.1768090745211452, 277.0023882860760409, -15.56867155119955015 ) ) ;
#45344 = CARTESIAN_POINT ( 'NONE',  ( 72.10371214944608198, 72.33074704757831341, 0.8698369498405258415 ) ) ;
#45345 = CARTESIAN_POINT ( 'NONE',  ( 72.47401207315012073, 70.81051498135123268, 7.656770371261347741 ) ) ;
#45347 = CARTESIAN_POINT ( 'NONE',  ( 33.52502306405203569, 19.75978393459167037, -1.583844403245396437 ) ) ;
#45346 = CARTESIAN_POINT ( 'NONE',  ( -4.614459115189767147, 158.9548013555409796, -4.594050593750042211 ) ) ;
#45348 = CARTESIAN_POINT ( 'NONE',  ( 185.2439061181696331, 295.2756445577334716, 8.340933124425840006 ) ) ;
#45349 = ORIENTED_EDGE ( 'NONE', *, *, #85701, .T. ) ;
#45350 = EDGE_LOOP ( 'NONE', ( #49864, #16884, #95577, #47286 ) ) ;
#45351 = CARTESIAN_POINT ( 'NONE',  ( 22.45462004596304695, 37.14601545153948337, 177.5919119679930134 ) ) ;
#45352 = CARTESIAN_POINT ( 'NONE',  ( 128.1703819823903245, 233.2592609112379876, 2.679491924311254714 ) ) ;
#45353 = EDGE_CURVE ( 'NONE', #76711, #70599, #86319, .T. ) ;
#45354 = DIRECTION ( 'NONE',  ( 0.000000000000000000, -0.000000000000000000, 1.000000000000000000 ) ) ;
#45355 = LINE ( 'NONE', #53450, #37217 ) ;
#45356 = CARTESIAN_POINT ( 'NONE',  ( 202.0712002603176813, 280.6494097331414537, -16.02287548436454045 ) ) ;
#45357 = CARTESIAN_POINT ( 'NONE',  ( 81.04334714743738743, 43.68570708857655660, -9.496964033599468280 ) ) ;
#45358 = CARTESIAN_POINT ( 'NONE',  ( 150.1592538715819671, 276.5420469420121208, 3.659585770713507547 ) ) ;
#45359 = CARTESIAN_POINT ( 'NONE',  ( 13.11156449881669595, 184.5024278399160949, -9.188101187500093303 ) ) ;
#45360 = CARTESIAN_POINT ( 'NONE',  ( 124.3418758452630613, 242.5958772461660544, -9.188101187500095079 ) ) ;
#45361 = CARTESIAN_POINT ( 'NONE',  ( 182.0298379502229693, 294.6333645221262714, -6.494620609296796410 ) ) ;
#45362 = CARTESIAN_POINT ( 'NONE',  ( 65.85576469104950093, 68.94656342641907543, 2.408941155072679585 ) ) ;
#45363 = CARTESIAN_POINT ( 'NONE',  ( 87.33294734268930881, 44.88192199842172414, 6.808005391826766228 ) ) ;
#45364 = CARTESIAN_POINT ( 'NONE',  ( 84.14312167556933275, 48.98415679381830756, 0.000000000000000000 ) ) ;
#45365 = CARTESIAN_POINT ( 'NONE',  ( 81.10163913880589348, 53.21425096942738264, -15.47470560983101073 ) ) ;
#45366 = CARTESIAN_POINT ( 'NONE',  ( 194.1011995340913074, 294.4538559273262877, 13.93949783759920713 ) ) ;
#45367 = CARTESIAN_POINT ( 'NONE',  ( 184.1072741032023146, 274.9104562530689009, 16.37390854714151800 ) ) ;
#45368 = CARTESIAN_POINT ( 'NONE',  ( 81.94022493854585321, 45.96546865081016620, 11.96996177621078949 ) ) ;
#45369 = EDGE_CURVE ( 'NONE', #91593, #51615, #31224, .T. ) ;
#45370 = EDGE_CURVE ( 'NONE', #1813, #65113, #75757, .T. ) ;
#45371 = CARTESIAN_POINT ( 'NONE',  ( 170.2786588980588363, 279.2388764142214086, 13.93236286921391631 ) ) ;
#45372 = CARTESIAN_POINT ( 'NONE',  ( 187.2183957178467608, 298.8926474041342658, -0.5935065169117408335 ) ) ;
#45373 = CARTESIAN_POINT ( 'NONE',  ( 191.4852287632733123, 298.9848502134979071, -9.870565261052552941 ) ) ;
#45374 = CARTESIAN_POINT ( 'NONE',  ( 184.4900473518464139, 268.6311471613904587, -15.53052497869454207 ) ) ;
#45375 = ORIENTED_EDGE ( 'NONE', *, *, #14490, .F. ) ;
#45376 = DIRECTION ( 'NONE',  ( 0.4174706225611763410, 0.9086904199442095154, 0.000000000000000000 ) ) ;
#45377 = CIRCLE ( 'NONE', #24342, 70.00000000000001421 ) ;
#45378 = EDGE_CURVE ( 'NONE', #39135, #19773, #52429, .T. ) ;
#45379 = CARTESIAN_POINT ( 'NONE',  ( 185.0590661537433164, 269.5214566935702010, 15.89575827224772731 ) ) ;
#45380 = CARTESIAN_POINT ( 'NONE',  ( 92.19068272976576850, 224.0333772461660544, 9.188101187500095079 ) ) ;
#45381 = CARTESIAN_POINT ( 'NONE',  ( 10.59179830548347745, 18.06628583063839599, -9.188101187500006262 ) ) ;
#45382 = CARTESIAN_POINT ( 'NONE',  ( 160.4237162281696953, 273.2376347127639633, -15.66572034412998882 ) ) ;
#45383 = EDGE_CURVE ( 'NONE', #62639, #15755, #74549, .T. ) ;
#45384 = CARTESIAN_POINT ( 'NONE',  ( 176.0127109592394277, 252.6004560315867593, -4.768680066900455650 ) ) ;
#45386 = CARTESIAN_POINT ( 'NONE',  ( 152.1253780900047161, 267.1581113579235307, 17.01065375775331745 ) ) ;
#45385 = CARTESIAN_POINT ( 'NONE',  ( 9.089523648746947515, 28.18080186712591484, 3.090169943749475401 ) ) ;
#45387 = CARTESIAN_POINT ( 'NONE',  ( 152.6547697591180111, 278.7515079535921814, -4.825746761778547445 ) ) ;
#45388 = DIRECTION ( 'NONE',  ( 0.8660254037844391517, 0.4999999999999990008, 0.000000000000000000 ) ) ;
#45389 = CARTESIAN_POINT ( 'NONE',  ( 149.2923684163597784, 272.0650280510108701, -12.99082738998495756 ) ) ;
#45390 = CARTESIAN_POINT ( 'NONE',  ( 43.88624854525928498, 27.19860640527296169, 2.839279412974134775 ) ) ;
#45391 = CARTESIAN_POINT ( 'NONE',  ( 125.0004159942834860, 249.6427522451419065, -10.00000000000009592 ) ) ;
#45392 = FACE_OUTER_BOUND ( 'NONE', #25098, .T. ) ;
#45393 = ORIENTED_EDGE ( 'NONE', *, *, #84255, .F. ) ;
#45394 = CARTESIAN_POINT ( 'NONE',  ( 24.26418115112394247, 34.98502408145593279, -5.678558825948271327 ) ) ;
#45395 = CARTESIAN_POINT ( 'NONE',  ( 177.8324374767559846, 280.3398814767268732, 16.75142732283180180 ) ) ;
#45396 = CARTESIAN_POINT ( 'NONE',  ( 146.8312060062178830, 276.3278863910550172, -4.807241325481028227 ) ) ;
#45397 = CARTESIAN_POINT ( 'NONE',  ( 197.0226655822963551, 289.3937282992477549, -17.28982543158101493 ) ) ;
#45398 = EDGE_CURVE ( 'NONE', #23843, #76681, #7837, .T. ) ;
#45399 = EDGE_CURVE ( 'NONE', #37942, #61117, #230, .T. ) ;
#45400 = ORIENTED_EDGE ( 'NONE', *, *, #48604, .T. ) ;
#45401 = CARTESIAN_POINT ( 'NONE',  ( 70.69745823082493530, 60.91555314307392877, 15.03376646005350459 ) ) ;
#45402 = CARTESIAN_POINT ( 'NONE',  ( 76.02744352951765450, 65.34233732453844823, -14.42760839744433632 ) ) ;
#45403 = CARTESIAN_POINT ( 'NONE',  ( 181.1554500484497794, 263.5640902285028915, -12.87665043090944650 ) ) ;
#45404 = CARTESIAN_POINT ( 'NONE',  ( 173.2694288764014345, 253.7023385635754380, -9.145525555831373055 ) ) ;
#45405 = CARTESIAN_POINT ( 'NONE',  ( 192.0645969571214096, 297.9813550654635605, 11.46542907566974812 ) ) ;
#45406 = ORIENTED_EDGE ( 'NONE', *, *, #2847, .T. ) ;
#45407 = CARTESIAN_POINT ( 'NONE',  ( 187.2093787057832515, 278.7783034237749007, 17.22333937481381483 ) ) ;
#45408 = ORIENTED_EDGE ( 'NONE', *, *, #20368, .T. ) ;
#45409 = CARTESIAN_POINT ( 'NONE',  ( 172.0728039219370658, 285.9831811572526021, 11.38650458882361427 ) ) ;
#45410 = CARTESIAN_POINT ( 'NONE',  ( 184.6894110187365641, 293.7322318964822330, -10.88359728165448814 ) ) ;
#45411 = VERTEX_POINT ( 'NONE', #38205 ) ;
#45412 = CARTESIAN_POINT ( 'NONE',  ( 86.30977306730703447, 47.58285218899635538, -10.62438056216879900 ) ) ;
#45413 = CARTESIAN_POINT ( 'NONE',  ( -13.76211276271269668, 162.8615022471902591, 0.000000000000000000 ) ) ;
#45414 = CARTESIAN_POINT ( 'NONE',  ( 190.4975935673924141, 278.7163863375838559, -16.50822108151892920 ) ) ;
#45415 = CARTESIAN_POINT ( 'NONE',  ( 192.4990000879081720, 297.2289467719743357, -12.72483680792790750 ) ) ;
#45416 = CARTESIAN_POINT ( 'NONE',  ( 153.0927037754837556, 265.4826541232073964, -16.15085267704102634 ) ) ;
#45417 = CARTESIAN_POINT ( 'NONE',  ( 35.53452623260358934, 35.91421378149921395, 9.188101187500008038 ) ) ;
#45418 = CARTESIAN_POINT ( 'NONE',  ( 190.0398248856338057, 298.8169614316505545, -8.166243001185458539 ) ) ;
#45419 = CARTESIAN_POINT ( 'NONE',  ( 70.24301845481265616, 63.89562358154542210, -13.37649194025576094 ) ) ;
#45420 = VERTEX_POINT ( 'NONE', #100050 ) ;
#45421 = CARTESIAN_POINT ( 'NONE',  ( 195.1948488736749709, 291.0624176751974233, 16.30441594086294543 ) ) ;
#45422 = EDGE_LOOP ( 'NONE', ( #72188, #14808, #65359, #17021 ) ) ;
#45423 = VERTEX_POINT ( 'NONE', #69623 ) ;
#45424 = DIRECTION ( 'NONE',  ( 0.000000000000000000, 0.000000000000000000, 1.000000000000000000 ) ) ;
#45425 = CARTESIAN_POINT ( 'NONE',  ( 170.5373622343556690, 269.7751423367952270, 17.81562764448176850 ) ) ;
#45426 =( BOUNDED_CURVE ( )  B_SPLINE_CURVE ( 2, ( #81633, #15040, #66882, #75007, #38340, #90742, #97320, #74009, #66391 ),
 .UNSPECIFIED., .F., .T. ) 
 B_SPLINE_CURVE_WITH_KNOTS ( ( 3, 2, 2, 2, 3 ),
 ( 0.8024193548387096309, 0.8037634408602150060, 0.8064516129032257563, 0.8091397849462365066, 0.8104838709677418818 ),
 .UNSPECIFIED. ) 
 CURVE ( )  GEOMETRIC_REPRESENTATION_ITEM ( )  RATIONAL_B_SPLINE_CURVE ( ( 0.9330127018922194093, 0.9330127018922194093, 1.000000000000000000, 0.8660254037844387076, 1.000000000000000000, 0.8660254037844387076, 1.000000000000000000, 0.9330127018922194093, 0.9330127018922194093 ) ) 
 REPRESENTATION_ITEM ( '' )  );
#45428 = CARTESIAN_POINT ( 'NONE',  ( 164.8817931653405253, 246.2093970608671327, 2.959562278375574618 ) ) ;
#45427 = CARTESIAN_POINT ( 'NONE',  ( 204.7610021263893429, 275.9905362388115577, 13.36619428527026976 ) ) ;
#45429 = CARTESIAN_POINT ( 'NONE',  ( 206.6961830126489303, 272.6387046219738295, -10.22526498917591375 ) ) ;
#45430 = CARTESIAN_POINT ( 'NONE',  ( 197.4562109845989255, 273.0769534991460432, -13.28701267068813152 ) ) ;
#45431 = CARTESIAN_POINT ( 'NONE',  ( 203.5137996566828633, 276.3711131836337813, 14.38221294039407994 ) ) ;
#45432 = CARTESIAN_POINT ( 'NONE',  ( 82.32629218823147710, 40.36489395171674488, 1.301855596286184635 ) ) ;
#45433 = CARTESIAN_POINT ( 'NONE',  ( 170.9667952754920748, 287.9054735324309604, -4.302708445872753806 ) ) ;
#45434 = CARTESIAN_POINT ( 'NONE',  ( 76.96225540874074511, 63.35506444885830035, -15.47139205492574554 ) ) ;
#45435 = CARTESIAN_POINT ( 'NONE',  ( 183.4135640167273209, 284.6506825199782043, -15.02283699949769158 ) ) ;
#45436 = CARTESIAN_POINT ( 'NONE',  ( 108.2389556718223673, 242.4869531367911009, 4.594050593750046652 ) ) ;
#45437 = VERTEX_POINT ( 'NONE', #37716 ) ;
#45438 = DIRECTION ( 'NONE',  ( 0.000000000000000000, 0.000000000000000000, -1.000000000000000000 ) ) ;
#45439 = CARTESIAN_POINT ( 'NONE',  ( 44.10936046141049616, 26.26216523072498887, -2.296566073217252530E-15 ) ) ;
#45440 = CARTESIAN_POINT ( 'NONE',  ( -19.02615211706134701, 34.39283837976707048, 59.99999999999999289 ) ) ;
#45441 = VERTEX_POINT ( 'NONE', #30637 ) ;
#45442 = ADVANCED_FACE ( 'NONE', ( #5841 ), #99547, .T. ) ;
#45443 = ORIENTED_EDGE ( 'NONE', *, *, #23730, .F. ) ;
#45444 = CARTESIAN_POINT ( 'NONE',  ( 74.11971290936233459, 68.38772044953262252, -11.66991619212280895 ) ) ;
#45445 = ADVANCED_FACE ( 'NONE', ( #61522 ), #14919, .T. ) ;
#45446 = CARTESIAN_POINT ( 'NONE',  ( 180.6820162318767871, 294.0274809239796809, -2.627441245078403931 ) ) ;
#45447 = CARTESIAN_POINT ( 'NONE',  ( 157.4177733328310467, 257.9914139036126812, 18.29188238796808363 ) ) ;
#45448 = CARTESIAN_POINT ( 'NONE',  ( 159.8597520197352537, 253.7617827468940277, -16.74905990210778839 ) ) ;
#45449 = LINE ( 'NONE', #61145, #33410 ) ;
#45450 = VERTEX_POINT ( 'NONE', #67634 ) ;
#45451 = CARTESIAN_POINT ( 'NONE',  ( 194.8100188241370176, 293.2261449035823375, 15.40535685002683586 ) ) ;
#45452 = VECTOR ( 'NONE', #77248, 1000.000000000000114 ) ;
#45453 = EDGE_LOOP ( 'NONE', ( #67664, #79244, #41177, #92320 ) ) ;
#45454 = CARTESIAN_POINT ( 'NONE',  ( 198.0699909391895233, 265.2131322728000669, -4.382015913889547143 ) ) ;
#45455 = EDGE_LOOP ( 'NONE', ( #93434, #59483 ) ) ;
#45457 = EDGE_CURVE ( 'NONE', #6076, #15004, #18924, .T. ) ;
#45456 = CARTESIAN_POINT ( 'NONE',  ( 188.6181737819976263, 265.0236329270882152, -12.14609691747098630 ) ) ;
#45458 = CARTESIAN_POINT ( 'NONE',  ( 191.8060291873681535, 298.4292075798759925, -10.98119608837455630 ) ) ;
#45459 = CARTESIAN_POINT ( 'NONE',  ( 158.3585752585947262, 263.3710999200782226, 17.79390465796247156 ) ) ;
#45460 = FACE_OUTER_BOUND ( 'NONE', #74955, .T. ) ;
#45462 = CARTESIAN_POINT ( 'NONE',  ( 159.5496032553882628, 280.9406269996898686, 5.636233419987954463 ) ) ;
#45461 = CARTESIAN_POINT ( 'NONE',  ( 184.3420480696962045, 288.6290895812416011, -13.42755799798725569 ) ) ;
#45463 = CARTESIAN_POINT ( 'NONE',  ( 153.2283961777204695, 265.2476279883323400, -17.66880461074566000 ) ) ;
#45464 = VERTEX_POINT ( 'NONE', #10344 ) ;
#45465 = CARTESIAN_POINT ( 'NONE',  ( 156.6812872898450735, 261.2670451491295012, 0.000000000000000000 ) ) ;
#45466 = CARTESIAN_POINT ( 'NONE',  ( 72.70312890837641362, 66.64619018610765977, 11.87070177491906442 ) ) ;
#45467 = CARTESIAN_POINT ( 'NONE',  ( 82.41110115525400204, 41.31668765478222838, -3.372589341468242186 ) ) ;
#45468 = CARTESIAN_POINT ( 'NONE',  ( 171.0478277236890676, 250.0784670999508421, -0.2578715090061357018 ) ) ;
#45470 = ADVANCED_FACE ( 'NONE', ( #78244 ), #85377, .T. ) ;
#45469 = CARTESIAN_POINT ( 'NONE',  ( 192.5993683522255537, 271.7468063364418072, -14.60450809009411621 ) ) ;
#45471 = CARTESIAN_POINT ( 'NONE',  ( 71.65180518398884146, 72.09936778357817388, 3.358463432740969257 ) ) ;
#45472 = EDGE_CURVE ( 'NONE', #90523, #93301, #21782, .T. ) ;
#45473 = CARTESIAN_POINT ( 'NONE',  ( 84.46573575848765358, 45.41160421943110492, 9.290855630086788608 ) ) ;
#45474 = CARTESIAN_POINT ( 'NONE',  ( 190.8679683466651227, 268.2575022531604532, 14.00021181731352016 ) ) ;
#45475 = CARTESIAN_POINT ( 'NONE',  ( 191.2323848354392055, 283.4409172823887388, -16.58526465056708687 ) ) ;
#45476 = CARTESIAN_POINT ( 'NONE',  ( 82.73042059842214258, 53.63367031839453603, -15.74978661431507909 ) ) ;
#45477 = CARTESIAN_POINT ( 'NONE',  ( 72.38035161819672680, 212.5958772461660544, -9.188101187500095079 ) ) ;
#45478 = LINE ( 'NONE', #53087, #78348 ) ;
#45479 = CARTESIAN_POINT ( 'NONE',  ( 192.9523350703175311, 296.4437475495926719, -13.35611922184540923 ) ) ;
#45480 = CARTESIAN_POINT ( 'NONE',  ( -6.281727404287059890, 25.63055774385195917, -10.00000000000000000 ) ) ;
#45481 = CARTESIAN_POINT ( 'NONE',  ( 196.9477862557387766, 288.8927537360994506, -16.71206681448230924 ) ) ;
#45482 = CARTESIAN_POINT ( 'NONE',  ( 161.0965315767822972, 251.6196177163260188, -13.76772246540905442 ) ) ;
#45483 = CARTESIAN_POINT ( 'NONE',  ( 162.5093986457823974, 284.9610020461826139, 2.827745808343583356 ) ) ;
#45485 = CARTESIAN_POINT ( 'NONE',  ( -20.89819060993944078, 95.07936095790239506, 45.19943155085691444 ) ) ;
#45484 = CARTESIAN_POINT ( 'NONE',  ( 73.64702576733991179, 69.30673894177056127, -9.977882152455165965 ) ) ;
#45486 = CARTESIAN_POINT ( 'NONE',  ( 2.403541337051680493, 23.16126292948892740, -6.180339887498951690 ) ) ;
#45487 = CARTESIAN_POINT ( 'NONE',  ( 45.86230232835321630, 26.28848085856235173, 1.475505719884397138E-15 ) ) ;
#45488 = CARTESIAN_POINT ( 'NONE',  ( -22.42236680055709641, 157.8615022471902591, 0.000000000000000000 ) ) ;
#45489 = DIRECTION ( 'NONE',  ( 0.4999999999999995004, 0.8660254037844389297, 0.000000000000000000 ) ) ;
#45490 = DIRECTION ( 'NONE',  ( 0.4635919272833914917, -0.8029647720336136052, 0.3746065934159158450 ) ) ;
#45491 = EDGE_CURVE ( 'NONE', #4092, #79192, #90362, .T. ) ;
#45492 = CARTESIAN_POINT ( 'NONE',  ( 34.68144358152915174, 181.6423013555409796, -4.594050593750043987 ) ) ;
#45493 = CARTESIAN_POINT ( 'NONE',  ( 43.61180991440864574, 205.1744531367911293, 4.594050593750047540 ) ) ;
#45494 = CARTESIAN_POINT ( 'NONE',  ( 157.6286460899086137, 257.6261715744221306, 18.25526781158026779 ) ) ;
#45495 = CARTESIAN_POINT ( 'NONE',  ( 28.46864935082048831, 149.7156766241961350, -21.50000000000001421 ) ) ;
#45496 = ADVANCED_FACE ( 'NONE', ( #39694 ), #4470, .F. ) ;
#45497 = CARTESIAN_POINT ( 'NONE',  ( 81.76532694727032435, 50.08884948260267578, -14.15377366074380738 ) ) ;
#45498 = CARTESIAN_POINT ( 'NONE',  ( -5.101858724868275630, 157.8615022471902023, 5.000000000000051514 ) ) ;
#45499 = CARTESIAN_POINT ( 'NONE',  ( 47.69862761034023180, 198.3458772461660544, 9.188101187500095079 ) ) ;
#45500 = CARTESIAN_POINT ( 'NONE',  ( 20.98410315089673261, 24.06628583063841376, -9.188101187500006262 ) ) ;
#45501 = CARTESIAN_POINT ( 'NONE',  ( 151.3124059063077311, 268.5662204852269497, -14.45542936000225609 ) ) ;
#45502 = CARTESIAN_POINT ( 'NONE',  ( 196.6800254274587019, 289.9871984561398222, -17.90749311895638129 ) ) ;
#45503 = CARTESIAN_POINT ( 'NONE',  ( 13.34262526062736676, 23.10171378149917842, 9.188101187500008038 ) ) ;
#45504 = CARTESIAN_POINT ( 'NONE',  ( 66.52392041426838887, 68.84470833973988135, -4.415679280545959706 ) ) ;
#45505 = CARTESIAN_POINT ( 'NONE',  ( 158.8666211102878947, 255.9103432951560535, -16.04241150037398711 ) ) ;
#45506 = DIRECTION ( 'NONE',  ( -0.5000000000000001110, 0.8660254037844384856, 2.775557561562890427E-17 ) ) ;
#45507 = EDGE_CURVE ( 'NONE', #27844, #39666, #78419, .T. ) ;
#45508 = CARTESIAN_POINT ( 'NONE',  ( 176.2472916049610205, 274.9672641557643828, 17.27598799561485876 ) ) ;
#45509 = CYLINDRICAL_SURFACE ( 'NONE', #57077, 17.82106496071139645 ) ;
#45510 = CARTESIAN_POINT ( 'NONE',  ( 153.2981356959497816, 276.9127835245838014, 7.993427546634691794 ) ) ;
#45511 = CIRCLE ( 'NONE', #6703, 70.00000000000001421 ) ;
#45512 = CARTESIAN_POINT ( 'NONE',  ( 153.7869224421094714, 276.6684750246370754, 9.963584371085772773 ) ) ;
#45513 = CARTESIAN_POINT ( 'NONE',  ( 105.7493929595398470, 231.8615022471902591, -10.00000000000009592 ) ) ;
#45514 = CARTESIAN_POINT ( 'NONE',  ( 161.7101619467568980, 250.5567787384628389, 13.05644392949610655 ) ) ;
#45515 = CARTESIAN_POINT ( 'NONE',  ( 164.8188621457609031, 269.4130389654807800, -16.30850380620819351 ) ) ;
#45516 = ORIENTED_EDGE ( 'NONE', *, *, #17750, .T. ) ;
#45517 = CARTESIAN_POINT ( 'NONE',  ( 77.66033283744638993, 49.34596622033864577, 15.30541677020318936 ) ) ;
#45518 = ORIENTED_EDGE ( 'NONE', *, *, #51118, .T. ) ;
#45519 = CARTESIAN_POINT ( 'NONE',  ( 165.6809110264175615, 265.1086644751799213, 16.57607991724843899 ) ) ;
#45520 = CARTESIAN_POINT ( 'NONE',  ( 187.8107902964165135, 277.2180192601347812, -16.66606730953470716 ) ) ;
#45521 = CARTESIAN_POINT ( 'NONE',  ( -50.31241255605538498, 43.89631431014924345, 59.99999999999999289 ) ) ;
#45522 = VERTEX_POINT ( 'NONE', #66028 ) ;
#45523 = DIRECTION ( 'NONE',  ( -2.816764622163176013E-16, -1.626259812849728177E-16, 1.000000000000000000 ) ) ;
#45524 = CARTESIAN_POINT ( 'NONE',  ( 79.29599111977559289, 45.69620181558697425, -12.92830799085840177 ) ) ;
#45525 = CARTESIAN_POINT ( 'NONE',  ( 194.5298665426430489, 293.7113828889860656, -16.13302716640051315 ) ) ;
#45526 = CARTESIAN_POINT ( 'NONE',  ( 177.2790252787945349, 274.8473450460222125, -17.02799535311900669 ) ) ;
#45527 = ORIENTED_EDGE ( 'NONE', *, *, #52370, .T. ) ;
#45528 = CARTESIAN_POINT ( 'NONE',  ( 19.79331822069313418, 23.37878583063840665, 9.188101187500006262 ) ) ;
#45529 = CARTESIAN_POINT ( 'NONE',  ( 75.32210451894222558, 56.33950100161004571, 16.14035722671651030 ) ) ;
#45530 = CARTESIAN_POINT ( 'NONE',  ( 68.38740636103155168, 69.72993023537252100, -3.234909568346066244 ) ) ;
#45531 = DIRECTION ( 'NONE',  ( -0.8614378286617615510, 0.5078630399532039208, 0.000000000000000000 ) ) ;
#45532 = VERTEX_POINT ( 'NONE', #41718 ) ;
#45533 = CARTESIAN_POINT ( 'NONE',  ( 171.7154418923348942, 259.3365693118849435, -15.26938553599716641 ) ) ;
#45534 = CARTESIAN_POINT ( 'NONE',  ( 159.2651917302844993, 254.7915913763855258, -16.53922207549818424 ) ) ;
#45535 = EDGE_LOOP ( 'NONE', ( #21548, #17190 ) ) ;
#45536 = EDGE_LOOP ( 'NONE', ( #68075, #45516, #5325, #69336 ) ) ;
#45537 = CARTESIAN_POINT ( 'NONE',  ( 174.7605424730916468, 286.1926619560792346, 10.62116624121103037 ) ) ;
#45539 = CARTESIAN_POINT ( 'NONE',  ( 67.68417759276564993, 65.75923827970558477, -10.63272006068741682 ) ) ;
#45538 = CARTESIAN_POINT ( 'NONE',  ( 159.5064483110165554, 282.2686952242540315, -3.232496309074801122 ) ) ;
#45540 = CARTESIAN_POINT ( 'NONE',  ( 162.9111474110223412, 248.4766108952035211, -9.702990628959184960 ) ) ;
#45541 = CARTESIAN_POINT ( 'NONE',  ( 163.7136804588959649, 247.0865828815331042, 6.783386239354816105 ) ) ;
#45542 = CARTESIAN_POINT ( 'NONE',  ( 198.4772197948566372, 286.8743665007300478, 18.43646439804394532 ) ) ;
#45543 = CARTESIAN_POINT ( 'NONE',  ( 164.6134528626768088, 265.2130342782942307, -16.63617519986410187 ) ) ;
#45545 = ADVANCED_FACE ( 'NONE', ( #3747 ), #81764, .T. ) ;
#45544 = B_SPLINE_CURVE_WITH_KNOTS ( 'NONE', 3,
 ( #70793, #95649, #57075, #889 ),
 .UNSPECIFIED., .F., .F.,
 ( 4, 4 ),
 ( 0.01095786972172493184, 0.01671678501755174268 ),
 .UNSPECIFIED. ) ;
#45546 = CARTESIAN_POINT ( 'NONE',  ( 129.3218690127885964, 233.2202760586659736, -5.415160957724236172E-17 ) ) ;
#45547 = CARTESIAN_POINT ( 'NONE',  ( 177.3894926443979614, 269.1231757516105176, 16.10179540431882472 ) ) ;
#45548 = CARTESIAN_POINT ( 'NONE',  ( 179.7076816803278234, 257.8881168337280201, 10.24022085344165411 ) ) ;
#45549 = CARTESIAN_POINT ( 'NONE',  ( 65.61435460324827318, 214.8149278399160664, 9.188101187500093303 ) ) ;
#45550 = ORIENTED_EDGE ( 'NONE', *, *, #20471, .T. ) ;
#45551 = CARTESIAN_POINT ( 'NONE',  ( 170.2874585057777210, 263.9538622975835551, 15.97034119630043314 ) ) ;
#45552 = CARTESIAN_POINT ( 'NONE',  ( -13.11024591527723615, 4.999999999999999112, -48.00000000000017053 ) ) ;
#45553 = PLANE ( 'NONE',  #43113 ) ;
#45554 = VERTEX_POINT ( 'NONE', #28018 ) ;
#45555 = CARTESIAN_POINT ( 'NONE',  ( 200.3804403721752578, 281.5778917628034606, 17.30444700233937994 ) ) ;
#45556 = B_SPLINE_CURVE_WITH_KNOTS ( 'NONE', 3,
 ( #70119, #53429, #29647, #45814 ),
 .UNSPECIFIED., .F., .F.,
 ( 4, 4 ),
 ( 0.008276874795924938841, 0.01457606355628901854 ),
 .UNSPECIFIED. ) ;
#45557 = VERTEX_POINT ( 'NONE', #57922 ) ;
#45558 = B_SPLINE_CURVE_WITH_KNOTS ( 'NONE', 3,
 ( #83114, #13684, #44557, #83616, #75492, #6077, #36970, #91210, #97152, #98631, #34794, #28704, #50012, #51499, #44388, #90044, #98119, #42877, #97633, #28198, #66213, #59074, #20617, #82468, #35804, #57595, #27718, #4925, #58586, #88576, #96651 ),
 .UNSPECIFIED., .F., .F.,
 ( 4, 3, 3, 3, 3, 3, 3, 3, 3, 3, 4 ),
 ( 0.000000000000000000, 0.1333490885032479201, 0.3007194338854572990, 0.4699862290245473417, 0.5844252810809665855, 0.6686540514502945509, 0.7354980260655585855, 0.8028463152565719074, 0.8633854507757248165, 0.9437142632667163689, 1.000000000000000000 ),
 .UNSPECIFIED. ) ;
#45559 = FACE_BOUND ( 'NONE', #3362, .T. ) ;
#45560 = CARTESIAN_POINT ( 'NONE',  ( 66.56339537322608635, 67.82455691954585575, 6.899508657999463779 ) ) ;
#45561 = CARTESIAN_POINT ( 'NONE',  ( 6.396987757676594555, 15.64441083166260427, 0.000000000000000000 ) ) ;
#45563 = B_SPLINE_SURFACE_WITH_KNOTS ( 'NONE', 3, 1, ( 
 ( #40450, #62242 ),
 ( #79513, #31847 ),
 ( #9586, #32860 ),
 ( #94205, #71385 ),
 ( #62750, #92702 ),
 ( #85622, #93706 ),
 ( #47064, #77978 ),
 ( #47556, #69364 ),
 ( #48574, #9071 ),
 ( #10075, #1973 ),
 ( #56144, #15649 ),
 ( #78483, #39937 ),
 ( #25261, #24269 ),
 ( #16662, #46548 ),
 ( #8574, #55639 ),
 ( #87143, #39439 ),
 ( #70358, #85102 ),
 ( #77483, #970 ),
 ( #8079, #17674 ),
 ( #55146, #86132 ),
 ( #100283, #1482 ),
 ( #23749, #48057 ),
 ( #63767, #30869 ),
 ( #32365, #93196 ),
 ( #63264, #61752 ),
 ( #38952, #24760 ),
 ( #94699, #54645 ),
 ( #54140, #86625 ),
 ( #470, #31359 ),
 ( #69857, #17159 ),
 ( #16166, #79000 ),
 ( #12073, #33892 ),
 ( #51045, #3489 ),
 ( #81505, #4459 ) ),
 .UNSPECIFIED., .T., .F., .F.,
 ( 4, 2, 2, 2, 2, 2, 2, 2, 2, 2, 2, 2, 2, 2, 2, 2, 4 ),
 ( 2, 2 ),
 ( 0.000000000000000000, 0.06250000000000000000, 0.1250000000000000000, 0.1875000000000000000, 0.2500000000000000000, 0.3125000000000000000, 0.3750000000000000000, 0.4375000000000000000, 0.5000000000000000000, 0.5625000000000000000, 0.6250000000000000000, 0.6875000000000000000, 0.7500000000000000000, 0.8125000000000000000, 0.8750000000000000000, 0.9375000000000000000, 1.000000000000000000 ),
 ( 0.000000000000000000, 1.000000000000000000 ),
 .UNSPECIFIED. ) ;
#45562 = CARTESIAN_POINT ( 'NONE',  ( 84.93732889701342970, 42.42729486305053399, -4.181145052139376261 ) ) ;
#45564 = CARTESIAN_POINT ( 'NONE',  ( 67.87358026886720097, 65.44943466354128248, 10.32536289689572584 ) ) ;
#45565 = CARTESIAN_POINT ( 'NONE',  ( 155.5888570658010508, 261.1591898008976500, 17.34682632352454945 ) ) ;
#45566 = FACE_OUTER_BOUND ( 'NONE', #81394, .T. ) ;
#45567 = CARTESIAN_POINT ( 'NONE',  ( 87.34055741008818075, 44.89555582937400402, 6.825810004488442218 ) ) ;
#45568 = ORIENTED_EDGE ( 'NONE', *, *, #27888, .T. ) ;
#45569 = CARTESIAN_POINT ( 'NONE',  ( 162.0157470128914952, 250.0274898778833688, -13.78877802034368649 ) ) ;
#45570 = ORIENTED_EDGE ( 'NONE', *, *, #75666, .F. ) ;
#45571 = CARTESIAN_POINT ( 'NONE',  ( 76.24518087481982320, 51.59313173972786615, -15.67787985409661111 ) ) ;
#45572 = EDGE_CURVE ( 'NONE', #10579, #47882, #2420, .T. ) ;
#45573 = DIRECTION ( 'NONE',  ( 0.7467472232290895962, 0.000000000000000000, -0.6651079495838584377 ) ) ;
#45574 = CARTESIAN_POINT ( 'NONE',  ( 196.2421909983451940, 290.7455499326673021, -17.31908925000307065 ) ) ;
#45575 = CARTESIAN_POINT ( 'NONE',  ( 195.1551897557243933, 279.2352859451050904, 16.33844644333552054 ) ) ;
#45576 = CARTESIAN_POINT ( 'NONE',  ( 162.2853105227554238, 261.2444871014557748, 16.87942141898201953 ) ) ;
#45577 = CARTESIAN_POINT ( 'NONE',  ( 142.8531688511554307, 253.2833772461660544, -9.188101187500095079 ) ) ;
#45578 = VERTEX_POINT ( 'NONE', #20437 ) ;
#45579 = DIRECTION ( 'NONE',  ( -0.1384676192453732635, 0.9903669614948382716, 0.000000000000000000 ) ) ;
#45580 = CARTESIAN_POINT ( 'NONE',  ( 183.1915443601783977, 257.6986921343423091, 6.833778512193781296 ) ) ;
#45581 = LINE ( 'NONE', #84152, #12512 ) ;
#45583 = EDGE_CURVE ( 'NONE', #93683, #27723, #51305, .T. ) ;
#45582 = CARTESIAN_POINT ( 'NONE',  ( 153.3506059258413643, 265.0359544954067132, -16.39100908615009899 ) ) ;
#45584 = CARTESIAN_POINT ( 'NONE',  ( 72.94747830045673709, 70.90780099059745112, 7.943658523256118542 ) ) ;
#45585 = EDGE_CURVE ( 'NONE', #826, #52395, #81735, .T. ) ;
#45586 = DIRECTION ( 'NONE',  ( -0.9919422576440838357, -0.1266907948509199411, 0.000000000000000000 ) ) ;
#45587 = ORIENTED_EDGE ( 'NONE', *, *, #61883, .F. ) ;
#45588 = CARTESIAN_POINT ( 'NONE',  ( 199.7626786811085822, 266.7967628138173950, 4.643313006584093294 ) ) ;
#45589 = CARTESIAN_POINT ( 'NONE',  ( 200.1133476818314705, 272.1141633677412415, 12.87458617912082914 ) ) ;
#45590 = CARTESIAN_POINT ( 'NONE',  ( 82.44914618329345046, 40.96452554122298295, 1.009388433876072355 ) ) ;
#45591 = CARTESIAN_POINT ( 'NONE',  ( 184.8342610281462726, 263.5722196047579473, -12.52600749362046528 ) ) ;
#45592 = CARTESIAN_POINT ( 'NONE',  ( 198.7518522379862418, 265.8040289700034577, 1.598954627491116165 ) ) ;
#45593 = ORIENTED_EDGE ( 'NONE', *, *, #3991, .T. ) ;
#45594 = CARTESIAN_POINT ( 'NONE',  ( 190.6218339396177441, 300.4802939150614520, -4.178005820806754755 ) ) ;
#45595 = CARTESIAN_POINT ( 'NONE',  ( 71.08151174896164548, 71.70762546245575209, 0.6123320000693289744 ) ) ;
#45596 = FACE_OUTER_BOUND ( 'NONE', #77541, .T. ) ;
#45598 = CARTESIAN_POINT ( 'NONE',  ( 192.8037126019380594, 268.3597080544300297, 12.45183830779196299 ) ) ;
#45597 = CARTESIAN_POINT ( 'NONE',  ( 155.6126298223767890, 261.1180141786725244, 18.15400560664037855 ) ) ;
#45599 = CARTESIAN_POINT ( 'NONE',  ( 28.21526782163968861, 21.45404122711134320, -8.090169943749478065 ) ) ;
#45600 = CARTESIAN_POINT ( 'NONE',  ( -11.40312891409031693, 78.77562236714182120, 59.99999999999999289 ) ) ;
#45601 = CARTESIAN_POINT ( 'NONE',  ( 163.1996623812120504, 283.9505196342968816, -3.834948744398505305 ) ) ;
#45602 = DIRECTION ( 'NONE',  ( -0.5104483989331241034, -0.8599083858334038988, 0.000000000000000000 ) ) ;
#45603 = PLANE ( 'NONE',  #65669 ) ;
#45604 = EDGE_CURVE ( 'NONE', #81025, #87907, #3258, .T. ) ;
#45605 = CARTESIAN_POINT ( 'NONE',  ( -13.03140383004354241, 163.2833772461660544, -9.188101187500095079 ) ) ;
#45606 = DIRECTION ( 'NONE',  ( 0.000000000000000000, 0.000000000000000000, -1.000000000000000000 ) ) ;
#45607 = ORIENTED_EDGE ( 'NONE', *, *, #57359, .F. ) ;
#45608 = CARTESIAN_POINT ( 'NONE',  ( 66.51752898485065657, 67.96052159512244373, -6.582747979517454162 ) ) ;
#45609 = CARTESIAN_POINT ( 'NONE',  ( 73.09646855998906290, 70.52920676086053220, -7.962158031461710195 ) ) ;
#45610 = CARTESIAN_POINT ( 'NONE',  ( 202.6716764631725027, 274.3364404589790411, -12.86965901471974227 ) ) ;
#45611 = CARTESIAN_POINT ( 'NONE',  ( 81.83412826008793672, 41.20383488999954835, 5.740616493571673473 ) ) ;
#45612 = CARTESIAN_POINT ( 'NONE',  ( 14.19444334931225349, 172.8768266524160140, 9.188101187500096856 ) ) ;
#45613 = VECTOR ( 'NONE', #6558, 1000.000000000000227 ) ;
#45614 = CARTESIAN_POINT ( 'NONE',  ( 178.7130411427290539, 273.8027002318069094, -16.86336393568773673 ) ) ;
#45615 = CARTESIAN_POINT ( 'NONE',  ( 27.45223038363779722, 27.80066082961423035, 10.00000000000000533 ) ) ;
#45616 = CARTESIAN_POINT ( 'NONE',  ( 82.70173759442589301, 41.68243550408067222, -4.153490145786375543 ) ) ;
#45617 = CARTESIAN_POINT ( 'NONE',  ( 170.5589339941222136, 270.9438782765666929, -16.77442372788140901 ) ) ;
#45618 = CARTESIAN_POINT ( 'NONE',  ( 133.3665344050969566, 236.2592609112379876, 2.679491924311254714 ) ) ;
#45619 = EDGE_CURVE ( 'NONE', #85223, #84967, #81273, .T. ) ;
#45620 = CARTESIAN_POINT ( 'NONE',  ( 175.5454376425959424, 253.5828794482383159, -3.844180409976710511 ) ) ;
#45621 = CARTESIAN_POINT ( 'NONE',  ( 191.3040952703574078, 261.0541660929657723, -1.520933822623211640 ) ) ;
#45622 = CARTESIAN_POINT ( 'NONE',  ( 55.08690683815022027, 192.6115022471902023, -5.000000000000041744 ) ) ;
#45623 = CARTESIAN_POINT ( 'NONE',  ( 81.87359138893998534, 41.32955797152818889, 5.976920566253458134 ) ) ;
#45624 = CARTESIAN_POINT ( 'NONE',  ( 190.4744901378711290, 300.7355008658671522, 0.04566709859947504224 ) ) ;
#45625 = CARTESIAN_POINT ( 'NONE',  ( 16.17015057563676450, 170.9548013555409796, -4.594050593750042211 ) ) ;
#45626 = CARTESIAN_POINT ( 'NONE',  ( 165.0391502558331069, 249.6778246878102436, -10.74756611015070717 ) ) ;
#45627 =( NAMED_UNIT ( * ) PLANE_ANGLE_UNIT ( ) SI_UNIT ( $, .RADIAN. ) );
#45628 = CARTESIAN_POINT ( 'NONE',  ( 36.89851624356406745, 36.70171378149922248, -9.188101187500004485 ) ) ;
#45629 = CARTESIAN_POINT ( 'NONE',  ( 48.98810889288134263, 89.24608170897542436, -10.00000000000000000 ) ) ;
#45630 = CARTESIAN_POINT ( 'NONE',  ( 206.9026071836525205, 272.2811674698855313, 7.240992997279449561 ) ) ;
#45631 = CARTESIAN_POINT ( 'NONE',  ( 185.2935054837330711, 266.5941941465212039, 14.38430047949690049 ) ) ;
#45632 = CARTESIAN_POINT ( 'NONE',  ( 47.28113444070024229, 72.57591296950349147, 177.5919119679930134 ) ) ;
#45633 = CARTESIAN_POINT ( 'NONE',  ( 179.7701192287809135, 262.8885550775633533, -12.91845977881626339 ) ) ;
#45634 = APPLICATION_PROTOCOL_DEFINITION ( 'draft international standard', 'automotive_design', 1998, #61525 ) ;
#45635 = CARTESIAN_POINT ( 'NONE',  ( 21.67811977205257890, 27.91421378149918553, 9.188101187500008038 ) ) ;
#45636 = CARTESIAN_POINT ( 'NONE',  ( 148.3519871123208986, 273.6938162480936398, 8.180046468253793890 ) ) ;
#45637 = CARTESIAN_POINT ( 'NONE',  ( 71.44576612263118420, 59.19700591949954571, 15.77431131436991407 ) ) ;
#45638 = CARTESIAN_POINT ( 'NONE',  ( 155.4186054393023255, 261.4540742680644598, 17.05753227160644769 ) ) ;
#45639 = VERTEX_POINT ( 'NONE', #38599 ) ;
#45640 = CARTESIAN_POINT ( 'NONE',  ( -22.42236680055709641, 157.8615022471902591, 0.000000000000000000 ) ) ;
#45641 = PLANE ( 'NONE',  #98764 ) ;
#45642 = CARTESIAN_POINT ( 'NONE',  ( 75.22004289090682505, 53.63718660003009120, -16.53846879587417718 ) ) ;
#45643 = CARTESIAN_POINT ( 'NONE',  ( 84.99999999999998579, 14.99999999999999467, -59.99999999999999289 ) ) ;
#45644 = CARTESIAN_POINT ( 'NONE',  ( 81.45834803924864786, 41.98143484532695169, 7.684766122967380930 ) ) ;
#45645 = EDGE_LOOP ( 'NONE', ( #100121, #80115, #49688, #65227 ) ) ;
#45646 = CARTESIAN_POINT ( 'NONE',  ( 196.1556763520775064, 289.0687990662340212, -17.19517613012386548 ) ) ;
#45647 = CARTESIAN_POINT ( 'NONE',  ( 70.18022655624727690, 70.95232338804223104, -2.456227850087851827 ) ) ;
#45648 = CARTESIAN_POINT ( 'NONE',  ( 76.86365259909378267, 63.86390198653350581, 14.89973402578624473 ) ) ;
#45649 = CARTESIAN_POINT ( 'NONE',  ( 203.4696564630250464, 278.2272125378923988, -16.38980782817167636 ) ) ;
#45650 = EDGE_CURVE ( 'NONE', #41317, #17810, #58694, .T. ) ;
#45651 = EDGE_LOOP ( 'NONE', ( #72135, #43080, #35322, #91208 ) ) ;
#45652 = ORIENTED_EDGE ( 'NONE', *, *, #67929, .T. ) ;
#45654 = CARTESIAN_POINT ( 'NONE',  ( 50.12332653952445582, 98.65487733484057742, 10.00000000000000000 ) ) ;
#45653 = CARTESIAN_POINT ( 'NONE',  ( 50.23025173566474422, 97.10399052176643409, 177.5919119679930134 ) ) ;
#45655 = ORIENTED_EDGE ( 'NONE', *, *, #11433, .T. ) ;
#45656 = CARTESIAN_POINT ( 'NONE',  ( 191.5451565139252068, 298.8810523045859213, 7.782291334092181323 ) ) ;
#45657 = DIRECTION ( 'NONE',  ( -0.8660254037844378194, -0.5000000000000014433, -0.000000000000000000 ) ) ;
#45658 = CARTESIAN_POINT ( 'NONE',  ( 79.86744359784395897, 58.00471593829997374, 16.26723200184080653 ) ) ;
#45659 = CARTESIAN_POINT ( 'NONE',  ( 70.69733468835805468, 69.84023709405138902, -7.592114496330573559 ) ) ;
#45661 = EDGE_LOOP ( 'NONE', ( #25365, #83982, #12378, #11691 ) ) ;
#45660 = EDGE_CURVE ( 'NONE', #7803, #45437, #53786, .T. ) ;
#45662 = CARTESIAN_POINT ( 'NONE',  ( 190.3144310910409445, 301.0127312671879167, -1.334877248546042949 ) ) ;
#45663 = CARTESIAN_POINT ( 'NONE',  ( 149.3141802193904368, 272.0272488999566463, -11.40332369054239336 ) ) ;
#45664 = ORIENTED_EDGE ( 'NONE', *, *, #39458, .T. ) ;
#45665 = CARTESIAN_POINT ( 'NONE',  ( 195.7291850945597957, 291.6341022226063160, 17.08310330964873813 ) ) ;
#45666 = CARTESIAN_POINT ( 'NONE',  ( 158.1219681159314518, 265.1686937430463331, 17.54345935383751964 ) ) ;
#45667 = ORIENTED_EDGE ( 'NONE', *, *, #81431, .F. ) ;
#45668 = CARTESIAN_POINT ( 'NONE',  ( 190.7705347155322499, 300.2227366160529414, 3.504769718465625239 ) ) ;
#45669 = FACE_OUTER_BOUND ( 'NONE', #80020, .T. ) ;
#45670 = EDGE_LOOP ( 'NONE', ( #96956, #37059, #94324, #28380 ) ) ;
#45671 = CARTESIAN_POINT ( 'NONE',  ( 174.8213806158123589, 292.3284732554488414, -0.08473646757267205842 ) ) ;
#45672 = FACE_OUTER_BOUND ( 'NONE', #45094, .T. ) ;
#45673 = CARTESIAN_POINT ( 'NONE',  ( 78.60735446187601383, 47.91558663937575346, -14.46554739992949834 ) ) ;
#45674 = CARTESIAN_POINT ( 'NONE',  ( 30.72385922946222792, 41.23654200823205684, 1.583844403245363353 ) ) ;
#45675 = ORIENTED_EDGE ( 'NONE', *, *, #10593, .T. ) ;
#45676 = VERTEX_POINT ( 'NONE', #90872 ) ;
#45677 = CARTESIAN_POINT ( 'NONE',  ( 72.91150544132388234, 59.06535682740706505, -15.54152198706926313 ) ) ;
#45678 = CARTESIAN_POINT ( 'NONE',  ( 146.8358616138309571, 276.3198226421291679, 4.054088818585255716 ) ) ;
#45679 = CARTESIAN_POINT ( 'NONE',  ( 148.2267527339363369, 273.9107285543102535, 7.913369084260907016 ) ) ;
#45680 = CARTESIAN_POINT ( 'NONE',  ( 149.2561433752359505, 272.1277716627430436, 12.99353668144589946 ) ) ;
#45681 = LINE ( 'NONE', #53778, #82533 ) ;
#45682 = CARTESIAN_POINT ( 'NONE',  ( 147.2930760453491246, 275.5279040167861240, 0.1825760380121495829 ) ) ;
#45683 = CARTESIAN_POINT ( 'NONE',  ( 191.4852287632733123, 298.9848502134979071, -9.870565261052552941 ) ) ;
#45684 = CARTESIAN_POINT ( 'NONE',  ( 149.0761751337341821, 272.4394858007734683, 11.56094486755886130 ) ) ;
#45685 = CARTESIAN_POINT ( 'NONE',  ( 70.69181040969623098, 69.05249515714282893, 7.974372502152151654 ) ) ;
#45686 = AXIS2_PLACEMENT_3D ( 'NONE', #54716, #48650, #93780 ) ;
#45687 = CARTESIAN_POINT ( 'NONE',  ( 86.69683407628214411, 230.8615022471903160, 5.000000000000046185 ) ) ;
#45688 = CARTESIAN_POINT ( 'NONE',  ( 66.97592682939898623, 66.94584532911248687, 8.711456034417569327 ) ) ;
#45689 = CARTESIAN_POINT ( 'NONE',  ( 168.7836086128107524, 286.6128497672082176, 4.077482129993557081 ) ) ;
#45690 = CARTESIAN_POINT ( 'NONE',  ( 78.18706620576766397, 47.52751489781214644, 14.39385552048683437 ) ) ;
#45691 = VERTEX_POINT ( 'NONE', #37107 ) ;
#45692 = CARTESIAN_POINT ( 'NONE',  ( 149.7654984860464253, 271.2455427317246404, -12.38634015387427034 ) ) ;
#45693 = CARTESIAN_POINT ( 'NONE',  ( 71.39380143430086889, 68.16157986366320642, 9.700154972268515863 ) ) ;
#45694 = LINE ( 'NONE', #67017, #46306 ) ;
#45695 = AXIS2_PLACEMENT_3D ( 'NONE', #68826, #30337, #67336 ) ;
#45696 = CARTESIAN_POINT ( 'NONE',  ( 79.12912844008201319, 45.88903201271446619, 13.12629439217962357 ) ) ;
#45697 = EDGE_CURVE ( 'NONE', #80286, #84464, #98936, .T. ) ;
#45698 = B_SPLINE_CURVE_WITH_KNOTS ( 'NONE', 3,
 ( #24987, #10809, #58380, #4186 ),
 .UNSPECIFIED., .F., .F.,
 ( 4, 4 ),
 ( 0.005865586104323563567, 0.01086301216498964349 ),
 .UNSPECIFIED. ) ;
#45699 = CARTESIAN_POINT ( 'NONE',  ( 12.00096474099108690, 32.03863464977599307, 10.00000000000000000 ) ) ;
#45700 = EDGE_CURVE ( 'NONE', #33613, #51377, #44202, .T. ) ;
#45701 = CARTESIAN_POINT ( 'NONE',  ( -17.42236680055705023, 149.2012482093457777, 0.000000000000000000 ) ) ;
#45702 = CARTESIAN_POINT ( 'NONE',  ( 165.5469076125238814, 284.0653433844562983, -8.492543197847592040 ) ) ;
#45703 = VERTEX_POINT ( 'NONE', #51830 ) ;
#45704 = CARTESIAN_POINT ( 'NONE',  ( 163.4222916751007801, 247.5912830598222172, -10.52132777929285012 ) ) ;
#45705 = ADVANCED_FACE ( 'NONE', ( #84747 ), #45203, .F. ) ;
#45706 = CARTESIAN_POINT ( 'NONE',  ( 72.58623256761462983, 71.41713459486039994, 5.736086548208264801 ) ) ;
#45707 = ADVANCED_FACE ( 'NONE', ( #21908 ), #89457, .T. ) ;
#45708 = CARTESIAN_POINT ( 'NONE',  ( 44.46005344233068257, 203.1427522451418781, -10.00000000000009415 ) ) ;
#45709 = CARTESIAN_POINT ( 'NONE',  ( 120.4447615282330588, 240.3458772461660544, 9.188101187500095079 ) ) ;
#45710 = CARTESIAN_POINT ( 'NONE',  ( 198.9832789858017463, 285.9978462703757600, -18.55676541969546278 ) ) ;
#45711 = AXIS2_PLACEMENT_3D ( 'NONE', #46502, #8527, #7510 ) ;
#45712 = CARTESIAN_POINT ( 'NONE',  ( 162.2336410148055279, 251.8862672885301492, -14.09881826716025799 ) ) ;
#45713 = CARTESIAN_POINT ( 'NONE',  ( 157.7365441389748923, 257.4392866714015895, 18.13124212464487073 ) ) ;
#45714 = CARTESIAN_POINT ( 'NONE',  ( 175.4373900952620886, 253.5400337193396467, -3.935082475582811323 ) ) ;
#45715 = CARTESIAN_POINT ( 'NONE',  ( 31.83936385565518279, 195.3149278399160664, 9.188101187500093303 ) ) ;
#45716 = CARTESIAN_POINT ( 'NONE',  ( 82.16888635695728738, 40.69672472932156637, 3.699334420833011450 ) ) ;
#45717 = EDGE_LOOP ( 'NONE', ( #46931, #26372, #29404 ) ) ;
#45718 = CARTESIAN_POINT ( 'NONE',  ( 199.3868061948075194, 268.7461186553251764, -9.827356238820643242 ) ) ;
#45719 = CARTESIAN_POINT ( 'NONE',  ( 74.35485255615375877, 67.94178241879927782, -11.69148233987723806 ) ) ;
#45720 =( BOUNDED_CURVE ( )  B_SPLINE_CURVE ( 2, ( #48855, #78254, #8834, #39703, #33139, #71159, #70633, #1244, #32126 ),
 .UNSPECIFIED., .F., .T. ) 
 B_SPLINE_CURVE_WITH_KNOTS ( ( 3, 2, 2, 2, 3 ),
 ( 0.7620967741935483764, 0.7634408602150537515, 0.7661290322580645018, 0.7688172043010752521, 0.7701612903225806273 ),
 .UNSPECIFIED. ) 
 CURVE ( )  GEOMETRIC_REPRESENTATION_ITEM ( )  RATIONAL_B_SPLINE_CURVE ( ( 0.9330127018922194093, 0.9330127018922194093, 1.000000000000000000, 0.8660254037844387076, 1.000000000000000000, 0.8660254037844387076, 1.000000000000000000, 0.9330127018922194093, 0.9330127018922194093 ) ) 
 REPRESENTATION_ITEM ( '' )  );
#45721 = PLANE ( 'NONE',  #38437 ) ;
#45722 = CARTESIAN_POINT ( 'NONE',  ( 190.3625087333586521, 300.9294583479858147, -4.271886578030237303 ) ) ;
#45723 = CARTESIAN_POINT ( 'NONE',  ( 81.68123830234790717, 41.59537758512663430, -5.490745364427081832 ) ) ;
#45724 = CARTESIAN_POINT ( 'NONE',  ( 181.2440676231241241, 294.5520841294345473, -6.623935519155441654 ) ) ;
#45725 = CARTESIAN_POINT ( 'NONE',  ( 164.1488579720687255, 250.0635283098263244, 10.33718753367986132 ) ) ;
#45726 = EDGE_CURVE ( 'NONE', #97002, #17498, #117, .T. ) ;
#45727 = CARTESIAN_POINT ( 'NONE',  ( 110.3501529135968013, 224.5177522451418213, 5.000000000000051514 ) ) ;
#45728 = CARTESIAN_POINT ( 'NONE',  ( 175.6063544791335573, 254.0105997054014040, 8.344378697908656051 ) ) ;
#45729 = ORIENTED_EDGE ( 'NONE', *, *, #92641, .F. ) ;
#45730 = CARTESIAN_POINT ( 'NONE',  ( 202.7865629936218284, 279.4103651332174536, 17.10878160033216133 ) ) ;
#45731 = CARTESIAN_POINT ( 'NONE',  ( 81.71726183135250210, 47.25007601922910538, -13.05188860062295042 ) ) ;
#45732 = CARTESIAN_POINT ( 'NONE',  ( 18.65997361151702449, 172.3923013555409796, 4.594050593750050204 ) ) ;
#45733 = CARTESIAN_POINT ( 'NONE',  ( 13.76346889243896321, 13.11029122506292843, -8.090169943749478065 ) ) ;
#45734 = CARTESIAN_POINT ( 'NONE',  ( -14.34210371876190315, 105.3327122335069816, 43.90660993338509144 ) ) ;
#45735 = CARTESIAN_POINT ( 'NONE',  ( 71.75673953893199553, 59.57128976058874059, -15.71773281170402825 ) ) ;
#45736 = B_SPLINE_CURVE_WITH_KNOTS ( 'NONE', 3,
 ( #92263, #22812, #53692, #15191, #69899, #62798, #39985, #19111, #93242, #54184, #70922, #88545, #57572, #39481, #15696, #31895, #93754, #80434, #94248, #23297, #24314, #8121, #30908, #78527 ),
 .UNSPECIFIED., .F., .F.,
 ( 4, 2, 2, 2, 2, 2, 2, 2, 2, 2, 2, 4 ),
 ( 0.006994835961790266815, 0.007754851833055070344, 0.008134859768687469073, 0.008514867704319870403, 0.009274883575584667861, 0.009654891511217062253, 0.01003489944684945491, 0.01079491531811423849, 0.01155493118937902207, 0.01193493912501142687, 0.01231494706064382993, 0.01307496293190867249 ),
 .UNSPECIFIED. ) ;
#45737 = DIRECTION ( 'NONE',  ( -0.7957378174433876739, 0.6056412518070690698, 0.000000000000000000 ) ) ;
#45739 = CARTESIAN_POINT ( 'NONE',  ( 75.81765026128996965, 205.3923013555409796, 4.594050593750050204 ) ) ;
#45738 = CARTESIAN_POINT ( 'NONE',  ( 195.0059191867570405, 275.0380839613920330, -16.17140022037657943 ) ) ;
#45740 = CARTESIAN_POINT ( 'NONE',  ( 161.5875797534026219, 250.7690973254556468, 12.95526170413129030 ) ) ;
#45741 = CARTESIAN_POINT ( 'NONE',  ( 72.55719605514633486, 57.27873603870379782, 15.85570519528398137 ) ) ;
#45742 = CARTESIAN_POINT ( 'NONE',  ( 46.26427303354824261, 207.5177522451419065, 5.000000000000046185 ) ) ;
#45743 = CARTESIAN_POINT ( 'NONE',  ( 207.5338226493333025, 271.1878702128032614, 6.432541580693135863 ) ) ;
#45744 = VERTEX_POINT ( 'NONE', #54800 ) ;
#45745 = CARTESIAN_POINT ( 'NONE',  ( 14.88889434582250537, 172.7365022471902023, -10.00000000000009059 ) ) ;
#45746 = CARTESIAN_POINT ( 'NONE',  ( 164.4414259850711915, 245.8260906552167171, -6.983224448873608381 ) ) ;
#45747 = CARTESIAN_POINT ( 'NONE',  ( 139.2268610206906203, 245.0643266524160140, 9.188101187500095079 ) ) ;
#45748 = CARTESIAN_POINT ( 'NONE',  ( 36.41017387241338810, 23.94754757982092030, 5.678558825948272215 ) ) ;
#45749 = CARTESIAN_POINT ( 'NONE',  ( 164.4637126465671884, 260.7786515323086860, -16.15215151101600455 ) ) ;
#45750 = CARTESIAN_POINT ( 'NONE',  ( 192.7288556637334125, 292.1918731402626577, -15.52061534916644447 ) ) ;
#45751 = CARTESIAN_POINT ( 'NONE',  ( -27.42236680055714260, 166.5217562850347406, 1.224646799147364892E-15 ) ) ;
#45753 = DIRECTION ( 'NONE',  ( 1.804112415015878984E-15, -1.000000000000000000, 0.000000000000000000 ) ) ;
#45752 = CARTESIAN_POINT ( 'NONE',  ( 88.30945731027941292, 43.97049527616571396, 2.452112525173334223 ) ) ;
#45754 = DIRECTION ( 'NONE',  ( -0.9055221650797476984, -0.4242989612870696758, 0.000000000000000000 ) ) ;
#45755 = ORIENTED_EDGE ( 'NONE', *, *, #96175, .T. ) ;
#45756 = DIRECTION ( 'NONE',  ( -0.03304531753667278721, -0.9994538543569185807, 0.000000000000000000 ) ) ;
#45757 = SHAPE_REPRESENTATION_RELATIONSHIP ( 'NONE' , 'NONE' ,  #35972, #14997 ) ;
#45758 = EDGE_CURVE ( 'NONE', #62226, #6303, #55778, .T. ) ;
#45759 = CARTESIAN_POINT ( 'NONE',  ( 143.0969038086192597, 260.4263049900483225, -7.951529393128359935 ) ) ;
#45760 = CIRCLE ( 'NONE', #66755, 70.00000000000001421 ) ;
#45761 = CARTESIAN_POINT ( 'NONE',  ( 172.9311764467664716, 268.4779053881692334, -17.72160738022306603 ) ) ;
#45762 = CARTESIAN_POINT ( 'NONE',  ( 7.453652514893187586, 19.70171378149916919, -9.188101187500004485 ) ) ;
#45763 = ORIENTED_EDGE ( 'NONE', *, *, #2788, .F. ) ;
#45764 = CARTESIAN_POINT ( 'NONE',  ( 206.8804362336228166, 272.3195686817890078, 7.951031312702417253 ) ) ;
#45765 = DIRECTION ( 'NONE',  ( -0.8660254037844387076, -0.4999999999999998890, -0.000000000000000000 ) ) ;
#45766 = VECTOR ( 'NONE', #1173, 1000.000000000000114 ) ;
#45767 = CARTESIAN_POINT ( 'NONE',  ( 149.0092716443465406, 273.2528299346296876, -9.628675884572079013 ) ) ;
#45768 = DIRECTION ( 'NONE',  ( 4.546899780356473057E-16, -0.000000000000000000, -1.000000000000000000 ) ) ;
#45769 = CARTESIAN_POINT ( 'NONE',  ( 38.54221318313706490, 186.3927522451418213, 10.00000000000009948 ) ) ;
#45770 = CARTESIAN_POINT ( 'NONE',  ( 69.25674720781552196, 70.45917808822757422, 2.199828333335145825 ) ) ;
#45771 = CARTESIAN_POINT ( 'NONE',  ( 153.4613150239306094, 264.8442007126561748, -16.86932470306368259 ) ) ;
#45772 = CARTESIAN_POINT ( 'NONE',  ( 197.0571419530650701, 283.2438395117923733, -17.78737236506320940 ) ) ;
#45773 = DIRECTION ( 'NONE',  ( 0.000000000000000000, 0.000000000000000000, -1.000000000000000000 ) ) ;
#45774 = EDGE_LOOP ( 'NONE', ( #54386, #23066, #53891, #15311 ) ) ;
#45775 = CARTESIAN_POINT ( 'NONE',  ( 149.7119746935222793, 271.3382486597900538, 12.05352563709836922 ) ) ;
#45776 = CARTESIAN_POINT ( 'NONE',  ( 69.48172542408106267, 66.96606747815684457, 10.45582737889983882 ) ) ;
#45777 = CARTESIAN_POINT ( 'NONE',  ( 85.89091867366458644, 45.03324537760627067, -7.686407249209525894 ) ) ;
#45778 = VERTEX_POINT ( 'NONE', #16306 ) ;
#45779 = CARTESIAN_POINT ( 'NONE',  ( 146.7434471017767521, 276.4798892723637209, 0.7354350123930684102 ) ) ;
#45780 = CARTESIAN_POINT ( 'NONE',  ( 79.31084698818210654, 59.85625551150463508, -16.50595436643998681 ) ) ;
#45781 = VECTOR ( 'NONE', #42902, 1000.000000000000000 ) ;
#45782 = CARTESIAN_POINT ( 'NONE',  ( 12.72979851930235107, 19.30066082961420548, -10.00000000000000533 ) ) ;
#45783 = CARTESIAN_POINT ( 'NONE',  ( 75.13365046141905168, 53.63593841991193045, -16.54225084687872283 ) ) ;
#45784 = CARTESIAN_POINT ( 'NONE',  ( 69.88684495751175518, 62.60609260009564281, 13.43558750483837372 ) ) ;
#45785 = ORIENTED_EDGE ( 'NONE', *, *, #38722, .F. ) ;
#45786 = CARTESIAN_POINT ( 'NONE',  ( 109.5926410088830920, 224.8923013555410080, 4.594050593750050204 ) ) ;
#45787 = CARTESIAN_POINT ( 'NONE',  ( 200.2316334480823912, 283.8356329158505105, 17.02791935830326508 ) ) ;
#45788 = CARTESIAN_POINT ( 'NONE',  ( 73.22483582419529569, 69.61542381504622767, -9.909891866396675297 ) ) ;
#45789 = CARTESIAN_POINT ( 'NONE',  ( 177.9271722668541429, 269.0421873018364067, -16.58597972526078479 ) ) ;
#45790 = CARTESIAN_POINT ( 'NONE',  ( 131.2304340799682052, 258.1199935810940929, 2.679491924311251605 ) ) ;
#45791 = B_SPLINE_SURFACE_WITH_KNOTS ( 'NONE', 3, 1, ( 
 ( #72926, #81049 ),
 ( #80540, #88157 ),
 ( #66294, #87672 ),
 ( #42960, #95749 ),
 ( #58183, #73901 ),
 ( #18206, #49099 ),
 ( #18705, #3516 ),
 ( #96233, #19222 ),
 ( #11612, #42471 ),
 ( #4489, #34878 ),
 ( #65778, #89167 ),
 ( #19713, #35382 ),
 ( #27795, #58668 ),
 ( #28277, #36880 ),
 ( #91123, #83523 ),
 ( #53567, #59154 ),
 ( #98204, #15065 ),
 ( #22688, #60159 ),
 ( #68273, #74905 ),
 ( #90124, #83025 ),
 ( #76402, #21688 ),
 ( #5984, #51587 ),
 ( #59667, #7469 ),
 ( #76871, #52567 ),
 ( #5490, #61167 ),
 ( #36372, #13594 ),
 ( #67785, #99196 ),
 ( #67278, #75400 ),
 ( #14589, #82543 ),
 ( #92135, #45467 ),
 ( #44468, #45954 ) ),
 .UNSPECIFIED., .F., .F., .F.,
 ( 4, 3, 3, 3, 3, 3, 3, 3, 3, 3, 4 ),
 ( 2, 2 ),
 ( 0.000000000000000000, 0.1122669598086790121, 0.2243161639709752020, 0.3396355846219183960, 0.4553962076585234553, 0.5677860799922451740, 0.6749047109689819690, 0.7773884377078301711, 0.8775581155834233371, 0.9782364162378153205, 1.000000000000000000 ),
 ( 0.000000000000000000, 1.000000000000000000 ),
 .UNSPECIFIED. ) ;
#45792 = VERTEX_POINT ( 'NONE', #46703 ) ;
#45793 = ORIENTED_EDGE ( 'NONE', *, *, #14742, .F. ) ;
#45794 = ORIENTED_EDGE ( 'NONE', *, *, #80026, .T. ) ;
#45795 = CARTESIAN_POINT ( 'NONE',  ( 155.9200296242932495, 280.3860598674420430, -5.539708607631867565 ) ) ;
#45796 = VERTEX_POINT ( 'NONE', #78626 ) ;
#45797 = CARTESIAN_POINT ( 'NONE',  ( 68.99318464718037092, 69.46180787594425965, 5.229098606639764668 ) ) ;
#45798 = ORIENTED_EDGE ( 'NONE', *, *, #28093, .T. ) ;
#45799 = CARTESIAN_POINT ( 'NONE',  ( 164.4405316900629259, 245.8276396196081350, -6.144538123479245328 ) ) ;
#45800 = DIRECTION ( 'NONE',  ( -0.8660254037844387076, -0.4999999999999998890, -0.000000000000000000 ) ) ;
#45801 = CARTESIAN_POINT ( 'NONE',  ( 147.8819534105757043, 274.5079385007862811, -9.338341377131436971 ) ) ;
#45802 = CARTESIAN_POINT ( 'NONE',  ( 67.52224811643590385, 68.26499532685183169, -5.959467176383858700 ) ) ;
#45803 = ORIENTED_EDGE ( 'NONE', *, *, #27289, .T. ) ;
#45804 = CARTESIAN_POINT ( 'NONE',  ( 203.0722418932742244, 271.9993247240984147, -11.15264743686702431 ) ) ;
#45805 = CARTESIAN_POINT ( 'NONE',  ( 12.79778405566451482, 30.49540643055186351, 3.479690158560446702E-15 ) ) ;
#45806 = CARTESIAN_POINT ( 'NONE',  ( 198.4552072442472195, 277.1389102503209187, -15.27480873049025334 ) ) ;
#45807 = CARTESIAN_POINT ( 'NONE',  ( 80.38386138148599969, 57.79680026592915709, 16.59996232260768068 ) ) ;
#45808 = EDGE_LOOP ( 'NONE', ( #65978, #12076, #68227, #55741 ) ) ;
#45809 = CARTESIAN_POINT ( 'NONE',  ( 202.3425522658138505, 280.1794142728863903, 15.86053073629060961 ) ) ;
#45810 = CARTESIAN_POINT ( 'NONE',  ( -30.04356256989597185, 94.88921800892812541, 45.19948692389422717 ) ) ;
#45811 = FACE_OUTER_BOUND ( 'NONE', #57752, .T. ) ;
#45812 = EDGE_CURVE ( 'NONE', #68464, #82593, #78123, .T. ) ;
#45813 = CARTESIAN_POINT ( 'NONE',  ( 83.01663263273712801, 45.84489330812576213, -10.66041702595184582 ) ) ;
#45814 = CARTESIAN_POINT ( 'NONE',  ( 172.8951663193395234, 288.9549776225803157, 8.104654168245465584 ) ) ;
#45815 = EDGE_CURVE ( 'NONE', #57901, #78755, #61029, .T. ) ;
#45816 = CARTESIAN_POINT ( 'NONE',  ( 193.9979983253333842, 262.2552985615510579, -0.8131695963413709816 ) ) ;
#45817 = ORIENTED_EDGE ( 'NONE', *, *, #93824, .T. ) ;
#45818 = CARTESIAN_POINT ( 'NONE',  ( 155.7883366700203283, 260.8136809913161756, -17.92854480136704609 ) ) ;
#45819 = CARTESIAN_POINT ( 'NONE',  ( 75.07659682177998661, 67.19019193167019921, -13.02721601185334066 ) ) ;
#45820 = DIRECTION ( 'NONE',  ( -0.9606745773021556634, 0.2776767122488391082, 0.000000000000000000 ) ) ;
#45821 = EDGE_CURVE ( 'NONE', #74796, #17687, #57793, .T. ) ;
#45822 = CARTESIAN_POINT ( 'NONE',  ( 2.890834060677622830, 179.1427522451419350, -10.00000000000009415 ) ) ;
#45823 = CARTESIAN_POINT ( 'NONE',  ( 193.4895222550737799, 267.7935039460338089, -10.92382970030925904 ) ) ;
#45824 = DIRECTION ( 'NONE',  ( 0.3958915996110438096, 0.9182972510888884887, 0.000000000000000000 ) ) ;
#45825 = CARTESIAN_POINT ( 'NONE',  ( 167.5469267500292574, 266.7168544022062520, -17.80679023418265672 ) ) ;
#45826 = CARTESIAN_POINT ( 'NONE',  ( 72.05561987901629095, 72.31305038834268828, 0.7486621910535968816 ) ) ;
#45827 = CARTESIAN_POINT ( 'NONE',  ( 162.7435819479956933, 250.7668427907593411, -13.06080741167749082 ) ) ;
#45829 = CARTESIAN_POINT ( 'NONE',  ( 76.26477717271305323, 65.12336802401900115, 14.59904178568168476 ) ) ;
#45828 = CARTESIAN_POINT ( 'NONE',  ( -5.047471817081990331, 158.7048013555409796, 4.594050593750051981 ) ) ;
#45830 = DIRECTION ( 'NONE',  ( 0.4493970231495826861, -0.7783784768652872721, -0.4383711467890751834 ) ) ;
#45831 = ORIENTED_EDGE ( 'NONE', *, *, #19104, .F. ) ;
#45832 = ORIENTED_EDGE ( 'NONE', *, *, #77318, .T. ) ;
#45833 = FACE_OUTER_BOUND ( 'NONE', #19433, .T. ) ;
#45834 = CARTESIAN_POINT ( 'NONE',  ( 67.44257088943838596, 67.25355904234817217, -8.657396272410824878 ) ) ;
#45835 = CARTESIAN_POINT ( 'NONE',  ( 85.04155063335291231, 42.38172213771981234, 0.7433201199607106791 ) ) ;
#45836 = CARTESIAN_POINT ( 'NONE',  ( 202.6121680448818836, 279.7124260450182192, -17.20265281220889619 ) ) ;
#45837 = CARTESIAN_POINT ( 'NONE',  ( 84.17792904279457389, 46.08690578416687345, 10.28387621250127104 ) ) ;
#45838 = CARTESIAN_POINT ( 'NONE',  ( 152.8043993858796910, 278.1759084314348911, 3.722792219655572055 ) ) ;
#45839 = CARTESIAN_POINT ( 'NONE',  ( 18.14551070619625150, 181.2833772461660544, -9.188101187500095079 ) ) ;
#45840 = AXIS2_PLACEMENT_3D ( 'NONE', #16728, #63327, #94268 ) ;
#45841 = CARTESIAN_POINT ( 'NONE',  ( 121.5815934185826421, 234.8768266524159856, -9.188101187500091527 ) ) ;
#45842 = CARTESIAN_POINT ( 'NONE',  ( 181.4801324847757371, 293.6536699639055996, -6.265443341854637360 ) ) ;
#45843 = CARTESIAN_POINT ( 'NONE',  ( 66.26992252404669159, 69.16262777561748010, 2.541374374801295133 ) ) ;
#45844 = CARTESIAN_POINT ( 'NONE',  ( 150.0125358617781046, 271.5677179990414629, -11.81783918238916975 ) ) ;
#45845 = CIRCLE ( 'NONE', #26513, 70.00000000000001421 ) ;
#45846 = CARTESIAN_POINT ( 'NONE',  ( 177.9706801847183044, 283.7805232136731206, -15.20094465328249100 ) ) ;
#45847 = CARTESIAN_POINT ( 'NONE',  ( 190.7809735039951420, 299.8080322731761953, -4.803559423902265202 ) ) ;
#45848 = CARTESIAN_POINT ( 'NONE',  ( 157.1338510812060747, 258.4831816688264325, 17.88958125218800888 ) ) ;
#45849 = CARTESIAN_POINT ( 'NONE',  ( 68.76220232199221982, 63.85858675847342880, -12.18730015502817920 ) ) ;
#45850 = CARTESIAN_POINT ( 'NONE',  ( 207.6129110656513035, 271.0508850574501025, -5.265106572941297358 ) ) ;
#45851 = CARTESIAN_POINT ( 'NONE',  ( 190.0457908948199304, 284.8755663360458925, 17.21853735360699034 ) ) ;
#45852 = LINE ( 'NONE', #91028, #82207 ) ;
#45853 = CARTESIAN_POINT ( 'NONE',  ( 189.2525414291476693, 262.7352831944227773, 8.031418296191455752 ) ) ;
#45854 = CARTESIAN_POINT ( 'NONE',  ( 168.4817192172301930, 278.3851404970916406, 14.18369869134152950 ) ) ;
#45855 = DIRECTION ( 'NONE',  ( -0.8660254037844387076, -0.4999999999999998890, -0.000000000000000000 ) ) ;
#45856 = CARTESIAN_POINT ( 'NONE',  ( 191.2111338740054975, 299.4595964878050154, -9.718193530796334301 ) ) ;
#45857 = DIRECTION ( 'NONE',  ( -0.4999999999999998890, 0.8660254037844387076, 0.000000000000000000 ) ) ;
#45858 = VERTEX_POINT ( 'NONE', #72024 ) ;
#45859 = DIRECTION ( 'NONE',  ( -0.4340522123146846045, 0.9008877160804935613, 0.000000000000000000 ) ) ;
#45860 = CARTESIAN_POINT ( 'NONE',  ( 184.6987793500286159, 269.2149976013500918, 16.08913214107394651 ) ) ;
#45861 = CARTESIAN_POINT ( 'NONE',  ( 95.54687826519547400, 213.7202760586659167, -5.415160957724236172E-17 ) ) ;
#45862 = CARTESIAN_POINT ( 'NONE',  ( 12.32384911305235420, 19.06628583063839955, -9.188101187500006262 ) ) ;
#45863 = CARTESIAN_POINT ( 'NONE',  ( 151.4327733764141612, 268.3577379114237829, 14.90862905801242100 ) ) ;
#45864 = CARTESIAN_POINT ( 'NONE',  ( 158.5750977676651132, 259.0605719887398095, -17.09334224669940028 ) ) ;
#45866 = CARTESIAN_POINT ( 'NONE',  ( 192.0134456341967564, 277.2561770618384003, 16.56410798670358631 ) ) ;
#45865 = CARTESIAN_POINT ( 'NONE',  ( 66.03570291327434916, 68.57356300261318438, 1.927684033228001859 ) ) ;
#45867 = CARTESIAN_POINT ( 'NONE',  ( 196.6029714102277808, 290.1206599289108112, 17.93210582400232767 ) ) ;
#45868 = CARTESIAN_POINT ( 'NONE',  ( 198.5511052797322975, 286.7463930869835167, -17.24711022262289006 ) ) ;
#45869 = CARTESIAN_POINT ( 'NONE',  ( 149.7247407264208618, 272.0633196944937140, -11.44969454563192279 ) ) ;
#45870 = ADVANCED_FACE ( 'NONE', ( #34029 ), #12726, .T. ) ;
#45871 = CARTESIAN_POINT ( 'NONE',  ( 38.02916716989017942, 40.14336893147758900, 7.433330006724141015 ) ) ;
#45872 = CARTESIAN_POINT ( 'NONE',  ( 146.8312060062178830, 276.3278863910550172, -4.807241325481028227 ) ) ;
#45873 = CARTESIAN_POINT ( 'NONE',  ( 196.3956310503436953, 264.1850728776087180, 4.154333235580330630 ) ) ;
#45874 = VERTEX_POINT ( 'NONE', #50204 ) ;
#45875 = CARTESIAN_POINT ( 'NONE',  ( 27.19903172117837542, 31.10171378149920329, 9.188101187500008038 ) ) ;
#45876 = CARTESIAN_POINT ( 'NONE',  ( 178.7883952590142940, 280.5407180839665102, 15.89476656820465728 ) ) ;
#45877 = DIRECTION ( 'NONE',  ( -0.8660254037844387076, -0.4999999999999998890, -0.000000000000000000 ) ) ;
#45878 = CARTESIAN_POINT ( 'NONE',  ( 149.0164813726494799, 272.5428784278667536, -11.67305721329070423 ) ) ;
#45879 = ORIENTED_EDGE ( 'NONE', *, *, #14840, .T. ) ;
#45880 = CARTESIAN_POINT ( 'NONE',  ( 43.24043327773039636, 120.8247932685368227, -10.00000000000000000 ) ) ;
#45881 = CARTESIAN_POINT ( 'NONE',  ( 159.9671766634011192, 253.5757178060795809, 16.49140845334465411 ) ) ;
#45883 = ADVANCED_FACE ( 'NONE', ( #64916 ), #10719, .T. ) ;
#45882 = CARTESIAN_POINT ( 'NONE',  ( 178.5747556458698853, 290.2456356026511344, -10.84108072231283515 ) ) ;
#45884 = CARTESIAN_POINT ( 'NONE',  ( 188.1799812681836102, 277.7687690950278920, 17.76449826988982394 ) ) ;
#45885 = CARTESIAN_POINT ( 'NONE',  ( -17.42236680055705023, 149.2012482093457777, 0.000000000000000000 ) ) ;
#45886 = ORIENTED_EDGE ( 'NONE', *, *, #99917, .F. ) ;
#45887 = CARTESIAN_POINT ( 'NONE',  ( 188.0035612729766115, 279.2325960380115362, 17.82077010991123700 ) ) ;
#45888 = CARTESIAN_POINT ( 'NONE',  ( 33.05914333415502426, 24.80170272979928470, 7.433330006724137462 ) ) ;
#45889 = ORIENTED_EDGE ( 'NONE', *, *, #54999, .T. ) ;
#45890 = CYLINDRICAL_SURFACE ( 'NONE', #85419, 10.00000000000010658 ) ;
#45891 = EDGE_CURVE ( 'NONE', #66403, #54956, #26418, .T. ) ;
#45892 = CARTESIAN_POINT ( 'NONE',  ( 181.6041183721993946, 291.2867937091023123, -11.32870443584723930 ) ) ;
#45893 = VERTEX_POINT ( 'NONE', #72538 ) ;
#45894 = CARTESIAN_POINT ( 'NONE',  ( 86.35276101173943175, 47.57280788579409148, -10.59090733898761627 ) ) ;
#45895 = CARTESIAN_POINT ( 'NONE',  ( 159.0925993676364953, 255.0905301174903457, 16.49470061235192020 ) ) ;
#45896 = CARTESIAN_POINT ( 'NONE',  ( 84.95191157424133621, 50.11551264433204267, 13.67402201518260441 ) ) ;
#45897 = CARTESIAN_POINT ( 'NONE',  ( 193.2875054959514785, 295.8632153432003520, -12.54951740302059982 ) ) ;
#45898 = B_SPLINE_CURVE_WITH_KNOTS ( 'NONE', 3,
 ( #39743, #70672, #46875, #15457 ),
 .UNSPECIFIED., .F., .F.,
 ( 4, 4 ),
 ( 1.260064970365687123E-16, 0.005076538409987941397 ),
 .UNSPECIFIED. ) ;
#45899 = CARTESIAN_POINT ( 'NONE',  ( 153.0444155045374544, 265.5662918618958201, -16.15173036748435109 ) ) ;
#45900 = AXIS2_PLACEMENT_3D ( 'NONE', #79598, #92781, #16248 ) ;
#45901 = DIRECTION ( 'NONE',  ( -0.8099771808667466377, -0.5864613938488684175, 0.000000000000000000 ) ) ;
#45902 = CARTESIAN_POINT ( 'NONE',  ( 82.90200020812584114, 45.15967755036723474, -10.71970635951677941 ) ) ;
#45903 = FACE_OUTER_BOUND ( 'NONE', #62400, .T. ) ;
#45904 = LINE ( 'NONE', #75865, #87059 ) ;
#45905 = VERTEX_POINT ( 'NONE', #81155 ) ;
#45906 = CARTESIAN_POINT ( 'NONE',  ( 171.1295603993285965, 249.6517061031812545, 4.344809613321301889 ) ) ;
#45907 = VERTEX_POINT ( 'NONE', #18324 ) ;
#45908 = AXIS2_PLACEMENT_3D ( 'NONE', #56765, #3588, #48686 ) ;
#45909 = ORIENTED_EDGE ( 'NONE', *, *, #83109, .T. ) ;
#45910 = CARTESIAN_POINT ( 'NONE',  ( 198.0529239074794532, 286.9055631288374570, 16.94304631173295306 ) ) ;
#45911 = CARTESIAN_POINT ( 'NONE',  ( 171.5095832474949304, 270.2981375784696638, 16.50875514196534155 ) ) ;
#45913 = CARTESIAN_POINT ( 'NONE',  ( 165.5170328988546373, 275.0156723620771686, -15.58398378318264754 ) ) ;
#45912 = LINE ( 'NONE', #76361, #42265 ) ;
#45914 = CARTESIAN_POINT ( 'NONE',  ( 206.3528985702396596, 273.2332907176744925, -9.687807306503337657 ) ) ;
#45915 = CARTESIAN_POINT ( 'NONE',  ( 197.6236242130358676, 272.7773651221880300, -13.22260735042824287 ) ) ;
#45916 = AXIS2_PLACEMENT_3D ( 'NONE', #95540, #87948, #17476 ) ;
#45917 = CARTESIAN_POINT ( 'NONE',  ( 74.94965141288585642, 60.80520178593948799, -15.45531043546616878 ) ) ;
#45918 = CARTESIAN_POINT ( 'NONE',  ( 146.9700173529739970, 276.0874580858064746, -5.099093031535578469 ) ) ;
#45919 = CARTESIAN_POINT ( 'NONE',  ( 169.7010302950471612, 250.3720810868360047, -5.484198761109861486 ) ) ;
#45920 = CARTESIAN_POINT ( 'NONE',  ( 76.90757676121016573, 64.01000647765765450, -15.22607040013521029 ) ) ;
#45921 = VECTOR ( 'NONE', #62736, 1000.000000000000114 ) ;
#45922 = CARTESIAN_POINT ( 'NONE',  ( 183.4601068508181640, 284.4945872344713962, -15.13106351166021213 ) ) ;
#45923 = CARTESIAN_POINT ( 'NONE',  ( 123.8009570636627785, 230.0327760586659736, 1.948934522072303157E-15 ) ) ;
#45924 = ORIENTED_EDGE ( 'NONE', *, *, #44375, .F. ) ;
#45925 = CARTESIAN_POINT ( 'NONE',  ( 183.7739455050309232, 260.7523580455279557, -9.220920309613330090 ) ) ;
#45926 = CARTESIAN_POINT ( 'NONE',  ( 40.42517716772906056, 31.84335787977767041, 9.188101187500006262 ) ) ;
#45927 = CARTESIAN_POINT ( 'NONE',  ( 188.2554578474332914, 273.5037763784579852, 15.65903759604143985 ) ) ;
#45928 = ORIENTED_EDGE ( 'NONE', *, *, #425, .F. ) ;
#45929 = B_SPLINE_CURVE_WITH_KNOTS ( 'NONE', 3,
 ( #9592, #63772, #79520, #89141 ),
 .UNSPECIFIED., .F., .F.,
 ( 4, 4 ),
 ( 0.008366579159829847998, 0.01473107717590894927 ),
 .UNSPECIFIED. ) ;
#45930 = CARTESIAN_POINT ( 'NONE',  ( 162.8931802014337791, 249.0911889412991229, -10.32038157250286048 ) ) ;
#45931 = EDGE_CURVE ( 'NONE', #96482, #76355, #24718, .T. ) ;
#45932 = CARTESIAN_POINT ( 'NONE',  ( 70.23932605309654775, 64.16367945268753203, -12.59136813384165166 ) ) ;
#45933 = CARTESIAN_POINT ( 'NONE',  ( 180.7483976610911611, 294.0911617732556351, -2.543390022621885294 ) ) ;
#45934 = CARTESIAN_POINT ( 'NONE',  ( 206.7927593038066618, 270.4714295788825780, 5.070506503021109168 ) ) ;
#45935 = CARTESIAN_POINT ( 'NONE',  ( 30.05030659499110968, 29.30066082961423746, -10.00000000000000533 ) ) ;
#45936 = CARTESIAN_POINT ( 'NONE',  ( 46.50192534792603283, 74.36443251879779837, -10.00000000000000000 ) ) ;
#45937 = ORIENTED_EDGE ( 'NONE', *, *, #55395, .T. ) ;
#45938 = CARTESIAN_POINT ( 'NONE',  ( 148.4581628440222971, 273.5099144862561502, 10.38959067216531373 ) ) ;
#45939 = ORIENTED_EDGE ( 'NONE', *, *, #99346, .T. ) ;
#45940 = CARTESIAN_POINT ( 'NONE',  ( 56.22356517706933943, 203.2677522451418781, 10.00000000000009592 ) ) ;
#45941 = LINE ( 'NONE', #91109, #991 ) ;
#45942 = ORIENTED_EDGE ( 'NONE', *, *, #83875, .F. ) ;
#45943 = CARTESIAN_POINT ( 'NONE',  ( 191.8443339775285494, 267.7755496645525000, -12.38404032343068373 ) ) ;
#45944 = EDGE_CURVE ( 'NONE', #29881, #74122, #4101, .T. ) ;
#45945 = CARTESIAN_POINT ( 'NONE',  ( 195.5588106879092152, 265.2999770288793684, 4.407320425118734342 ) ) ;
#45946 = CARTESIAN_POINT ( 'NONE',  ( 158.2848466404973919, 263.3015549465852700, 17.37201711831807316 ) ) ;
#45947 = CARTESIAN_POINT ( 'NONE',  ( 10.75723147838630034, 177.0177522451418497, -10.00000000000009592 ) ) ;
#45949 = CARTESIAN_POINT ( 'NONE',  ( 156.8470823004346641, 280.2066661834281831, 5.893157905567727006 ) ) ;
#45948 = CARTESIAN_POINT ( 'NONE',  ( 186.0921632850933065, 290.0109707162887958, -13.31660835586359681 ) ) ;
#45950 = DIRECTION ( 'NONE',  ( -0.6833540297821713017, 0.7300871660154474307, 0.000000000000000000 ) ) ;
#45951 = VERTEX_POINT ( 'NONE', #66402 ) ;
#45952 = CARTESIAN_POINT ( 'NONE',  ( 204.7552454032017408, 272.8428230285074960, -9.594377649449842949 ) ) ;
#45953 = CARTESIAN_POINT ( 'NONE',  ( 73.45867522032249042, 68.92373273176619364, 10.23420689778941473 ) ) ;
#45954 = CARTESIAN_POINT ( 'NONE',  ( 82.41630873631589793, 41.31828431233921606, -3.367117793111293889 ) ) ;
#45955 = CARTESIAN_POINT ( 'NONE',  ( -19.65312891409030271, 93.06504152958497400, 10.00000000000000888 ) ) ;
#45956 = CARTESIAN_POINT ( 'NONE',  ( 189.6692937066967488, 270.4073510551538106, -14.09879195927397788 ) ) ;
#45957 = CARTESIAN_POINT ( 'NONE',  ( 176.0535401773562683, 259.9697838701345631, -14.17309044617966407 ) ) ;
#45958 = DIRECTION ( 'NONE',  ( -0.000000000000000000, -0.000000000000000000, -1.000000000000000000 ) ) ;
#45959 = CARTESIAN_POINT ( 'NONE',  ( 169.3928097498865668, 252.4249310383071645, 11.01504250006889229 ) ) ;
#45960 = CARTESIAN_POINT ( 'NONE',  ( 194.5047661587782386, 293.7548580291293092, 14.86680123054176583 ) ) ;
#45961 = CARTESIAN_POINT ( 'NONE',  ( 191.3906598757142490, 282.8513481914541217, -16.97112179597618820 ) ) ;
#45962 = CARTESIAN_POINT ( 'NONE',  ( 73.75605216947923282, 65.80208602379973115, -13.43874901075588824 ) ) ;
#45963 = CARTESIAN_POINT ( 'NONE',  ( 77.03558525930309031, 203.0327760586659451, 1.948934522072303157E-15 ) ) ;
#45964 = CARTESIAN_POINT ( 'NONE',  ( 206.2041691044954348, 273.4908977089264113, -9.455375957961031474 ) ) ;
#45965 = CARTESIAN_POINT ( 'NONE',  ( 147.2089949622447875, 275.6735367246781720, -3.633014386235353221 ) ) ;
#45966 = DIRECTION ( 'NONE',  ( -0.5000000000000003331, 0.8660254037844383745, -9.251858538542982674E-17 ) ) ;
#45967 = CARTESIAN_POINT ( 'NONE',  ( 66.54075137518580618, 68.81555626029071959, -2.231460399992863497 ) ) ;
#45968 = B_SPLINE_CURVE_WITH_KNOTS ( 'NONE', 3,
 ( #80349, #40777, #33720, #42283, #88978, #10918, #95566, #57484, #34209, #9919, #4291, #3329, #19028, #72225, #41792, #87972, #2831, #96052, #50393, #26112, #64610, #34693, #11919, #65101, #95049, #25611, #35191, #2321, #49901, #56498, #80859, #71728, #18020, #3812, #49402, #11431, #73218, #42775, #65594, #33201, #64102, #27114, #19533, #72738, #56988, #73709, #94537, #48913, #25090, #55971 ),
 .UNSPECIFIED., .F., .F.,
 ( 4, 2, 2, 2, 2, 2, 2, 2, 2, 2, 2, 2, 2, 2, 2, 2, 2, 2, 2, 2, 2, 2, 2, 2, 4 ),
 ( 0.001408021394296337303, 0.001871204839914372654, 0.002334388285532408222, 0.002565980008341460158, 0.002681775869745926712, 0.002797571731150393700, 0.002913367592554860688, 0.003029163453959327242, 0.003260755176768255145, 0.003723938622386087534, 0.004187122068003919055, 0.005113488959239669701, 0.006039855850475420347, 0.006503039296093259675, 0.006966222741711099002, 0.007082018603115559051, 0.007139916533817849791, 0.007197814464520141398, 0.007313610325924579762, 0.007429406187329018127, 0.007660997910138013685, 0.007892589632947010977, 0.008124181355756005668, 0.008355773078565002093, 0.008818956524182994944 ),
 .UNSPECIFIED. ) ;
#45969 = CARTESIAN_POINT ( 'NONE',  ( 161.1750406344237661, 251.4836360396366501, -14.21198410781773802 ) ) ;
#45970 = CARTESIAN_POINT ( 'NONE',  ( 78.56719005003022005, 47.98515344134877836, 13.96283253221395704 ) ) ;
#45972 = CARTESIAN_POINT ( 'NONE',  ( 75.98104421115762364, 51.53574906944388800, 16.18761828526978164 ) ) ;
#45971 = CARTESIAN_POINT ( 'NONE',  ( 73.30483403957811106, 69.17932697374330075, -9.895411455429709235 ) ) ;
#45973 = FACE_OUTER_BOUND ( 'NONE', #50141, .T. ) ;
#45974 = CARTESIAN_POINT ( 'NONE',  ( 164.0407096501202204, 246.5201517067746977, -4.555688043559123379 ) ) ;
#45975 = CARTESIAN_POINT ( 'NONE',  ( 157.3988263959001870, 258.0242309610243865, 16.72376558639979294 ) ) ;
#45976 = CARTESIAN_POINT ( 'NONE',  ( 71.81503955391033855, 71.89711284198503449, 2.894600326227580567 ) ) ;
#45977 = AXIS2_PLACEMENT_3D ( 'NONE', #528, #31415, #16227 ) ;
#45978 = CARTESIAN_POINT ( 'NONE',  ( 29.56604717072103483, 194.0024278399160949, 9.188101187500095079 ) ) ;
#45979 = CARTESIAN_POINT ( 'NONE',  ( 55.81761577081934433, 203.0333772461660544, 9.188101187500095079 ) ) ;
#45980 = LINE ( 'NONE', #21224, #53065 ) ;
#45982 = CARTESIAN_POINT ( 'NONE',  ( 199.5166962049540018, 277.5858014024767613, 15.20220047213190995 ) ) ;
#45981 = VECTOR ( 'NONE', #2863, 1000.000000000000000 ) ;
#45983 = CARTESIAN_POINT ( 'NONE',  ( -22.42236680055709641, 157.8615022471902591, 0.000000000000000000 ) ) ;
#45984 = CARTESIAN_POINT ( 'NONE',  ( -7.266922234329411978, 166.6115022471902591, 10.00000000000009592 ) ) ;
#45985 = CARTESIAN_POINT ( 'NONE',  ( -53.02163307513389867, 51.85713630120221751, 59.99999999999999289 ) ) ;
#45986 = EDGE_CURVE ( 'NONE', #1733, #74953, #97330, .T. ) ;
#45987 = CARTESIAN_POINT ( 'NONE',  ( 20.27082849090286842, 27.10171378149918908, 9.188101187500008038 ) ) ;
#45988 = CARTESIAN_POINT ( 'NONE',  ( 150.6438662863770332, 269.7241650738195631, -14.92510732909997628 ) ) ;
#45989 = DIRECTION ( 'NONE',  ( -0.000000000000000000, 0.000000000000000000, -1.000000000000000000 ) ) ;
#45990 = CARTESIAN_POINT ( 'NONE',  ( 14.76917458061509514, 17.03085787977762067, 9.188101187500006262 ) ) ;
#45991 = CARTESIAN_POINT ( 'NONE',  ( 58.87550765610937731, 213.9869531367911009, 4.594050593750046652 ) ) ;
#45992 = CARTESIAN_POINT ( 'NONE',  ( -40.95769633352519890, 38.39369580655643688, 59.99999999999999289 ) ) ;
#45993 = CARTESIAN_POINT ( 'NONE',  ( 79.17632907059281422, 57.86865562274022068, -16.61182437452083249 ) ) ;
#45994 = CARTESIAN_POINT ( 'NONE',  ( 159.7608930362198407, 253.9330115291272421, 15.38895778945778581 ) ) ;
#45995 = CARTESIAN_POINT ( 'NONE',  ( 156.1095879582928774, 264.4631574034182222, 17.55859510772456389 ) ) ;
#45996 = CARTESIAN_POINT ( 'NONE',  ( 153.3697773540452545, 276.7804196118793243, 7.402161975777190150 ) ) ;
#45997 = EDGE_CURVE ( 'NONE', #9815, #72762, #96851, .T. ) ;
#45998 = CARTESIAN_POINT ( 'NONE',  ( 74.34271649381057046, 57.05639872568476534, -16.02907805139209074 ) ) ;
#46000 =( BOUNDED_CURVE ( )  B_SPLINE_CURVE ( 2, ( #3858, #66644, #57538, #97574, #72791, #82409, #59016, #19078, #27163 ),
 .UNSPECIFIED., .F., .T. ) 
 B_SPLINE_CURVE_WITH_KNOTS ( ( 3, 2, 2, 2, 3 ),
 ( 0.07661290322580645296, 0.07795698924731182811, 0.08064516129032257841, 0.08333333333333332871, 0.08467741935483871774 ),
 .UNSPECIFIED. ) 
 CURVE ( )  GEOMETRIC_REPRESENTATION_ITEM ( )  RATIONAL_B_SPLINE_CURVE ( ( 0.9330127018922194093, 0.9330127018922194093, 1.000000000000000000, 0.8660254037844387076, 1.000000000000000000, 0.8660254037844387076, 1.000000000000000000, 0.9330127018922189652, 0.9330127018922192983 ) ) 
 REPRESENTATION_ITEM ( '' )  );
#45999 = CARTESIAN_POINT ( 'NONE',  ( 108.2753003872444140, 239.9865022471903444, -10.00000000000009415 ) ) ;
#46001 = CARTESIAN_POINT ( 'NONE',  ( 161.3227470381586102, 251.2278010437646856, 14.45097375514160731 ) ) ;
#46002 = CARTESIAN_POINT ( 'NONE',  ( 207.5338226493333025, 271.1878702128032614, 6.432541580693135863 ) ) ;
#46003 = ORIENTED_EDGE ( 'NONE', *, *, #16470, .T. ) ;
#46004 = CARTESIAN_POINT ( 'NONE',  ( 76.91861570892473310, 49.78243787368231921, 15.09545489314607281 ) ) ;
#46005 = MANIFOLD_SOLID_BREP ( 'Move Face1', #89593 ) ;
#46006 = VERTEX_POINT ( 'NONE', #13220 ) ;
#46007 = CARTESIAN_POINT ( 'NONE',  ( 206.7408728089182546, 272.5612996242556960, -10.63134519248043475 ) ) ;
#46008 = CARTESIAN_POINT ( 'NONE',  ( 187.7710022618638277, 277.0665775429750397, -17.72351784843695555 ) ) ;
#46009 = EDGE_CURVE ( 'NONE', #14998, #8310, #31524, .T. ) ;
#46010 = CARTESIAN_POINT ( 'NONE',  ( -75.57215499213535281, 50.95729256953105590, 10.00000000000000000 ) ) ;
#46011 = ORIENTED_EDGE ( 'NONE', *, *, #12807, .F. ) ;
#46012 = ORIENTED_EDGE ( 'NONE', *, *, #35961, .F. ) ;
#46013 = CARTESIAN_POINT ( 'NONE',  ( 79.19750788024767019, 46.06220688912179639, -13.21515928786401695 ) ) ;
#46014 = CARTESIAN_POINT ( 'NONE',  ( 148.3874010092782498, 273.6324775792697892, -8.328854486678444857 ) ) ;
#46015 = CARTESIAN_POINT ( 'NONE',  ( 87.10572595599398937, 44.47484308406081510, 6.276395280311344749 ) ) ;
#46016 = DIRECTION ( 'NONE',  ( 0.000000000000000000, 0.7457702847286276082, 0.6662031840330557841 ) ) ;
#46017 = VERTEX_POINT ( 'NONE', #5599 ) ;
#46018 = CARTESIAN_POINT ( 'NONE',  ( 16.80975711337266176, 31.74646525600390135, 2.839279412974139660 ) ) ;
#46019 = CARTESIAN_POINT ( 'NONE',  ( 75.03770635709581427, 55.01706581963784259, 16.14491965273878904 ) ) ;
#46020 = DIRECTION ( 'NONE',  ( -0.000000000000000000, -1.000000000000000000, -0.000000000000000000 ) ) ;
#46021 = CARTESIAN_POINT ( 'NONE',  ( 178.0191268533054938, 276.9262132288450857, 17.58692550855656123 ) ) ;
#46022 = EDGE_CURVE ( 'NONE', #104, #30236, #80486, .T. ) ;
#46023 = VERTEX_POINT ( 'NONE', #60763 ) ;
#46024 = CARTESIAN_POINT ( 'NONE',  ( 152.6977370281523179, 272.7175316449822731, 13.26472897831007458 ) ) ;
#46025 = EDGE_CURVE ( 'NONE', #82781, #10047, #58445, .T. ) ;
#46026 = CARTESIAN_POINT ( 'NONE',  ( 206.7893622945242385, 272.4773133715531230, -10.52881283832460291 ) ) ;
#46027 = EDGE_LOOP ( 'NONE', ( #19449, #13387, #66237, #8314, #65829, #78849, #47306, #30113, #2726, #66004, #86875, #51892, #6314, #92196, #51556, #31052, #92519, #27877, #42656, #77456, #14387, #26247, #41450, #42566, #82489, #61346, #74368, #54379, #35501, #80325, #60709, #41193, #7777, #77512, #20934, #100139, #40169, #47329, #75719, #74623, #88109, #93097, #11701, #62029, #64742, #59773, #5962, #19299, #72236, #20673, #2497, #81852, #83962, #12189, #59079, #26990, #48813, #10589, #78986, #55619, #19975, #30853, #53748, #472, #11536, #60903, #40747, #39163, #58479, #91304, #55763, #46273, #18918, #15162, #83716, #13826, #84507, #70479, #52424, #56039, #38336, #9851, #94611, #12739, #23475, #57427, #48919, #94702, #75385, #72735, #29163, #96972, #80166, #29383, #89529, #43289, #83791, #60464, #70710, #19425, #13791, #29291, #64149, #68727, #58515, #80525, #53689, #82235, #15018, #66736, #49660, #82008, #19942, #26423, #11464, #62503, #30117, #23613, #15015, #20075, #83509, #28019, #51798, #50051, #37925, #93231, #38556, #43035, #99179, #12852, #73857, #91814, #24546, #95366, #55504, #97475, #19645, #50656, #1844, #12464, #74053, #6339, #14137, #2714, #53825, #62813, #42333, #87928, #43013, #36480, #35534, #79103, #77984, #98578, #95282, #94090, #13663, #22859, #15433, #40307, #17679, #70000, #82911, #10843, #66624, #17976, #45190, #33746, #97397, #45155, #99530, #69491, #64776, #68113, #205, #5928, #31589, #13540, #16633, #20641, #72366, #45793, #68487, #45550, #7268, #71161, #12319, #49801, #30625, #14782, #78503, #81864, #16406, #92558, #83229, #30690, #15396, #45272, #40698, #5740, #60951, #47034, #55458, #96082, #88970, #34927, #78509, #36698, #60213, #89913, #63358, #17673, #42196, #41815, #40797, #45400, #82756, #93954, #68366, #68389, #95186, #41465, #63462, #83106, #17642, #17126, #94189, #33452, #59085, #53893, #67771, #66270, #71898, #63563, #76104, #36812, #81617, #73277, #89976, #7213, #96185, #19156, #74647, #12859, #54604, #73593, #7679, #79130, #39560, #42250, #2589, #16183, #92316, #37435, #29218, #34107, #88897, #89259, #41100, #32596, #21493, #35379, #31080, #70373, #22270, #67985, #89283, #75220, #7294, #34151, #15110, #18030, #88745, #87278, #31967, #33098, #19037, #99899, #24176, #94582, #32367, #64270, #97537, #70693, #71973, #79630, #27185, #4362, #51060, #38801, #34874, #37427, #96156, #31741, #57153, #79115, #30399, #68225, #25141, #32630, #575, #20475, #87183, #58436, #76281, #51794, #33622, #49635, #35770, #38346, #22545, #39323, #35929, #8662, #36607, #74279, #62484, #100256, #58414, #51948, #41948, #91700, #80298, #6787, #22536, #31632, #20783, #39304, #67743, #68728, #79905, #95332, #54683, #88808, #4700, #57747, #54749, #87283, #70728, #44954, #60798, #16720, #69369, #16690, #46960, #97291, #39087, #38230, #55860, #42804, #39422, #12295, #81035, #89122, #80750, #24641, #85817, #34634, #82262, #14149, #96656, #96229, #44516, #54260, #25224, #76977, #46512, #59498, #99415, #20290, #94673, #4951, #99681, #95849, #94956, #48056, #8657, #74405, #65015, #81746, #36226, #41546, #52360, #28731, #3001, #83342, #67218, #87362, #42799, #80359, #23489, #44186, #65484, #37545, #92942, #43689, #33059, #57506, #44465, #56898, #18645, #74505, #63382, #36491 ) ) ;
#46028 = CARTESIAN_POINT ( 'NONE',  ( 27.92801399040350319, 72.76188621587162686, 59.99999999999999289 ) ) ;
#46030 = CARTESIAN_POINT ( 'NONE',  ( 67.80572549195380816, 65.59792567543669861, -10.86872875137217243 ) ) ;
#46029 = CARTESIAN_POINT ( 'NONE',  ( 161.8718470072856803, 283.0133716661769654, -3.127779434105778744 ) ) ;
#46031 = CARTESIAN_POINT ( 'NONE',  ( 207.9328781051891042, 270.4966858882232259, -0.8820402142964423042 ) ) ;
#46032 = CARTESIAN_POINT ( 'NONE',  ( 204.1780753366177237, 277.0001950557890495, 14.05599973203924158 ) ) ;
#46033 = CARTESIAN_POINT ( 'NONE',  ( 198.6012358295098750, 286.6595644277572887, 18.21911298807435386 ) ) ;
#46034 = CARTESIAN_POINT ( 'NONE',  ( 164.5827125224535905, 265.0803347849686702, -16.62742669594850753 ) ) ;
#46035 = B_SPLINE_CURVE_WITH_KNOTS ( 'NONE', 3,
 ( #98711, #29296, #21201, #97709, #13107, #28787, #44972, #37860, #75910, #29782, #84519, #6490, #68769, #90640, #20699, #60654, #99693, #43967, #91610, #22183, #52080, #30277, #53076, #84030, #874, #38362, #87044, #24670, #379, #78393, #1887, #55554, #92616, #86537, #54054, #15555, #31268, #85011, #62154, #23657, #16074, #17068, #47959, #94613, #17577, #77388, #69771, #32769, #40357, #39844, #77895, #85532, #78901, #63675 ),
 .UNSPECIFIED., .F., .F.,
 ( 4, 2, 2, 2, 2, 2, 2, 2, 2, 2, 2, 2, 2, 2, 2, 2, 2, 2, 2, 2, 2, 2, 2, 2, 2, 2, 4 ),
 ( 0.0001092562925467074387, 0.0006072969982681204098, 0.001105337703989533408, 0.001354358056850239961, 0.001603378409710946298, 0.001727888586141281685, 0.001852398762571617072, 0.001976908939001952459, 0.002101419115432288064, 0.002350439468292954935, 0.002599459821153621373, 0.003097500526874954682, 0.004093581938317621301, 0.005089663349760287919, 0.005587704055481584366, 0.005836724408342232155, 0.005961234584772556050, 0.006085744761202879077, 0.006147999849418073551, 0.006210254937633268024, 0.006334765114063651767, 0.006583785466924451345, 0.006832805819785250923, 0.007081826172646049633, 0.007330846525506850078, 0.007579866878367648789, 0.008077907584089218454 ),
 .UNSPECIFIED. ) ;
#46036 = CARTESIAN_POINT ( 'NONE',  ( 134.5444773117747275, 257.6744531367911577, 4.594050593750047540 ) ) ;
#46037 = CARTESIAN_POINT ( 'NONE',  ( 159.6585898550698630, 255.0347362821099750, -15.85242424285993401 ) ) ;
#46038 = CARTESIAN_POINT ( 'NONE',  ( 181.9960526061360326, 260.3811653260469825, 9.445214464232433826 ) ) ;
#46039 = CARTESIAN_POINT ( 'NONE',  ( 71.35211999908521818, 205.8768266524160140, 9.188101187500098632 ) ) ;
#46040 = ORIENTED_EDGE ( 'NONE', *, *, #65026, .F. ) ;
#46042 = CARTESIAN_POINT ( 'NONE',  ( 51.80235952159637236, 80.00000000000000000, 59.99999999999999289 ) ) ;
#46041 = B_SPLINE_CURVE_WITH_KNOTS ( 'NONE', 3,
 ( #78798, #92520, #31170, #39256 ),
 .UNSPECIFIED., .F., .F.,
 ( 4, 4 ),
 ( 0.04113468878722496835, 0.04887066958154939050 ),
 .UNSPECIFIED. ) ;
#46043 = DIRECTION ( 'NONE',  ( 0.4999999999999998890, -0.8660254037844385966, 0.000000000000000000 ) ) ;
#46044 = CARTESIAN_POINT ( 'NONE',  ( -27.42236680055714260, 166.5217562850347406, 1.224646799147364892E-15 ) ) ;
#46045 = EDGE_LOOP ( 'NONE', ( #6564, #9439, #12717, #31026 ) ) ;
#46046 = DIRECTION ( 'NONE',  ( -0.09573633691164462611, -0.9954067278227227700, 0.000000000000000000 ) ) ;
#46047 = ORIENTED_EDGE ( 'NONE', *, *, #42284, .F. ) ;
#46048 = ORIENTED_EDGE ( 'NONE', *, *, #63337, .F. ) ;
#46049 = EDGE_CURVE ( 'NONE', #71264, #79283, #20820, .T. ) ;
#46050 = CARTESIAN_POINT ( 'NONE',  ( -19.65312891409030271, 93.06504152958497400, 59.99999999999999289 ) ) ;
#46051 = CARTESIAN_POINT ( 'NONE',  ( 66.87684795978640295, 67.53304424843219067, 6.646635947192834237 ) ) ;
#46052 = CARTESIAN_POINT ( 'NONE',  ( 2.233356772565878057, 160.5494855054051584, -2.679491924311248496 ) ) ;
#46053 = CARTESIAN_POINT ( 'NONE',  ( 146.6647111637776106, 276.6162639173599587, -0.6373001129109082674 ) ) ;
#46054 = FACE_OUTER_BOUND ( 'NONE', #81093, .T. ) ;
#46055 = CARTESIAN_POINT ( 'NONE',  ( 155.0303156110108489, 262.1266119787277944, 17.11986653161320859 ) ) ;
#46056 = CARTESIAN_POINT ( 'NONE',  ( 70.35440405002556474, 63.74960742650419121, 12.91260164709814084 ) ) ;
#46057 = CARTESIAN_POINT ( 'NONE',  ( 76.95378796010953693, 224.4244531367911293, -4.594050593750046652 ) ) ;
#46058 = VERTEX_POINT ( 'NONE', #31873 ) ;
#46059 = VECTOR ( 'NONE', #29032, 1000.000000000000000 ) ;
#46060 = EDGE_CURVE ( 'NONE', #52312, #43398, #90158, .T. ) ;
#46061 = CARTESIAN_POINT ( 'NONE',  ( 200.5982530106205388, 283.2006292064855870, -16.76555514870729624 ) ) ;
#46062 = ORIENTED_EDGE ( 'NONE', *, *, #61273, .T. ) ;
#46063 = DIRECTION ( 'NONE',  ( -0.5000000000000014433, 0.8660254037844379305, 0.000000000000000000 ) ) ;
#46064 = VECTOR ( 'NONE', #56747, 1000.000000000000000 ) ;
#46065 = EDGE_CURVE ( 'NONE', #64385, #40435, #62266, .T. ) ;
#46066 = CARTESIAN_POINT ( 'NONE',  ( 183.6775799446257622, 275.6805839496243493, 16.80015316766806421 ) ) ;
#46067 = EDGE_CURVE ( 'NONE', #39162, #78092, #30647, .T. ) ;
#46068 = CARTESIAN_POINT ( 'NONE',  ( 162.6897041064822247, 284.0413850360118317, 0.5105129000292804031 ) ) ;
#46069 = DIRECTION ( 'NONE',  ( -0.8660254037844387076, -0.4999999999999998890, -0.000000000000000000 ) ) ;
#46070 = CARTESIAN_POINT ( 'NONE',  ( 162.1730311952291572, 261.1847194969478210, 16.85311962717550571 ) ) ;
#46071 = ORIENTED_EDGE ( 'NONE', *, *, #737, .T. ) ;
#46072 = CARTESIAN_POINT ( 'NONE',  ( 83.09294558526256935, 43.66384112246667826, -7.909259972356729840 ) ) ;
#46073 = EDGE_CURVE ( 'NONE', #22887, #83079, #1995, .T. ) ;
#46074 = CARTESIAN_POINT ( 'NONE',  ( 156.6719645457748982, 274.0816551557289245, 13.52539259823061357 ) ) ;
#46075 = EDGE_CURVE ( 'NONE', #64873, #94973, #730, .T. ) ;
#46076 = CARTESIAN_POINT ( 'NONE',  ( 147.7561322771605319, 275.4500581284187888, -3.854405246717441447 ) ) ;
#46077 = CARTESIAN_POINT ( 'NONE',  ( 153.2513309553138470, 265.2079037882803618, -16.24091495603130397 ) ) ;
#46078 = CARTESIAN_POINT ( 'NONE',  ( 79.49298289701215481, 59.22797875817073532, -16.22298816110328445 ) ) ;
#46079 = CARTESIAN_POINT ( 'NONE',  ( 68.91844246388177453, 67.43096903599641223, -8.746045204043648269 ) ) ;
#46080 = ORIENTED_EDGE ( 'NONE', *, *, #92511, .T. ) ;
#46081 = CARTESIAN_POINT ( 'NONE',  ( 199.6331895497083337, 266.8549210871742048, 4.611541600118369111 ) ) ;
#46082 = CARTESIAN_POINT ( 'NONE',  ( 152.5423653171682474, 268.4358682943698682, -15.78187745328793490 ) ) ;
#46083 = CARTESIAN_POINT ( 'NONE',  ( 193.8477229354528220, 262.3541544976313844, 2.578193913946859706 ) ) ;
#46084 = CARTESIAN_POINT ( 'NONE',  ( 184.8052499677449134, 263.9936221479479173, -12.13309983589799046 ) ) ;
#46085 = CARTESIAN_POINT ( 'NONE',  ( 83.90995141641640487, 51.89037297248786018, 14.88406197085304150 ) ) ;
#46086 = CARTESIAN_POINT ( 'NONE',  ( 156.9199168296383391, 272.6955506662872608, 14.53585852203788598 ) ) ;
#46087 = ORIENTED_EDGE ( 'NONE', *, *, #36576, .T. ) ;
#46088 = CARTESIAN_POINT ( 'NONE',  ( 146.8881680668833951, 276.2292252078784145, 4.973452195244782104 ) ) ;
#46089 = CARTESIAN_POINT ( 'NONE',  ( 186.8476719251497968, 282.1398254177984768, 17.29477932248579819 ) ) ;
#46090 = VECTOR ( 'NONE', #9291, 1000.000000000000227 ) ;
#46091 = CARTESIAN_POINT ( 'NONE',  ( 207.0548180518391916, 272.0175305127218053, 7.721676452263806389 ) ) ;
#46093 = CARTESIAN_POINT ( 'NONE',  ( 74.05984977965144367, 55.09172014556617114, 16.60385058087775434 ) ) ;
#46092 = CARTESIAN_POINT ( 'NONE',  ( -66.34925969370661392, 42.61035540433362456, 10.00000000000000000 ) ) ;
#46094 = CARTESIAN_POINT ( 'NONE',  ( 22.68382546022871438, 31.83478043621389020, -8.090169943749479842 ) ) ;
#46095 = DIRECTION ( 'NONE',  ( 0.000000000000000000, 0.000000000000000000, 1.000000000000000000 ) ) ;
#46096 = CARTESIAN_POINT ( 'NONE',  ( 163.3401707525704296, 283.7542478731094207, -3.207333608244951062 ) ) ;
#46097 = CARTESIAN_POINT ( 'NONE',  ( -31.59160691316810343, 24.09060609829247568, -10.00000000000000000 ) ) ;
#46098 = CARTESIAN_POINT ( 'NONE',  ( 198.5558597050348908, 286.7381581807989051, 17.16554469393394200 ) ) ;
#46099 = CARTESIAN_POINT ( 'NONE',  ( -9.134289513013563067, 165.5333772461660828, 9.188101187500095079 ) ) ;
#46100 = CARTESIAN_POINT ( 'NONE',  ( 26.11609497015385983, 119.4899152597536869, 54.99999999999999289 ) ) ;
#46101 = ORIENTED_EDGE ( 'NONE', *, *, #75275, .T. ) ;
#46102 = CARTESIAN_POINT ( 'NONE',  ( 178.8506441891429120, 256.6935935793209751, 8.649200206363696353 ) ) ;
#46103 = CARTESIAN_POINT ( 'NONE',  ( 72.67905965592417772, 70.26320000030698054, -8.002569769838697056 ) ) ;
#46104 = CARTESIAN_POINT ( 'NONE',  ( -29.91485116994501325, 25.08783183303773967, -10.00000000000000000 ) ) ;
#46105 = DIRECTION ( 'NONE',  ( 0.4999999999999998890, -0.8660254037844385966, 0.000000000000000000 ) ) ;
#46106 = CARTESIAN_POINT ( 'NONE',  ( 11.05475416482865114, 183.3149278399161233, 9.188101187500093303 ) ) ;
#46107 = CARTESIAN_POINT ( 'NONE',  ( 76.96225540874074511, 63.35506444885830035, -15.47139205492574554 ) ) ;
#46108 = CARTESIAN_POINT ( 'NONE',  ( 24.08258844821711264, 36.83705186507755514, 3.090169943749475401 ) ) ;
#46109 = CARTESIAN_POINT ( 'NONE',  ( 119.7014708956357794, 251.4637435831425023, 2.679491924311251605 ) ) ;
#46110 = CARTESIAN_POINT ( 'NONE',  ( 157.4893260420801653, 257.8674809757739013, -18.30842125257398223 ) ) ;
#46111 = DIRECTION ( 'NONE',  ( 0.8660254037844379305, 0.5000000000000014433, 0.000000000000000000 ) ) ;
#46112 = CARTESIAN_POINT ( 'NONE',  ( 175.5045987706217829, 253.5154819701446058, -3.738308729259062435 ) ) ;
#46113 = CARTESIAN_POINT ( 'NONE',  ( -52.83961229143921656, 94.84783475815204667, -10.00000000000000000 ) ) ;
#46114 = VECTOR ( 'NONE', #97424, 1000.000000000000000 ) ;
#46115 = CARTESIAN_POINT ( 'NONE',  ( 75.43850382708453139, 204.3615022471901739, 5.000000000000051514 ) ) ;
#46116 = CARTESIAN_POINT ( 'NONE',  ( 44.67827877960949223, 26.76426979415094110, 3.090169943749476733 ) ) ;
#46117 = CARTESIAN_POINT ( 'NONE',  ( 148.3190727836317535, 273.7508255376806119, 8.080277324579027365 ) ) ;
#46118 = CARTESIAN_POINT ( 'NONE',  ( 32.11017034222032862, 189.3458772461660544, 9.188101187500095079 ) ) ;
#46119 = CARTESIAN_POINT ( 'NONE',  ( 66.45982511243997237, 67.83556696074005288, 6.764132809977054350 ) ) ;
#46120 = CARTESIAN_POINT ( 'NONE',  ( 36.98912467918979274, 21.75978393459167393, -1.583844403245396437 ) ) ;
#46121 = CARTESIAN_POINT ( 'NONE',  ( 77.16105698610837749, 49.60253137911669796, -14.98352156587448114 ) ) ;
#46122 = CARTESIAN_POINT ( 'NONE',  ( 199.0363797504450929, 285.9058730480928716, -17.12190301149298222 ) ) ;
#46124 = EDGE_CURVE ( 'NONE', #77820, #63549, #96239, .T. ) ;
#46123 = CIRCLE ( 'NONE', #18693, 70.00000000000001421 ) ;
#46125 = CARTESIAN_POINT ( 'NONE',  ( 207.6727254509676186, 270.9472835030587703, 7.315149605389819953 ) ) ;
#46126 = CARTESIAN_POINT ( 'NONE',  ( 185.1787217285512384, 266.7930642242706654, 13.70357059227357688 ) ) ;
#46127 = CARTESIAN_POINT ( 'NONE',  ( 162.0955723731790101, 279.9228038994015719, -9.850904930694312611 ) ) ;
#46128 = CARTESIAN_POINT ( 'NONE',  ( 164.0322825057177170, 281.5311351839372946, 8.862866254731592619 ) ) ;
#46129 = PRODUCT_CONTEXT ( 'NONE', #67032, 'mechanical' ) ;
#46130 = CARTESIAN_POINT ( 'NONE',  ( 26.78885238572174998, 16.26216523072495690, -2.296566073217252530E-15 ) ) ;
#46131 = CARTESIAN_POINT ( 'NONE',  ( -68.10632939235270555, 44.28490124273479012, -10.00000000000000000 ) ) ;
#46132 = CARTESIAN_POINT ( 'NONE',  ( 71.40067601551650966, 59.33978977576644098, 15.72537452617927478 ) ) ;
#46133 = CARTESIAN_POINT ( 'NONE',  ( 188.8338017993633571, 269.9617145311643185, -14.08363440685359791 ) ) ;
#46134 = ORIENTED_EDGE ( 'NONE', *, *, #18760, .T. ) ;
#46135 = CARTESIAN_POINT ( 'NONE',  ( 6.802937163926562114, 15.87878583063839066, -9.188101187500006262 ) ) ;
#46136 = DIRECTION ( 'NONE',  ( -0.000000000000000000, -1.000000000000000000, -0.000000000000000000 ) ) ;
#46137 = CARTESIAN_POINT ( 'NONE',  ( 81.64627816295647733, 42.63038875969535724, 7.551097713807430445 ) ) ;
#46138 = ADVANCED_FACE ( 'NONE', ( #54667 ), #7586, .T. ) ;
#46139 = ORIENTED_EDGE ( 'NONE', *, *, #41602, .F. ) ;
#46140 = CARTESIAN_POINT ( 'NONE',  ( 23.90999230191033575, 194.6115022471903160, -5.000000000000047962 ) ) ;
#46141 = CARTESIAN_POINT ( 'NONE',  ( 72.57727468335085064, 71.31820506079068878, -5.984807345722121141 ) ) ;
#46142 = CARTESIAN_POINT ( 'NONE',  ( 76.78727678290111669, 63.87399086453137187, 14.88032377382801030 ) ) ;
#46143 = EDGE_CURVE ( 'NONE', #21282, #99967, #15169, .T. ) ;
#46144 = CARTESIAN_POINT ( 'NONE',  ( 170.6538086303071111, 280.9384219949420185, -14.72317928558904754 ) ) ;
#46145 = ORIENTED_EDGE ( 'NONE', *, *, #4718, .F. ) ;
#46146 = VERTEX_POINT ( 'NONE', #62776 ) ;
#46148 = CARTESIAN_POINT ( 'NONE',  ( 85.27848080570771572, 42.86259319836502613, -3.223099939885945453 ) ) ;
#46147 = CARTESIAN_POINT ( 'NONE',  ( 187.1893300299016687, 272.3238949448195285, -16.82286396092820979 ) ) ;
#46149 = ORIENTED_EDGE ( 'NONE', *, *, #98556, .T. ) ;
#46150 = CARTESIAN_POINT ( 'NONE',  ( 150.6790040019602088, 269.6633047651677089, 15.38315204620803378 ) ) ;
#46151 = CARTESIAN_POINT ( 'NONE',  ( 21.80251038182309031, 34.36126292948896577, 6.180339887498949913 ) ) ;
#46152 = CARTESIAN_POINT ( 'NONE',  ( 80.03994542435373205, 57.65115798690544580, 16.60126445886218249 ) ) ;
#46153 = CARTESIAN_POINT ( 'NONE',  ( 52.39861964368810732, 194.3927522451417929, -10.00000000000009237 ) ) ;
#46154 = ORIENTED_EDGE ( 'NONE', *, *, #82211, .T. ) ;
#46155 = CARTESIAN_POINT ( 'NONE',  ( 148.0427192501136062, 274.2294838985851015, 9.385226820296049155 ) ) ;
#46156 = CARTESIAN_POINT ( 'NONE',  ( 149.1939152435731728, 272.2355539484436235, -11.44223522189843933 ) ) ;
#46157 = ORIENTED_EDGE ( 'NONE', *, *, #16678, .F. ) ;
#46158 = CARTESIAN_POINT ( 'NONE',  ( 195.8947060313465443, 291.3474115503753410, 16.07878593000791767 ) ) ;
#46159 = CARTESIAN_POINT ( 'NONE',  ( 158.5477485432647313, 265.3246957002631916, 17.03042601231237896 ) ) ;
#46160 = ORIENTED_EDGE ( 'NONE', *, *, #6151, .T. ) ;
#46161 = CARTESIAN_POINT ( 'NONE',  ( 149.2561433752359505, 272.1277716627430436, 12.99353668144589946 ) ) ;
#46162 = CARTESIAN_POINT ( 'NONE',  ( -1.588913428802907202, 65.16871292612921707, -10.00000000000000000 ) ) ;
#46163 = ORIENTED_EDGE ( 'NONE', *, *, #59614, .T. ) ;
#46164 = CARTESIAN_POINT ( 'NONE',  ( -14.36410898293827998, 72.70576163098405686, 13.91634736112990645 ) ) ;
#46165 = CARTESIAN_POINT ( 'NONE',  ( 150.6487462746963502, 269.7157126861102370, 15.18501655901553704 ) ) ;
#46166 = DIRECTION ( 'NONE',  ( -0.009162850352631533510, 0.9999580202055560196, 0.000000000000000000 ) ) ;
#46167 = VECTOR ( 'NONE', #58410, 1000.000000000000000 ) ;
#46168 = CARTESIAN_POINT ( 'NONE',  ( 31.01079167849261964, 40.83705186507756224, 3.090169943749475401 ) ) ;
#46169 = VERTEX_POINT ( 'NONE', #86648 ) ;
#46170 = ORIENTED_EDGE ( 'NONE', *, *, #16976, .F. ) ;
#46171 = ADVANCED_FACE ( 'NONE', ( #47579 ), #16191, .T. ) ;
#46172 = CARTESIAN_POINT ( 'NONE',  ( 86.97134532988273747, 46.47825607565307138, 8.944163774166895564 ) ) ;
#46173 = CARTESIAN_POINT ( 'NONE',  ( 82.50043972687433325, 42.71205652650662188, -6.855908010978745359 ) ) ;
#46174 = CARTESIAN_POINT ( 'NONE',  ( 77.46154149802761424, 203.9824982072973967, 3.021315404115420679E-15 ) ) ;
#46175 = CARTESIAN_POINT ( 'NONE',  ( 147.8465295590381743, 274.5692944114487091, 9.322947948439978205 ) ) ;
#46176 = CARTESIAN_POINT ( 'NONE',  ( 190.1190668544949460, 301.3511120508678118, 4.410340539513557090 ) ) ;
#46177 = CARTESIAN_POINT ( 'NONE',  ( 172.1606859485697498, 275.9764482197007851, -15.78976850212529826 ) ) ;
#46178 = CARTESIAN_POINT ( 'NONE',  ( 164.1654149204426858, 248.3041558426086226, -9.671695341034215687 ) ) ;
#46179 = CARTESIAN_POINT ( 'NONE',  ( 147.2658550951450422, 275.5750520855697800, -5.215660180131691526 ) ) ;
#46180 = EDGE_CURVE ( 'NONE', #87041, #18408, #78507, .T. ) ;
#46181 = CARTESIAN_POINT ( 'NONE',  ( 163.9020937770961552, 257.0909063598783746, 15.75990737960287369 ) ) ;
#46182 = CARTESIAN_POINT ( 'NONE',  ( -22.42236680055709641, 157.8615022471902591, 0.000000000000000000 ) ) ;
#46183 = CARTESIAN_POINT ( 'NONE',  ( 67.56897137201481485, 70.11578694084727204, 0.8315581512064480485 ) ) ;
#46184 = CARTESIAN_POINT ( 'NONE',  ( 67.17708281894157096, 66.61742757574968721, 8.430827746126428934 ) ) ;
#46185 = CARTESIAN_POINT ( 'NONE',  ( 72.64749865597310929, 65.05606228103368949, -12.97249523173932317 ) ) ;
#46186 = CARTESIAN_POINT ( 'NONE',  ( 78.12916722883838361, 47.65424050001094969, 14.47278094148724747 ) ) ;
#46187 = CARTESIAN_POINT ( 'NONE',  ( 107.4275774994220001, 223.6423013555409796, -4.594050593750043987 ) ) ;
#46188 = ORIENTED_EDGE ( 'NONE', *, *, #95834, .F. ) ;
#46189 = AXIS2_PLACEMENT_3D ( 'NONE', #96295, #59221, #35945 ) ;
#46190 = CARTESIAN_POINT ( 'NONE',  ( 149.2237128415488598, 272.1839429948059319, -13.04302063563883607 ) ) ;
#46191 = CARTESIAN_POINT ( 'NONE',  ( 82.53859975423060291, 41.16651341379471774, -2.370924961068094028 ) ) ;
#46192 = EDGE_CURVE ( 'NONE', #64644, #31200, #79222, .T. ) ;
#46193 = CARTESIAN_POINT ( 'NONE',  ( -76.23101443460923576, 54.01191295053621388, -10.00000000000000000 ) ) ;
#46194 = CARTESIAN_POINT ( 'NONE',  ( 78.88871661031990357, 46.37012301642865708, 12.94053771451172352 ) ) ;
#46195 = CARTESIAN_POINT ( 'NONE',  ( 179.9795673731253487, 282.8863147452317435, -15.33225209653127585 ) ) ;
#46196 = CARTESIAN_POINT ( 'NONE',  ( 189.9366275249276157, 301.6671062389771691, -0.07615766263248391343 ) ) ;
#46197 = CARTESIAN_POINT ( 'NONE',  ( 168.6230640848619373, 286.4021248756633895, -8.144242964583304101 ) ) ;
#46198 = ORIENTED_EDGE ( 'NONE', *, *, #44935, .F. ) ;
#46199 = CARTESIAN_POINT ( 'NONE',  ( 207.6067494229581314, 271.0615573356529353, -1.924113146155245868 ) ) ;
#46200 = CARTESIAN_POINT ( 'NONE',  ( 72.27003297432077034, 71.75159315020286499, 5.546042747704616360 ) ) ;
#46201 = CARTESIAN_POINT ( 'NONE',  ( 49.80054343233477709, 192.8927522451417929, -10.00000000000009059 ) ) ;
#46202 = CARTESIAN_POINT ( 'NONE',  ( 122.2847184155099995, 253.6589784336661069, -6.496448406907676862E-16 ) ) ;
#46203 = CARTESIAN_POINT ( 'NONE',  ( 180.4966966598214242, 294.5715408904403603, -3.526636318079005239 ) ) ;
#46204 = LINE ( 'NONE', #14823, #43199 ) ;
#46205 = CARTESIAN_POINT ( 'NONE',  ( 157.7861133721078772, 257.3534302411229646, 18.03837896619386783 ) ) ;
#46206 = CARTESIAN_POINT ( 'NONE',  ( 175.1236258135627679, 253.3313582753198716, -3.877381073628868524 ) ) ;
#46207 = CARTESIAN_POINT ( 'NONE',  ( 48.99766571601688270, 199.0958772461660544, -9.188101187500095079 ) ) ;
#46208 = CARTESIAN_POINT ( 'NONE',  ( 113.5436215935997808, 236.3615022471902307, -10.00000000000009592 ) ) ;
#46209 = CARTESIAN_POINT ( 'NONE',  ( 189.4199209167946663, 300.3895034224956930, 3.306026617473488027 ) ) ;
#46210 = ORIENTED_EDGE ( 'NONE', *, *, #61176, .T. ) ;
#46211 = CARTESIAN_POINT ( 'NONE',  ( 71.03260519239540827, 63.40884879191646917, 13.38662637038426162 ) ) ;
#46212 = CARTESIAN_POINT ( 'NONE',  ( 88.07640460957951234, 44.67800788684087365, -4.250388008292100395 ) ) ;
#46213 = CARTESIAN_POINT ( 'NONE',  ( 48.91560817564824504, 80.00000000000000000, 10.00000000000000178 ) ) ;
#46214 = LINE ( 'NONE', #54827, #17507 ) ;
#46215 = LINE ( 'NONE', #36637, #98089 ) ;
#46216 = DIRECTION ( 'NONE',  ( -0.3473291852295006810, 0.6015917957689992379, 0.7193398003386451967 ) ) ;
#46217 = CARTESIAN_POINT ( 'NONE',  ( 108.1850894041355957, 243.2677522451419065, -5.000000000000047962 ) ) ;
#46218 = CARTESIAN_POINT ( 'NONE',  ( 172.9311764467664716, 268.4779053881692334, -17.72160738022306603 ) ) ;
#46219 = ORIENTED_EDGE ( 'NONE', *, *, #8287, .T. ) ;
#46220 = EDGE_CURVE ( 'NONE', #57499, #41965, #26080, .T. ) ;
#46221 = B_SPLINE_CURVE_WITH_KNOTS ( 'NONE', 3,
 ( #36489, #6601, #67392, #83637 ),
 .UNSPECIFIED., .F., .F.,
 ( 4, 4 ),
 ( 0.01296617310113466065, 0.01931249317442805188 ),
 .UNSPECIFIED. ) ;
#46222 = CARTESIAN_POINT ( 'NONE',  ( 189.8123550829396891, 301.8823524224806647, -0.5679054518196169354 ) ) ;
#46223 = CARTESIAN_POINT ( 'NONE',  ( 80.76073326117044360, 47.44888180215133389, -13.52495504245785796 ) ) ;
#46224 = VECTOR ( 'NONE', #51059, 1000.000000000000114 ) ;
#46225 = CARTESIAN_POINT ( 'NONE',  ( 31.65035466828360100, 179.8923013555409796, 4.594050593750050204 ) ) ;
#46226 = CARTESIAN_POINT ( 'NONE',  ( 13.59582392308679033, 19.80066082961420548, 10.00000000000000533 ) ) ;
#46227 = CARTESIAN_POINT ( 'NONE',  ( -17.37321732699747656, 104.5861979058573752, 44.53294705236607598 ) ) ;
#46228 = CARTESIAN_POINT ( 'NONE',  ( 146.8729474948188454, 276.2555880120147549, 3.934020695290606273 ) ) ;
#46229 = CARTESIAN_POINT ( 'NONE',  ( 75.20389695419315501, 52.88180760346911313, -15.99093876381489920 ) ) ;
#46231 = CARTESIAN_POINT ( 'NONE',  ( 73.21957404993666785, 203.8923013555409796, 4.594050593750050204 ) ) ;
#46230 = CARTESIAN_POINT ( 'NONE',  ( 174.6162333118450931, 286.4903673861072662, 10.29252846444475722 ) ) ;
#46232 = CARTESIAN_POINT ( 'NONE',  ( 161.3644539559160478, 251.1555625431813894, 12.97746593258196413 ) ) ;
#46233 = CARTESIAN_POINT ( 'NONE',  ( 73.08053648531546287, 57.27840619054814653, 15.90006795040070564 ) ) ;
#46234 = CARTESIAN_POINT ( 'NONE',  ( -30.94311057985214575, 96.87776860595468520, 44.50898273599062804 ) ) ;
#46235 = CARTESIAN_POINT ( 'NONE',  ( 66.61202643439548865, 68.34816216382951382, -4.339165927432250491 ) ) ;
#46236 = VERTEX_POINT ( 'NONE', #65772 ) ;
#46237 = AXIS2_PLACEMENT_3D ( 'NONE', #28625, #98555, #29142 ) ;
#46238 = CARTESIAN_POINT ( 'NONE',  ( 27.87927540258900549, 200.2365022471903160, 2.944929066748280225E-16 ) ) ;
#46239 = CARTESIAN_POINT ( 'NONE',  ( 207.9622466093905189, 270.4458181468041289, 3.586592550214158681 ) ) ;
#46240 = CARTESIAN_POINT ( 'NONE',  ( 148.5637841791828464, 247.3923013555409796, 4.594050593750050204 ) ) ;
#46241 = CARTESIAN_POINT ( 'NONE',  ( 25.24689923506580769, 37.68290643055188838, 3.479690158560446702E-15 ) ) ;
#46242 = CARTESIAN_POINT ( 'NONE',  ( 164.5139018292655919, 259.6662038739244736, -17.01387605652571366 ) ) ;
#46243 = CARTESIAN_POINT ( 'NONE',  ( 185.4827390772690876, 260.4226536598483790, 6.340749577449164676 ) ) ;
#46244 = CARTESIAN_POINT ( 'NONE',  ( 164.4573439719129340, 245.7985198932525748, 1.541132361166968501 ) ) ;
#46245 = EDGE_CURVE ( 'NONE', #95962, #90569, #25808, .T. ) ;
#46247 = CARTESIAN_POINT ( 'NONE',  ( 189.0720805967732758, 299.7343203868808246, 4.955419684386629164 ) ) ;
#46246 = CARTESIAN_POINT ( 'NONE',  ( 68.81692840119013965, 68.11752969850674333, 8.558253326585221643 ) ) ;
#46248 = CARTESIAN_POINT ( 'NONE',  ( 68.45038622130651618, 64.39200674863153040, 12.27119139371030876 ) ) ;
#46249 = VERTEX_POINT ( 'NONE', #87666 ) ;
#46250 = CARTESIAN_POINT ( 'NONE',  ( 190.8443993347725325, 300.0947993426467519, 8.522468760355437212 ) ) ;
#46251 = CARTESIAN_POINT ( 'NONE',  ( 178.4979445755931806, 285.4942094443755991, 13.01262888890980385 ) ) ;
#46252 = CARTESIAN_POINT ( 'NONE',  ( 156.3390064593949944, 279.7328267885979471, -5.286091551933326471 ) ) ;
#46253 = CARTESIAN_POINT ( 'NONE',  ( 8.064688198948626763, 22.84336893147754211, -7.433330006724137462 ) ) ;
#46254 = EDGE_LOOP ( 'NONE', ( #98527, #45817, #22397, #19442 ) ) ;
#46255 = DIRECTION ( 'NONE',  ( 0.000000000000000000, -0.000000000000000000, 1.000000000000000000 ) ) ;
#46256 = CARTESIAN_POINT ( 'NONE',  ( 168.0457992865198662, 281.9604434737263432, -10.94842533682070140 ) ) ;
#46257 = VECTOR ( 'NONE', #5996, 1000.000000000000000 ) ;
#46258 = CARTESIAN_POINT ( 'NONE',  ( 157.5487431480040925, 257.7645675294749594, -18.29554785922338311 ) ) ;
#46259 = EDGE_CURVE ( 'NONE', #56418, #31865, #2506, .T. ) ;
#46260 = DIRECTION ( 'NONE',  ( 0.4999999999999992784, -0.8660254037844390407, 0.000000000000000000 ) ) ;
#46261 = CARTESIAN_POINT ( 'NONE',  ( 190.7144704529493140, 295.3703424786987739, 12.68450966750776843 ) ) ;
#46262 = CARTESIAN_POINT ( 'NONE',  ( -19.64260764713147012, 93.20647363903802329, 59.99999999999999289 ) ) ;
#46263 = EDGE_CURVE ( 'NONE', #9173, #58927, #50087, .T. ) ;
#46264 = CARTESIAN_POINT ( 'NONE',  ( 207.6163508138795635, 271.0449272387537576, -1.385071889578343152 ) ) ;
#46265 = CARTESIAN_POINT ( 'NONE',  ( 200.8251833487811666, 282.8075743310126882, -16.74393672780000131 ) ) ;
#46266 = EDGE_LOOP ( 'NONE', ( #40449, #26862, #23490, #52510 ) ) ;
#46267 = CARTESIAN_POINT ( 'NONE',  ( 190.6261097325742355, 281.3049748184752161, 16.80476181508462474 ) ) ;
#46268 = CARTESIAN_POINT ( 'NONE',  ( 72.94255135865869022, 70.82539339859251015, 7.334897578941317775 ) ) ;
#46269 = VERTEX_POINT ( 'NONE', #26297 ) ;
#46270 = CARTESIAN_POINT ( 'NONE',  ( 190.7862358025146534, 300.1955415356651429, 3.573119809004446257 ) ) ;
#46271 = CARTESIAN_POINT ( 'NONE',  ( 17.37407021781635663, 33.52903772873357013, -1.583844403245363575 ) ) ;
#46272 = CARTESIAN_POINT ( 'NONE',  ( 82.67802903814479976, 45.32635663605926624, -10.34136681600037022 ) ) ;
#46273 = ORIENTED_EDGE ( 'NONE', *, *, #55410, .T. ) ;
#46274 = CARTESIAN_POINT ( 'NONE',  ( 191.3413020738616410, 299.2341385521244774, -8.295023558158421295 ) ) ;
#46275 = CARTESIAN_POINT ( 'NONE',  ( 79.32566820500106530, 59.73991648520960496, -16.51753030644416498 ) ) ;
#46276 = CARTESIAN_POINT ( 'NONE',  ( 149.4456112649506281, 271.7996036513546869, -12.95648166494593667 ) ) ;
#46277 = CARTESIAN_POINT ( 'NONE',  ( 69.78819819425497428, 62.70547683012449625, 13.91779829744284314 ) ) ;
#46278 = EDGE_LOOP ( 'NONE', ( #77574, #25505, #52908, #47791 ) ) ;
#46279 = CARTESIAN_POINT ( 'NONE',  ( 96.25000326212280299, 232.5024278399160664, -9.188101187500093303 ) ) ;
#46280 = CARTESIAN_POINT ( 'NONE',  ( 200.4116241316243645, 283.5238799070667142, 18.37703770054986663 ) ) ;
#46281 = CARTESIAN_POINT ( 'NONE',  ( 190.9061255863007318, 299.9878863388391892, 7.497146773253707153 ) ) ;
#46282 = CARTESIAN_POINT ( 'NONE',  ( 81.47153209085804804, 42.18456630836416110, -8.000817679882061384 ) ) ;
#46283 = ORIENTED_EDGE ( 'NONE', *, *, #70529, .T. ) ;
#46284 = VERTEX_POINT ( 'NONE', #18200 ) ;
#46285 = ORIENTED_EDGE ( 'NONE', *, *, #51710, .F. ) ;
#46286 = CARTESIAN_POINT ( 'NONE',  ( 74.34779163019582882, 65.75635227628464463, 13.22858955973211970 ) ) ;
#46287 = ORIENTED_EDGE ( 'NONE', *, *, #77073, .T. ) ;
#46288 = CARTESIAN_POINT ( 'NONE',  ( 70.29083157674634208, 70.92442123829498257, 3.057200561768157687 ) ) ;
#46289 = ORIENTED_EDGE ( 'NONE', *, *, #32493, .T. ) ;
#46290 = CARTESIAN_POINT ( 'NONE',  ( 207.5583741822599393, 271.1453457103705205, 3.140867606700001424 ) ) ;
#46291 = ADVANCED_FACE ( 'NONE', ( #41983 ), #49581, .T. ) ;
#46292 = CARTESIAN_POINT ( 'NONE',  ( 83.82827945288542537, 51.88092520783234818, 14.50189114860043205 ) ) ;
#46293 = CARTESIAN_POINT ( 'NONE',  ( 167.7567270317426846, 281.0680522135961610, 11.62081748593863395 ) ) ;
#46294 = ADVANCED_FACE ( 'NONE', ( #34872 ), #68793, .T. ) ;
#46295 = CARTESIAN_POINT ( 'NONE',  ( 147.6095889327917803, 274.9796876144846465, -8.460961150142429332 ) ) ;
#46296 = B_SPLINE_CURVE_WITH_KNOTS ( 'NONE', 3,
 ( #42425, #82979, #52040, #58620, #28741, #13554, #5937, #27255, #58138, #66733, #5446, #81983, #73358, #89595, #20160, #88609, #81486, #89118, #81001, #12557, #3946, #43431, #4439, #98664, #4958, #42910, #59617, #35839, #34829, #97666, #28234, #13065, #90082, #73851, #44427, #20650, #21159, #90595, #75356, #36831, #67740, #65730, #29246, #19176, #96685, #6924 ),
 .UNSPECIFIED., .F., .F.,
 ( 4, 1, 1, 1, 2, 2, 1, 1, 1, 2, 2, 1, 1, 2, 2, 1, 1, 2, 2, 1, 1, 2, 2, 1, 2, 2, 1, 2, 2, 4 ),
 ( 0.000000000000000000, 0.06249999999997736533, 0.09374999999996795619, 0.1093749999999633349, 0.1171874999999610173, 0.1249999999999586997, 0.1874999999999466260, 0.2187499999999406863, 0.2343749999999379663, 0.2421874999999366063, 0.2499999999999352185, 0.3124999999999348854, 0.3437499999999346634, 0.3593749999999363842, 0.3749999999999381051, 0.4374999999999475420, 0.4687499999999538147, 0.4843749999999565348, 0.4999999999999592548, 0.5624999999999614753, 0.5937499999999609201, 0.6093749999999625855, 0.6249999999999642508, 0.6874999999999723554, 0.7187499999999767963, 0.7499999999999812372, 0.8124999999999902300, 0.8437499999999923395, 0.8749999999999944489, 1.000000000000000000 ),
 .UNSPECIFIED. ) ;
#46297 = CARTESIAN_POINT ( 'NONE',  ( 82.62542648728522465, 54.14492212412226024, -15.90696914271030238 ) ) ;
#46298 = VERTEX_POINT ( 'NONE', #89114 ) ;
#46299 = CARTESIAN_POINT ( 'NONE',  ( 79.88009824201490972, 55.32498818933279949, -16.43691830321638747 ) ) ;
#46300 = CARTESIAN_POINT ( 'NONE',  ( 14.59716579798650571, 20.37878583063839955, 9.188101187500006262 ) ) ;
#46301 = AXIS2_PLACEMENT_3D ( 'NONE', #94478, #25033, #50334 ) ;
#46302 = CARTESIAN_POINT ( 'NONE',  ( -27.42236680055714260, 166.5217562850347406, 1.224646799147364892E-15 ) ) ;
#46303 = CARTESIAN_POINT ( 'NONE',  ( 80.35079170152107508, 57.80872192622026517, 16.60075256504292796 ) ) ;
#46305 = VERTEX_POINT ( 'NONE', #49536 ) ;
#46304 = CARTESIAN_POINT ( 'NONE',  ( -40.08433460452723551, 25.84155934987275671, 10.00000000000000000 ) ) ;
#46306 = VECTOR ( 'NONE', #43714, 1000.000000000000000 ) ;
#46307 = CARTESIAN_POINT ( 'NONE',  ( 170.3868164922740505, 258.7065172848251677, -13.94078176683852810 ) ) ;
#46308 = CARTESIAN_POINT ( 'NONE',  ( 44.85148386036637191, 26.86426979415093541, -3.090169943749474069 ) ) ;
#46309 = CARTESIAN_POINT ( 'NONE',  ( 77.23415525214731758, 49.64680416525870044, -15.49634504973622562 ) ) ;
#46310 = SHAPE_REPRESENTATION ( 'Center Base Mounting Screw', ( #68784 ), #26785 ) ;
#46311 = VECTOR ( 'NONE', #41962, 1000.000000000000227 ) ;
#46312 = CARTESIAN_POINT ( 'NONE',  ( 178.6026051973306323, 254.4708812555809345, 5.813106864979912913 ) ) ;
#46313 = CARTESIAN_POINT ( 'NONE',  ( 171.2382477466557305, 255.5321334004109133, 11.22453428535387943 ) ) ;
#46314 = CARTESIAN_POINT ( 'NONE',  ( 194.4417037765285841, 263.4645709469522785, -0.7758984588134626437 ) ) ;
#46315 = ORIENTED_EDGE ( 'NONE', *, *, #74265, .F. ) ;
#46316 = DIRECTION ( 'NONE',  ( -0.8660254037844387076, -0.4999999999999998890, -0.000000000000000000 ) ) ;
#46317 = CARTESIAN_POINT ( 'NONE',  ( 139.6993451667227646, 239.9155109091896065, 2.679491924311254714 ) ) ;
#46318 = CARTESIAN_POINT ( 'NONE',  ( 161.1710432324487954, 255.5389764900634191, -16.30050909083865207 ) ) ;
#46319 = CARTESIAN_POINT ( 'NONE',  ( 12.05626958406300098, 167.7677522451417929, -5.000000000000041744 ) ) ;
#46320 = CARTESIAN_POINT ( 'NONE',  ( 95.60083130504949622, 219.8768266524159856, -9.188101187500093303 ) ) ;
#46321 = CARTESIAN_POINT ( 'NONE',  ( 193.7449971229907533, 267.0691033174243785, -11.57060755736609003 ) ) ;
#46322 = CARTESIAN_POINT ( 'NONE',  ( 174.5292714763907895, 282.4389550827968378, -15.07491654093877287 ) ) ;
#46323 = CARTESIAN_POINT ( 'NONE',  ( 170.1035794950240359, 280.7289576921961611, -14.13142533609434004 ) ) ;
#46324 = EDGE_CURVE ( 'NONE', #97061, #89775, #78499, .T. ) ;
#46325 = CARTESIAN_POINT ( 'NONE',  ( 72.55393231385352237, 70.87694079910581024, 7.622851120052400731 ) ) ;
#46327 = CARTESIAN_POINT ( 'NONE',  ( 106.5950644350847369, 243.8967562850346837, -4.648177544792955347E-16 ) ) ;
#46326 = CARTESIAN_POINT ( 'NONE',  ( -0.8802452050168975139, 179.4869531367911293, 4.594050593750046652 ) ) ;
#46328 = CARTESIAN_POINT ( 'NONE',  ( 187.0158281458424767, 295.8913910117000796, 8.146972701975970566 ) ) ;
#46329 = ORIENTED_EDGE ( 'NONE', *, *, #15389, .T. ) ;
#46330 = AXIS2_PLACEMENT_3D ( 'NONE', #24558, #54955, #47355 ) ;
#46331 = ORIENTED_EDGE ( 'NONE', *, *, #92946, .T. ) ;
#46332 = CARTESIAN_POINT ( 'NONE',  ( 149.8800565769795696, 277.8602840446432083, 1.406115164305642651 ) ) ;
#46333 = CARTESIAN_POINT ( 'NONE',  ( 198.4097421844162170, 265.0824675037606539, -3.039349057205883664 ) ) ;
#46334 = CARTESIAN_POINT ( 'NONE',  ( 85.28648675625211695, 46.08015217243080031, -9.601151076074931012 ) ) ;
#46335 = AXIS2_PLACEMENT_3D ( 'NONE', #8387, #39254, #47372 ) ;
#46336 = B_SPLINE_CURVE_WITH_KNOTS ( 'NONE', 3,
 ( #85364, #23498, #47308, #93961, #31104, #77739, #71137, #40703, #54388, #24013, #32105, #61992, #78732, #24513, #92460, #23005, #38707, #48324, #1740, #32619, #55392, #40196, #15911, #8324, #46815, #15398, #54909, #77221, #100040, #53898, #94454, #63516, #39189, #9322, #25009, #17414, #70103, #79269, #86379, #70611, #93458, #92944, #8815, #9842, #62491, #46292 ),
 .UNSPECIFIED., .F., .F.,
 ( 4, 1, 1, 1, 2, 2, 1, 1, 1, 2, 2, 1, 1, 2, 2, 1, 1, 2, 2, 1, 1, 2, 2, 1, 2, 2, 1, 2, 2, 4 ),
 ( 0.000000000000000000, 0.06250000000000717482, 0.09375000000001090794, 0.1093750000000126149, 0.1171875000000136141, 0.1250000000000146272, 0.1875000000000213163, 0.2187500000000239531, 0.2343750000000244804, 0.2421875000000247580, 0.2500000000000249800, 0.3125000000000254796, 0.3437500000000270339, 0.3593750000000276446, 0.3750000000000282552, 0.4375000000000335842, 0.4687500000000353606, 0.4843750000000357492, 0.5000000000000360822, 0.5625000000000328626, 0.5937500000000315303, 0.6093750000000305311, 0.6250000000000295319, 0.6875000000000242029, 0.7187500000000208722, 0.7500000000000175415, 0.8125000000000122125, 0.8437500000000094369, 0.8750000000000067724, 1.000000000000000000 ),
 .UNSPECIFIED. ) ;
#46337 = LINE ( 'NONE', #77260, #85160 ) ;
#46338 = CARTESIAN_POINT ( 'NONE',  ( 82.38813812040005757, 42.78134201135360115, 7.123226640718979930 ) ) ;
#46339 = CARTESIAN_POINT ( 'NONE',  ( 150.2560907947555791, 276.5831698823408829, 3.693008398856615138 ) ) ;
#46340 = CARTESIAN_POINT ( 'NONE',  ( 25.39882055865594168, 173.2202760586659736, -5.415160957724236172E-17 ) ) ;
#46341 = CARTESIAN_POINT ( 'NONE',  ( 121.2028808523094767, 228.5327760586659451, 1.948934522072303157E-15 ) ) ;
#46342 = DIRECTION ( 'NONE',  ( -0.3297783986044553473, -0.8484238185761712181, 0.4140328874455617147 ) ) ;
#46343 = CARTESIAN_POINT ( 'NONE',  ( 182.9759581861415825, 257.6832614031042112, -2.318740451596759566 ) ) ;
#46344 = ORIENTED_EDGE ( 'NONE', *, *, #60318, .F. ) ;
#46345 = DIRECTION ( 'NONE',  ( -0.8660254037844387076, -0.4999999999999998890, -0.000000000000000000 ) ) ;
#46346 = CARTESIAN_POINT ( 'NONE',  ( 175.2394285866089092, 281.2249514087385478, -15.30553675368379274 ) ) ;
#46347 = CARTESIAN_POINT ( 'NONE',  ( 29.70092825881656751, 40.08080186712595605, -3.090169943749475845 ) ) ;
#46348 = CARTESIAN_POINT ( 'NONE',  ( 195.8947060313465443, 291.3474115503753410, 16.07878593000791767 ) ) ;
#46349 = CARTESIAN_POINT ( 'NONE',  ( 194.0672051292551430, 294.5127359636757660, 15.53337744471869364 ) ) ;
#46350 = CARTESIAN_POINT ( 'NONE',  ( 207.1285138014047504, 271.8898857301724661, -5.752177443817618752 ) ) ;
#46351 = CARTESIAN_POINT ( 'NONE',  ( 81.38957022129915231, 44.58922959300493716, 11.03339234182588413 ) ) ;
#46352 = CARTESIAN_POINT ( 'NONE',  ( 148.2352135776142177, 273.8960739431854563, -9.245976304249309052 ) ) ;
#46353 = CARTESIAN_POINT ( 'NONE',  ( 189.5408823802965230, 263.1112053540622355, 7.934038689971461444 ) ) ;
#46354 = CARTESIAN_POINT ( 'NONE',  ( 164.9640897230306962, 249.8568093354230371, -10.60187880726004650 ) ) ;
#46355 = CARTESIAN_POINT ( 'NONE',  ( 18.14444784528756216, 192.8297689869269504, -2.679491924311252493 ) ) ;
#46356 = CARTESIAN_POINT ( 'NONE',  ( 69.40468783160719113, 69.42147328788952620, 5.860110772957342284 ) ) ;
#46357 = CARTESIAN_POINT ( 'NONE',  ( 189.9457600613112902, 301.6512882219586800, 0.04117870562599101891 ) ) ;
#46358 = CARTESIAN_POINT ( 'NONE',  ( 181.1288997990943699, 267.1128527043363192, -14.76543443481348206 ) ) ;
#46359 = VERTEX_POINT ( 'NONE', #42420 ) ;
#46360 = CARTESIAN_POINT ( 'NONE',  ( 74.07655054661930194, 57.25575122610550949, 16.47418694559453556 ) ) ;
#46361 = CARTESIAN_POINT ( 'NONE',  ( 179.4583960273904211, 270.4090523040318885, 17.47970616590194837 ) ) ;
#46362 = CARTESIAN_POINT ( 'NONE',  ( 98.14495447654879001, 215.2202760586659167, -5.415160957724236172E-17 ) ) ;
#46363 = CARTESIAN_POINT ( 'NONE',  ( 18.23327619575285041, 19.03085787977762067, 9.188101187500006262 ) ) ;
#46364 = CARTESIAN_POINT ( 'NONE',  ( 150.6790040019602088, 269.6633047651677089, 15.38315204620803378 ) ) ;
#46365 = CARTESIAN_POINT ( 'NONE',  ( 77.75856728979914578, 57.69604372946123050, -16.59626237126559900 ) ) ;
#46367 = CARTESIAN_POINT ( 'NONE',  ( 193.0705714787908960, 277.9200196554784839, 16.36204623017445314 ) ) ;
#46366 = CYLINDRICAL_SURFACE ( 'NONE', #64628, 10.00000000000000355 ) ;
#46368 = CARTESIAN_POINT ( 'NONE',  ( -2.330697855141256269, 26.52822386297705393, 10.00000000000000000 ) ) ;
#46369 = DIRECTION ( 'NONE',  ( -1.000000000000000000, 0.000000000000000000, 0.000000000000000000 ) ) ;
#46370 = LINE ( 'NONE', #24089, #28362 ) ;
#46371 = DIRECTION ( 'NONE',  ( 0.9364604334398963781, -0.2023802897980917226, -0.2865031848039421014 ) ) ;
#46372 = DIRECTION ( 'NONE',  ( -0.000000000000000000, -0.000000000000000000, -1.000000000000000000 ) ) ;
#46373 = CARTESIAN_POINT ( 'NONE',  ( 86.15627751966195547, 47.68681392592237955, 10.83869660506637089 ) ) ;
#46374 = EDGE_LOOP ( 'NONE', ( #14920, #82732, #17390, #29764 ) ) ;
#46375 = FACE_OUTER_BOUND ( 'NONE', #15788, .T. ) ;
#46376 = CARTESIAN_POINT ( 'NONE',  ( 30.51038259252555207, 29.56628583063842441, 9.188101187500006262 ) ) ;
#46377 = CARTESIAN_POINT ( 'NONE',  ( 28.46864935082050252, 149.7156766241961350, -37.49999999999994316 ) ) ;
#46378 = AXIS2_PLACEMENT_3D ( 'NONE', #49552, #90093, #96199 ) ;
#46379 = CARTESIAN_POINT ( 'NONE',  ( -27.42236680055714260, 166.5217562850347406, 1.224646799147364892E-15 ) ) ;
#46380 = CARTESIAN_POINT ( 'NONE',  ( 196.4808189786114951, 290.3322341467384717, -17.84817245450773271 ) ) ;
#46381 = ORIENTED_EDGE ( 'NONE', *, *, #54575, .F. ) ;
#46382 = B_SPLINE_SURFACE_WITH_KNOTS ( 'NONE', 3, 1, ( 
 ( #9112, #32409 ),
 ( #77000, #85150 ),
 ( #7608, #34285 ),
 ( #77528, #38495 ),
 ( #3411, #63306 ),
 ( #513, #57070 ),
 ( #70405, #1013 ),
 ( #78023, #96130 ),
 ( #88051, #31400 ),
 ( #23, #46593 ),
 ( #18599, #86173 ),
 ( #49478, #69412 ),
 ( #23799, #54685 ),
 ( #61796, #92742 ),
 ( #38994, #85671 ),
 ( #16209, #11008 ),
 ( #16706, #47102 ),
 ( #47599, #8613 ),
 ( #41881, #72819 ),
 ( #65182, #26684 ),
 ( #32612, #63508 ),
 ( #18427, #50301 ),
 ( #72643, #69730 ),
 ( #96453, #88377 ),
 ( #81253, #95474 ),
 ( #65017, #11341 ),
 ( #26523, #1732 ),
 ( #64517, #73133 ),
 ( #57903, #26027 ),
 ( #33110, #56897 ),
 ( #9833, #94447 ),
 ( #49316, #40694 ),
 ( #41698, #18932 ),
 ( #80255, #86874 ) ),
 .UNSPECIFIED., .T., .F., .F.,
 ( 4, 2, 2, 2, 2, 2, 2, 2, 2, 2, 2, 2, 2, 2, 2, 2, 4 ),
 ( 2, 2 ),
 ( 0.000000000000000000, 0.06250000000000000000, 0.1250000000000000000, 0.1875000000000000000, 0.2500000000000000000, 0.3125000000000000000, 0.3750000000000000000, 0.4375000000000000000, 0.5000000000000000000, 0.5625000000000000000, 0.6250000000000000000, 0.6875000000000000000, 0.7500000000000000000, 0.8125000000000000000, 0.8750000000000000000, 0.9375000000000000000, 1.000000000000000000 ),
 ( 0.000000000000000000, 1.000000000000000000 ),
 .UNSPECIFIED. ) ;
#46383 = EDGE_CURVE ( 'NONE', #7164, #5821, #12052, .T. ) ;
#46384 = VECTOR ( 'NONE', #6209, 1000.000000000000000 ) ;
#46385 = CARTESIAN_POINT ( 'NONE',  ( 152.8230551641381396, 275.2333800586559391, 10.94291057119876420 ) ) ;
#46386 = CARTESIAN_POINT ( 'NONE',  ( 79.06941788075492639, 49.65996601992884507, 14.60823914099390919 ) ) ;
#46387 = CARTESIAN_POINT ( 'NONE',  ( 194.3209714950976945, 287.2951553348708558, -17.43383849888540027 ) ) ;
#46388 = ADVANCED_FACE ( 'NONE', ( #73353 ), #34824, .F. ) ;
#46389 = LINE ( 'NONE', #39282, #76023 ) ;
#46390 = CARTESIAN_POINT ( 'NONE',  ( 153.1164404339926080, 265.4415410246681972, 16.15325778160653414 ) ) ;
#46391 = B_SPLINE_CURVE_WITH_KNOTS ( 'NONE', 3,
 ( #99000, #30580, #16376, #52872 ),
 .UNSPECIFIED., .F., .F.,
 ( 4, 4 ),
 ( 0.01049495788375092234, 0.01588891246743844368 ),
 .UNSPECIFIED. ) ;
#46392 = EDGE_LOOP ( 'NONE', ( #38136, #52147, #58028, #52640 ) ) ;
#46393 = CARTESIAN_POINT ( 'NONE',  ( 188.0737869051473012, 299.5124861214166572, -3.734995909225475863 ) ) ;
#46394 = EDGE_CURVE ( 'NONE', #3492, #42198, #19978, .T. ) ;
#46395 = CARTESIAN_POINT ( 'NONE',  ( 37.18115723113500337, 22.26216523072496400, -2.296566073217252530E-15 ) ) ;
#46396 = ORIENTED_EDGE ( 'NONE', *, *, #96408, .T. ) ;
#46397 = DIRECTION ( 'NONE',  ( -0.8660254037844387076, -0.4999999999999998890, -0.000000000000000000 ) ) ;
#46398 = EDGE_CURVE ( 'NONE', #20684, #89824, #21843, .T. ) ;
#46399 = DIRECTION ( 'NONE',  ( -0.4897629171537585258, 0.8718556560469402639, 0.000000000000000000 ) ) ;
#46400 = ORIENTED_EDGE ( 'NONE', *, *, #14043, .F. ) ;
#46401 = CARTESIAN_POINT ( 'NONE',  ( 86.53662601515709696, 47.28685775360474253, -10.20020400134509408 ) ) ;
#46402 = LINE ( 'NONE', #83971, #49218 ) ;
#46403 = CARTESIAN_POINT ( 'NONE',  ( 84.51504024060453446, 50.21520769139153373, 13.87897165174792846 ) ) ;
#46404 = CARTESIAN_POINT ( 'NONE',  ( 154.1166010273282438, 263.7092120612824147, -17.33440268030034304 ) ) ;
#46405 = CARTESIAN_POINT ( 'NONE',  ( 167.5861325596884797, 256.5095974891418109, 15.03189046419509367 ) ) ;
#46406 = VECTOR ( 'NONE', #7350, 1000.000000000000000 ) ;
#46407 = CARTESIAN_POINT ( 'NONE',  ( 42.15722797529793553, 32.84335787977767041, 9.188101187500006262 ) ) ;
#46408 = VECTOR ( 'NONE', #51716, 1000.000000000000000 ) ;
#46409 = CARTESIAN_POINT ( 'NONE',  ( 197.3327212804159103, 267.5970440452412049, 9.861675131224707513 ) ) ;
#46410 = EDGE_LOOP ( 'NONE', ( #7065, #9573, #21198, #73495 ) ) ;
#46411 = CARTESIAN_POINT ( 'NONE',  ( 202.5650245025327081, 277.7940810556053179, -15.59262966521933791 ) ) ;
#46412 = VECTOR ( 'NONE', #3597, 1000.000000000000000 ) ;
#46413 = ORIENTED_EDGE ( 'NONE', *, *, #67437, .F. ) ;
#46414 = ORIENTED_EDGE ( 'NONE', *, *, #74352, .T. ) ;
#46415 = CARTESIAN_POINT ( 'NONE',  ( 172.3434955255090699, 270.7759313641087715, 16.44516896573899345 ) ) ;
#46416 = ORIENTED_EDGE ( 'NONE', *, *, #3450, .T. ) ;
#46417 = CARTESIAN_POINT ( 'NONE',  ( 164.7580746839756785, 246.2315630300633131, 2.864679634845263223 ) ) ;
#46418 = CARTESIAN_POINT ( 'NONE',  ( 205.9226911964632052, 273.9784317468465815, -10.54881836492553404 ) ) ;
#46419 = CARTESIAN_POINT ( 'NONE',  ( 197.4711460630325632, 273.2607306827283651, -13.37816035555838035 ) ) ;
#46420 = LINE ( 'NONE', #79389, #62578 ) ;
#46421 = CARTESIAN_POINT ( 'NONE',  ( 147.1125781744767949, 275.8405354997948962, -5.216646253929903665 ) ) ;
#46422 = CARTESIAN_POINT ( 'NONE',  ( 167.7614935370554008, 249.2934080693781027, -5.466447205817170030 ) ) ;
#46423 = CARTESIAN_POINT ( 'NONE',  ( 52.99401211233780629, 194.7365022471902307, 10.00000000000009948 ) ) ;
#46424 = CARTESIAN_POINT ( 'NONE',  ( 186.5050373472817284, 286.7230076623727086, -15.46505519963496589 ) ) ;
#46425 = CARTESIAN_POINT ( 'NONE',  ( 116.0067284296028589, 225.5327760586659451, 1.948934522072303157E-15 ) ) ;
#46426 = CARTESIAN_POINT ( 'NONE',  ( 185.3936501019832406, 261.9788283115297531, -9.055590929688063895 ) ) ;
#46427 = CARTESIAN_POINT ( 'NONE',  ( 42.00264329202813229, 26.11110640527295601, -2.839279412974138328 ) ) ;
#46428 = CARTESIAN_POINT ( 'NONE',  ( 177.3729564342710034, 288.8709971325815786, -9.341937108417035063 ) ) ;
#46429 = ORIENTED_EDGE ( 'NONE', *, *, #40480, .F. ) ;
#46430 = CARTESIAN_POINT ( 'NONE',  ( 73.98570270871887544, 68.92876820612472955, -11.10152750440661862 ) ) ;
#46431 = CARTESIAN_POINT ( 'NONE',  ( 75.56481254617771981, 62.80431594364750936, -14.94990648061137328 ) ) ;
#46432 = DIRECTION ( 'NONE',  ( -0.8653701635463872943, 0.5011331959107268030, 0.000000000000000000 ) ) ;
#46433 = CARTESIAN_POINT ( 'NONE',  ( 196.3021893095863959, 290.6416298092292436, 17.45656988653421138 ) ) ;
#46434 = CARTESIAN_POINT ( 'NONE',  ( 72.24607194888514528, 62.62084493799169138, 14.18516964437414352 ) ) ;
#46435 = CARTESIAN_POINT ( 'NONE',  ( 66.73387148584731676, 68.35900400491371443, 4.521128723796655535 ) ) ;
#46436 = CARTESIAN_POINT ( 'NONE',  ( 177.1640229826661823, 288.7756000595433079, -9.303873556051240001 ) ) ;
#46437 = ORIENTED_EDGE ( 'NONE', *, *, #34876, .T. ) ;
#46438 = CARTESIAN_POINT ( 'NONE',  ( 36.61341721041482344, 22.10801979619931501, 3.090169943749476733 ) ) ;
#46439 = ORIENTED_EDGE ( 'NONE', *, *, #54078, .F. ) ;
#46440 = CARTESIAN_POINT ( 'NONE',  ( 148.4042165687623083, 273.6033521758856750, -8.709765892313745539 ) ) ;
#46441 = CARTESIAN_POINT ( 'NONE',  ( 46.40065236557224893, 186.0494855054051868, -2.679491924311248496 ) ) ;
#46442 = ORIENTED_EDGE ( 'NONE', *, *, #86538, .T. ) ;
#46443 = CARTESIAN_POINT ( 'NONE',  ( 188.0248464885530666, 266.0881402788382388, -11.75859168027853840 ) ) ;
#46444 = CARTESIAN_POINT ( 'NONE',  ( 157.5254383281065600, 276.9205291671078157, 10.24548677782836670 ) ) ;
#46445 = CARTESIAN_POINT ( 'NONE',  ( 192.5542622421363603, 262.6158310691380962, 4.646693819196449304 ) ) ;
#46446 = CARTESIAN_POINT ( 'NONE',  ( 187.8362272217282509, 287.5474138042418417, -16.31275406728138933 ) ) ;
#46448 = EDGE_CURVE ( 'NONE', #63646, #93711, #88107, .T. ) ;
#46447 = VECTOR ( 'NONE', #53474, 1000.000000000000000 ) ;
#46449 = CARTESIAN_POINT ( 'NONE',  ( 15.10771242554802463, 167.9824982072973967, -5.229199737892075682E-14 ) ) ;
#46451 = PLANE ( 'NONE',  #26956 ) ;
#46450 = CARTESIAN_POINT ( 'NONE',  ( 185.4082111984200765, 289.5490485375350431, -13.24228234091079592 ) ) ;
#46452 = CARTESIAN_POINT ( 'NONE',  ( 200.8665851640556070, 282.7358642834317948, -16.69422397739980823 ) ) ;
#46453 = ORIENTED_EDGE ( 'NONE', *, *, #58740, .F. ) ;
#46455 = CARTESIAN_POINT ( 'NONE',  ( 190.9559560067148425, 299.9015775189195665, -4.895152914295826108 ) ) ;
#46454 = AXIS2_PLACEMENT_3D ( 'NONE', #18867, #11278, #64960 ) ;
#46456 = CARTESIAN_POINT ( 'NONE',  ( 73.01434170154392689, 67.59968775764829729, 11.23568329902283125 ) ) ;
#46457 = CARTESIAN_POINT ( 'NONE',  ( 190.5138415335236743, 260.7340691433176971, 3.969352497929276691 ) ) ;
#46458 = CARTESIAN_POINT ( 'NONE',  ( 183.2115438791051645, 276.4014300552622672, -16.48630945905322776 ) ) ;
#46459 = CARTESIAN_POINT ( 'NONE',  ( 9.004826742577897392, 187.5530062829863027, -4.648177544792955347E-16 ) ) ;
#46460 = CARTESIAN_POINT ( 'NONE',  ( -19.65312891409030271, 93.06504152958497400, 59.99999999999999289 ) ) ;
#46461 = CARTESIAN_POINT ( 'NONE',  ( 185.3661735032551974, 296.9378314866745541, -4.315971704415366261 ) ) ;
#46462 = CARTESIAN_POINT ( 'NONE',  ( 83.50657803916486444, 43.71961979256885655, 7.634715688034919623 ) ) ;
#46463 = CARTESIAN_POINT ( 'NONE',  ( 75.43017357788674815, 188.3759306620403891, -30.52142883766498116 ) ) ;
#46464 = AXIS2_PLACEMENT_3D ( 'NONE', #52190, #92250, #99317 ) ;
#46465 = DIRECTION ( 'NONE',  ( -0.9997524133706772176, 0.02225111142182466945, 0.000000000000000000 ) ) ;
#46466 = CARTESIAN_POINT ( 'NONE',  ( 70.47935399718505778, 60.87681273810773064, -14.99835320260665306 ) ) ;
#46467 = CARTESIAN_POINT ( 'NONE',  ( 75.63268008801900066, 65.14737934564519151, -14.41129995628930516 ) ) ;
#46468 = CARTESIAN_POINT ( 'NONE',  ( 70.81050702595493362, 217.8149278399160664, 9.188101187500093303 ) ) ;
#46469 = FACE_OUTER_BOUND ( 'NONE', #9436, .T. ) ;
#46470 = CARTESIAN_POINT ( 'NONE',  ( 192.5551423381268989, 297.1317055421444024, -13.20528585388119858 ) ) ;
#46471 = CARTESIAN_POINT ( 'NONE',  ( 51.98364914125591696, 207.4865022471903160, 10.00000000000009415 ) ) ;
#46472 = EDGE_CURVE ( 'NONE', #55984, #58170, #84061, .T. ) ;
#46473 = CARTESIAN_POINT ( 'NONE',  ( 155.4810912439522212, 261.3458456796594760, -18.44218279064527266 ) ) ;
#46474 = CARTESIAN_POINT ( 'NONE',  ( 161.4816992964961742, 250.9524876563463067, -12.92750327687364198 ) ) ;
#46475 = CARTESIAN_POINT ( 'NONE',  ( 84.78922593834768406, 50.40041394048158452, -13.47278310779192623 ) ) ;
#46476 = CIRCLE ( 'NONE', #90225, 0.1418229129684159262 ) ;
#46477 = CYLINDRICAL_SURFACE ( 'NONE', #59784, 17.82106496071139645 ) ;
#46479 = CARTESIAN_POINT ( 'NONE',  ( 75.97679052025780777, 51.38226631630038810, 16.15713118531126469 ) ) ;
#46478 = CARTESIAN_POINT ( 'NONE',  ( 104.2879750871056928, 231.0177522451418781, -10.00000000000009592 ) ) ;
#46480 = LINE ( 'NONE', #53585, #85461 ) ;
#46481 = DIRECTION ( 'NONE',  ( 0.7499999999999997780, 0.4330127018922197979, 0.5000000000000000000 ) ) ;
#46482 = CARTESIAN_POINT ( 'NONE',  ( 164.2035862026529287, 246.2380412424262204, -4.285327505657965830 ) ) ;
#46483 = CARTESIAN_POINT ( 'NONE',  ( 195.8449251089225811, 291.4336346372613775, 16.14492769602857081 ) ) ;
#46484 = CARTESIAN_POINT ( 'NONE',  ( 71.64065041137482126, 72.08859242525181799, 3.376608021325395725 ) ) ;
#46485 = DIRECTION ( 'NONE',  ( -0.7696402260561131525, -0.6384778167143280170, 0.000000000000000000 ) ) ;
#46486 = CARTESIAN_POINT ( 'NONE',  ( 41.01373370305532973, 203.6744531367911293, 4.594050593750047540 ) ) ;
#46487 = VECTOR ( 'NONE', #3888, 1000.000000000000000 ) ;
#46488 = CARTESIAN_POINT ( 'NONE',  ( 49.86334402403631572, 211.8464784336661637, 1.353441290958777327E-15 ) ) ;
#46489 = CARTESIAN_POINT ( 'NONE',  ( 70.62955678152276562, 60.80479719363771807, -15.06269029744276011 ) ) ;
#46490 = CARTESIAN_POINT ( 'NONE',  ( 88.31734708748101070, 44.16587181541018481, 0.3721755419053404124 ) ) ;
#46491 = CARTESIAN_POINT ( 'NONE',  ( 166.8965953329662568, 259.4083194189263963, 16.50658842888446642 ) ) ;
#46492 = CARTESIAN_POINT ( 'NONE',  ( 148.6720373546558847, 247.4548013555409796, -4.594050593750042211 ) ) ;
#46493 = CARTESIAN_POINT ( 'NONE',  ( 200.0612311737130540, 271.1040812139211198, -11.28087083430611592 ) ) ;
#46494 = CARTESIAN_POINT ( 'NONE',  ( 32.30976433484754295, 19.44966523072496045, -2.296566073217252530E-15 ) ) ;
#46495 = DIRECTION ( 'NONE',  ( 0.5000000000000014433, -0.8660254037844378194, 0.000000000000000000 ) ) ;
#46496 = CARTESIAN_POINT ( 'NONE',  ( 80.85352406992397789, 47.50882711102294564, -12.96424570248204944 ) ) ;
#46497 = CARTESIAN_POINT ( 'NONE',  ( 10.20631340951632104, 27.93396525600388713, 2.839279412974139660 ) ) ;
#46498 = CARTESIAN_POINT ( 'NONE',  ( 67.02199298016300588, 203.3768266524159856, -9.188101187500093303 ) ) ;
#46499 = CARTESIAN_POINT ( 'NONE',  ( 77.32817876982274186, 63.13942984521013813, 15.61058464551961933 ) ) ;
#46500 = CARTESIAN_POINT ( 'NONE',  ( 82.60582504534620796, 54.05721848903051807, -15.51501040363680772 ) ) ;
#46501 = CARTESIAN_POINT ( 'NONE',  ( 198.2414483977475754, 287.2827345394944700, 16.94931984969033678 ) ) ;
#46502 = CARTESIAN_POINT ( 'NONE',  ( 45.66470909604093720, 114.5311720768849995, -10.00000000000000000 ) ) ;
#46503 = CARTESIAN_POINT ( 'NONE',  ( 153.3323608220152607, 276.8159399788930273, 7.221710064476104307 ) ) ;
#46504 = EDGE_CURVE ( 'NONE', #66013, #64000, #99824, .T. ) ;
#46505 = DIRECTION ( 'NONE',  ( 1.000000000000000000, 0.000000000000000000, 0.000000000000000000 ) ) ;
#46506 = CARTESIAN_POINT ( 'NONE',  ( 118.8119427999551760, 232.7365022471901739, -10.00000000000009059 ) ) ;
#46507 = CARTESIAN_POINT ( 'NONE',  ( 161.7587802986029999, 250.4725692828850754, 14.33336164792646450 ) ) ;
#46508 = CARTESIAN_POINT ( 'NONE',  ( 206.8968397926183229, 272.2911568841838061, 7.145103750817420440 ) ) ;
#46509 = ORIENTED_EDGE ( 'NONE', *, *, #14609, .F. ) ;
#46510 = CARTESIAN_POINT ( 'NONE',  ( 77.55434755293194371, 49.25411156172739879, 15.29420696795023993 ) ) ;
#46511 = CARTESIAN_POINT ( 'NONE',  ( 82.73238768416140942, 53.97435551261711595, 15.47794029334955290 ) ) ;
#46512 = ORIENTED_EDGE ( 'NONE', *, *, #65746, .F. ) ;
#46513 = CARTESIAN_POINT ( 'NONE',  ( 159.2122473525774069, 254.8832937285494609, -16.22689353966294590 ) ) ;
#46514 = CARTESIAN_POINT ( 'NONE',  ( 194.2437465966334571, 293.7439872100536036, 14.26449127607053313 ) ) ;
#46515 = CARTESIAN_POINT ( 'NONE',  ( 71.60825314380221585, 68.87726608393772665, -8.959588779531696190 ) ) ;
#46516 = EDGE_CURVE ( 'NONE', #39570, #71517, #86597, .T. ) ;
#46517 = ORIENTED_EDGE ( 'NONE', *, *, #32855, .F. ) ;
#46518 = CARTESIAN_POINT ( 'NONE',  ( 173.3536786335043587, 251.5408331122485208, 0.1975630382450959399 ) ) ;
#46519 = ORIENTED_EDGE ( 'NONE', *, *, #32298, .T. ) ;
#46520 = CARTESIAN_POINT ( 'NONE',  ( 79.47501604884325843, 46.39112505788885699, -12.72631656372365327 ) ) ;
#46521 = CARTESIAN_POINT ( 'NONE',  ( 194.7900911235093133, 293.2606606935473792, -14.66228443412922999 ) ) ;
#46522 = ORIENTED_EDGE ( 'NONE', *, *, #79482, .F. ) ;
#46523 = CIRCLE ( 'NONE', #75704, 70.00000000000001421 ) ;
#46524 = CARTESIAN_POINT ( 'NONE',  ( 22.11595037535113661, 30.95586893147756413, 7.433330006724141015 ) ) ;
#46525 = CARTESIAN_POINT ( 'NONE',  ( 75.35044267779828431, 56.47610766855712683, 16.13648771087090950 ) ) ;
#46526 = CARTESIAN_POINT ( 'NONE',  ( 153.8774496355958661, 270.8400042090240163, -14.95803277361719097 ) ) ;
#46527 = CARTESIAN_POINT ( 'NONE',  ( 74.86346538573357634, 67.47285165321517297, -12.74145591711592296 ) ) ;
#46528 = VERTEX_POINT ( 'NONE', #64647 ) ;
#46529 = DIRECTION ( 'NONE',  ( 0.000000000000000000, 0.000000000000000000, 1.000000000000000000 ) ) ;
#46530 = CARTESIAN_POINT ( 'NONE',  ( 44.18536904650256503, 64.34838820550514527, 10.00000000000000000 ) ) ;
#46531 = VERTEX_POINT ( 'NONE', #95596 ) ;
#46532 = CYLINDRICAL_SURFACE ( 'NONE', #16867, 70.00000000000002842 ) ;
#46533 = CIRCLE ( 'NONE', #48135, 70.00000000000001421 ) ;
#46535 = CARTESIAN_POINT ( 'NONE',  ( 67.93659143534979705, 65.44611157119403799, -10.36544933898279552 ) ) ;
#46534 = CARTESIAN_POINT ( 'NONE',  ( 68.07754589302088277, 65.45337442352710866, 10.44018349253913946 ) ) ;
#46536 = CARTESIAN_POINT ( 'NONE',  ( 162.8480293090835005, 248.5859346546387769, -9.753154585358942086 ) ) ;
#46537 = CARTESIAN_POINT ( 'NONE',  ( 164.0777181605478745, 246.4560510864015441, 5.763760713451748785 ) ) ;
#46538 = CARTESIAN_POINT ( 'NONE',  ( 198.2819808855875863, 287.2125302111982705, 18.53535247371401695 ) ) ;
#46539 = CARTESIAN_POINT ( 'NONE',  ( 157.8159121039657293, 257.3018173235443555, -17.05074702406642118 ) ) ;
#46540 = CARTESIAN_POINT ( 'NONE',  ( 147.0210896547505399, 249.5643266524160140, 9.188101187500095079 ) ) ;
#46541 = CARTESIAN_POINT ( 'NONE',  ( 163.9868517627649283, 262.4765967983332757, 17.63283070717088208 ) ) ;
#46542 = CIRCLE ( 'NONE', #80597, 70.00000000000001421 ) ;
#46543 = CARTESIAN_POINT ( 'NONE',  ( 195.5194402673059528, 290.4564941404553338, -16.58695021901899125 ) ) ;
#46544 = B_SPLINE_CURVE_WITH_KNOTS ( 'NONE', 3,
 ( #14673, #76484, #7061, #37943 ),
 .UNSPECIFIED., .F., .F.,
 ( 4, 4 ),
 ( 0.03315600111831654845, 0.04206725051739886034 ),
 .UNSPECIFIED. ) ;
#46545 = CARTESIAN_POINT ( 'NONE',  ( 72.54255783352381570, 218.8149278399160664, -9.188101187500095079 ) ) ;
#46547 = ORIENTED_EDGE ( 'NONE', *, *, #60001, .T. ) ;
#46546 = B_SPLINE_CURVE_WITH_KNOTS ( 'NONE', 3,
 ( #59721, #92183, #53127, #90687 ),
 .UNSPECIFIED., .F., .F.,
 ( 4, 4 ),
 ( 0.008574140209404586613, 0.01493074025973913956 ),
 .UNSPECIFIED. ) ;
#46548 = CARTESIAN_POINT ( 'NONE',  ( 151.3284628043366524, 268.5384091220288383, 14.49047510809488237 ) ) ;
#46549 = CARTESIAN_POINT ( 'NONE',  ( 183.8301289239822722, 272.2411597453489662, -17.34995410509954183 ) ) ;
#46550 = ORIENTED_EDGE ( 'NONE', *, *, #13163, .F. ) ;
#46551 = AXIS2_PLACEMENT_3D ( 'NONE', #44060, #74512, #35971 ) ;
#46552 = CARTESIAN_POINT ( 'NONE',  ( 189.6666044902458168, 284.7049877867155487, 17.41007887138588117 ) ) ;
#46553 = ORIENTED_EDGE ( 'NONE', *, *, #64872, .F. ) ;
#46554 = EDGE_LOOP ( 'NONE', ( #73114, #38967, #46198, #39452 ) ) ;
#46555 = CARTESIAN_POINT ( 'NONE',  ( 66.87731416404506035, 67.95854068482356070, 6.988359128739752180 ) ) ;
#46556 = CARTESIAN_POINT ( 'NONE',  ( 197.9002110616137884, 286.8208446428124034, 16.93415638934909495 ) ) ;
#46557 = CARTESIAN_POINT ( 'NONE',  ( 191.7247331938518187, 298.5700163710982338, -9.650650827884682315 ) ) ;
#46558 = LINE ( 'NONE', #68864, #33688 ) ;
#46559 = CARTESIAN_POINT ( 'NONE',  ( 77.79060403590699480, 49.02752842191024030, -14.64657546086520590 ) ) ;
#46560 = FACE_OUTER_BOUND ( 'NONE', #99022, .T. ) ;
#46561 = CARTESIAN_POINT ( 'NONE',  ( 84.66726058227095564, 213.5643266524160140, 9.188101187500095079 ) ) ;
#46562 = ORIENTED_EDGE ( 'NONE', *, *, #93239, .F. ) ;
#46563 = AXIS2_PLACEMENT_3D ( 'NONE', #1919, #63710, #16109 ) ;
#46564 = ORIENTED_EDGE ( 'NONE', *, *, #2405, .T. ) ;
#46565 = FACE_OUTER_BOUND ( 'NONE', #83868, .T. ) ;
#46566 = ORIENTED_EDGE ( 'NONE', *, *, #93120, .F. ) ;
#46567 = CARTESIAN_POINT ( 'NONE',  ( 76.36355602522917252, 51.65656375226136987, -16.16753059234807566 ) ) ;
#46568 = CARTESIAN_POINT ( 'NONE',  ( 76.25827818320625795, 65.17332737998212622, -14.17717953946896436 ) ) ;
#46569 = CARTESIAN_POINT ( 'NONE',  ( 164.5813345449211624, 245.5837619211427523, 1.447064457712487373 ) ) ;
#46570 = EDGE_CURVE ( 'NONE', #43346, #40913, #830, .T. ) ;
#46571 = CARTESIAN_POINT ( 'NONE',  ( -32.03049420854435425, 93.46753386908051198, 43.95878507283718761 ) ) ;
#46572 = CARTESIAN_POINT ( 'NONE',  ( 98.80083580102481733, 239.3967562850347122, -4.648177544792955347E-16 ) ) ;
#46573 = LINE ( 'NONE', #23781, #30230 ) ;
#46574 = ORIENTED_EDGE ( 'NONE', *, *, #90749, .T. ) ;
#46575 = CARTESIAN_POINT ( 'NONE',  ( 83.28364122651360901, 43.66763108505107027, -7.749604338574708429 ) ) ;
#46576 = CARTESIAN_POINT ( 'NONE',  ( 185.9340259846279650, 259.2058230038674083, 6.068042760456333617 ) ) ;
#46577 = ADVANCED_FACE ( 'NONE', ( #78856 ), #8438, .F. ) ;
#46578 = CARTESIAN_POINT ( 'NONE',  ( 33.51440821012886317, 31.30066082961424456, -10.00000000000000533 ) ) ;
#46579 = CARTESIAN_POINT ( 'NONE',  ( 200.9445292274600092, 282.6008612054670266, -16.62830946367346741 ) ) ;
#46580 = CARTESIAN_POINT ( 'NONE',  ( 72.45510692969175182, 70.78848362686431983, 7.675293421552856543 ) ) ;
#46581 = PLANE ( 'NONE',  #85885 ) ;
#46582 = VERTEX_POINT ( 'NONE', #78351 ) ;
#46583 = CARTESIAN_POINT ( 'NONE',  ( 199.8090841209456698, 266.6002589468719748, 4.696852429360418135 ) ) ;
#46584 = CARTESIAN_POINT ( 'NONE',  ( 181.8671909181005333, 291.4740761920108412, 9.945688837270767024 ) ) ;
#46585 = DIRECTION ( 'NONE',  ( -0.2502735827033141236, -0.9681751565707764628, 0.000000000000000000 ) ) ;
#46586 = VECTOR ( 'NONE', #81579, 1000.000000000000114 ) ;
#46587 = CARTESIAN_POINT ( 'NONE',  ( 185.1689866119487249, 264.3216279136979665, -12.02713122612823504 ) ) ;
#46588 = CARTESIAN_POINT ( 'NONE',  ( -44.30466402961319972, 27.54938068083718861, -10.00000000000000000 ) ) ;
#46589 = ADVANCED_FACE ( 'NONE', ( #72259 ), #19030, .F. ) ;
#46590 = CARTESIAN_POINT ( 'NONE',  ( -50.24117156905492720, 92.72553494444620981, 36.50000000000000000 ) ) ;
#46591 = ORIENTED_EDGE ( 'NONE', *, *, #27213, .F. ) ;
#46592 = DIRECTION ( 'NONE',  ( 0.000000000000000000, 0.000000000000000000, 1.000000000000000000 ) ) ;
#46593 = CARTESIAN_POINT ( 'NONE',  ( 162.6220573360242270, 248.9773295930640131, 10.49878733418918486 ) ) ;
#46594 = AXIS2_PLACEMENT_3D ( 'NONE', #3240, #34605, #65503 ) ;
#46595 = AXIS2_PLACEMENT_3D ( 'NONE', #3496, #42451, #33900 ) ;
#46596 = DIRECTION ( 'NONE',  ( 0.02977611660965746171, -0.9995565931350001154, 0.000000000000000000 ) ) ;
#46598 = CARTESIAN_POINT ( 'NONE',  ( 73.95246095525199337, 55.20797954095843352, 16.12289266927081854 ) ) ;
#46597 = CARTESIAN_POINT ( 'NONE',  ( 155.5770330754656072, 261.1796695529068302, 18.26969263326161297 ) ) ;
#46599 = CARTESIAN_POINT ( 'NONE',  ( 178.7764833861777163, 287.8890986131111731, -12.93556640157745719 ) ) ;
#46600 = APPLICATION_CONTEXT ( 'automotive_design' ) ;
#46601 = CARTESIAN_POINT ( 'NONE',  ( 24.67798091686682938, 37.18080186712595037, 3.090169943749475401 ) ) ;
#46602 = EDGE_CURVE ( 'NONE', #82505, #63013, #20275, .T. ) ;
#46603 = CARTESIAN_POINT ( 'NONE',  ( 168.6924467145065307, 273.0555373943842028, 15.94676933137322372 ) ) ;
#46604 = CARTESIAN_POINT ( 'NONE',  ( 163.3442030120103823, 283.7586793589214267, -3.186042431646216588 ) ) ;
#46605 = CARTESIAN_POINT ( 'NONE',  ( 67.69237348538018750, 66.82088825431439716, 8.559571887000263501 ) ) ;
#46606 = CARTESIAN_POINT ( 'NONE',  ( 189.7858391559284428, 261.6244128272988974, 2.876109323323718492 ) ) ;
#46607 = VECTOR ( 'NONE', #45773, 1000.000000000000000 ) ;
#46608 =( BOUNDED_CURVE ( )  B_SPLINE_CURVE ( 2, ( #16796, #56792, #72529, #94339, #41078, #24894, #86762, #17296, #72015 ),
 .UNSPECIFIED., .F., .T. ) 
 B_SPLINE_CURVE_WITH_KNOTS ( ( 3, 2, 2, 2, 3 ),
 ( 0.7379032258064516236, 0.7392473118279569988, 0.7419354838709677491, 0.7446236559139784994, 0.7459677419354838745 ),
 .UNSPECIFIED. ) 
 CURVE ( )  GEOMETRIC_REPRESENTATION_ITEM ( )  RATIONAL_B_SPLINE_CURVE ( ( 0.9330127018922194093, 0.9330127018922194093, 1.000000000000000000, 0.8660254037844387076, 1.000000000000000000, 0.8660254037844387076, 1.000000000000000000, 0.9330127018922194093, 0.9330127018922194093 ) ) 
 REPRESENTATION_ITEM ( '' )  );
#46609 = CARTESIAN_POINT ( 'NONE',  ( -9.405095999578703569, 171.5024278399160949, 9.188101187500095079 ) ) ;
#46610 = CARTESIAN_POINT ( 'NONE',  ( 190.7050128886200753, 296.3700851971329939, -11.76232993392748583 ) ) ;
#46611 = VERTEX_POINT ( 'NONE', #57522 ) ;
#46612 = CARTESIAN_POINT ( 'NONE',  ( 174.9397293896797976, 255.2796731743772796, 8.271871831370619432 ) ) ;
#46613 = CARTESIAN_POINT ( 'NONE',  ( 73.10686818167350509, 70.63172961811761752, -7.803365976151034111 ) ) ;
#46614 = CARTESIAN_POINT ( 'NONE',  ( 202.4695312440243526, 274.0310513324629937, -13.04997687495370684 ) ) ;
#46615 = FACE_OUTER_BOUND ( 'NONE', #28646, .T. ) ;
#46616 = CARTESIAN_POINT ( 'NONE',  ( 25.77718602916411328, 191.8149278399160949, -9.188101187500095079 ) ) ;
#46617 = CARTESIAN_POINT ( 'NONE',  ( 77.08262651433446422, 63.62497865693946153, -15.40261155718560815 ) ) ;
#46618 = CARTESIAN_POINT ( 'NONE',  ( 178.9869515928023986, 273.9622273161898534, -16.75238912495000676 ) ) ;
#46619 = CARTESIAN_POINT ( 'NONE',  ( 26.78025984663613457, 31.16454794089042224, -10.00000000000000355 ) ) ;
#46620 = CARTESIAN_POINT ( 'NONE',  ( 82.65091073267497279, 41.67014845218071173, -4.206092679686253888 ) ) ;
#46621 = CARTESIAN_POINT ( 'NONE',  ( 170.4904982756437732, 270.9068794242204490, -16.80084387905754895 ) ) ;
#46622 = CARTESIAN_POINT ( 'NONE',  ( 81.25383428119911855, 56.17809469613565909, 16.10000759051138175 ) ) ;
#46623 = B_SPLINE_SURFACE_WITH_KNOTS ( 'NONE', 3, 1, ( 
 ( #94331, #77612 ),
 ( #30492, #46165 ),
 ( #31978, #1614 ),
 ( #8196, #61381 ),
 ( #53769, #61871 ),
 ( #92823, #46685 ),
 ( #9718, #87275 ),
 ( #26402, #19325 ),
 ( #25389, #11217 ),
 ( #42084, #65387 ),
 ( #41580, #50188 ),
 ( #56277, #4085 ),
 ( #64394, #72521 ),
 ( #3130, #41068 ),
 ( #79137, #95357 ),
 ( #49205, #89256 ),
 ( #72006, #25912 ),
 ( #95846, #2610 ),
 ( #17805, #81141 ),
 ( #34976, #26899 ),
 ( #34015, #57279 ),
 ( #32985, #71514 ),
 ( #63889, #48705 ),
 ( #11707, #64900 ),
 ( #58280, #88255 ),
 ( #10205, #48190 ),
 ( #88753, #49685 ),
 ( #40573, #96834 ),
 ( #96329, #18802 ),
 ( #10702, #33498 ),
 ( #65880, #2104 ),
 ( #80640, #73016 ),
 ( #56784, #79638 ),
 ( #3608, #27399 ) ),
 .UNSPECIFIED., .T., .F., .F.,
 ( 4, 2, 2, 2, 2, 2, 2, 2, 2, 2, 2, 2, 2, 2, 2, 2, 4 ),
 ( 2, 2 ),
 ( 0.000000000000000000, 0.06250000000000000000, 0.1250000000000000000, 0.1875000000000000000, 0.2500000000000000000, 0.3125000000000000000, 0.3750000000000000000, 0.4375000000000000000, 0.5000000000000000000, 0.5625000000000000000, 0.6250000000000000000, 0.6875000000000000000, 0.7500000000000000000, 0.8125000000000000000, 0.8750000000000000000, 0.9375000000000000000, 1.000000000000000000 ),
 ( 0.000000000000000000, 1.000000000000000000 ),
 .UNSPECIFIED. ) ;
#46624 = EDGE_CURVE ( 'NONE', #81636, #46528, #58517, .T. ) ;
#46625 = EDGE_CURVE ( 'NONE', #42203, #6702, #2496, .T. ) ;
#46626 = CARTESIAN_POINT ( 'NONE',  ( 83.96886348723032256, 46.13120489799907631, 11.07011704621705128 ) ) ;
#46627 = CARTESIAN_POINT ( 'NONE',  ( 84.07404364193551771, 51.51966214638420638, 14.67759748506154338 ) ) ;
#46628 = ADVANCED_FACE ( 'NONE', ( #89967 ), #20547, .T. ) ;
#46629 = CARTESIAN_POINT ( 'NONE',  ( 183.1016766898827939, 295.7534076944302228, 1.248025944548516675 ) ) ;
#46630 = CARTESIAN_POINT ( 'NONE',  ( 75.87151652897671283, 214.6115022471902591, 10.00000000000009592 ) ) ;
#46631 = CARTESIAN_POINT ( 'NONE',  ( 36.46445469440066489, 39.79103043416552055, 8.090169943749478065 ) ) ;
#46632 = AXIS2_PLACEMENT_3D ( 'NONE', #81795, #3288, #42732 ) ;
#46633 = CARTESIAN_POINT ( 'NONE',  ( -22.42236680055709641, 157.8615022471902591, 0.000000000000000000 ) ) ;
#46634 = CARTESIAN_POINT ( 'NONE',  ( 30.81113223654366706, 188.5958772461660544, -9.188101187500095079 ) ) ;
#46635 = FACE_OUTER_BOUND ( 'NONE', #25247, .T. ) ;
#46636 = CARTESIAN_POINT ( 'NONE',  ( -59.65739779450132829, 37.15562860896454112, 10.00000000000000000 ) ) ;
#46637 = CARTESIAN_POINT ( 'NONE',  ( 203.2055155232897619, 269.6379347368149411, -5.981236179145930976 ) ) ;
#46638 = CARTESIAN_POINT ( 'NONE',  ( 199.2383506163646132, 285.5560492466715345, -17.78808061564097898 ) ) ;
#46639 = DIRECTION ( 'NONE',  ( -0.8660254037844377084, -0.5000000000000014433, -0.000000000000000000 ) ) ;
#46640 = EDGE_CURVE ( 'NONE', #12952, #52938, #68773, .T. ) ;
#46641 = CARTESIAN_POINT ( 'NONE',  ( 5.290446120544989306, 163.8615022471902023, 5.000000000000051514 ) ) ;
#46642 = CARTESIAN_POINT ( 'NONE',  ( 161.9461893331167914, 280.9078031139047198, -10.53061385661272276 ) ) ;
#46643 = DIRECTION ( 'NONE',  ( -0.1696015684586882066, -0.9855127132494805320, 0.000000000000000000 ) ) ;
#46644 = APPLICATION_PROTOCOL_DEFINITION ( 'draft international standard', 'automotive_design', 1998, #54587 ) ;
#46645 = CARTESIAN_POINT ( 'NONE',  ( 23.10466909204031083, 21.84335787977762777, 9.188101187500006262 ) ) ;
#46646 = CARTESIAN_POINT ( 'NONE',  ( 148.0389988358468827, 274.2359278451201590, 7.783622668412842671 ) ) ;
#46647 = CARTESIAN_POINT ( 'NONE',  ( 71.55582279638187515, 59.08747183676958770, 15.82285513313428105 ) ) ;
#46648 = CARTESIAN_POINT ( 'NONE',  ( 188.0957521190605348, 269.5173058182602404, -14.08221027142250925 ) ) ;
#46649 = ORIENTED_EDGE ( 'NONE', *, *, #43760, .T. ) ;
#46650 = CARTESIAN_POINT ( 'NONE',  ( 11.99908958663318970, 18.87878583063839955, -9.188101187500006262 ) ) ;
#46651 = EDGE_CURVE ( 'NONE', #68627, #30181, #33239, .T. ) ;
#46652 = CARTESIAN_POINT ( 'NONE',  ( 73.06697666995047769, 59.88521403644757868, -15.37108490149400275 ) ) ;
#46653 = CARTESIAN_POINT ( 'NONE',  ( 88.22316733864592209, 44.26875609612613971, 2.029272769359137474 ) ) ;
#46654 = EDGE_CURVE ( 'NONE', #28403, #43346, #67889, .T. ) ;
#46655 = ORIENTED_EDGE ( 'NONE', *, *, #52909, .F. ) ;
#46656 = DIRECTION ( 'NONE',  ( -0.7005979833698863235, -0.7135562106085605594, 0.000000000000000000 ) ) ;
#46657 = CARTESIAN_POINT ( 'NONE',  ( -17.42236680055705023, 149.2012482093457777, 0.000000000000000000 ) ) ;
#46658 = CARTESIAN_POINT ( 'NONE',  ( 77.22649460905378760, 63.31555197798695644, 15.15381191669832184 ) ) ;
#46659 = CARTESIAN_POINT ( 'NONE',  ( 86.45920310846531720, 44.18811037999328306, 6.432687887546634009 ) ) ;
#46660 = B_SPLINE_CURVE_WITH_KNOTS ( 'NONE', 3,
 ( #66138, #81878, #26648, #11956 ),
 .UNSPECIFIED., .F., .F.,
 ( 4, 4 ),
 ( 0.02488339598696336433, 0.03413011071240022731 ),
 .UNSPECIFIED. ) ;
#46661 = EDGE_LOOP ( 'NONE', ( #34206, #43696, #19328, #16624 ) ) ;
#46662 = ORIENTED_EDGE ( 'NONE', *, *, #96431, .F. ) ;
#46664 = CARTESIAN_POINT ( 'NONE',  ( 82.38352151192086126, 42.31992766688023977, -6.241314886312054888 ) ) ;
#46663 = CARTESIAN_POINT ( 'NONE',  ( -55.13986305262019982, 55.42364176852501600, 59.99999999999999289 ) ) ;
#46665 = ORIENTED_EDGE ( 'NONE', *, *, #5426, .T. ) ;
#46666 = CARTESIAN_POINT ( 'NONE',  ( 151.4384131719918685, 268.3479694989391078, 14.98299707687648841 ) ) ;
#46667 = AXIS2_PLACEMENT_3D ( 'NONE', #24523, #25018, #10841 ) ;
#46668 = LINE ( 'NONE', #77594, #96636 ) ;
#46669 = CARTESIAN_POINT ( 'NONE',  ( 72.92091214766469420, 56.78235363556951398, -15.96102170641831819 ) ) ;
#46670 = CARTESIAN_POINT ( 'NONE',  ( 3.540199675970839177, 23.81751292744053927, -6.180339887498951690 ) ) ;
#46671 = CARTESIAN_POINT ( 'NONE',  ( 147.6140518775699491, 274.9719575673779559, 8.457032797753797126 ) ) ;
#46672 = CARTESIAN_POINT ( 'NONE',  ( 196.8104339078508076, 289.7613243423628546, -16.40335862274955403 ) ) ;
#46673 = AXIS2_PLACEMENT_3D ( 'NONE', #42342, #28152, #35754 ) ;
#46674 = DIRECTION ( 'NONE',  ( 1.000000000000000000, 0.000000000000000000, 0.000000000000000000 ) ) ;
#46675 = EDGE_LOOP ( 'NONE', ( #41173, #9457, #1373, #18357 ) ) ;
#46676 = CARTESIAN_POINT ( 'NONE',  ( 157.1338510812060747, 258.4831816688264325, 17.88958125218800888 ) ) ;
#46677 = AXIS2_PLACEMENT_3D ( 'NONE', #42415, #73349, #66238 ) ;
#46678 = CARTESIAN_POINT ( 'NONE',  ( 161.9072444017735677, 267.0357427074497423, 16.52068954757439556 ) ) ;
#46679 = ORIENTED_EDGE ( 'NONE', *, *, #23169, .F. ) ;
#46680 = CARTESIAN_POINT ( 'NONE',  ( 33.71705561599726053, 20.26216523072496045, -2.296566073217252530E-15 ) ) ;
#46681 = CARTESIAN_POINT ( 'NONE',  ( 149.7128599965862463, 271.3367152699035501, 12.33532264622322394 ) ) ;
#46682 = CARTESIAN_POINT ( 'NONE',  ( 155.3598242554943454, 267.1614050273207113, -16.86360361314166667 ) ) ;
#46683 = ORIENTED_EDGE ( 'NONE', *, *, #60251, .T. ) ;
#46684 = CARTESIAN_POINT ( 'NONE',  ( -4.653128914090328472, 78.77562236714182120, 13.81405534229504717 ) ) ;
#46685 = CARTESIAN_POINT ( 'NONE',  ( 150.6931560952953646, 269.6387926204777727, 14.65021044537114037 ) ) ;
#46686 = LINE ( 'NONE', #76598, #19182 ) ;
#46688 = B_SPLINE_CURVE_WITH_KNOTS ( 'NONE', 3,
 ( #90438, #6281, #52869, #21976 ),
 .UNSPECIFIED., .F., .F.,
 ( 4, 4 ),
 ( 0.009394083817439216264, 0.01463245930893269410 ),
 .UNSPECIFIED. ) ;
#46687 = CARTESIAN_POINT ( 'NONE',  ( 83.50150581922116544, 52.39864595077343523, 14.81182293697902530 ) ) ;
#46689 = ORIENTED_EDGE ( 'NONE', *, *, #97722, .T. ) ;
#46690 = ORIENTED_EDGE ( 'NONE', *, *, #87389, .T. ) ;
#46691 = CIRCLE ( 'NONE', #6269, 10.00000000000001066 ) ;
#46692 = CARTESIAN_POINT ( 'NONE',  ( 193.8652130780152731, 280.5836658925297229, -17.72338988841175933 ) ) ;
#46693 = DIRECTION ( 'NONE',  ( 0.1550826972584426755, 0.9879014915521923124, 0.000000000000000000 ) ) ;
#46694 = CARTESIAN_POINT ( 'NONE',  ( 147.9710862514405960, 274.3535558917855042, 7.785500222159708272 ) ) ;
#46695 = ORIENTED_EDGE ( 'NONE', *, *, #334, .F. ) ;
#46696 = CARTESIAN_POINT ( 'NONE',  ( 149.5593209768671841, 271.6026526530012575, 11.55487339793564949 ) ) ;
#46697 = CARTESIAN_POINT ( 'NONE',  ( 161.8668411317136986, 250.2854024296290447, -13.43522912998426655 ) ) ;
#46698 = CARTESIAN_POINT ( 'NONE',  ( 192.6170194583582429, 297.0245312260774995, -11.90166228306590490 ) ) ;
#46699 = CARTESIAN_POINT ( 'NONE',  ( 163.9688125216115679, 256.9763212860731301, 15.96522343182667569 ) ) ;
#46700 = CARTESIAN_POINT ( 'NONE',  ( 69.89728461977614415, 67.46325532689361637, 9.448739956629149006 ) ) ;
#46701 = AXIS2_PLACEMENT_3D ( 'NONE', #64062, #56454, #87446 ) ;
#46702 = DIRECTION ( 'NONE',  ( -0.8279987035736640077, -0.5607300124661883656, 0.000000000000000000 ) ) ;
#46703 = CARTESIAN_POINT ( 'NONE',  ( 43.24043327773040346, 120.8247932685368227, -10.00000000000000000 ) ) ;
#46704 = CARTESIAN_POINT ( 'NONE',  ( 69.62290603085084228, 65.57344325233756877, -11.19888540440396696 ) ) ;
#46705 = CARTESIAN_POINT ( 'NONE',  ( 78.50823532819325123, 47.87735602650093369, 13.92489207041279897 ) ) ;
#46706 = CARTESIAN_POINT ( 'NONE',  ( 112.9752924205922824, 236.0333772461660544, 9.188101187500095079 ) ) ;
#46707 = ORIENTED_EDGE ( 'NONE', *, *, #39203, .F. ) ;
#46708 = CARTESIAN_POINT ( 'NONE',  ( 149.0029452494615327, 272.5663236809658088, -12.62683636271733079 ) ) ;
#46709 = DIRECTION ( 'NONE',  ( 0.5000000000000005551, -0.8660254037844384856, 0.000000000000000000 ) ) ;
#46710 = CARTESIAN_POINT ( 'NONE',  ( -86.81108781737714253, 15.00000000000000000, 9.212605237762131694 ) ) ;
#46711 = CARTESIAN_POINT ( 'NONE',  ( 154.8579861482817535, 262.4250953638155011, -17.69813260923097786 ) ) ;
#46712 = CARTESIAN_POINT ( 'NONE',  ( 180.1020640141543652, 283.3390819473285092, -16.04965679842496229 ) ) ;
#46713 = CARTESIAN_POINT ( 'NONE',  ( 83.61062943468348863, 51.62670160475642689, -14.84472182808584328 ) ) ;
#46714 = CARTESIAN_POINT ( 'NONE',  ( 168.6545886844981794, 284.7638151564323721, -7.963406596605243415 ) ) ;
#46715 = ORIENTED_EDGE ( 'NONE', *, *, #45986, .T. ) ;
#46716 = FACE_OUTER_BOUND ( 'NONE', #38934, .T. ) ;
#46717 = CARTESIAN_POINT ( 'NONE',  ( 72.11862359525288468, 71.68643115293319568, 5.491312638656053124 ) ) ;
#46718 = CARTESIAN_POINT ( 'NONE',  ( 74.65352423280955918, 67.09549399619112364, 12.48430392623164309 ) ) ;
#46719 = CARTESIAN_POINT ( 'NONE',  ( 130.0524911732904343, 236.7048013555409796, 4.594050593750051981 ) ) ;
#46720 = EDGE_CURVE ( 'NONE', #94946, #19691, #69477, .T. ) ;
#46721 = CARTESIAN_POINT ( 'NONE',  ( 192.9518127100452034, 296.0217619941561793, -12.12386602825073645 ) ) ;
#46722 = CARTESIAN_POINT ( 'NONE',  ( 185.2824853868734181, 297.7695098558858149, 4.231266468330407093 ) ) ;
#46723 = CARTESIAN_POINT ( 'NONE',  ( 195.8947060313465443, 291.3474115503753410, 16.07878593000791767 ) ) ;
#46724 = DIRECTION ( 'NONE',  ( 0.000000000000000000, 0.000000000000000000, 1.000000000000000000 ) ) ;
#46725 = CARTESIAN_POINT ( 'NONE',  ( 47.34706511187656020, 188.9548013555409796, -4.594050593750042211 ) ) ;
#46726 = CARTESIAN_POINT ( 'NONE',  ( 85.68890431086639126, 48.40205047417678230, -11.72463670400526325 ) ) ;
#46727 = ORIENTED_EDGE ( 'NONE', *, *, #40587, .T. ) ;
#46728 = CARTESIAN_POINT ( 'NONE',  ( 71.19401572595349137, 63.93336477220826453, 13.13347857285084785 ) ) ;
#46729 = CARTESIAN_POINT ( 'NONE',  ( 87.83581743205598968, 44.43730844317693141, -3.939890015914216725 ) ) ;
#46730 = ADVANCED_FACE ( 'NONE', ( #73240 ), #67110, .T. ) ;
#46731 = CARTESIAN_POINT ( 'NONE',  ( 73.46955079657830368, 61.49715917090933459, 15.42325390693441456 ) ) ;
#46732 = ADVANCED_FACE ( 'NONE', ( #96072 ), #36858, .T. ) ;
#46733 = DIRECTION ( 'NONE',  ( -0.000000000000000000, -0.000000000000000000, 1.000000000000000000 ) ) ;
#46734 = CARTESIAN_POINT ( 'NONE',  ( 151.2656506589457592, 278.4592319541795291, -1.679994777838232922 ) ) ;
#46735 = FACE_OUTER_BOUND ( 'NONE', #11988, .T. ) ;
#46736 = CARTESIAN_POINT ( 'NONE',  ( 178.3983311753540306, 261.1767784504364727, 12.27131754663537500 ) ) ;
#46737 = CARTESIAN_POINT ( 'NONE',  ( 109.4119587261635758, 240.6427522451419065, -10.00000000000009415 ) ) ;
#46738 = AXIS2_PLACEMENT_3D ( 'NONE', #100064, #85911, #39708 ) ;
#46739 = CARTESIAN_POINT ( 'NONE',  ( -10.80656490723494123, 24.88181024604956804, -10.00000000000000000 ) ) ;
#46740 = ORIENTED_EDGE ( 'NONE', *, *, #10312, .F. ) ;
#46741 = VECTOR ( 'NONE', #21591, 1000.000000000000000 ) ;
#46742 = B_SPLINE_CURVE_WITH_KNOTS ( 'NONE', 3,
 ( #26927, #57806, #48221, #40607 ),
 .UNSPECIFIED., .F., .F.,
 ( 4, 4 ),
 ( 0.02452775330616315669, 0.03377330297669509096 ),
 .UNSPECIFIED. ) ;
#46743 = CARTESIAN_POINT ( 'NONE',  ( 162.6937333994314656, 248.8531830095558632, 10.02305144031113926 ) ) ;
#46744 = CARTESIAN_POINT ( 'NONE',  ( 84.99999999999998579, 14.99999999999999467, 59.99999999999999289 ) ) ;
#46745 = B_SPLINE_CURVE_WITH_KNOTS ( 'NONE', 3,
 ( #41799, #64108, #48414, #95574 ),
 .UNSPECIFIED., .F., .F.,
 ( 4, 4 ),
 ( 0.03913036675905790657, 0.04762113371402499490 ),
 .UNSPECIFIED. ) ;
#46746 = AXIS2_PLACEMENT_3D ( 'NONE', #13110, #60657, #67789 ) ;
#46747 = CARTESIAN_POINT ( 'NONE',  ( 17.19803509898326510, 189.9244531367911293, -4.594050593750046652 ) ) ;
#46748 = AXIS2_PLACEMENT_3D ( 'NONE', #69725, #1340, #94072 ) ;
#46749 = CARTESIAN_POINT ( 'NONE',  ( 14.26779446008844410, 16.43677371833800294, -10.00000000000000355 ) ) ;
#46750 = LINE ( 'NONE', #16351, #50082 ) ;
#46751 = CARTESIAN_POINT ( 'NONE',  ( -76.86719868626529717, 52.73452925779879763, -10.00000000000000000 ) ) ;
#46752 = CARTESIAN_POINT ( 'NONE',  ( 73.13496796734084171, 69.72571060213493865, 9.125874619874972282 ) ) ;
#46754 = CARTESIAN_POINT ( 'NONE',  ( 66.20992061623260838, 209.0333772461660544, 9.188101187500095079 ) ) ;
#46753 = CARTESIAN_POINT ( 'NONE',  ( 194.7888003072046104, 275.1355240377584437, -15.74026182316778666 ) ) ;
#46755 = CARTESIAN_POINT ( 'NONE',  ( 200.5810378487751393, 283.2304467414622877, 18.38516374632547112 ) ) ;
#46756 = CARTESIAN_POINT ( 'NONE',  ( 73.11532976057090139, 57.21814247004398624, 16.39520198499102932 ) ) ;
#46757 = CARTESIAN_POINT ( 'NONE',  ( -29.38772878418747325, 95.39667460785805986, 44.61190340104155894 ) ) ;
#46758 = CARTESIAN_POINT ( 'NONE',  ( 66.64344042913042188, 68.36362187625169895, -4.347781399904284250 ) ) ;
#46759 = ORIENTED_EDGE ( 'NONE', *, *, #77623, .F. ) ;
#46760 = AXIS2_PLACEMENT_3D ( 'NONE', #96065, #20525, #27130 ) ;
#46761 = EDGE_CURVE ( 'NONE', #55485, #74117, #7255, .T. ) ;
#46762 = CARTESIAN_POINT ( 'NONE',  ( 35.67350403664903524, 184.7365022471902023, -10.00000000000009059 ) ) ;
#46763 = CARTESIAN_POINT ( 'NONE',  ( 164.4915767550571957, 245.7392269735623529, -6.407198159945809657 ) ) ;
#46764 = CARTESIAN_POINT ( 'NONE',  ( -13.35616335646270691, 163.0958772461660544, -9.188101187500095079 ) ) ;
#46765 = CARTESIAN_POINT ( 'NONE',  ( 28.23826220571969969, 31.70171378149920471, -9.188101187500004485 ) ) ;
#46766 = CARTESIAN_POINT ( 'NONE',  ( 164.2882805638152774, 260.0608980275483759, -16.19707932525749072 ) ) ;
#46767 = CARTESIAN_POINT ( 'NONE',  ( 188.4741096679671841, 261.7728559205870624, 6.464328172697664243 ) ) ;
#46768 = EDGE_CURVE ( 'NONE', #38420, #24993, #86404, .T. ) ;
#46769 = CARTESIAN_POINT ( 'NONE',  ( 206.1932826529868805, 273.5097535960530877, 11.72208607728249241 ) ) ;
#46770 = CARTESIAN_POINT ( 'NONE',  ( 88.48864216585432985, 44.00423028902886813, 2.007554169862328486 ) ) ;
#46771 = EDGE_CURVE ( 'NONE', #3544, #40063, #77210, .T. ) ;
#46772 = CARTESIAN_POINT ( 'NONE',  ( 66.30941063773362032, 69.19462254233461351, 2.488570590289448159 ) ) ;
#46773 = ORIENTED_EDGE ( 'NONE', *, *, #15155, .F. ) ;
#46774 = DIRECTION ( 'NONE',  ( -0.4272584830711199100, -0.9041295198387040433, 0.000000000000000000 ) ) ;
#46775 = CARTESIAN_POINT ( 'NONE',  ( 164.0776496603550925, 246.4561697322156419, 8.566708626497000267 ) ) ;
#46776 = CARTESIAN_POINT ( 'NONE',  ( 179.0267790344579453, 285.7867660831970511, 13.04357193698000295 ) ) ;
#46777 = CARTESIAN_POINT ( 'NONE',  ( 196.2629180738001082, 288.9574505909730533, 17.19408331658577183 ) ) ;
#46778 = CARTESIAN_POINT ( 'NONE',  ( 16.58301002715608519, 15.28920272979925876, -7.433330006724141015 ) ) ;
#46780 = VERTEX_POINT ( 'NONE', #15899 ) ;
#46779 = VECTOR ( 'NONE', #4278, 1000.000000000000000 ) ;
#46781 = CARTESIAN_POINT ( 'NONE',  ( 206.8783240872470230, 272.3232270266246928, 9.546753091190767648 ) ) ;
#46782 = B_SPLINE_CURVE_WITH_KNOTS ( 'NONE', 3,
 ( #71089, #63469, #86831, #65959, #89325, #19879, #11784, #4155, #8377, #39243, #70153, #23549, #38760, #84412, #7364, #16959, #62044, #32164, #61560, #77792, #54442, #85418, #8868, #763 ),
 .UNSPECIFIED., .F., .F.,
 ( 4, 2, 2, 2, 2, 2, 2, 2, 2, 2, 2, 4 ),
 ( 0.000000000000000000, 0.1249999999999867051, 0.2499999999999734102, 0.3749999999999601430, 0.4374999999999588662, 0.4999999999999575895, 0.5624999999999563682, 0.6249999999999551470, 0.6874999999999539257, 0.7499999999999527045, 0.8749999999999764633, 1.000000000000000000 ),
 .UNSPECIFIED. ) ;
#46783 = EDGE_CURVE ( 'NONE', #69110, #35956, #81771, .T. ) ;
#46784 = CARTESIAN_POINT ( 'NONE',  ( 205.1793861064249711, 275.2658739283173759, -14.08953480709093675 ) ) ;
#46785 = EDGE_CURVE ( 'NONE', #56036, #7074, #73094, .T. ) ;
#46786 = CARTESIAN_POINT ( 'NONE',  ( 192.1859061758433143, 297.7712413352111298, 11.15082371775444336 ) ) ;
#46787 = CARTESIAN_POINT ( 'NONE',  ( 207.6727254509676186, 270.9472835030587703, 7.315149605389819953 ) ) ;
#46788 = CARTESIAN_POINT ( 'NONE',  ( 188.0035612729766115, 279.2325960380115362, 17.82077010991123700 ) ) ;
#46789 = CARTESIAN_POINT ( 'NONE',  ( 207.6837091943624785, 270.9282591014416539, -1.156610046911421552 ) ) ;
#46790 = CARTESIAN_POINT ( 'NONE',  ( 200.6985908945154335, 283.0268388936558495, -17.74173253065502820 ) ) ;
#46791 = VERTEX_POINT ( 'NONE', #56893 ) ;
#46792 = EDGE_LOOP ( 'NONE', ( #1527, #17173, #71752, #50234 ) ) ;
#46793 = B_SPLINE_CURVE_WITH_KNOTS ( 'NONE', 3,
 ( #13560, #74869, #81492, #5451, #36336, #67237, #75365, #12061, #5944, #36838, #98671, #77338, #55020, #38320, #23611, #14551, #7946, #37821, #39799, #69228, #62110, #86001, #70223, #16527, #47424, #78350, #31708, #61119, #8933, #38820, #30239 ),
 .UNSPECIFIED., .F., .F.,
 ( 4, 3, 3, 3, 3, 3, 3, 3, 3, 3, 4 ),
 ( 0.000000000000000000, 0.1333490885032394824, 0.3007194338854430882, 0.4699862290245251373, 0.5844252810809388299, 0.6686540514502711252, 0.7354980260655488156, 0.8028463152565757932, 0.8633854507757249275, 0.9437142632667384623, 1.000000000000000000 ),
 .UNSPECIFIED. ) ;
#46794 = CARTESIAN_POINT ( 'NONE',  ( 190.4775783470208523, 281.5643400410450568, 17.30152405614960287 ) ) ;
#46795 = CARTESIAN_POINT ( 'NONE',  ( 79.99999999999998579, 9.999999999999985789, 59.99999999999999289 ) ) ;
#46796 = EDGE_LOOP ( 'NONE', ( #66643, #68651, #25539, #66358 ) ) ;
#46797 = CARTESIAN_POINT ( 'NONE',  ( -75.14068524134967220, 52.46521621197197760, -10.00000000000000000 ) ) ;
#46798 = CARTESIAN_POINT ( 'NONE',  ( 81.09808841527535606, 45.53856527529837450, -11.38469005618299335 ) ) ;
#46799 = VERTEX_POINT ( 'NONE', #47788 ) ;
#46800 = CARTESIAN_POINT ( 'NONE',  ( 193.2752197284765998, 263.9480352582601768, 7.898392093415175452 ) ) ;
#46801 = CARTESIAN_POINT ( 'NONE',  ( 79.49673530597218019, 59.23457754060601133, -16.22261858990263761 ) ) ;
#46802 = FACE_OUTER_BOUND ( 'NONE', #28866, .T. ) ;
#46803 = EDGE_LOOP ( 'NONE', ( #29470, #89046, #58642, #54748 ) ) ;
#46804 = CARTESIAN_POINT ( 'NONE',  ( 155.7347251133665225, 260.9065389313133778, 17.38482804120033975 ) ) ;
#46805 = CARTESIAN_POINT ( 'NONE',  ( 151.3560786774222322, 268.4905770267490652, 15.54402364351346932 ) ) ;
#46806 = CARTESIAN_POINT ( 'NONE',  ( 173.4606779374792325, 267.5814416807811540, -17.58000433512257032 ) ) ;
#46807 = VERTEX_POINT ( 'NONE', #23999 ) ;
#46808 = ORIENTED_EDGE ( 'NONE', *, *, #24012, .F. ) ;
#46809 = ORIENTED_EDGE ( 'NONE', *, *, #65690, .T. ) ;
#46810 = CARTESIAN_POINT ( 'NONE',  ( 79.76359975193354046, 44.98417069036879923, 11.54310746654911846 ) ) ;
#46811 = ORIENTED_EDGE ( 'NONE', *, *, #8906, .F. ) ;
#46812 = CARTESIAN_POINT ( 'NONE',  ( 68.28783021080273841, 68.52322149771096349, 6.374026897414869275 ) ) ;
#46813 = EDGE_LOOP ( 'NONE', ( #77713, #13809, #18026, #57481 ) ) ;
#46814 = CARTESIAN_POINT ( 'NONE',  ( 207.5408646414791178, 271.1756731246201753, 3.050859480894625886 ) ) ;
#46815 = CARTESIAN_POINT ( 'NONE',  ( 82.72537510787563519, 47.46459017876031083, 12.21375674901907615 ) ) ;
#46816 = CARTESIAN_POINT ( 'NONE',  ( 165.1439403752926864, 271.0709351213488389, 16.99278240859458933 ) ) ;
#46818 = EDGE_CURVE ( 'NONE', #20252, #11356, #24504, .T. ) ;
#46817 = CARTESIAN_POINT ( 'NONE',  ( 168.5857730741145986, 281.5268171081109472, 11.65604101945246995 ) ) ;
#46819 = CARTESIAN_POINT ( 'NONE',  ( 147.6508870500795467, 274.9081571770856272, -8.950912509993816712 ) ) ;
#46821 = CARTESIAN_POINT ( 'NONE',  ( 174.7916223044742026, 289.9785585703071433, 6.260260462112181123 ) ) ;
#46820 = AXIS2_PLACEMENT_3D ( 'NONE', #49924, #80881, #72246 ) ;
#46822 = DIRECTION ( 'NONE',  ( -0.8660254037844387076, -0.4999999999999998890, -0.000000000000000000 ) ) ;
#46823 = PLANE ( 'NONE',  #49590 ) ;
#46824 = CARTESIAN_POINT ( 'NONE',  ( 11.28581492663933084, 21.91421378149917487, 9.188101187500008038 ) ) ;
#46825 = CARTESIAN_POINT ( 'NONE',  ( 198.5400493072713459, 276.9865022881721188, -15.28351296223202382 ) ) ;
#46826 = CARTESIAN_POINT ( 'NONE',  ( 80.75322455565131463, 57.27148952657293535, 16.56885343786527187 ) ) ;
#46827 = VECTOR ( 'NONE', #7373, 1000.000000000000000 ) ;
#46829 = ORIENTED_EDGE ( 'NONE', *, *, #59102, .T. ) ;
#46828 = DIRECTION ( 'NONE',  ( -0.9619696745371179025, 0.2731562652969018457, 0.000000000000000000 ) ) ;
#46830 = CARTESIAN_POINT ( 'NONE',  ( 146.9087229868707425, 276.1936230421149503, -4.111764399247472390 ) ) ;
#46831 = CARTESIAN_POINT ( 'NONE',  ( 178.0495033679298160, 294.1167481546831368, 1.468944331028391614 ) ) ;
#46832 = CARTESIAN_POINT ( 'NONE',  ( 159.5895502557670795, 254.2297859303815244, -16.92708575547316485 ) ) ;
#46833 = FACE_OUTER_BOUND ( 'NONE', #49195, .T. ) ;
#46834 = CARTESIAN_POINT ( 'NONE',  ( 84.05047897864028528, 45.71949378961764410, -9.925846697072392644 ) ) ;
#46835 = CARTESIAN_POINT ( 'NONE',  ( 171.9867212485171990, 254.6089363721731900, 11.25268575585596409 ) ) ;
#46836 = CARTESIAN_POINT ( 'NONE',  ( 161.2739978509602565, 283.4540655898655928, 2.136591234652173377 ) ) ;
#46837 = EDGE_LOOP ( 'NONE', ( #92458, #70604, #17007, #96951 ) ) ;
#46838 = CARTESIAN_POINT ( 'NONE',  ( 194.1350435649782185, 294.3952363462973949, -14.11333646480683512 ) ) ;
#46839 = CARTESIAN_POINT ( 'NONE',  ( 74.89653295760797391, 66.81943746227949532, -13.20645658646817822 ) ) ;
#46840 = CARTESIAN_POINT ( 'NONE',  ( -16.25778278694858869, 23.14743555886464321, 177.5919119679930134 ) ) ;
#46841 = CARTESIAN_POINT ( 'NONE',  ( 4.695053651895191749, 183.5177522451419350, 5.000000000000046185 ) ) ;
#46842 = CARTESIAN_POINT ( 'NONE',  ( 88.91628449352961638, 212.9548013555409796, -4.594050593750042211 ) ) ;
#46843 = EDGE_CURVE ( 'NONE', #93369, #92094, #41584, .T. ) ;
#46844 = CARTESIAN_POINT ( 'NONE',  ( 82.32950663482070297, 40.35259760736478540, -1.135274614268407589 ) ) ;
#46845 = CARTESIAN_POINT ( 'NONE',  ( 8.827418999677703937, 23.83478043621386178, -8.090169943749479842 ) ) ;
#46846 = CARTESIAN_POINT ( 'NONE',  ( 166.9710079792242539, 278.1405409321207003, -13.47372957072173172 ) ) ;
#46847 = CARTESIAN_POINT ( 'NONE',  ( 72.57700935610729687, 70.89248372566723333, 7.619130926959984507 ) ) ;
#46849 = CARTESIAN_POINT ( 'NONE',  ( 75.65669688662353565, 65.40331689797208981, 14.28920693795837948 ) ) ;
#46848 = CARTESIAN_POINT ( 'NONE',  ( 15.06046875309669630, 173.3768266524159856, -9.188101187500091527 ) ) ;
#46850 = VECTOR ( 'NONE', #55244, 1000.000000000000227 ) ;
#46851 = CARTESIAN_POINT ( 'NONE',  ( 200.3134965941964651, 283.6938417875134064, 18.29802468362849766 ) ) ;
#46852 = ORIENTED_EDGE ( 'NONE', *, *, #16877, .T. ) ;
#46853 = VERTEX_POINT ( 'NONE', #54898 ) ;
#46854 = CARTESIAN_POINT ( 'NONE',  ( 188.1720092016451247, 260.2520035817423150, -6.289840127462773545 ) ) ;
#46855 = EDGE_CURVE ( 'NONE', #81160, #10579, #10319, .T. ) ;
#46856 = DIRECTION ( 'NONE',  ( -0.7280311630581435267, -0.6855440362341479466, 0.000000000000000000 ) ) ;
#46857 = EDGE_CURVE ( 'NONE', #35590, #38181, #77728, .T. ) ;
#46858 = DIRECTION ( 'NONE',  ( 0.8660254037844375974, 0.5000000000000017764, 3.252519625699413953E-16 ) ) ;
#46859 = CARTESIAN_POINT ( 'NONE',  ( 109.4841275098123248, 234.0177522451418781, -10.00000000000009592 ) ) ;
#46860 = CARTESIAN_POINT ( 'NONE',  ( 74.30189495389348053, 67.90489423305770345, -11.69701164576238384 ) ) ;
#46861 = CARTESIAN_POINT ( 'NONE',  ( 38.93012039702277605, 193.2833772461660544, -9.188101187500095079 ) ) ;
#46862 = CARTESIAN_POINT ( 'NONE',  ( 120.7963240266967375, 249.7369531367911293, -4.594050593750048428 ) ) ;
#46863 = CARTESIAN_POINT ( 'NONE',  ( 195.9325654604906788, 275.2851410020765570, 15.59701231568197066 ) ) ;
#46864 = EDGE_LOOP ( 'NONE', ( #82631, #92727, #38485, #42943 ) ) ;
#46865 = DIRECTION ( 'NONE',  ( 0.4999999999999998890, -0.8660254037844385966, 0.000000000000000000 ) ) ;
#46866 = CARTESIAN_POINT ( 'NONE',  ( 181.4204268205617154, 259.5203828285251006, -11.17471347674236348 ) ) ;
#46867 = CARTESIAN_POINT ( 'NONE',  ( 152.7730629122270898, 271.2363297891400293, 14.33490734661111610 ) ) ;
#46868 = LINE ( 'NONE', #47361, #26571 ) ;
#46869 = CARTESIAN_POINT ( 'NONE',  ( 193.9204722154232741, 294.7668848255750049, 15.43855698596013859 ) ) ;
#46870 = CARTESIAN_POINT ( 'NONE',  ( 175.0286707332103902, 254.6843269425917526, -9.831770975638562504 ) ) ;
#46871 = CARTESIAN_POINT ( 'NONE',  ( 194.3177355571849318, 294.0788045336591381, -15.93712594727561616 ) ) ;
#46872 = CARTESIAN_POINT ( 'NONE',  ( 148.3629184514745987, 273.6748826132846375, -8.219814532462343948 ) ) ;
#46873 = CARTESIAN_POINT ( 'NONE',  ( 191.2696313288225838, 264.4260228325948674, 7.786588993488871679 ) ) ;
#46874 = CARTESIAN_POINT ( 'NONE',  ( 171.3086152948395693, 279.7961921927451954, 13.89506224002436419 ) ) ;
#46875 = CARTESIAN_POINT ( 'NONE',  ( 186.9764723332892231, 298.1440520839146870, 5.986317207956076913 ) ) ;
#46876 = CARTESIAN_POINT ( 'NONE',  ( 71.70511086140308521, 71.96099529401990935, 1.996604445853504162 ) ) ;
#46877 = CARTESIAN_POINT ( 'NONE',  ( 148.3837145175834280, 273.6388627701866767, 8.841971351370922605 ) ) ;
#46878 = CARTESIAN_POINT ( 'NONE',  ( 181.1787732913807076, 266.0605537588476750, -14.95906821892703320 ) ) ;
#46879 = EDGE_LOOP ( 'NONE', ( #70567, #3720, #66009, #27276 ) ) ;
#46880 = CARTESIAN_POINT ( 'NONE',  ( 75.52901426996652390, 64.87836950227075761, 14.51720410870508537 ) ) ;
#46881 = EDGE_CURVE ( 'NONE', #13304, #61069, #96090, .T. ) ;
#46882 = CARTESIAN_POINT ( 'NONE',  ( 160.6734846709049691, 282.6943762970620924, -6.583290857611773461 ) ) ;
#46883 = CARTESIAN_POINT ( 'NONE',  ( 107.0210206738092609, 244.8464784336661353, 1.353441290958777327E-15 ) ) ;
#46884 = CARTESIAN_POINT ( 'NONE',  ( 17.79544559245429625, 15.98920272979925628, 7.433330006724137462 ) ) ;
#46885 = CARTESIAN_POINT ( 'NONE',  ( 151.4281781455628675, 268.3656970847310390, 15.24742929158552585 ) ) ;
#46886 = VECTOR ( 'NONE', #43070, 1000.000000000000000 ) ;
#46887 = CARTESIAN_POINT ( 'NONE',  ( 44.98086946945896614, 119.9434018396067785, -10.00000000000000000 ) ) ;
#46889 = LINE ( 'NONE', #47870, #65167 ) ;
#46888 = CARTESIAN_POINT ( 'NONE',  ( 15.90241741327948866, 17.38052372038639604, 10.00000000000000533 ) ) ;
#46890 = CARTESIAN_POINT ( 'NONE',  ( 150.5770346625965601, 269.8399208417597492, -15.30223397899647964 ) ) ;
#46891 = CARTESIAN_POINT ( 'NONE',  ( 150.7850480413316632, 269.4796311011364764, -14.43114374163211089 ) ) ;
#46892 = CARTESIAN_POINT ( 'NONE',  ( 149.3253462891332219, 272.0079086998416074, -12.99539319630191336 ) ) ;
#46893 = CARTESIAN_POINT ( 'NONE',  ( 81.96759120377315355, 40.97872302293440328, -3.040391630107510679 ) ) ;
#46894 = FACE_OUTER_BOUND ( 'NONE', #82148, .T. ) ;
#46895 = LINE ( 'NONE', #23083, #94430 ) ;
#46896 = EDGE_LOOP ( 'NONE', ( #27362, #63267, #80253, #43542 ) ) ;
#46897 = CARTESIAN_POINT ( 'NONE',  ( 163.3822952242776125, 256.1223835475196324, -14.91910106040644024 ) ) ;
#46898 = CARTESIAN_POINT ( 'NONE',  ( 159.3056354669941470, 256.7215407695565546, 17.03060606420897471 ) ) ;
#46899 = CARTESIAN_POINT ( 'NONE',  ( 80.87172617107097494, 46.94429920451448623, 13.16013926657569932 ) ) ;
#46900 = EDGE_CURVE ( 'NONE', #20229, #91452, #32608, .T. ) ;
#46901 = ORIENTED_EDGE ( 'NONE', *, *, #58424, .T. ) ;
#46902 = CARTESIAN_POINT ( 'NONE',  ( 75.93601443309867705, 65.18730796954976370, -14.47772449952195117 ) ) ;
#46903 = CARTESIAN_POINT ( 'NONE',  ( 179.9551071249317715, 262.8846855073763891, -12.83320019091600983 ) ) ;
#46904 = CARTESIAN_POINT ( 'NONE',  ( 72.40857565946932084, 71.84120774512069829, -5.522868224832428119 ) ) ;
#46905 = VECTOR ( 'NONE', #21205, 1000.000000000000000 ) ;
#46906 = CARTESIAN_POINT ( 'NONE',  ( 146.0195742355162452, 255.1115022471902591, 10.00000000000009592 ) ) ;
#46907 = VERTEX_POINT ( 'NONE', #41188 ) ;
#46908 = CARTESIAN_POINT ( 'NONE',  ( 73.39522077465731797, 69.90148087279546019, 9.687480369506271671 ) ) ;
#46909 = B_SPLINE_SURFACE_WITH_KNOTS ( 'NONE', 3, 1, ( 
 ( #30957, #61847 ),
 ( #91629, #22196 ),
 ( #60669, #37383 ),
 ( #85026, #54071 ),
 ( #52093, #90657 ),
 ( #67293, #69290 ),
 ( #61183, #98220 ),
 ( #92630, #67803 ),
 ( #75415, #15080 ),
 ( #13611, #46474 ),
 ( #44985, #99211 ),
 ( #59687, #5999 ),
 ( #44484, #28802 ),
 ( #15572, #98729 ),
 ( #21214, #83039 ),
 ( #22704, #29309 ),
 ( #83540, #84047 ),
 ( #14103, #77405 ),
 ( #14604, #45482 ),
 ( #76417, #6989 ),
 ( #36892, #37874 ),
 ( #91138, #45969 ),
 ( #75928, #60173 ),
 ( #68289, #36388 ),
 ( #21700, #30296 ),
 ( #6507, #52585 ),
 ( #53091, #29797 ),
 ( #68785, #99708 ),
 ( #92152, #53581 ),
 ( #84535, #76886 ),
 ( #7484, #23179 ),
 ( #38376, #100215 ),
 ( #30800, #61680 ),
 ( #39860, #16589 ) ),
 .UNSPECIFIED., .T., .F., .F.,
 ( 4, 2, 2, 2, 2, 2, 2, 2, 2, 2, 2, 2, 2, 2, 2, 2, 4 ),
 ( 2, 2 ),
 ( 0.000000000000000000, 0.06250000000000000000, 0.1250000000000000000, 0.1875000000000000000, 0.2500000000000000000, 0.3125000000000000000, 0.3750000000000000000, 0.4375000000000000000, 0.5000000000000000000, 0.5625000000000000000, 0.6250000000000000000, 0.6875000000000000000, 0.7500000000000000000, 0.8125000000000000000, 0.8750000000000000000, 0.9375000000000000000, 1.000000000000000000 ),
 ( 0.000000000000000000, 1.000000000000000000 ),
 .UNSPECIFIED. ) ;
#46910 = CARTESIAN_POINT ( 'NONE',  ( 40.09738740370236343, 25.01110640527295104, 2.839279412974134775 ) ) ;
#46911 = EDGE_LOOP ( 'NONE', ( #3980, #85008, #65983, #31548 ) ) ;
#46912 = CARTESIAN_POINT ( 'NONE',  ( 166.4874640644562476, 283.5895171948562279, 10.47325102323563861 ) ) ;
#46913 = CARTESIAN_POINT ( 'NONE',  ( -52.33464467766007289, 32.58262665401804270, 10.00000000000000000 ) ) ;
#46914 = CARTESIAN_POINT ( 'NONE',  ( 157.3094609834150788, 258.1790163958882545, 18.30007615310968916 ) ) ;
#46915 = ORIENTED_EDGE ( 'NONE', *, *, #12143, .T. ) ;
#46916 = CARTESIAN_POINT ( 'NONE',  ( 79.42847595952265749, 59.61293774653857724, 16.17779656922536802 ) ) ;
#46917 = CARTESIAN_POINT ( 'NONE',  ( -50.27375324258477463, 105.9839577528636738, -10.00000000000000000 ) ) ;
#46918 = CARTESIAN_POINT ( 'NONE',  ( 192.5903950300756264, 297.0706460885853062, -12.26281696942424482 ) ) ;
#46919 = DIRECTION ( 'NONE',  ( -1.000000000000000000, 0.000000000000000000, 0.000000000000000000 ) ) ;
#46920 = EDGE_CURVE ( 'NONE', #1592, #72762, #33204, .T. ) ;
#46921 = VECTOR ( 'NONE', #59564, 1000.000000000000000 ) ;
#46922 = PLANE ( 'NONE',  #72353 ) ;
#46923 = B_SPLINE_CURVE_WITH_KNOTS ( 'NONE', 3,
 ( #28232, #34343, #58134, #97664 ),
 .UNSPECIFIED., .F., .F.,
 ( 4, 4 ),
 ( 0.01035187532749593138, 0.01557239096276301533 ),
 .UNSPECIFIED. ) ;
#46924 = CARTESIAN_POINT ( 'NONE',  ( 87.35668359673078953, 44.84080960044052944, -6.701380392922970053 ) ) ;
#46925 = CARTESIAN_POINT ( 'NONE',  ( 81.52014092374062670, 55.46057516179622837, -16.31907950184206157 ) ) ;
#46927 = EDGE_LOOP ( 'NONE', ( #71987, #67093, #100154, #42445, #44902 ) ) ;
#46926 =( BOUNDED_CURVE ( )  B_SPLINE_CURVE ( 2, ( #51757, #85044, #70304, #59831, #44127, #23199, #15593, #62694, #8518 ),
 .UNSPECIFIED., .F., .T. ) 
 B_SPLINE_CURVE_WITH_KNOTS ( ( 3, 2, 2, 2, 3 ),
 ( 0.1895161290322580627, 0.1908602150537634379, 0.1935483870967741882, 0.1962365591397849385, 0.1975806451612903136 ),
 .UNSPECIFIED. ) 
 CURVE ( )  GEOMETRIC_REPRESENTATION_ITEM ( )  RATIONAL_B_SPLINE_CURVE ( ( 0.9330127018922194093, 0.9330127018922194093, 1.000000000000000000, 0.8660254037844387076, 1.000000000000000000, 0.8660254037844387076, 1.000000000000000000, 0.9330127018922194093, 0.9330127018922194093 ) ) 
 REPRESENTATION_ITEM ( '' )  );
#46928 = CARTESIAN_POINT ( 'NONE',  ( 195.6440376929661511, 290.9937640891101296, 16.03543930387630922 ) ) ;
#46929 = ORIENTED_EDGE ( 'NONE', *, *, #29907, .F. ) ;
#46930 = CARTESIAN_POINT ( 'NONE',  ( 81.23909821190164848, 55.73431417435049440, 16.38583623711208404 ) ) ;
#46931 = ORIENTED_EDGE ( 'NONE', *, *, #73436, .T. ) ;
#46932 = CARTESIAN_POINT ( 'NONE',  ( 169.6661456060803062, 269.2651292227166095, 17.56127676152747341 ) ) ;
#46933 = CARTESIAN_POINT ( 'NONE',  ( 79.06962916857435175, 52.50278213231310076, 15.56900390533574097 ) ) ;
#46934 = ORIENTED_EDGE ( 'NONE', *, *, #9947, .F. ) ;
#46935 = CARTESIAN_POINT ( 'NONE',  ( 189.8111788993726918, 300.3393367352153973, -3.345254087122194075 ) ) ;
#46936 = CARTESIAN_POINT ( 'NONE',  ( 164.3104563928357322, 246.0529366432151051, -1.966241142131954334 ) ) ;
#46937 = CARTESIAN_POINT ( 'NONE',  ( 190.6614556884314311, 300.4116670330316765, 2.330378985950405824 ) ) ;
#46938 = CARTESIAN_POINT ( 'NONE',  ( 148.9228818358559749, 272.7049975811580680, 12.13823097167056275 ) ) ;
#46939 = CARTESIAN_POINT ( 'NONE',  ( 193.8987971561367090, 262.1765911843755248, 0.2925312025757377254 ) ) ;
#46941 = EDGE_CURVE ( 'NONE', #58155, #42571, #57266, .T. ) ;
#46940 = CARTESIAN_POINT ( 'NONE',  ( 168.1437700021587318, 248.2856729686970993, -4.993057267767092355 ) ) ;
#46942 = LINE ( 'NONE', #54514, #19456 ) ;
#46943 = CARTESIAN_POINT ( 'NONE',  ( 183.5690767159531731, 284.2936931788220818, -15.45078497124822725 ) ) ;
#46944 = CARTESIAN_POINT ( 'NONE',  ( 120.4447615282330588, 240.3458772461660544, 9.188101187500095079 ) ) ;
#46946 = CARTESIAN_POINT ( 'NONE',  ( 185.9689676041826658, 262.3423500751161441, -9.039159276176199853 ) ) ;
#46945 = B_SPLINE_CURVE_WITH_KNOTS ( 'NONE', 3,
 ( #13936, #89977, #91465, #5835, #29147, #36724, #52925, #83877, #67628, #6827 ),
 .UNSPECIFIED., .F., .F.,
 ( 4, 2, 2, 2, 4 ),
 ( 0.000000000000000000, 0.2499999999999998890, 0.4999999999999998890, 0.7499999999999998890, 1.000000000000000000 ),
 .UNSPECIFIED. ) ;
#46947 = CARTESIAN_POINT ( 'NONE',  ( 161.2880211751412958, 283.7149074318706994, 2.164506641643817009 ) ) ;
#46948 = CARTESIAN_POINT ( 'NONE',  ( 180.3605947894885730, 291.0927862716739014, -9.605956182346858441 ) ) ;
#46949 = ORIENTED_EDGE ( 'NONE', *, *, #96915, .T. ) ;
#46950 = EDGE_LOOP ( 'NONE', ( #8591, #33488, #8175, #47213 ) ) ;
#46951 = CARTESIAN_POINT ( 'NONE',  ( 200.0930818951990489, 273.8593626791692373, 13.67973991811845558 ) ) ;
#46952 = CARTESIAN_POINT ( 'NONE',  ( 180.6189675032831303, 256.1636222267840139, 1.305556376142541275 ) ) ;
#46953 = CARTESIAN_POINT ( 'NONE',  ( 174.3074440017029190, 290.4856170877609429, -4.843019479348414258 ) ) ;
#46954 = CARTESIAN_POINT ( 'NONE',  ( 146.6932111911164327, 276.5669004219916474, 3.080321240977672126 ) ) ;
#46955 = CARTESIAN_POINT ( 'NONE',  ( -22.85267942241863182, 23.13820207187276168, -10.00000000000000000 ) ) ;
#46956 = CARTESIAN_POINT ( 'NONE',  ( 200.7134601498536028, 283.0010845879393742, -16.98649239173277792 ) ) ;
#46957 = CARTESIAN_POINT ( 'NONE',  ( -14.83894680564148238, 24.48641780169620219, 10.00000000000000000 ) ) ;
#46958 = LINE ( 'NONE', #77876, #64129 ) ;
#46959 = CARTESIAN_POINT ( 'NONE',  ( 174.0357770199878473, 253.2726379897468689, -7.670654613122240839 ) ) ;
#46960 = ORIENTED_EDGE ( 'NONE', *, *, #7740, .F. ) ;
#46961 = CARTESIAN_POINT ( 'NONE',  ( 200.4981329224417550, 282.9858865130267986, -16.73064699428216784 ) ) ;
#46962 = FACE_OUTER_BOUND ( 'NONE', #40407, .T. ) ;
#46963 = ORIENTED_EDGE ( 'NONE', *, *, #78442, .F. ) ;
#46964 = CARTESIAN_POINT ( 'NONE',  ( 191.2010045876914432, 266.9569875230786806, -12.78557827834137761 ) ) ;
#46965 = VECTOR ( 'NONE', #49002, 1000.000000000000000 ) ;
#46966 = LINE ( 'NONE', #16563, #19612 ) ;
#46967 = DIRECTION ( 'NONE',  ( -0.000000000000000000, -0.000000000000000000, -1.000000000000000000 ) ) ;
#46968 = CARTESIAN_POINT ( 'NONE',  ( 149.2511585606875428, 272.1364056148075292, 11.40684181024752242 ) ) ;
#46969 = CARTESIAN_POINT ( 'NONE',  ( 204.6797164308104584, 272.9778086334555951, -9.766007597308432153 ) ) ;
#46971 = CARTESIAN_POINT ( 'NONE',  ( 151.3919346942391257, 275.1019727134247432, -9.604374707620896956 ) ) ;
#46970 = CARTESIAN_POINT ( 'NONE',  ( 164.6595611665577508, 284.1616173530609331, -6.908293781447585324 ) ) ;
#46972 = CARTESIAN_POINT ( 'NONE',  ( 200.6737073311291795, 283.0699384897140476, -17.61533935526990291 ) ) ;
#46973 = ORIENTED_EDGE ( 'NONE', *, *, #22163, .F. ) ;
#46974 = CARTESIAN_POINT ( 'NONE',  ( 205.0608245822267293, 272.3115459547129262, -9.418476286974653888 ) ) ;
#46975 = CARTESIAN_POINT ( 'NONE',  ( 72.36980820381833723, 65.60254448469738975, 12.49385853657623713 ) ) ;
#46976 = CARTESIAN_POINT ( 'NONE',  ( 163.6234338235976224, 247.9473133546832457, -8.351226439232171117 ) ) ;
#46977 = CARTESIAN_POINT ( 'NONE',  ( 129.4230657250939203, 233.9824982072973683, 3.021315404115420679E-15 ) ) ;
#46978 = CARTESIAN_POINT ( 'NONE',  ( 191.9824032073976241, 287.6194387751458521, -17.05427143794285882 ) ) ;
#46979 = EDGE_CURVE ( 'NONE', #42396, #80773, #3237, .T. ) ;
#46980 = CARTESIAN_POINT ( 'NONE',  ( 188.1364496919973703, 299.4054452434185691, -3.692017684402327138 ) ) ;
#46981 = CARTESIAN_POINT ( 'NONE',  ( 192.1149248854976861, 297.8941845364767005, 12.26771790733441314 ) ) ;
#46982 = ADVANCED_FACE ( 'NONE', ( #34121 ), #81742, .T. ) ;
#46983 = DIRECTION ( 'NONE',  ( 0.000000000000000000, 1.000000000000000000, -1.090355031989287297E-16 ) ) ;
#46984 = AXIS2_PLACEMENT_3D ( 'NONE', #16210, #514, #22813 ) ;
#46985 = CARTESIAN_POINT ( 'NONE',  ( 74.17864136715245138, 68.61070255371173232, 11.00189009658737760 ) ) ;
#46986 = CARTESIAN_POINT ( 'NONE',  ( 165.3118168859175796, 246.3185293925050701, -4.432402497422931020 ) ) ;
#46987 = CARTESIAN_POINT ( 'NONE',  ( 71.04509092612660481, 70.63270342239739819, -5.353015442558778147 ) ) ;
#46988 = EDGE_CURVE ( 'NONE', #64873, #62347, #27015, .T. ) ;
#46989 = CARTESIAN_POINT ( 'NONE',  ( 94.11243691623624841, 215.9548013555409796, -4.594050593750042211 ) ) ;
#46990 = CARTESIAN_POINT ( 'NONE',  ( 76.54518344956915143, 148.6051630683315921, 8.938084663576969700E-16 ) ) ;
#46991 = CARTESIAN_POINT ( 'NONE',  ( 147.3379027498079381, 275.4502618871274535, -3.695260257281167249 ) ) ;
#46992 = CARTESIAN_POINT ( 'NONE',  ( 59.85004655896462111, 195.3615022471901739, 5.000000000000051514 ) ) ;
#46993 = EDGE_CURVE ( 'NONE', #99166, #54753, #42682, .T. ) ;
#46994 = CARTESIAN_POINT ( 'NONE',  ( 203.2732885619977026, 278.5673317194472247, -16.64305493556850024 ) ) ;
#46995 = CARTESIAN_POINT ( 'NONE',  ( 78.41884288903450795, 57.22565492815783728, 16.22179344803242174 ) ) ;
#46996 = DIRECTION ( 'NONE',  ( -1.000000000000000000, 0.000000000000000000, 0.000000000000000000 ) ) ;
#46998 = CARTESIAN_POINT ( 'NONE',  ( 75.84431070414076714, 51.61172808879248208, 15.73310713704503172 ) ) ;
#46997 = CARTESIAN_POINT ( 'NONE',  ( 73.38460905275829305, 69.71371501254900238, -9.902851190597802500 ) ) ;
#46999 = CARTESIAN_POINT ( 'NONE',  ( 207.2200715578708810, 271.7313030441461024, 6.059433301868463850 ) ) ;
#47000 = CARTESIAN_POINT ( 'NONE',  ( -8.728340106763610606, 175.7677522451419350, -5.000000000000047962 ) ) ;
#47001 = CARTESIAN_POINT ( 'NONE',  ( 205.5564942343509927, 274.6127034908020050, -12.67609813140607677 ) ) ;
#47002 = CARTESIAN_POINT ( 'NONE',  ( 196.4677418905696129, 290.3548843276421394, 17.08610552292358520 ) ) ;
#47003 = CARTESIAN_POINT ( 'NONE',  ( 190.3167824967908643, 299.0086585129598689, -8.112609889089975823 ) ) ;
#47004 = CARTESIAN_POINT ( 'NONE',  ( 32.16412338207434374, 195.5024278399160949, 9.188101187500095079 ) ) ;
#47005 = CARTESIAN_POINT ( 'NONE',  ( 78.41572647264329987, 206.8923013555409796, 4.594050593750050204 ) ) ;
#47006 = CARTESIAN_POINT ( 'NONE',  ( -19.65312891409030271, 93.06504152958497400, 177.5919119679930134 ) ) ;
#47007 = CARTESIAN_POINT ( 'NONE',  ( 88.08442549207046568, 44.03285108406542747, 0.5600040541675376238 ) ) ;
#47008 = CARTESIAN_POINT ( 'NONE',  ( 159.1311797733062861, 257.0237068946943282, -17.13424826516079946 ) ) ;
#47009 = CARTESIAN_POINT ( 'NONE',  ( -15.06115086838940442, 172.1115022471903160, -5.000000000000047962 ) ) ;
#47011 = FACE_OUTER_BOUND ( 'NONE', #63116, .T. ) ;
#47010 = DIRECTION ( 'NONE',  ( 0.8660254037844379305, 0.5000000000000012212, 0.000000000000000000 ) ) ;
#47012 = CARTESIAN_POINT ( 'NONE',  ( 196.7097633948733915, 269.7859973795743826, -10.82099196770793803 ) ) ;
#47013 = CARTESIAN_POINT ( 'NONE',  ( 24.61059131263772670, 35.18502408145593563, 5.678558825948276656 ) ) ;
#47014 = CARTESIAN_POINT ( 'NONE',  ( 128.9696990949621522, 255.2677522451419350, -5.000000000000047962 ) ) ;
#47015 = CARTESIAN_POINT ( 'NONE',  ( 83.02916638930869908, 47.07448630088824615, -11.77228440242573448 ) ) ;
#47016 = CARTESIAN_POINT ( 'NONE',  ( 11.52878981408637848, 24.84336893147754921, -7.433330006724137462 ) ) ;
#47017 = CARTESIAN_POINT ( 'NONE',  ( 53.24634253151052832, 210.7369531367911293, -4.594050593750048428 ) ) ;
#47018 = CARTESIAN_POINT ( 'NONE',  ( 158.6964626966795322, 256.6164276897989112, -16.48947266769615538 ) ) ;
#47019 = DIRECTION ( 'NONE',  ( -0.8660254037844378194, -0.5000000000000014433, -0.000000000000000000 ) ) ;
#47020 = CARTESIAN_POINT ( 'NONE',  ( 198.4706398937704819, 286.8857632237200619, 17.04020736381253798 ) ) ;
#47021 = CARTESIAN_POINT ( 'NONE',  ( -13.11024591527723615, 4.999999999999999112, -32.50000000000017053 ) ) ;
#47022 = CARTESIAN_POINT ( 'NONE',  ( 152.1494898648788876, 276.2488230399721374, 7.208019174511549387 ) ) ;
#47023 = B_SPLINE_CURVE_WITH_KNOTS ( 'NONE', 3,
 ( #47459, #864, #63163, #56042, #54043, #24660, #39835, #86528, #77885, #8965, #55052, #70256, #1381, #87034, #31743, #62647, #48474, #7979, #61656, #23152, #79416, #85001, #69761, #15545, #17058, #9982, #46444, #32261, #47949, #369, #31257, #16064, #62144, #93090, #54537, #96115, #73775, #27177, #10990, #12483, #48976, #11497, #81904, #56562, #34269, #73280, #97113, #49971 ),
 .UNSPECIFIED., .F., .F.,
 ( 4, 2, 2, 2, 2, 2, 2, 2, 2, 2, 2, 2, 2, 2, 2, 2, 2, 2, 2, 2, 2, 2, 2, 4 ),
 ( 0.002066062993612058103, 0.002506753530674276243, 0.002727098799205442126, 0.002947444067736608442, 0.003057616702002205478, 0.003167789336267802947, 0.003277961970533399983, 0.003388134604798997019, 0.003608479873330146422, 0.003828825141861295391, 0.004710206215986056932, 0.005591587290110819342, 0.006472968364235581751, 0.006913658901297997650, 0.007354349438360415284, 0.007464522072626019258, 0.007519608389758753592, 0.007574694706891489659, 0.007684867341156831691, 0.007795039975422173723, 0.008015385243952859520, 0.008235730512483545318, 0.008676421049544958547, 0.009117111586606371776 ),
 .UNSPECIFIED. ) ;
#47024 = CARTESIAN_POINT ( 'NONE',  ( 110.8733765985978295, 221.4865022471901455, 1.119607411625061291E-15 ) ) ;
#47025 = FACE_BOUND ( 'NONE', #65930, .T. ) ;
#47026 = CARTESIAN_POINT ( 'NONE',  ( 164.3274319858398087, 246.0235340536434592, -1.770631424362269168 ) ) ;
#47027 = ORIENTED_EDGE ( 'NONE', *, *, #52092, .T. ) ;
#47028 = CARTESIAN_POINT ( 'NONE',  ( 77.17767550845273661, 49.49660620011481882, 14.94353481738494516 ) ) ;
#47029 = CARTESIAN_POINT ( 'NONE',  ( 185.0467156058686271, 271.2432507303810780, 16.62608513826324241 ) ) ;
#47030 = VERTEX_POINT ( 'NONE', #65014 ) ;
#47031 = CARTESIAN_POINT ( 'NONE',  ( 206.1062572280473546, 273.6604860535989587, -9.773577984388410300 ) ) ;
#47032 = CARTESIAN_POINT ( 'NONE',  ( 190.1052544924596361, 279.3404689574773556, -17.51920321573983230 ) ) ;
#47033 = CARTESIAN_POINT ( 'NONE',  ( 69.40581272701848548, 68.85202937589532723, -6.985974446829570361 ) ) ;
#47034 = ORIENTED_EDGE ( 'NONE', *, *, #13996, .F. ) ;
#47035 = CARTESIAN_POINT ( 'NONE',  ( 173.4904780533158259, 251.2976502526514935, 0.4376931724216052144 ) ) ;
#47036 = ORIENTED_EDGE ( 'NONE', *, *, #849, .T. ) ;
#47037 = CARTESIAN_POINT ( 'NONE',  ( 79.48193946498695084, 46.39014452590906501, -12.72302186241215871 ) ) ;
#47038 = CARTESIAN_POINT ( 'NONE',  ( 147.7785919239399846, 274.6869658471848652, -7.924750738206837397 ) ) ;
#47039 = CARTESIAN_POINT ( 'NONE',  ( 7.819191540449068611, 28.68125778831127803, 177.5919119679930134 ) ) ;
#47040 = EDGE_CURVE ( 'NONE', #42087, #96482, #50296, .T. ) ;
#47041 = ORIENTED_EDGE ( 'NONE', *, *, #32298, .F. ) ;
#47042 = CARTESIAN_POINT ( 'NONE',  ( 20.27385872851041526, 33.74646525600390135, 2.839279412974139660 ) ) ;
#47043 = CARTESIAN_POINT ( 'NONE',  ( 75.07462636293115565, 55.18389248688383475, 16.14775407556821207 ) ) ;
#47044 = CARTESIAN_POINT ( 'NONE',  ( 66.06214068257196459, 68.71579393632853794, -0.4716098740908659659 ) ) ;
#47045 = CARTESIAN_POINT ( 'NONE',  ( 75.19555136791578320, 66.41508560950431672, -13.15604408571534911 ) ) ;
#47046 = EDGE_LOOP ( 'NONE', ( #80815, #58408, #39302, #40628 ) ) ;
#47047 = CARTESIAN_POINT ( 'NONE',  ( 79.58936028502597537, 59.22294857574253513, 16.56770033466462166 ) ) ;
#47048 = CARTESIAN_POINT ( 'NONE',  ( 192.1109889407927369, 285.6170536346646145, 17.50456793668967848 ) ) ;
#47049 = ORIENTED_EDGE ( 'NONE', *, *, #7400, .F. ) ;
#47050 = CIRCLE ( 'NONE', #22759, 14.82106496071134671 ) ;
#47051 = CARTESIAN_POINT ( 'NONE',  ( 172.0728039219370658, 285.9831811572526021, 11.38650458882361427 ) ) ;
#47053 = CARTESIAN_POINT ( 'NONE',  ( 67.68680448008480255, 65.78880813601070088, -10.60348352081087064 ) ) ;
#47052 = CARTESIAN_POINT ( 'NONE',  ( 67.66077361873938401, 65.75280524250749181, 10.62536374143375362 ) ) ;
#47054 = CARTESIAN_POINT ( 'NONE',  ( 81.37674444193763179, 55.19836804271280783, -15.94010240901345199 ) ) ;
#47055 = CARTESIAN_POINT ( 'NONE',  ( 154.9455285025717615, 262.2734675583710100, 18.28470720339922551 ) ) ;
#47056 = CARTESIAN_POINT ( 'NONE',  ( 186.4817412336421114, 293.3135959024839963, -10.75848554020329928 ) ) ;
#47057 = CARTESIAN_POINT ( 'NONE',  ( 204.6235849755581455, 276.2285497258825444, -13.59355699282649432 ) ) ;
#47058 = ADVANCED_FACE ( 'NONE', ( #11824 ), #81250, .T. ) ;
#47059 = CARTESIAN_POINT ( 'NONE',  ( 136.7095408212358052, 258.9244531367911577, -4.594050593750046652 ) ) ;
#47060 = CARTESIAN_POINT ( 'NONE',  ( -17.42236680055705023, 149.2012482093457777, 0.000000000000000000 ) ) ;
#47061 = CARTESIAN_POINT ( 'NONE',  ( 182.1519740190898915, 260.1784896748602023, 9.240519323136620500 ) ) ;
#47062 = CARTESIAN_POINT ( 'NONE',  ( 94.73480590126506229, 219.3768266524160140, 9.188101187500098632 ) ) ;
#47063 = ORIENTED_EDGE ( 'NONE', *, *, #55574, .F. ) ;
#47064 = CARTESIAN_POINT ( 'NONE',  ( 190.8001679306945277, 300.1714103817999444, 7.815449226872675403 ) ) ;
#47065 = CARTESIAN_POINT ( 'NONE',  ( 77.99401760355904401, 61.40429962668400776, -16.15929906019731632 ) ) ;
#47066 = EDGE_LOOP ( 'NONE', ( #62797, #2878, #24305, #51570 ) ) ;
#47067 = CARTESIAN_POINT ( 'NONE',  ( 195.7264009744229725, 291.6389244601378437, -15.67420937712721241 ) ) ;
#47068 = ORIENTED_EDGE ( 'NONE', *, *, #26480, .T. ) ;
#47069 = CARTESIAN_POINT ( 'NONE',  ( 80.14490519927410617, 44.22583949863496855, -11.35176587220589717 ) ) ;
#47070 = CARTESIAN_POINT ( 'NONE',  ( 58.43017357788679789, 217.8207943907112849, 17.47570218321536473 ) ) ;
#47071 = CARTESIAN_POINT ( 'NONE',  ( 146.5502055023624735, 276.8145935406849389, 0.3770461397900869427 ) ) ;
#47072 = DIRECTION ( 'NONE',  ( -0.000000000000000000, -0.000000000000000000, 1.000000000000000000 ) ) ;
#47073 = CARTESIAN_POINT ( 'NONE',  ( 49.65620586503731460, 206.1427522451419350, -10.00000000000009592 ) ) ;
#47074 = CARTESIAN_POINT ( 'NONE',  ( 208.0964157306580375, 270.2134304119617809, 3.093366075300640894 ) ) ;
#47075 = CARTESIAN_POINT ( 'NONE',  ( 72.86731735994297310, 219.0024278399160664, -9.188101187500093303 ) ) ;
#47076 = ORIENTED_EDGE ( 'NONE', *, *, #94947, .T. ) ;
#47077 = ORIENTED_EDGE ( 'NONE', *, *, #32550, .T. ) ;
#47078 = CARTESIAN_POINT ( 'NONE',  ( 201.0418987006243015, 282.4322123308404571, -17.97701256704421624 ) ) ;
#47079 = ORIENTED_EDGE ( 'NONE', *, *, #86226, .T. ) ;
#47080 = CARTESIAN_POINT ( 'NONE',  ( -110.0000000000000000, 0.000000000000000000, -59.99999999999999289 ) ) ;
#47081 = CARTESIAN_POINT ( 'NONE',  ( 184.1252449710846690, 275.2156845598054247, 16.36999343884330571 ) ) ;
#47082 = CARTESIAN_POINT ( 'NONE',  ( -29.66248920917699294, 94.05350397404733087, 44.45454265775622105 ) ) ;
#47083 = CARTESIAN_POINT ( 'NONE',  ( 207.4148176945302851, 271.0058409609101204, -1.674630231550592763 ) ) ;
#47084 = CARTESIAN_POINT ( 'NONE',  ( 88.18953256495667858, 44.42393962918851713, 4.547252263720216625 ) ) ;
#47085 = VERTEX_POINT ( 'NONE', #10818 ) ;
#47086 = CARTESIAN_POINT ( 'NONE',  ( 189.1055522710370838, 294.9567770444353982, 11.45155291829760635 ) ) ;
#47087 = CARTESIAN_POINT ( 'NONE',  ( 185.2880202283114386, 260.2658527302596667, 6.255690438817225640 ) ) ;
#47088 = CARTESIAN_POINT ( 'NONE',  ( 155.8843544236747221, 262.1387722156669611, -16.98283378502294738 ) ) ;
#47089 = CARTESIAN_POINT ( 'NONE',  ( 200.9061540366740246, 282.6673289856585143, -18.13083321883407351 ) ) ;
#47090 = LINE ( 'NONE', #25292, #6109 ) ;
#47091 = DIRECTION ( 'NONE',  ( -0.9981117208278914577, 0.06142469166373826922, 0.000000000000000000 ) ) ;
#47092 = ORIENTED_EDGE ( 'NONE', *, *, #36134, .T. ) ;
#47093 = CARTESIAN_POINT ( 'NONE',  ( 195.7593054227485823, 265.4221328166344165, 4.448014571397773231 ) ) ;
#47094 = CARTESIAN_POINT ( 'NONE',  ( 148.3402371503543122, 276.4804746445443016, -3.894670276620923133 ) ) ;
#47095 = CARTESIAN_POINT ( 'NONE',  ( 72.19109158906036328, 71.10838548458626462, -5.953967166465967686 ) ) ;
#47096 = CARTESIAN_POINT ( 'NONE',  ( 171.5709521921977228, 251.6229358086910395, 7.178360255118172439 ) ) ;
#47097 = CARTESIAN_POINT ( 'NONE',  ( 198.7195985473925646, 265.8573709945092105, 1.571795761342086761 ) ) ;
#47098 = CARTESIAN_POINT ( 'NONE',  ( 154.0195336324254640, 270.6124772311886773, 14.00887731801343783 ) ) ;
#47099 = EDGE_CURVE ( 'NONE', #526, #43182, #62315, .T. ) ;
#47100 = ORIENTED_EDGE ( 'NONE', *, *, #23976, .T. ) ;
#47101 = CYLINDRICAL_SURFACE ( 'NONE', #25503, 17.82106496071139645 ) ;
#47102 = CARTESIAN_POINT ( 'NONE',  ( 162.9148248802443106, 248.4702413316674381, 9.709394404200100581 ) ) ;
#47103 = DIRECTION ( 'NONE',  ( -0.4999999999999987788, 0.8660254037844392627, 0.000000000000000000 ) ) ;
#47105 = FACE_OUTER_BOUND ( 'NONE', #61855, .T. ) ;
#47104 = CARTESIAN_POINT ( 'NONE',  ( 194.1153812227096864, 294.4292925221022870, 15.54001482840963710 ) ) ;
#47106 = CARTESIAN_POINT ( 'NONE',  ( 79.81461207562318805, 55.55380833237374105, 16.46868291673067830 ) ) ;
#47107 = CARTESIAN_POINT ( 'NONE',  ( 24.41587626779758580, 32.83478043621389020, -8.090169943749479842 ) ) ;
#47108 = CARTESIAN_POINT ( 'NONE',  ( 168.4528758249346936, 273.4544194249853035, 16.10234030937003169 ) ) ;
#47109 = CARTESIAN_POINT ( 'NONE',  ( 163.4695553787563256, 283.8388210698513490, -3.127313904983202608 ) ) ;
#47110 = CARTESIAN_POINT ( 'NONE',  ( 133.0291931787496935, 237.6115022471901739, -5.000000000000041744 ) ) ;
#47111 = CARTESIAN_POINT ( 'NONE',  ( 188.3505816287238872, 260.6072362739506616, 3.597359921573489494 ) ) ;
#47112 = VECTOR ( 'NONE', #56764, 1000.000000000000114 ) ;
#47113 = CARTESIAN_POINT ( 'NONE',  ( 161.2488013048736377, 251.3558788108169040, -13.10044423494716170 ) ) ;
#47114 = CARTESIAN_POINT ( 'NONE',  ( 9.810363290536042058, 164.2202760586659736, -5.415160957724236172E-17 ) ) ;
#47115 = CARTESIAN_POINT ( 'NONE',  ( 151.9175917390909376, 272.5014707736564219, -13.07602542188641159 ) ) ;
#47116 = ORIENTED_EDGE ( 'NONE', *, *, #19412, .T. ) ;
#47117 = CARTESIAN_POINT ( 'NONE',  ( 160.5864543089798246, 253.1986605448440173, -14.65770029701640631 ) ) ;
#47118 = FACE_OUTER_BOUND ( 'NONE', #35769, .T. ) ;
#47119 = CARTESIAN_POINT ( 'NONE',  ( 151.1126408083691501, 268.9122237844355254, -15.82705194100464396 ) ) ;
#47120 = CARTESIAN_POINT ( 'NONE',  ( 26.56245542105003210, 176.9548013555409796, -4.594050593750042211 ) ) ;
#47121 = CARTESIAN_POINT ( 'NONE',  ( 181.6638189564591528, 276.3585937635120331, -17.48262025715165890 ) ) ;
#47122 = CARTESIAN_POINT ( 'NONE',  ( 28.51231065420500954, 32.16454794089043645, -10.00000000000000355 ) ) ;
#47123 = CARTESIAN_POINT ( 'NONE',  ( 165.0528804069804494, 264.4852527057752241, -17.76608744198970768 ) ) ;
#47124 = CARTESIAN_POINT ( 'NONE',  ( 173.6403832423602864, 272.8088530217519860, -16.35538478938354956 ) ) ;
#47125 = CARTESIAN_POINT ( 'NONE',  ( 73.76584831522595209, 68.38082682530665579, 11.49424229391075514 ) ) ;
#47126 = CARTESIAN_POINT ( 'NONE',  ( 190.0778721158842473, 298.5574750956744765, -8.040639183429819425 ) ) ;
#47127 = CARTESIAN_POINT ( 'NONE',  ( 190.7186658257535044, 261.9562542827834477, -0.7910153147876757274 ) ) ;
#47128 = CARTESIAN_POINT ( 'NONE',  ( 192.9932412455602559, 295.9775479609656372, -12.16274212864271753 ) ) ;
#47129 = CARTESIAN_POINT ( 'NONE',  ( 66.85041857288881317, 202.7365022471902023, -10.00000000000009059 ) ) ;
#47130 = CARTESIAN_POINT ( 'NONE',  ( 37.34220537994156786, 54.61056725541210710, -10.00000000000000000 ) ) ;
#47131 = CARTESIAN_POINT ( 'NONE',  ( 203.6409074000794703, 269.6153886175684420, 7.070074589036742907 ) ) ;
#47132 = CARTESIAN_POINT ( 'NONE',  ( 30.97333845187074886, 194.8149278399160949, -9.188101187500095079 ) ) ;
#47133 = CARTESIAN_POINT ( 'NONE',  ( 70.06557347674625191, 70.21240958854686198, -6.167066747300089524 ) ) ;
#47134 = CARTESIAN_POINT ( 'NONE',  ( 133.5343746642906240, 241.2365022471902307, 10.00000000000009948 ) ) ;
#47135 = CARTESIAN_POINT ( 'NONE',  ( 203.5276888907893635, 269.0805626209144634, -6.031028571504151614 ) ) ;
#47136 = CARTESIAN_POINT ( 'NONE',  ( 198.7357616895271804, 286.4265588032756114, -17.04018524297827497 ) ) ;
#47137 = CARTESIAN_POINT ( 'NONE',  ( -11.23413608767113026, 23.57316747377392119, -10.00000000000000000 ) ) ;
#47138 = CARTESIAN_POINT ( 'NONE',  ( 194.2321518193436987, 294.2270399159019121, 13.98132384850917020 ) ) ;
#47139 = CARTESIAN_POINT ( 'NONE',  ( 159.8837875743465986, 278.5245631928274292, -9.817169623836209169 ) ) ;
#47140 = FACE_OUTER_BOUND ( 'NONE', #73508, .T. ) ;
#47141 = CARTESIAN_POINT ( 'NONE',  ( 25.05680157815287146, 15.26216523072494624, -2.296566073217252530E-15 ) ) ;
#47142 = CARTESIAN_POINT ( 'NONE',  ( 202.7865629936218284, 279.4103651332174536, 17.10878160033216133 ) ) ;
#47143 = CARTESIAN_POINT ( 'NONE',  ( 181.8774662184618194, 285.1120569720015965, 15.89814067624403116 ) ) ;
#47144 = EDGE_CURVE ( 'NONE', #40913, #6085, #35095, .T. ) ;
#47145 = CARTESIAN_POINT ( 'NONE',  ( 174.8146681715918476, 256.6396774605312316, 12.00018018173206613 ) ) ;
#47146 = ORIENTED_EDGE ( 'NONE', *, *, #75864, .T. ) ;
#47147 = CARTESIAN_POINT ( 'NONE',  ( 14.11662529016922640, 10.01110640527290663, 2.839279412974134775 ) ) ;
#47148 = CARTESIAN_POINT ( 'NONE',  ( 48.16808589598787904, 104.3116767361652535, 10.00000000000000000 ) ) ;
#47149 = CARTESIAN_POINT ( 'NONE',  ( 85.29362735876655677, 48.41412782346649379, 12.38048700662148072 ) ) ;
#47150 = CARTESIAN_POINT ( 'NONE',  ( 88.04483770822093902, 44.27991475445110581, 2.801538001295460045 ) ) ;
#47151 = VERTEX_POINT ( 'NONE', #57900 ) ;
#47152 = DIRECTION ( 'NONE',  ( 1.000000000000000000, 0.000000000000000000, -5.984665299743594308E-16 ) ) ;
#47153 = CARTESIAN_POINT ( 'NONE',  ( 72.54986628483382560, 71.52703918853448783, -5.429478830856362848 ) ) ;
#47154 = CARTESIAN_POINT ( 'NONE',  ( 82.65729034470932390, 41.03234709804823410, -0.08711758718608976493 ) ) ;
#47155 = CARTESIAN_POINT ( 'NONE',  ( 155.4810912439522212, 261.3458456796594760, -18.44218279064527266 ) ) ;
#47156 = EDGE_CURVE ( 'NONE', #22952, #64642, #29454, .T. ) ;
#47157 = ORIENTED_EDGE ( 'NONE', *, *, #72763, .T. ) ;
#47158 = ORIENTED_EDGE ( 'NONE', *, *, #55194, .T. ) ;
#47160 = CARTESIAN_POINT ( 'NONE',  ( 83.13734387462676523, 42.41847577218787535, -5.524755388486198626 ) ) ;
#47159 = FACE_OUTER_BOUND ( 'NONE', #45717, .T. ) ;
#47161 = VERTEX_POINT ( 'NONE', #52771 ) ;
#47162 = CARTESIAN_POINT ( 'NONE',  ( 153.3506059258413643, 265.0359544954067132, -16.39100908615009899 ) ) ;
#47163 = CARTESIAN_POINT ( 'NONE',  ( 72.10046935555597258, 72.37486351763082837, -3.289382622874389206 ) ) ;
#47164 = CARTESIAN_POINT ( 'NONE',  ( 80.06670661031179748, 58.13998254173431235, 16.26766733971359358 ) ) ;
#47165 = CYLINDRICAL_SURFACE ( 'NONE', #9546, 15.50000000000000000 ) ;
#47166 = EDGE_CURVE ( 'NONE', #42571, #32950, #21062, .T. ) ;
#47167 = CARTESIAN_POINT ( 'NONE',  ( 190.1158090214649405, 301.3567547831981983, -1.340987185199551845 ) ) ;
#47168 = B_SPLINE_CURVE_WITH_KNOTS ( 'NONE', 3,
 ( #54707, #24330, #55206, #86187 ),
 .UNSPECIFIED., .F., .F.,
 ( 4, 4 ),
 ( 0.01606534115735265555, 0.02489855931191051891 ),
 .UNSPECIFIED. ) ;
#47169 = CARTESIAN_POINT ( 'NONE',  ( 196.4808189786114951, 290.3322341467384717, -17.84817245450773271 ) ) ;
#47170 = CARTESIAN_POINT ( 'NONE',  ( 180.5405277538137625, 287.0200771715591372, -13.55746091599727521 ) ) ;
#47171 = EDGE_LOOP ( 'NONE', ( #84163, #95829, #51220, #14269 ) ) ;
#47172 = CARTESIAN_POINT ( 'NONE',  ( 195.6986305151803549, 291.6870243064952888, 16.84182339398051909 ) ) ;
#47173 = CARTESIAN_POINT ( 'NONE',  ( 176.3152674796077974, 277.8542160414133946, -17.23542792216073138 ) ) ;
#47174 = ORIENTED_EDGE ( 'NONE', *, *, #80927, .T. ) ;
#47175 = CARTESIAN_POINT ( 'NONE',  ( 25.06043674821822265, 32.65586893147757053, -7.433330006724137462 ) ) ;
#47176 = CARTESIAN_POINT ( 'NONE',  ( 198.0792648159935538, 287.5636447432459022, 17.04758482866669667 ) ) ;
#47177 = CARTESIAN_POINT ( 'NONE',  ( 173.8805019302338621, 250.6242863632701585, 0.4030408839048176262 ) ) ;
#47178 = CARTESIAN_POINT ( 'NONE',  ( 60.22919299317007358, 196.3923013555409796, 4.594050593750050204 ) ) ;
#47179 = VERTEX_POINT ( 'NONE', #14784 ) ;
#47180 = B_SPLINE_CURVE_WITH_KNOTS ( 'NONE', 3,
 ( #51639, #76445, #99743, #52120 ),
 .UNSPECIFIED., .F., .F.,
 ( 4, 4 ),
 ( 0.01234167213556876079, 0.01858179642034042678 ),
 .UNSPECIFIED. ) ;
#47181 = DIRECTION ( 'NONE',  ( -0.6625377181876236365, -0.7490285521785781109, 0.000000000000000000 ) ) ;
#47182 = CARTESIAN_POINT ( 'NONE',  ( 160.6673679105988697, 254.1955030722899380, 15.77102516331386362 ) ) ;
#47183 = CYLINDRICAL_SURFACE ( 'NONE', #30497, 17.82106496071139645 ) ;
#47184 = CARTESIAN_POINT ( 'NONE',  ( 175.1271263694729328, 272.4273639404348728, 17.81557788710851042 ) ) ;
#47185 = ORIENTED_EDGE ( 'NONE', *, *, #50620, .T. ) ;
#47186 = AXIS2_PLACEMENT_3D ( 'NONE', #89333, #58355, #19886 ) ;
#47187 = ORIENTED_EDGE ( 'NONE', *, *, #94357, .F. ) ;
#47188 = CARTESIAN_POINT ( 'NONE',  ( 86.75857413767654691, 46.45790643663872288, 9.084114997326295793 ) ) ;
#47189 = CARTESIAN_POINT ( 'NONE',  ( 69.21394623383588396, 220.7677522451419065, -5.000000000000047962 ) ) ;
#47190 = CARTESIAN_POINT ( 'NONE',  ( 148.3280470635002928, 273.7352816289870248, 9.058704604771318003 ) ) ;
#47191 = VERTEX_POINT ( 'NONE', #14294 ) ;
#47192 = LINE ( 'NONE', #52788, #65707 ) ;
#47193 = DIRECTION ( 'NONE',  ( 0.2237140788069379993, 0.9746548163034761680, 0.000000000000000000 ) ) ;
#47194 = CARTESIAN_POINT ( 'NONE',  ( 207.8718670335145475, 270.6023601641878713, -6.322166851501095586 ) ) ;
#47195 = CARTESIAN_POINT ( 'NONE',  ( 146.9978162861947908, 276.0393089210717790, -5.134868500856280882 ) ) ;
#47196 = CARTESIAN_POINT ( 'NONE',  ( 163.3751545559699707, 257.8073145213600128, 15.56062503124628726 ) ) ;
#47197 = CARTESIAN_POINT ( 'NONE',  ( 155.5207183646172950, 261.6826666266933898, -16.99780945766855922 ) ) ;
#47198 = CARTESIAN_POINT ( 'NONE',  ( 164.7297297678022403, 245.3267338555121455, 3.020078936458732599 ) ) ;
#47199 = CARTESIAN_POINT ( 'NONE',  ( 67.69237348538017329, 66.82088825431436874, 8.559571887000258172 ) ) ;
#47200 = CARTESIAN_POINT ( 'NONE',  ( 68.34576586436469370, 65.68917945663493185, -10.35820680181607401 ) ) ;
#47201 = CARTESIAN_POINT ( 'NONE',  ( 69.35253854976203058, 63.01665765323906498, 13.58811665770852350 ) ) ;
#47202 = CARTESIAN_POINT ( 'NONE',  ( 109.5926410088830920, 224.8923013555410080, 4.594050593750050204 ) ) ;
#47203 = ORIENTED_EDGE ( 'NONE', *, *, #11288, .T. ) ;
#47204 = CARTESIAN_POINT ( 'NONE',  ( 147.0660117096331874, 275.9211909828330249, -0.7354350123930680772 ) ) ;
#47205 = EDGE_CURVE ( 'NONE', #51689, #57017, #69481, .T. ) ;
#47206 = LINE ( 'NONE', #78129, #54566 ) ;
#47207 = ADVANCED_FACE ( 'NONE', ( #37085 ), #68976, .F. ) ;
#47208 = CARTESIAN_POINT ( 'NONE',  ( -19.77026489254404495, 92.98508590942948615, 59.99999999999999289 ) ) ;
#47209 = CARTESIAN_POINT ( 'NONE',  ( 155.6066474290145720, 261.1283759879266881, -18.16552045242181279 ) ) ;
#47210 = CARTESIAN_POINT ( 'NONE',  ( 183.0265560501797495, 285.2188940410537725, -14.98214014822414164 ) ) ;
#47211 = CARTESIAN_POINT ( 'NONE',  ( 83.55263137061618295, 51.48653217629340162, -14.41405146157727479 ) ) ;
#47212 = CARTESIAN_POINT ( 'NONE',  ( 165.6338766894626531, 283.5762763500268306, -8.233634190165624034 ) ) ;
#47213 = ORIENTED_EDGE ( 'NONE', *, *, #55887, .T. ) ;
#47214 = CARTESIAN_POINT ( 'NONE',  ( 163.3020905273760093, 247.7994775548095845, -11.05431316445765155 ) ) ;
#47215 =( BOUNDED_CURVE ( )  B_SPLINE_CURVE ( 2, ( #58472, #12404, #65089, #41782, #50384, #34683, #4282, #19018, #89445, #35181, #97038, #42274, #3318 ),
 .UNSPECIFIED., .F., .T. ) 
 B_SPLINE_CURVE_WITH_KNOTS ( ( 3, 2, 2, 2, 2, 2, 3 ),
 ( 0.2625000000000000111, 0.2650000000000000133, 0.2700000000000000178, 0.2750000000000000222, 0.2800000000000000266, 0.2849999999999999756, 0.2874999999999999778 ),
 .UNSPECIFIED. ) 
 CURVE ( )  GEOMETRIC_REPRESENTATION_ITEM ( )  RATIONAL_B_SPLINE_CURVE ( ( 0.9755282581475768211, 0.9755282581475768211, 1.000000000000000000, 0.9510565162951535312, 1.000000000000000000, 0.9510565162951535312, 1.000000000000000000, 0.9510565162951535312, 1.000000000000000000, 0.9510565162951535312, 1.000000000000000000, 0.9755282581475768211, 0.9755282581475768211 ) ) 
 REPRESENTATION_ITEM ( '' )  );
#47216 = CARTESIAN_POINT ( 'NONE',  ( 71.95473880081605955, 71.54457537667215661, 5.606738443688825235 ) ) ;
#47217 = CARTESIAN_POINT ( 'NONE',  ( 165.0807124393095364, 244.7188140358855151, -1.586079993046279446 ) ) ;
#47218 = CARTESIAN_POINT ( 'NONE',  ( 123.3944002380500677, 251.2369531367911293, -4.594050593750048428 ) ) ;
#47219 = CARTESIAN_POINT ( 'NONE',  ( 150.9363692955544991, 269.2175350005573478, -14.27857383982596140 ) ) ;
#47220 = EDGE_CURVE ( 'NONE', #14650, #62301, #59880, .T. ) ;
#47221 = CARTESIAN_POINT ( 'NONE',  ( 188.9842081906053295, 299.1938366728135748, 4.832788090775505196 ) ) ;
#47222 = CARTESIAN_POINT ( 'NONE',  ( 187.5788460363194758, 281.4634433164364964, -17.49678885218273550 ) ) ;
#47223 = CARTESIAN_POINT ( 'NONE',  ( 45.11483101423404918, 69.99284853207299761, -10.00000000000000000 ) ) ;
#47224 = CARTESIAN_POINT ( 'NONE',  ( 49.53858449761714411, 211.6589784336661637, -6.496448406907675876E-16 ) ) ;
#47225 = VECTOR ( 'NONE', #47273, 1000.000000000000000 ) ;
#47226 = CARTESIAN_POINT ( 'NONE',  ( 72.42166623772517653, 61.87394061769263942, -15.04969437984479796 ) ) ;
#47227 = ORIENTED_EDGE ( 'NONE', *, *, #81869, .T. ) ;
#47229 = EDGE_CURVE ( 'NONE', #54866, #82108, #36445, .T. ) ;
#47228 = CARTESIAN_POINT ( 'NONE',  ( 38.90713690219553200, 54.71539658304151743, 177.5919119679930134 ) ) ;
#47230 = CARTESIAN_POINT ( 'NONE',  ( -106.6146531411567224, 123.6868197944957188, -37.49999999999997868 ) ) ;
#47231 = EDGE_CURVE ( 'NONE', #57637, #71229, #29490, .T. ) ;
#47232 = B_SPLINE_SURFACE_WITH_KNOTS ( 'NONE', 3, 1, ( 
 ( #51469, #50965 ),
 ( #82437, #74801 ),
 ( #28665, #69530 ),
 ( #77654, #21097 ),
 ( #636, #51974 ),
 ( #66669, #13000 ),
 ( #69023, #8240 ),
 ( #12494, #140 ),
 ( #5379, #99953 ),
 ( #62410, #43361 ),
 ( #92376, #35774 ),
 ( #36265, #31024 ),
 ( #67165, #74311 ),
 ( #22923, #61915 ),
 ( #30536, #54307 ),
 ( #61423, #92863 ),
 ( #15823, #46726 ),
 ( #78147, #1655 ),
 ( #17848, #24435 ),
 ( #95396, #32540 ),
 ( #87314, #71053 ),
 ( #32018, #79178 ),
 ( #62927, #85802 ),
 ( #2650, #40617 ),
 ( #23923, #8734 ),
 ( #55311, #2147 ),
 ( #63928, #9757 ),
 ( #78651, #39605 ),
 ( #94372, #86292 ),
 ( #9236, #63435 ),
 ( #48233, #24927 ) ),
 .UNSPECIFIED., .F., .F., .F.,
 ( 4, 3, 3, 3, 3, 3, 3, 3, 3, 3, 4 ),
 ( 2, 2 ),
 ( 0.000000000000000000, 0.1333490885032397044, 0.3007194338854659588, 0.4699862290245639951, 0.5844252810809660303, 0.6686540514503046539, 0.7354980260655714641, 0.8028463152565815664, 0.8633854507757389163, 0.9437142632667553377, 1.000000000000000000 ),
 ( 0.000000000000000000, 1.000000000000000000 ),
 .UNSPECIFIED. ) ;
#47233 = CARTESIAN_POINT ( 'NONE',  ( 73.87133013375215285, 63.28806875567715196, 14.81981384368521582 ) ) ;
#47234 = CARTESIAN_POINT ( 'NONE',  ( 175.0574341850002895, 261.2992596373129572, 14.66236234505684877 ) ) ;
#47235 = CARTESIAN_POINT ( 'NONE',  ( 152.6547697591180111, 278.7515079535921814, -4.825746761778547445 ) ) ;
#47236 = CARTESIAN_POINT ( 'NONE',  ( 202.7754741559590173, 279.4295715634463022, -15.65855077192107636 ) ) ;
#47237 = CARTESIAN_POINT ( 'NONE',  ( 178.3679663846656354, 261.2045661951830198, 12.31888526918040583 ) ) ;
#47238 = CARTESIAN_POINT ( 'NONE',  ( 119.8042635715768540, 246.6427522451419065, -10.00000000000009415 ) ) ;
#47239 = CARTESIAN_POINT ( 'NONE',  ( -15.10528209597770299, 24.46087392797018722, 10.00000000000000000 ) ) ;
#47240 = EDGE_LOOP ( 'NONE', ( #78568, #2222, #59181 ) ) ;
#47241 = CARTESIAN_POINT ( 'NONE',  ( 202.6551236945213361, 279.6380246773706517, 15.55476940527561425 ) ) ;
#47242 = CARTESIAN_POINT ( 'NONE',  ( 87.89309248043456080, 44.79219472772870603, 4.915507336728490273 ) ) ;
#47243 = CARTESIAN_POINT ( 'NONE',  ( 30.59497298136257726, 176.2202760586660020, -5.415160957724236172E-17 ) ) ;
#47244 = CARTESIAN_POINT ( 'NONE',  ( 18.10888558598233899, 12.58380873178785819, 6.180339887498953466 ) ) ;
#47245 = CARTESIAN_POINT ( 'NONE',  ( 192.3713340522295709, 271.8780416168410170, 15.57788208939756380 ) ) ;
#47246 = DIRECTION ( 'NONE',  ( 0.7280311630581364213, 0.6855440362341556071, 0.000000000000000000 ) ) ;
#47247 = DIRECTION ( 'NONE',  ( 0.1710100716628310258, -0.2961981327260192476, 0.9396926207859104263 ) ) ;
#47249 = CARTESIAN_POINT ( 'NONE',  ( 64.74867629522887569, 202.0643266524159856, -9.188101187500093303 ) ) ;
#47248 = CARTESIAN_POINT ( 'NONE',  ( 191.2126589609105736, 267.4645585149979752, 13.28012995173027733 ) ) ;
#47250 = CARTESIAN_POINT ( 'NONE',  ( 12.12248498587032586, 9.127558733836242055, -6.180339887498949025 ) ) ;
#47251 = CARTESIAN_POINT ( 'NONE',  ( 163.1976272564393184, 256.1029571228265809, -14.97062603987144058 ) ) ;
#47252 = CARTESIAN_POINT ( 'NONE',  ( -31.06813028187898240, 96.88955183556316797, 44.49079097436682417 ) ) ;
#47253 = CARTESIAN_POINT ( 'NONE',  ( 11.78719504716597299, 22.50829794293879260, -10.00000000000000355 ) ) ;
#47254 = VERTEX_POINT ( 'NONE', #53763 ) ;
#47255 = CARTESIAN_POINT ( 'NONE',  ( 27.87927540258908365, 180.2365022471902023, -10.00000000000009059 ) ) ;
#47256 = PLANE ( 'NONE',  #19923 ) ;
#47257 = CARTESIAN_POINT ( 'NONE',  ( 162.6476498368881494, 248.9330020812748785, 10.75824100428386743 ) ) ;
#47258 = CARTESIAN_POINT ( 'NONE',  ( -9.459049039432731121, 165.3458772461660544, 9.188101187500095079 ) ) ;
#47259 = CARTESIAN_POINT ( 'NONE',  ( 27.63686232447692603, 34.14336893147756768, 7.433330006724141015 ) ) ;
#47261 = CARTESIAN_POINT ( 'NONE',  ( 170.4370497408796723, 263.6275113357616533, 15.80834233833078351 ) ) ;
#47260 = CARTESIAN_POINT ( 'NONE',  ( 167.2771105491443677, 262.3221479689785269, -16.42317405296926935 ) ) ;
#47262 = CARTESIAN_POINT ( 'NONE',  ( 189.2125443449212696, 261.8290248071659221, 6.598221272828422634 ) ) ;
#47263 = CARTESIAN_POINT ( 'NONE',  ( 164.8616299252405213, 245.0982760813026857, 1.544363874765093625 ) ) ;
#47264 = CARTESIAN_POINT ( 'NONE',  ( 187.0048093878013731, 259.3019680120904695, -2.391362674332986771 ) ) ;
#47265 = CARTESIAN_POINT ( 'NONE',  ( 66.20598794047340618, 69.12131181250303769, 2.565109441349023189 ) ) ;
#47266 = ORIENTED_EDGE ( 'NONE', *, *, #22121, .F. ) ;
#47267 = CARTESIAN_POINT ( 'NONE',  ( 37.34220537994157496, 54.61056725541210710, -10.00000000000000000 ) ) ;
#47268 = CARTESIAN_POINT ( 'NONE',  ( 181.7502613149374326, 287.7871512160830889, 13.52857313414122054 ) ) ;
#47269 = CARTESIAN_POINT ( 'NONE',  ( 196.2865739685663300, 290.0389735281796675, 16.35500968239857755 ) ) ;
#47270 = CARTESIAN_POINT ( 'NONE',  ( 14.61458989734527947, 10.29860640527290805, -2.839279412974138328 ) ) ;
#47271 = CARTESIAN_POINT ( 'NONE',  ( 206.5215086902351516, 272.9412494231720530, 8.384715559417665887 ) ) ;
#47272 = EDGE_CURVE ( 'NONE', #33261, #77716, #21884, .T. ) ;
#47273 = DIRECTION ( 'NONE',  ( 0.06415622980647768536, -0.9979398670145503969, 0.000000000000000000 ) ) ;
#47274 = EDGE_CURVE ( 'NONE', #86364, #38315, #9006, .T. ) ;
#47275 = LINE ( 'NONE', #55362, #47366 ) ;
#47276 = CARTESIAN_POINT ( 'NONE',  ( 89.31526421587503251, 210.8262482093457777, 3.021315404115420679E-15 ) ) ;
#47277 = CARTESIAN_POINT ( 'NONE',  ( 94.49106271034210636, 235.3615022471903160, 5.000000000000046185 ) ) ;
#47278 = CARTESIAN_POINT ( 'NONE',  ( 207.5920568422024814, 271.0870056320159165, -1.586464549033245186 ) ) ;
#47279 = CARTESIAN_POINT ( 'NONE',  ( 193.8913555215501390, 294.8173164187117550, 15.40725395879721837 ) ) ;
#47280 = ORIENTED_EDGE ( 'NONE', *, *, #43884, .T. ) ;
#47281 = CARTESIAN_POINT ( 'NONE',  ( 156.4864942492372677, 277.0302591896826812, -10.06882784799783437 ) ) ;
#47282 = CARTESIAN_POINT ( 'NONE',  ( 72.98255309615508679, 70.80854987616386609, 7.399406208479893721 ) ) ;
#47283 = VERTEX_POINT ( 'NONE', #71505 ) ;
#47284 = CARTESIAN_POINT ( 'NONE',  ( 17.99199860517156324, 32.16126292948895582, -6.180339887498951690 ) ) ;
#47285 = CARTESIAN_POINT ( 'NONE',  ( 155.4185480231587064, 262.3956844143579588, -17.21684874643274554 ) ) ;
#47287 = EDGE_CURVE ( 'NONE', #2005, #86000, #92815, .T. ) ;
#47286 = ORIENTED_EDGE ( 'NONE', *, *, #50252, .F. ) ;
#47288 = CARTESIAN_POINT ( 'NONE',  ( 191.1687199697037443, 299.5330595250031820, -8.491751560014430211 ) ) ;
#47289 = FACE_OUTER_BOUND ( 'NONE', #84848, .T. ) ;
#47290 = CARTESIAN_POINT ( 'NONE',  ( 17.29678581741014654, 10.39040679176981996, 1.333680081654574804E-15 ) ) ;
#47292 = VECTOR ( 'NONE', #36433, 1000.000000000000114 ) ;
#47291 = CARTESIAN_POINT ( 'NONE',  ( 69.39239498971687681, 62.76033227987573326, 13.75497651673264521 ) ) ;
#47293 = ORIENTED_EDGE ( 'NONE', *, *, #43183, .F. ) ;
#47294 = CARTESIAN_POINT ( 'NONE',  ( 200.2631011806900005, 283.7811292041749311, 18.23377125296567058 ) ) ;
#47295 = CARTESIAN_POINT ( 'NONE',  ( 133.0291931787496651, 247.6115022471902591, 10.00000000000009592 ) ) ;
#47296 = CARTESIAN_POINT ( 'NONE',  ( 191.2056514706806070, 299.4690922889112699, 7.290007621276087590 ) ) ;
#47297 = CARTESIAN_POINT ( 'NONE',  ( 177.4640749235418866, 269.0261679207779935, -17.44345675124527517 ) ) ;
#47298 = VERTEX_POINT ( 'NONE', #31969 ) ;
#47299 = EDGE_CURVE ( 'NONE', #69624, #19580, #36820, .T. ) ;
#47300 = ORIENTED_EDGE ( 'NONE', *, *, #31149, .T. ) ;
#47301 = EDGE_CURVE ( 'NONE', #94538, #43912, #94323, .T. ) ;
#47302 = ORIENTED_EDGE ( 'NONE', *, *, #89569, .T. ) ;
#47303 = CARTESIAN_POINT ( 'NONE',  ( 72.84729272447545156, 59.04174750966416241, 15.54885058021578814 ) ) ;
#47304 = ORIENTED_EDGE ( 'NONE', *, *, #57998, .F. ) ;
#47305 = CARTESIAN_POINT ( 'NONE',  ( 163.8111981134063342, 274.4328725233862087, -16.00973502687279648 ) ) ;
#47306 = ORIENTED_EDGE ( 'NONE', *, *, #76722, .T. ) ;
#47307 = CARTESIAN_POINT ( 'NONE',  ( 88.09111776262265892, 44.56188567158400815, -5.102872454969319627 ) ) ;
#47308 = CARTESIAN_POINT ( 'NONE',  ( 81.27042111320733397, 44.06946909743304985, 9.799045354441355826 ) ) ;
#47309 = CARTESIAN_POINT ( 'NONE',  ( 165.1854192917994624, 270.9806551308440703, 16.59870098112833148 ) ) ;
#47310 = CARTESIAN_POINT ( 'NONE',  ( 171.0782956557647196, 283.4844436738434865, 12.11060603767918131 ) ) ;
#47311 = CARTESIAN_POINT ( 'NONE',  ( 147.6264044922760377, 274.9505622111005323, -8.841872555777701592 ) ) ;
#47312 = CARTESIAN_POINT ( 'NONE',  ( 82.60068805421772709, 53.27059767035463267, -15.30334251677975388 ) ) ;
#47313 = CARTESIAN_POINT ( 'NONE',  ( 159.0969231069750549, 255.0830411812770535, -17.15863751354124034 ) ) ;
#47314 = AXIS2_PLACEMENT_3D ( 'NONE', #16926, #48852, #79288 ) ;
#47315 = DIRECTION ( 'NONE',  ( 1.156482317317871331E-15, -1.000000000000000000, 0.000000000000000000 ) ) ;
#47316 = CARTESIAN_POINT ( 'NONE',  ( 23.79748941506785442, 22.24335787977763346, -9.188101187500008038 ) ) ;
#47317 = DIRECTION ( 'NONE',  ( -0.9413434404457832194, 0.3374500364938435859, 0.000000000000000000 ) ) ;
#47318 = FACE_OUTER_BOUND ( 'NONE', #66547, .T. ) ;
#47320 = VERTEX_POINT ( 'NONE', #47669 ) ;
#47319 = CARTESIAN_POINT ( 'NONE',  ( 206.9182786203111277, 271.7016349257525576, 5.804932932542666180 ) ) ;
#47321 = CYLINDRICAL_SURFACE ( 'NONE', #4518, 16.60714546451156792 ) ;
#47322 = EDGE_CURVE ( 'NONE', #39676, #98547, #85750, .T. ) ;
#47323 = CARTESIAN_POINT ( 'NONE',  ( 174.9358745049650565, 292.2217799751211942, 2.235529367806339263 ) ) ;
#47324 = CARTESIAN_POINT ( 'NONE',  ( 206.1062572280473546, 273.6604860535989587, -9.773577984388410300 ) ) ;
#47325 = DIRECTION ( 'NONE',  ( -0.8660254037844387076, -0.4999999999999998890, -0.000000000000000000 ) ) ;
#47326 = CARTESIAN_POINT ( 'NONE',  ( 80.31171660912499988, 46.24781510277671970, -12.29402398486336701 ) ) ;
#47327 = CARTESIAN_POINT ( 'NONE',  ( 199.3695014196146644, 285.3288893919889802, -18.21719466810020549 ) ) ;
#47328 = CARTESIAN_POINT ( 'NONE',  ( 71.38818891405433931, 59.36944044145746346, 15.71463273504962110 ) ) ;
#47329 = ORIENTED_EDGE ( 'NONE', *, *, #72071, .F. ) ;
#47331 = EDGE_CURVE ( 'NONE', #48909, #32826, #78601, .T. ) ;
#47330 = CARTESIAN_POINT ( 'NONE',  ( 194.4557758866845916, 293.8397116694720808, -14.23894577158402086 ) ) ;
#47332 = CARTESIAN_POINT ( 'NONE',  ( 74.68932948184826159, 66.80812537921995897, -13.13442079021221431 ) ) ;
#47333 = DIRECTION ( 'NONE',  ( -0.8660254037844387076, -0.4999999999999998890, -0.000000000000000000 ) ) ;
#47334 = CARTESIAN_POINT ( 'NONE',  ( 17.25242200676963833, 170.7677522451417929, -5.000000000000041744 ) ) ;
#47335 = CARTESIAN_POINT ( 'NONE',  ( 78.11742282250361313, 228.1589784336661353, -6.496448406907676862E-16 ) ) ;
#47336 = CARTESIAN_POINT ( 'NONE',  ( 82.33632248375091933, 40.34752097026218820, -1.014975778927596828 ) ) ;
#47337 = ADVANCED_FACE ( 'NONE', ( #17798 ), #10920, .F. ) ;
#47338 = PLANE ( 'NONE',  #66432 ) ;
#47339 = CARTESIAN_POINT ( 'NONE',  ( 170.0185468137966609, 280.2994163020263727, -13.67235037299359668 ) ) ;
#47341 = CARTESIAN_POINT ( 'NONE',  ( 75.67456858315887303, 65.42170317558291970, 14.28506259273864565 ) ) ;
#47340 = CARTESIAN_POINT ( 'NONE',  ( 14.19444334931225349, 172.8768266524160140, 9.188101187500098632 ) ) ;
#47342 = EDGE_CURVE ( 'NONE', #61372, #45744, #45243, .T. ) ;
#47343 = CARTESIAN_POINT ( 'NONE',  ( 200.5810378487751393, 283.2304467414622877, 18.38516374632547112 ) ) ;
#47344 = ORIENTED_EDGE ( 'NONE', *, *, #80604, .F. ) ;
#47346 = ORIENTED_EDGE ( 'NONE', *, *, #88798, .T. ) ;
#47345 = UNCERTAINTY_MEASURE_WITH_UNIT (LENGTH_MEASURE( 1.000000000000000082E-05 ), #60965, 'distance_accuracy_value', 'NONE');
#47347 = ADVANCED_FACE ( 'NONE', ( #29871 ), #83111, .F. ) ;
#47348 = PLANE ( 'NONE',  #85294 ) ;
#47349 = CARTESIAN_POINT ( 'NONE',  ( 81.67133165517434179, 46.72149670578906466, -12.10404611631500060 ) ) ;
#47350 = CARTESIAN_POINT ( 'NONE',  ( 83.90260833528412832, 43.42355591996152953, 6.759210671933336911 ) ) ;
#47351 = CARTESIAN_POINT ( 'NONE',  ( 47.78135487164287554, 106.4364430393875267, -10.00000000000000000 ) ) ;
#47352 = CARTESIAN_POINT ( 'NONE',  ( 94.05805000844996755, 215.1115022471902023, -5.000000000000041744 ) ) ;
#47353 = CARTESIAN_POINT ( 'NONE',  ( 74.27638480340351634, 67.89356557358171074, -11.69403406648106447 ) ) ;
#47354 = CARTESIAN_POINT ( 'NONE',  ( 32.08336737017582152, 180.1423013555409796, -4.594050593750043987 ) ) ;
#47355 = DIRECTION ( 'NONE',  ( -0.7713975076906485207, 0.000000000000000000, 0.6363535849892383300 ) ) ;
#47356 = VERTEX_POINT ( 'NONE', #91207 ) ;
#47357 = CARTESIAN_POINT ( 'NONE',  ( 30.40518283029366842, 188.3615022471902591, -10.00000000000009592 ) ) ;
#47358 = CARTESIAN_POINT ( 'NONE',  ( 182.6002590226659663, 260.6490965261490373, -10.86303761599557660 ) ) ;
#47359 = B_SPLINE_CURVE_WITH_KNOTS ( 'NONE', 3,
 ( #72536, #94346, #94841, #24407 ),
 .UNSPECIFIED., .F., .F.,
 ( 4, 4 ),
 ( 0.000000000000000000, 0.1734847945017928272 ),
 .UNSPECIFIED. ) ;
#47360 = CARTESIAN_POINT ( 'NONE',  ( -86.81108781737714253, -8.000000000000000000, 0.000000000000000000 ) ) ;
#47361 = CARTESIAN_POINT ( 'NONE',  ( -25.89332989531674301, 24.59406508915897760, -10.00000000000000000 ) ) ;
#47362 = FACE_OUTER_BOUND ( 'NONE', #80890, .T. ) ;
#47363 = CARTESIAN_POINT ( 'NONE',  ( 68.41462912126404206, 198.7592609112380728, 2.679491924311254714 ) ) ;
#47364 = CARTESIAN_POINT ( 'NONE',  ( 186.2368818158729198, 283.2115614060767825, 16.35907209874016388 ) ) ;
#47365 = CARTESIAN_POINT ( 'NONE',  ( 194.9757425430702824, 292.9391030023704161, -15.21392314336593365 ) ) ;
#47366 = VECTOR ( 'NONE', #16878, 1000.000000000000000 ) ;
#47367 = CARTESIAN_POINT ( 'NONE',  ( 192.2383246029743873, 265.0112368890651169, 7.772948199626619648 ) ) ;
#47368 = CARTESIAN_POINT ( 'NONE',  ( 168.0937730764468370, 278.6755643525841606, 14.89096657633803744 ) ) ;
#47369 = DIRECTION ( 'NONE',  ( 1.000000000000000000, 0.000000000000000000, -5.984665299743594308E-16 ) ) ;
#47370 = CARTESIAN_POINT ( 'NONE',  ( 68.20121996687745991, 67.65983906480657595, 7.773794612277492355 ) ) ;
#47371 = CARTESIAN_POINT ( 'NONE',  ( 148.3519871123208986, 273.6938162480936398, 8.180046468253793890 ) ) ;
#47372 = DIRECTION ( 'NONE',  ( 1.000000000000000000, 0.000000000000000000, 0.000000000000000000 ) ) ;
#47373 = ORIENTED_EDGE ( 'NONE', *, *, #71081, .T. ) ;
#47374 = CARTESIAN_POINT ( 'NONE',  ( 74.44098624100845996, 58.95453109306149031, 16.23807160063391208 ) ) ;
#47375 = CARTESIAN_POINT ( 'NONE',  ( 16.56913029798217352, 168.8262482093458061, 3.021315404115420679E-15 ) ) ;
#47376 = CARTESIAN_POINT ( 'NONE',  ( 109.5926410088830920, 224.8923013555410080, 4.594050593750050204 ) ) ;
#47377 = CARTESIAN_POINT ( 'NONE',  ( 8.301057521190555732, 26.83396525600388571, -2.839279412974133887 ) ) ;
#47379 = CARTESIAN_POINT ( 'NONE',  ( 150.7530568467738590, 269.5350414755053521, 15.60317050893315916 ) ) ;
#47378 = B_SPLINE_CURVE_WITH_KNOTS ( 'NONE', 3,
 ( #20607, #43880, #60562, #52981, #83930, #74821, #60069, #45374, #5401, #36285, #30180, #61068, #67184, #82934, #98108, #13509, #5892, #75311, #50981, #21597, #81934, #43382, #84917, #24077, #46358, #61569, #78295, #62056, #70675, #92517, #100105, #15460, #31660, #72581, #31167, #30689, #38260, #64454, #7374, #77803, #7893, #46878, #23065, #85949, #95414, #69173, #70165, #54971 ),
 .UNSPECIFIED., .F., .F.,
 ( 4, 2, 2, 2, 2, 2, 2, 2, 2, 2, 2, 2, 2, 2, 2, 2, 2, 2, 2, 2, 2, 2, 2, 4 ),
 ( 0.0001223504472693309937, 0.001139333269370160261, 0.001647824680420526336, 0.001902070385945734635, 0.002029193238708323823, 0.002156316091470912577, 0.002410561796996093121, 0.002664807502521273665, 0.003173298913571691564, 0.004190281735672526063, 0.005207264557773360995, 0.005715755968823742900, 0.005970001674348896122, 0.006224247379874050211, 0.006287808806255272380, 0.006351370232636494549, 0.006414931659017716718, 0.006478493085398939755, 0.006732738790923782461, 0.006986984496448626035, 0.007241230201973469609, 0.007495475907498313183, 0.007749721613023156756, 0.008258213024072825689 ),
 .UNSPECIFIED. ) ;
#47380 = CARTESIAN_POINT ( 'NONE',  ( 77.16803028340585513, 57.91059354089997413, -16.56554699001202025 ) ) ;
#47381 = CIRCLE ( 'NONE', #49071, 17.82106496071138224 ) ;
#47383 = CARTESIAN_POINT ( 'NONE',  ( 194.5245920682378369, 278.7753957560683489, 16.29798302962802126 ) ) ;
#47382 = CARTESIAN_POINT ( 'NONE',  ( 195.9920715006079490, 291.1787696107118677, 15.99608784761372071 ) ) ;
#47384 = DIRECTION ( 'NONE',  ( -0.8660254037844387076, -0.4999999999999998890, -0.000000000000000000 ) ) ;
#47385 = CARTESIAN_POINT ( 'NONE',  ( 193.1052853069701882, 263.5410494637605439, -5.234861273610968091 ) ) ;
#47386 = PLANE ( 'NONE',  #38025 ) ;
#47387 = CARTESIAN_POINT ( 'NONE',  ( 44.29582294825809896, 31.28920272979930672, -7.433330006724141015 ) ) ;
#47388 = CARTESIAN_POINT ( 'NONE',  ( 41.55205903992003158, 29.15404122711137447, 8.090169943749479842 ) ) ;
#47389 = DIRECTION ( 'NONE',  ( -0.9820299053580079374, -0.1887253692075927247, 0.000000000000000000 ) ) ;
#47390 = ORIENTED_EDGE ( 'NONE', *, *, #17228, .T. ) ;
#47391 = CARTESIAN_POINT ( 'NONE',  ( 191.1348134016154745, 266.6500986785706573, 10.84710269163073271 ) ) ;
#47392 = CARTESIAN_POINT ( 'NONE',  ( 179.0380341696543383, 280.7593727008336373, 16.07746832305279128 ) ) ;
#47393 = CARTESIAN_POINT ( 'NONE',  ( 196.6211565541474613, 267.8594331423399808, 9.474020388104994694 ) ) ;
#47394 = VERTEX_POINT ( 'NONE', #7064 ) ;
#47395 = CARTESIAN_POINT ( 'NONE',  ( 188.8639537394926720, 283.4252602687708986, -17.55272065613104715 ) ) ;
#47396 = CARTESIAN_POINT ( 'NONE',  ( 192.4888807200563292, 285.7021917670288644, -17.52758604510307450 ) ) ;
#47397 = CARTESIAN_POINT ( 'NONE',  ( 167.9549855348998335, 286.6226398335882095, 7.176453026111839328 ) ) ;
#47398 = CARTESIAN_POINT ( 'NONE',  ( 74.99443409587989606, 53.05053269064024590, -16.02027138122841876 ) ) ;
#47399 = CARTESIAN_POINT ( 'NONE',  ( 192.1149248854976861, 297.8941845364767005, 12.26771790733441314 ) ) ;
#47400 = ORIENTED_EDGE ( 'NONE', *, *, #95548, .T. ) ;
#47401 = CARTESIAN_POINT ( 'NONE',  ( 191.2550863981256271, 280.2068698123553645, 17.52853399581771399 ) ) ;
#47402 = CARTESIAN_POINT ( 'NONE',  ( 31.21403501649405854, 38.99752408145594273, 5.678558825948277544 ) ) ;
#47403 = EDGE_LOOP ( 'NONE', ( #89697, #26136, #24628, #31443 ) ) ;
#47404 = CARTESIAN_POINT ( 'NONE',  ( 78.44279992643997446, 61.32017871564067946, 16.22697472196324853 ) ) ;
#47405 = CARTESIAN_POINT ( 'NONE',  ( -13.51183432020139819, 142.4280072687214442, 0.000000000000000000 ) ) ;
#47406 = CARTESIAN_POINT ( 'NONE',  ( 107.6156973702194648, 244.4860189848785126, -2.679491924311252493 ) ) ;
#47408 = EDGE_CURVE ( 'NONE', #7177, #84862, #6505, .T. ) ;
#47407 = ORIENTED_EDGE ( 'NONE', *, *, #14912, .T. ) ;
#47409 = CARTESIAN_POINT ( 'NONE',  ( 86.54659259230355417, 47.35344409918261732, -10.80230753912618802 ) ) ;
#47410 = CARTESIAN_POINT ( 'NONE',  ( -22.42236680055709641, 157.8615022471902591, 0.000000000000000000 ) ) ;
#47411 = CARTESIAN_POINT ( 'NONE',  ( 163.7239493340838123, 247.0687966679708438, 6.286946239157660266 ) ) ;
#47412 = DIRECTION ( 'NONE',  ( 0.9140770918436947889, 0.4055404667435467680, 0.000000000000000000 ) ) ;
#47413 = FACE_OUTER_BOUND ( 'NONE', #12634, .T. ) ;
#47414 = CARTESIAN_POINT ( 'NONE',  ( 80.14677080614116278, 45.54587722633649349, -12.47700090210163104 ) ) ;
#47415 = DIRECTION ( 'NONE',  ( -0.000000000000000000, -0.000000000000000000, -1.000000000000000000 ) ) ;
#47416 = VERTEX_POINT ( 'NONE', #30372 ) ;
#47417 = EDGE_CURVE ( 'NONE', #18290, #75148, #53670, .T. ) ;
#47418 = ORIENTED_EDGE ( 'NONE', *, *, #75277, .T. ) ;
#47419 = CARTESIAN_POINT ( 'NONE',  ( 200.1038300618348273, 276.8705922012964606, -15.82546249815781181 ) ) ;
#47420 = EDGE_CURVE ( 'NONE', #47179, #71872, #83612, .T. ) ;
#47421 = VERTEX_POINT ( 'NONE', #28369 ) ;
#47422 = CARTESIAN_POINT ( 'NONE',  ( 77.27258907709742175, 49.66860660035752062, -15.49621856359588357 ) ) ;
#47423 = ORIENTED_EDGE ( 'NONE', *, *, #41241, .T. ) ;
#47424 = CARTESIAN_POINT ( 'NONE',  ( 86.95562746175168911, 45.78762616370607930, -8.653322509500107174 ) ) ;
#47425 = CARTESIAN_POINT ( 'NONE',  ( 203.4357368910538355, 278.2859629599173559, -16.45855118664066197 ) ) ;
#47426 = EDGE_LOOP ( 'NONE', ( #62411, #20796 ) ) ;
#47427 = CARTESIAN_POINT ( 'NONE',  ( 190.5325656458726087, 300.1042792322296009, -3.574822255195763798 ) ) ;
#47428 = CARTESIAN_POINT ( 'NONE',  ( 206.5431607373320730, 272.9037469775124691, -11.15649369879132102 ) ) ;
#47429 = CARTESIAN_POINT ( 'NONE',  ( 147.4587540121967209, 275.2409413605112718, -7.408606599236415846 ) ) ;
#47430 = CARTESIAN_POINT ( 'NONE',  ( 196.0380285978610289, 284.4171904029984717, -17.66719457817500682 ) ) ;
#47431 = CARTESIAN_POINT ( 'NONE',  ( 82.81294776526844714, 40.62066890938785946, 0.9850604075177307184 ) ) ;
#47432 = CARTESIAN_POINT ( 'NONE',  ( 167.6414094296473820, 249.1822265415601123, -5.393406076269569027 ) ) ;
#47433 = CYLINDRICAL_SURFACE ( 'NONE', #64698, 12.50000000000000000 ) ;
#47434 = CARTESIAN_POINT ( 'NONE',  ( 155.4191430981459519, 279.8345045701359481, 2.111987297901974703 ) ) ;
#47435 = CARTESIAN_POINT ( 'NONE',  ( 133.7059490715648167, 241.8768266524159856, 9.188101187500098632 ) ) ;
#47436 = CARTESIAN_POINT ( 'NONE',  ( 183.4116579307454913, 260.3025310349262327, -9.357811455373186149 ) ) ;
#47437 = CARTESIAN_POINT ( 'NONE',  ( 39.17063663036994114, 34.56628583063844928, 9.188101187500006262 ) ) ;
#47438 = VERTEX_POINT ( 'NONE', #68365 ) ;
#47440 = EDGE_LOOP ( 'NONE', ( #32005, #25103 ) ) ;
#47439 = CARTESIAN_POINT ( 'NONE',  ( 83.09463924182568917, 43.40643806361209300, -8.435373655842957064 ) ) ;
#47441 = DIRECTION ( 'NONE',  ( -0.5435407515102095299, 0.8393827800519358950, 0.000000000000000000 ) ) ;
#47442 = CARTESIAN_POINT ( 'NONE',  ( 180.8220585722234830, 256.2043429177185772, 1.036815351425113052 ) ) ;
#47443 = CARTESIAN_POINT ( 'NONE',  ( 165.2023837071825483, 246.1063600852122875, -2.838470414776972817 ) ) ;
#47444 = CARTESIAN_POINT ( 'NONE',  ( 192.3733747235286557, 297.4465362857985724, 11.01966089874153631 ) ) ;
#47445 = DIRECTION ( 'NONE',  ( 1.000000000000000000, 0.000000000000000000, 0.000000000000000000 ) ) ;
#47446 = CARTESIAN_POINT ( 'NONE',  ( 81.04401415297212452, 43.04793497936152846, 9.543169053269965119 ) ) ;
#47447 = CARTESIAN_POINT ( 'NONE',  ( 173.4984831628007953, 287.1903257367396805, -9.639986186396646062 ) ) ;
#47448 = CARTESIAN_POINT ( 'NONE',  ( 26.12309927540532328, 38.58029201028043076, 1.583844403245397769 ) ) ;
#47449 = CARTESIAN_POINT ( 'NONE',  ( 181.1060688601531297, 255.8911062559022298, -5.777534809724734544 ) ) ;
#47450 = ORIENTED_EDGE ( 'NONE', *, *, #84369, .F. ) ;
#47452 = EDGE_CURVE ( 'NONE', #7762, #21258, #30724, .T. ) ;
#47451 = CARTESIAN_POINT ( 'NONE',  ( 194.4826705584825390, 293.7931287314651740, -16.11258321617245315 ) ) ;
#47453 = CARTESIAN_POINT ( 'NONE',  ( 151.3107971817505586, 272.4644232592236790, 11.71674968251862836 ) ) ;
#47454 = CIRCLE ( 'NONE', #49128, 70.00000000000001421 ) ;
#47455 = ORIENTED_EDGE ( 'NONE', *, *, #47648, .T. ) ;
#47456 = CARTESIAN_POINT ( 'NONE',  ( 191.7826753266332673, 267.7942839150106238, -12.33540156790041742 ) ) ;
#47457 = VECTOR ( 'NONE', #45424, 1000.000000000000000 ) ;
#47458 = ADVANCED_FACE ( 'NONE', ( #91706 ), #22776, .F. ) ;
#47459 = CARTESIAN_POINT ( 'NONE',  ( 159.3291946290163992, 279.0199804063916531, 10.96233109238993109 ) ) ;
#47460 = CARTESIAN_POINT ( 'NONE',  ( 151.8373860759844831, 267.6569281583805946, -16.78611463437632167 ) ) ;
#47461 = CARTESIAN_POINT ( 'NONE',  ( 148.9498507103374152, 272.6582861203333437, 11.90061892622094852 ) ) ;
#47462 = CARTESIAN_POINT ( 'NONE',  ( 6.860117161356284576, 184.7677522451419065, -5.000000000000047962 ) ) ;
#47464 = CARTESIAN_POINT ( 'NONE',  ( 154.9357316289406015, 277.4855806559950224, -8.880802751379739846 ) ) ;
#47463 = CARTESIAN_POINT ( 'NONE',  ( 161.6287415102018770, 281.5831586784601654, -6.602482105918118904 ) ) ;
#47465 = DIRECTION ( 'NONE',  ( -0.8660254037844387076, -0.4999999999999998890, -0.000000000000000000 ) ) ;
#47466 = ORIENTED_EDGE ( 'NONE', *, *, #84316, .T. ) ;
#47467 = CARTESIAN_POINT ( 'NONE',  ( 204.6849407614616041, 272.9629571217342914, -9.743767658441230495 ) ) ;
#47468 = B_SPLINE_SURFACE_WITH_KNOTS ( 'NONE', 3, 1, ( 
 ( #88754, #4086 ),
 ( #96835, #89257 ),
 ( #27400, #19807 ),
 ( #50674, #81627 ),
 ( #7573, #68865 ),
 ( #15158, #52170 ),
 ( #22784, #38461 ),
 ( #92712, #84135 ),
 ( #22276, #82646 ),
 ( #30878, #46055 ),
 ( #68374, #92233 ),
 ( #13204, #76971 ),
 ( #60259, #61765 ),
 ( #44062, #21296 ),
 ( #98809, #53180 ),
 ( #67377, #45074 ),
 ( #13689, #91215 ),
 ( #44562, #100294 ),
 ( #14684, #45565 ),
 ( #29879, #23262 ),
 ( #21778, #75002 ),
 ( #52667, #61263 ),
 ( #83622, #83119 ),
 ( #76494, #5581 ),
 ( #76013, #69375 ),
 ( #37957, #99791 ),
 ( #7072, #30380 ),
 ( #84617, #36473 ),
 ( #98303, #53661 ),
 ( #59770, #28893 ),
 ( #90738, #14189 ),
 ( #75497, #6082 ),
 ( #36975, #60751 ),
 ( #67887, #29390 ) ),
 .UNSPECIFIED., .T., .F., .F.,
 ( 4, 2, 2, 2, 2, 2, 2, 2, 2, 2, 2, 2, 2, 2, 2, 2, 4 ),
 ( 2, 2 ),
 ( 0.000000000000000000, 0.06250000000000000000, 0.1250000000000000000, 0.1875000000000000000, 0.2500000000000000000, 0.3125000000000000000, 0.3750000000000000000, 0.4375000000000000000, 0.5000000000000000000, 0.5625000000000000000, 0.6250000000000000000, 0.6875000000000000000, 0.7500000000000000000, 0.8125000000000000000, 0.8750000000000000000, 0.9375000000000000000, 1.000000000000000000 ),
 ( 0.000000000000000000, 1.000000000000000000 ),
 .UNSPECIFIED. ) ;
#47469 = CARTESIAN_POINT ( 'NONE',  ( 73.40128984104008225, 64.43477936578551635, 14.11777066946370063 ) ) ;
#47470 = EDGE_CURVE ( 'NONE', #42192, #80375, #59246, .T. ) ;
#47471 = CARTESIAN_POINT ( 'NONE',  ( 192.5737543603648589, 275.7597456448726234, -15.97875861998497626 ) ) ;
#47472 = CARTESIAN_POINT ( 'NONE',  ( 144.7205361298395871, 254.3615022471902307, -10.00000000000009592 ) ) ;
#47473 = CARTESIAN_POINT ( 'NONE',  ( 197.2328925967401858, 274.3547493420543333, 15.41857190266785871 ) ) ;
#47474 = CARTESIAN_POINT ( 'NONE',  ( 192.5712965840290849, 297.1037255674836501, 11.03742858512898906 ) ) ;
#47475 = CARTESIAN_POINT ( 'NONE',  ( 74.41176536287696308, 68.30213538679808494, 11.88880159922067747 ) ) ;
#47476 = CARTESIAN_POINT ( 'NONE',  ( 73.79690245017815187, 68.46445494392735043, 10.93464038932060411 ) ) ;
#47477 = CARTESIAN_POINT ( 'NONE',  ( 69.79493031643249878, 70.93090587422946669, -0.9144303869529551987 ) ) ;
#47478 = CARTESIAN_POINT ( 'NONE',  ( -8.349714312657674498, 175.1744531367911293, 4.594050593750047540 ) ) ;
#47479 = CARTESIAN_POINT ( 'NONE',  ( 98.19890751640281223, 221.3768266524159856, -9.188101187500091527 ) ) ;
#47480 = CARTESIAN_POINT ( 'NONE',  ( 155.5587153255869453, 261.2113968263770971, -18.30500480654006878 ) ) ;
#47481 = CARTESIAN_POINT ( 'NONE',  ( 192.6170194583582429, 297.0245312260774995, -11.90166228306590490 ) ) ;
#47482 = CYLINDRICAL_SURFACE ( 'NONE', #86844, 70.00000000000002842 ) ;
#47483 = CARTESIAN_POINT ( 'NONE',  ( 202.7602807045765019, 279.4558873931827065, -15.90558713185497020 ) ) ;
#47484 = CARTESIAN_POINT ( 'NONE',  ( 78.63106618800820513, 59.04553955275220289, 16.18459533489969360 ) ) ;
#47485 = CARTESIAN_POINT ( 'NONE',  ( 84.52323392980522954, 49.80928010723963695, -13.22128011046212670 ) ) ;
#47486 = CARTESIAN_POINT ( 'NONE',  ( 78.19610093930316452, 61.82192816133139956, 15.73638231904944718 ) ) ;
#47488 = CARTESIAN_POINT ( 'NONE',  ( -20.78562219458220284, 95.22657743062728741, 45.19937630303414267 ) ) ;
#47487 = PLANE ( 'NONE',  #71065 ) ;
#47489 = CARTESIAN_POINT ( 'NONE',  ( 180.5623436295364854, 290.8789022247497087, 9.334073381727758800 ) ) ;
#47490 = CARTESIAN_POINT ( 'NONE',  ( 169.2406489442459190, 252.1939778885328849, -9.400937777832105269 ) ) ;
#47491 = CARTESIAN_POINT ( 'NONE',  ( 204.7998534689117491, 275.9232437396207729, -13.00948150499847067 ) ) ;
#47492 = CARTESIAN_POINT ( 'NONE',  ( 196.0034224882197975, 291.1591091234520263, 17.53794140922627776 ) ) ;
#47493 = LINE ( 'NONE', #70809, #44678 ) ;
#47494 = ADVANCED_FACE ( 'NONE', ( #5085 ), #53172, .F. ) ;
#47495 = CARTESIAN_POINT ( 'NONE',  ( 207.4541616930702617, 271.3258470364304458, -6.834942797545373594 ) ) ;
#47496 = CARTESIAN_POINT ( 'NONE',  ( 46.18343024948246978, 185.2202760586659736, -5.415160957724236172E-17 ) ) ;
#47497 = EDGE_CURVE ( 'NONE', #31208, #32891, #89973, .T. ) ;
#47498 = CARTESIAN_POINT ( 'NONE',  ( 67.34675250658217749, 203.5643266524159856, -9.188101187500093303 ) ) ;
#47499 = CARTESIAN_POINT ( 'NONE',  ( 61.58209736653347477, 206.3615022471902307, -10.00000000000009592 ) ) ;
#47500 = B_SPLINE_CURVE_WITH_KNOTS ( 'NONE', 3,
 ( #58128, #73841, #27742, #58610, #89586, #20149, #81971, #67222, #22624, #7410, #98147, #44416, #15003, #98653, #60597, #52030, #28732, #36818, #91553 ),
 .UNSPECIFIED., .F., .F.,
 ( 4, 2, 2, 2, 1, 2, 2, 2, 2, 4 ),
 ( 0.4743041966560226363, 0.5400161720740214166, 0.6057281474920201969, 0.6385841352010184213, 0.6714401229100168678, 0.7371520983280135386, 0.8028640737460100985, 0.8685760491640068803, 0.9342880245820035512, 1.000000000000000000 ),
 .UNSPECIFIED. ) ;
#47501 = CARTESIAN_POINT ( 'NONE',  ( 88.21238909966383801, 43.70556102481675964, 0.1923655077720384798 ) ) ;
#47502 = CARTESIAN_POINT ( 'NONE',  ( 166.7607585703058817, 259.6620056817021123, 15.79927695026398382 ) ) ;
#47503 = CARTESIAN_POINT ( 'NONE',  ( 71.76465953926796715, 72.09915442159702081, -3.621776363507912766 ) ) ;
#47504 = CARTESIAN_POINT ( 'NONE',  ( 196.2630425146829225, 269.4134538897955622, -10.69405362647414925 ) ) ;
#47505 = CARTESIAN_POINT ( 'NONE',  ( 33.66714878060290772, 21.29860640527294180, -2.839279412974138328 ) ) ;
#47506 = CARTESIAN_POINT ( 'NONE',  ( 150.6815632051821581, 269.6588720951601772, -14.68790257316217307 ) ) ;
#47507 = CARTESIAN_POINT ( 'NONE',  ( 81.93674055385325516, 47.28776839916499597, -12.40202553389867823 ) ) ;
#47508 = CARTESIAN_POINT ( 'NONE',  ( 12.04840505635704417, 25.14336893147754282, 7.433330006724141015 ) ) ;
#47509 = CARTESIAN_POINT ( 'NONE',  ( 74.43750904794978851, 201.5327760586659167, 1.948934522072302763E-15 ) ) ;
#47510 = CARTESIAN_POINT ( 'NONE',  ( 76.67587641197377479, 63.85108742147927074, 14.86537621106540819 ) ) ;
#47511 = CARTESIAN_POINT ( 'NONE',  ( 155.3716771045260714, 261.5353565282119348, -18.54934131471355840 ) ) ;
#47512 = CARTESIAN_POINT ( 'NONE',  ( 198.6562788533279615, 286.5642271139020636, 17.47134757795404525 ) ) ;
#47513 = CARTESIAN_POINT ( 'NONE',  ( 48.86234924490155862, 209.0177522451419065, 5.000000000000046185 ) ) ;
#47514 = CARTESIAN_POINT ( 'NONE',  ( 198.9730007453206042, 281.0620181772907245, 17.36568714939058822 ) ) ;
#47515 =( BOUNDED_CURVE ( )  B_SPLINE_CURVE ( 2, ( #65314, #79051, #9640, #87193, #25309, #19248, #49122, #26817, #87694 ),
 .UNSPECIFIED., .F., .T. ) 
 B_SPLINE_CURVE_WITH_KNOTS ( ( 3, 2, 2, 2, 3 ),
 ( 0.6733870967741935054, 0.6747311827956988806, 0.6774193548387096309, 0.6801075268817203812, 0.6814516129032257563 ),
 .UNSPECIFIED. ) 
 CURVE ( )  GEOMETRIC_REPRESENTATION_ITEM ( )  RATIONAL_B_SPLINE_CURVE ( ( 0.9330127018922194093, 0.9330127018922194093, 1.000000000000000000, 0.8660254037844387076, 1.000000000000000000, 0.8660254037844387076, 1.000000000000000000, 0.9330127018922194093, 0.9330127018922194093 ) ) 
 REPRESENTATION_ITEM ( '' )  );
#47516 = AXIS2_PLACEMENT_3D ( 'NONE', #82621, #13184, #53155 ) ;
#47517 = CARTESIAN_POINT ( 'NONE',  ( 74.58224166234337815, 56.98362197102031956, -16.05243990554664890 ) ) ;
#47518 = CARTESIAN_POINT ( 'NONE',  ( 114.4096469973842858, 226.8615022471902023, 5.000000000000051514 ) ) ;
#47519 = LINE ( 'NONE', #23215, #24121 ) ;
#47520 = ORIENTED_EDGE ( 'NONE', *, *, #39834, .F. ) ;
#47521 = CARTESIAN_POINT ( 'NONE',  ( 77.63908229418555607, 49.31861150414459871, 15.29991512875208137 ) ) ;
#47522 = CARTESIAN_POINT ( 'NONE',  ( 186.6564022441646671, 272.5344008312805499, 15.68346972453315402 ) ) ;
#47523 = ORIENTED_EDGE ( 'NONE', *, *, #6392, .F. ) ;
#47524 = CARTESIAN_POINT ( 'NONE',  ( 159.2394649670193303, 254.8361514374751664, -16.43133403737800791 ) ) ;
#47525 = CARTESIAN_POINT ( 'NONE',  ( 193.7402390244666606, 294.2808330005247512, 13.97520787983859236 ) ) ;
#47526 = CARTESIAN_POINT ( 'NONE',  ( 72.07913036110144844, 68.84169458634234218, -9.362130312896965734 ) ) ;
#47527 = VERTEX_POINT ( 'NONE', #74994 ) ;
#47528 = CARTESIAN_POINT ( 'NONE',  ( 168.1726423428391399, 255.4859975196775963, 14.21197738914692366 ) ) ;
#47529 = VERTEX_POINT ( 'NONE', #5573 ) ;
#47530 = CARTESIAN_POINT ( 'NONE',  ( 65.93560523737669143, 69.04367854582200437, -2.085430103607250008 ) ) ;
#47531 = CARTESIAN_POINT ( 'NONE',  ( 148.3629184514745987, 273.6748826132846375, -8.219814532462343948 ) ) ;
#47532 = CARTESIAN_POINT ( 'NONE',  ( 148.4666013490241596, 274.0772673839664435, 7.858165846707668045 ) ) ;
#47533 = ORIENTED_EDGE ( 'NONE', *, *, #69640, .F. ) ;
#47534 = CARTESIAN_POINT ( 'NONE',  ( 22.00590953607929023, 34.74646525600390845, 2.839279412974139660 ) ) ;
#47535 = CARTESIAN_POINT ( 'NONE',  ( -13.11024591527723615, 15.00000000000000000, -40.00000000000016342 ) ) ;
#47536 = CARTESIAN_POINT ( 'NONE',  ( 74.73078456835838779, 66.79972942087577792, -13.15602295301254721 ) ) ;
#47537 = CARTESIAN_POINT ( 'NONE',  ( 79.26897965571234295, 49.31431488444046352, -14.41357357798955974 ) ) ;
#47538 = VERTEX_POINT ( 'NONE', #98295 ) ;
#47540 = EDGE_CURVE ( 'NONE', #81228, #60097, #24273, .T. ) ;
#47539 = DIRECTION ( 'NONE',  ( -0.8660254037844378194, -0.5000000000000014433, -0.000000000000000000 ) ) ;
#47541 = CARTESIAN_POINT ( 'NONE',  ( 173.6836341738550971, 260.0703094413875647, 15.05886286463676349 ) ) ;
#47542 = EDGE_CURVE ( 'NONE', #7044, #21557, #66948, .T. ) ;
#47543 = VERTEX_POINT ( 'NONE', #46552 ) ;
#47544 = CARTESIAN_POINT ( 'NONE',  ( 170.9926132455484264, 284.6176199787537939, 10.85232337705370576 ) ) ;
#47546 = CARTESIAN_POINT ( 'NONE',  ( 68.03752145569828258, 65.19644328924185572, -10.68142545458115933 ) ) ;
#47545 = CARTESIAN_POINT ( 'NONE',  ( 67.87593105113009528, 65.67175317894806597, 10.83526793861203430 ) ) ;
#47547 = CARTESIAN_POINT ( 'NONE',  ( 81.78126323850756307, 55.46774195332329782, -15.94567292164773420 ) ) ;
#47548 = CARTESIAN_POINT ( 'NONE',  ( 155.6518451030846961, 261.0500913200531841, 17.91778754207898317 ) ) ;
#47549 = CARTESIAN_POINT ( 'NONE',  ( 185.6025440602765002, 292.7411672476788453, -10.71517798447736425 ) ) ;
#47550 = CARTESIAN_POINT ( 'NONE',  ( 157.2104826425669728, 258.3504519110855995, -16.92635148710569482 ) ) ;
#47551 = CARTESIAN_POINT ( 'NONE',  ( 148.5637841791828464, 247.3923013555409796, 4.594050593750050204 ) ) ;
#47552 = CARTESIAN_POINT ( 'NONE',  ( 89.16490563351598553, 155.8911630683315934, 0.000000000000000000 ) ) ;
#47553 = CARTESIAN_POINT ( 'NONE',  ( 79.15819921557465477, 59.82093924937031204, 16.50069780760281901 ) ) ;
#47554 = CARTESIAN_POINT ( 'NONE',  ( 96.71051312758956442, 217.4548013555409511, -4.594050593750042211 ) ) ;
#47555 = ORIENTED_EDGE ( 'NONE', *, *, #41313, .F. ) ;
#47556 = CARTESIAN_POINT ( 'NONE',  ( 190.8604783348975502, 300.0669496974951471, 7.597731640149610222 ) ) ;
#47557 = LINE ( 'NONE', #9587, #77089 ) ;
#47558 = CARTESIAN_POINT ( 'NONE',  ( 77.99937045744943021, 62.11896432438783933, -16.00068414206377554 ) ) ;
#47559 = VERTEX_POINT ( 'NONE', #7563 ) ;
#47560 = CARTESIAN_POINT ( 'NONE',  ( 156.7527532867754019, 259.1432624114326586, -17.18866891080081416 ) ) ;
#47561 = ORIENTED_EDGE ( 'NONE', *, *, #7635, .T. ) ;
#47562 = ORIENTED_EDGE ( 'NONE', *, *, #38263, .F. ) ;
#47563 = CARTESIAN_POINT ( 'NONE',  ( 80.02183673286208432, 44.83754558038893379, -11.27937077477422356 ) ) ;
#47564 = FACE_OUTER_BOUND ( 'NONE', #92537, .T. ) ;
#47565 = DIRECTION ( 'NONE',  ( -1.000000000000000000, 0.000000000000000000, 0.000000000000000000 ) ) ;
#47566 = CYLINDRICAL_SURFACE ( 'NONE', #59543, 17.82106496071139645 ) ;
#47567 = CARTESIAN_POINT ( 'NONE',  ( 79.84557217427597209, 48.50462519541254380, -13.88470291381558219 ) ) ;
#47568 = CARTESIAN_POINT ( 'NONE',  ( 207.6470076888861342, 270.9918279736407385, 2.882721586646819212 ) ) ;
#47569 = CARTESIAN_POINT ( 'NONE',  ( 83.25962220535622293, 225.0024278399160664, -9.188101187500093303 ) ) ;
#47570 = VERTEX_POINT ( 'NONE', #32368 ) ;
#47571 = ORIENTED_EDGE ( 'NONE', *, *, #28876, .T. ) ;
#47572 = ADVANCED_FACE ( 'NONE', ( #54648 ), #56990, .F. ) ;
#47573 = CARTESIAN_POINT ( 'NONE',  ( 200.5761841437080193, 283.2388536052437757, -18.29075185947827364 ) ) ;
#47574 = ORIENTED_EDGE ( 'NONE', *, *, #71251, .F. ) ;
#47575 = DIRECTION ( 'NONE',  ( 0.4330127018922168558, -0.7499999999999987788, 0.5000000000000039968 ) ) ;
#47576 = CARTESIAN_POINT ( 'NONE',  ( 204.8008807586744524, 272.7600038595665524, -10.89009281376315741 ) ) ;
#47577 = CARTESIAN_POINT ( 'NONE',  ( 22.87232021560678064, 28.90829794293881605, 10.00000000000000355 ) ) ;
#47578 = CARTESIAN_POINT ( 'NONE',  ( 161.6188153416260604, 283.9408672562620950, 0.5238794243677475926 ) ) ;
#47579 = FACE_OUTER_BOUND ( 'NONE', #1926, .T. ) ;
#47580 = CARTESIAN_POINT ( 'NONE',  ( 88.03991489039286478, 44.69748799199468436, 4.347629997315069161 ) ) ;
#47581 = ORIENTED_EDGE ( 'NONE', *, *, #15768, .T. ) ;
#47582 = CARTESIAN_POINT ( 'NONE',  ( 190.1843253477620408, 295.3820500736599115, 11.30047355920397223 ) ) ;
#47583 = LINE ( 'NONE', #31385, #75577 ) ;
#47584 = CARTESIAN_POINT ( 'NONE',  ( 159.5221561062548972, 254.3465160214695118, -16.91023001054109542 ) ) ;
#47585 = CARTESIAN_POINT ( 'NONE',  ( 147.8939059469516621, 275.2579607316754959, -4.845476154560380166 ) ) ;
#47586 = DIRECTION ( 'NONE',  ( -0.8660254037844387076, -0.4999999999999998890, -0.000000000000000000 ) ) ;
#47587 = CARTESIAN_POINT ( 'NONE',  ( 110.7831656154890254, 224.7677522451417929, -5.000000000000041744 ) ) ;
#47588 = VECTOR ( 'NONE', #16975, 1000.000000000000000 ) ;
#47589 = CARTESIAN_POINT ( 'NONE',  ( 195.6387348270936002, 279.6800705220005057, -17.43641212817176722 ) ) ;
#47590 = EDGE_LOOP ( 'NONE', ( #50439, #89600, #76857, #24051 ) ) ;
#47591 = CARTESIAN_POINT ( 'NONE',  ( -2.524136441754524451, 180.8967562850347406, 2.649461200531984646E-14 ) ) ;
#47592 = CARTESIAN_POINT ( 'NONE',  ( 161.3227470381586102, 251.2278010437646856, 14.45097375514160731 ) ) ;
#47593 = CARTESIAN_POINT ( 'NONE',  ( 83.75763820169687790, 42.17253232718462641, 3.815062152321099465 ) ) ;
#47594 = CARTESIAN_POINT ( 'NONE',  ( 187.8464235218109195, 266.1023814865406507, -11.84412950951504229 ) ) ;
#47595 = DIRECTION ( 'NONE',  ( -0.8660254037844387076, -0.4999999999999998890, -0.000000000000000000 ) ) ;
#47596 = CARTESIAN_POINT ( 'NONE',  ( 46.43574122514302616, 74.10519008736565638, -10.00000000000000000 ) ) ;
#47597 = EDGE_LOOP ( 'NONE', ( #80511, #56434, #78783, #62880 ) ) ;
#47598 = VECTOR ( 'NONE', #33846, 1000.000000000000114 ) ;
#47599 = CARTESIAN_POINT ( 'NONE',  ( 202.4900219881211854, 279.9239892212719383, 15.63116161057562259 ) ) ;
#47600 = ADVANCED_FACE ( 'NONE', ( #59008 ), #33368, .T. ) ;
#47601 = CARTESIAN_POINT ( 'NONE',  ( 207.4764081617721843, 271.2873150223495600, 6.359972247200924578 ) ) ;
#47603 = DIRECTION ( 'NONE',  ( 0.5000000000000014433, -0.8660254037844378194, 0.000000000000000000 ) ) ;
#47602 = CARTESIAN_POINT ( 'NONE',  ( 194.5047661587782386, 293.7548580291293092, 14.86680123054176583 ) ) ;
#47604 = CARTESIAN_POINT ( 'NONE',  ( 69.93344588439701681, 62.81717858415346001, -13.32880143434356235 ) ) ;
#47605 = CARTESIAN_POINT ( 'NONE',  ( 24.93549151006825326, 33.13478043621389446, 8.090169943749478065 ) ) ;
#47606 = CARTESIAN_POINT ( 'NONE',  ( 172.1884445069138678, 275.0993914995688669, 16.85348085832728060 ) ) ;
#47607 = CARTESIAN_POINT ( 'NONE',  ( 163.2958758767942697, 283.7880877081312292, -3.557553060821605939 ) ) ;
#47608 = DIRECTION ( 'NONE',  ( 0.5000000000000013323, -0.8660254037844378194, 0.000000000000000000 ) ) ;
#47609 = B_SPLINE_CURVE_WITH_KNOTS ( 'NONE', 3,
 ( #77361, #44448, #75381, #60140, #21668, #52548, #83500, #47443, #9463, #850 ),
 .UNSPECIFIED., .F., .F.,
 ( 4, 2, 2, 2, 4 ),
 ( 0.001342876365094863422, 0.001763185234570876624, 0.002183494104046890261, 0.002603802973522903463, 0.003024111842998916666 ),
 .UNSPECIFIED. ) ;
#47610 = CARTESIAN_POINT ( 'NONE',  ( 191.1700880229242614, 262.1676510039363279, 2.914548928543342576 ) ) ;
#47611 = CARTESIAN_POINT ( 'NONE',  ( 161.8935665241663457, 250.2391126920490194, -13.69501063978231770 ) ) ;
#47612 = CARTESIAN_POINT ( 'NONE',  ( 2.394847222749281190, 166.0643266524160140, -9.188101187500093303 ) ) ;
#47613 = CARTESIAN_POINT ( 'NONE',  ( 82.65478504301806595, 49.50942564885856711, 13.62198326750848310 ) ) ;
#47614 = EDGE_LOOP ( 'NONE', ( #55692, #70882, #19941, #31459 ) ) ;
#47615 = CARTESIAN_POINT ( 'NONE',  ( 175.6243877072629402, 255.6581301832358122, 8.239597966241703375 ) ) ;
#47616 = DIRECTION ( 'NONE',  ( 0.1162373735601425762, 0.9932214622066117826, 0.000000000000000000 ) ) ;
#47617 = CARTESIAN_POINT ( 'NONE',  ( 81.84418131458886592, 41.19320572020597382, 5.701826843178367632 ) ) ;
#47618 = CARTESIAN_POINT ( 'NONE',  ( 16.87327557256410060, 189.7369531367911293, -4.594050593750048428 ) ) ;
#47619 = CARTESIAN_POINT ( 'NONE',  ( 181.7508493730100554, 276.2066116400742999, -17.76433735679825432 ) ) ;
#47620 = CARTESIAN_POINT ( 'NONE',  ( 27.37348498259797935, 38.73705186507756082, -3.090169943749475845 ) ) ;
#47621 = CARTESIAN_POINT ( 'NONE',  ( 128.3382222415839635, 238.2365022471902307, 10.00000000000009948 ) ) ;
#47622 = CARTESIAN_POINT ( 'NONE',  ( 173.4424205204250882, 272.5764413300324804, -16.36125399428295779 ) ) ;
#47623 = CARTESIAN_POINT ( 'NONE',  ( 73.80638704669730998, 68.31061168272385942, -11.57820046455322505 ) ) ;
#47624 = DIRECTION ( 'NONE',  ( 0.4999999999999998890, -0.8660254037844385966, 0.000000000000000000 ) ) ;
#47625 = CARTESIAN_POINT ( 'NONE',  ( 186.8357342210453851, 295.8110015290263277, -7.913238257363107486 ) ) ;
#47626 = CARTESIAN_POINT ( 'NONE',  ( 190.3064699681596608, 261.7168245545821037, -0.7557934191962326631 ) ) ;
#47627 = CARTESIAN_POINT ( 'NONE',  ( 74.50030963965139108, 200.4865022471901739, 1.119607411625061291E-15 ) ) ;
#47628 = CARTESIAN_POINT ( 'NONE',  ( 74.14183300149377942, 66.03016674703368949, -12.94810846154004302 ) ) ;
#47629 = CARTESIAN_POINT ( 'NONE',  ( 203.5904874318909492, 269.7020407831449802, 7.034387229931597929 ) ) ;
#47630 = CARTESIAN_POINT ( 'NONE',  ( 31.75860784375665702, 179.9548013555409796, -4.594050593750042211 ) ) ;
#47631 = FACE_OUTER_BOUND ( 'NONE', #8318, .T. ) ;
#47632 = CARTESIAN_POINT ( 'NONE',  ( 202.9930240272727815, 270.0243998824601590, -6.379419799043575701 ) ) ;
#47633 = CARTESIAN_POINT ( 'NONE',  ( 198.8533049117289977, 286.2229679703367538, -18.60939981449148561 ) ) ;
#47634 = CARTESIAN_POINT ( 'NONE',  ( 67.04476328957329656, 66.83327842152489495, -8.922081757671701752 ) ) ;
#47635 = CARTESIAN_POINT ( 'NONE',  ( 66.22544472841278207, 69.36168339246577830, 0.1681495645362227065 ) ) ;
#47636 = LINE ( 'NONE', #45632, #97877 ) ;
#47637 = LINE ( 'NONE', #93283, #92495 ) ;
#47638 = CARTESIAN_POINT ( 'NONE',  ( 27.42516030814984163, 18.76004757982090609, 5.678558825948272215 ) ) ;
#47639 = CARTESIAN_POINT ( 'NONE',  ( 202.4943568615953779, 279.9164810001701085, 17.09064351659286984 ) ) ;
#47640 = CARTESIAN_POINT ( 'NONE',  ( 149.4456112649506281, 271.7996036513546869, -12.95648166494593667 ) ) ;
#47641 = CARTESIAN_POINT ( 'NONE',  ( 185.6350556674202892, 267.8156451814128332, -14.47898365169702828 ) ) ;
#47642 = ORIENTED_EDGE ( 'NONE', *, *, #63312, .F. ) ;
#47643 = CARTESIAN_POINT ( 'NONE',  ( 185.5630754609182986, 290.7785217972672172, 12.70007870419082430 ) ) ;
#47644 = CARTESIAN_POINT ( 'NONE',  ( 195.2466578971736908, 263.4181923903869915, -3.779627582060766322 ) ) ;
#47645 = CARTESIAN_POINT ( 'NONE',  ( 71.61159621314317292, 72.40963678617121957, -1.342178375522450562 ) ) ;
#47646 = CARTESIAN_POINT ( 'NONE',  ( 25.13686162393831225, 191.9865022471903160, -10.00000000000009592 ) ) ;
#47648 = EDGE_CURVE ( 'NONE', #51005, #47892, #28628, .T. ) ;
#47647 = CARTESIAN_POINT ( 'NONE',  ( 72.26191451101281871, 71.91445694603925176, -5.118044210176697639 ) ) ;
#47649 = CARTESIAN_POINT ( 'NONE',  ( 191.3638605175971747, 299.1950661814348678, 7.382965314423603154 ) ) ;
#47650 = CARTESIAN_POINT ( 'NONE',  ( 178.5653124836910877, 256.7979852036974080, -7.281116805671778991 ) ) ;
#47651 = AXIS2_PLACEMENT_3D ( 'NONE', #95609, #57034, #18566 ) ;
#47652 = EDGE_CURVE ( 'NONE', #33225, #62454, #2941, .T. ) ;
#47653 = EDGE_LOOP ( 'NONE', ( #72524, #83462, #46315 ) ) ;
#47654 = ORIENTED_EDGE ( 'NONE', *, *, #10351, .F. ) ;
#47656 = CARTESIAN_POINT ( 'NONE',  ( 83.32680864440213497, 42.44806103200585312, -5.336843269292388392 ) ) ;
#47655 = DIRECTION ( 'NONE',  ( 0.5000000000000013323, -0.8660254037844378194, 0.000000000000000000 ) ) ;
#47657 = VERTEX_POINT ( 'NONE', #75750 ) ;
#47658 = LINE ( 'NONE', #87750, #95232 ) ;
#47659 = EDGE_CURVE ( 'NONE', #49332, #52913, #6334, .T. ) ;
#47660 = CARTESIAN_POINT ( 'NONE',  ( 71.68807920414248258, 72.06984970416017688, -3.563505611461031286 ) ) ;
#47661 = FACE_OUTER_BOUND ( 'NONE', #75600, .T. ) ;
#47662 = CARTESIAN_POINT ( 'NONE',  ( 5.995650155809629567, 19.16454794089039382, -10.00000000000000355 ) ) ;
#47664 = EDGE_CURVE ( 'NONE', #88081, #3978, #65242, .T. ) ;
#47663 = CARTESIAN_POINT ( 'NONE',  ( 148.3190727836317535, 273.7508255376806119, 8.080277324579027365 ) ) ;
#47665 = AXIS2_PLACEMENT_3D ( 'NONE', #48666, #17766, #18267 ) ;
#47666 = CARTESIAN_POINT ( 'NONE',  ( 180.7465490385022520, 287.0650312162388786, -13.47353663417578673 ) ) ;
#47667 = ORIENTED_EDGE ( 'NONE', *, *, #80380, .F. ) ;
#47668 = DIRECTION ( 'NONE',  ( 1.000000000000000000, 0.000000000000000000, 0.000000000000000000 ) ) ;
#47669 = CARTESIAN_POINT ( 'NONE',  ( 172.4419760422836134, 290.9306500000749907, -0.6531725299933459628 ) ) ;
#47670 = VERTEX_POINT ( 'NONE', #17657 ) ;
#47671 = CARTESIAN_POINT ( 'NONE',  ( 27.31210279805776509, 33.95586893147756768, 7.433330006724141015 ) ) ;
#47672 = CARTESIAN_POINT ( 'NONE',  ( 159.6610344727618269, 254.1059716346071866, 15.33388637456589620 ) ) ;
#47673 = CARTESIAN_POINT ( 'NONE',  ( 50.35065686154756293, 206.0024278399161233, 9.188101187500095079 ) ) ;
#47674 = CARTESIAN_POINT ( 'NONE',  ( 74.38015889281619764, 68.44084013566667579, 11.75477996513195933 ) ) ;
#47675 = CARTESIAN_POINT ( 'NONE',  ( 159.5503045904109740, 254.6834971896836919, 15.44555384949675236 ) ) ;
#47676 = CARTESIAN_POINT ( 'NONE',  ( 86.94711308317737064, 232.5530062829863027, -4.648177544792955347E-16 ) ) ;
#47677 = CARTESIAN_POINT ( 'NONE',  ( -17.42236680055705023, 149.2012482093457777, 0.000000000000000000 ) ) ;
#47678 = ORIENTED_EDGE ( 'NONE', *, *, #55408, .F. ) ;
#47679 = CARTESIAN_POINT ( 'NONE',  ( 189.7094295309238419, 300.0606247079692253, 5.078421157105148076 ) ) ;
#47680 = CARTESIAN_POINT ( 'NONE',  ( 48.32408078245681793, 82.80331927372955647, -10.00000000000000000 ) ) ;
#47681 = CARTESIAN_POINT ( 'NONE',  ( 168.2925188335944711, 279.9374692537770102, 14.50896303939727261 ) ) ;
#47682 = VERTEX_POINT ( 'NONE', #11068 ) ;
#47683 = CARTESIAN_POINT ( 'NONE',  ( 175.1988943574488644, 261.2637229863152015, -14.23086624307204850 ) ) ;
#47684 = CARTESIAN_POINT ( 'NONE',  ( 59.87444983769439943, 192.0767206835448633, -1.126254757482173519E-14 ) ) ;
#47685 = DIRECTION ( 'NONE',  ( 0.4999999999999998890, -0.8660254037844385966, 0.000000000000000000 ) ) ;
#47686 = CARTESIAN_POINT ( 'NONE',  ( 147.5851099763508216, 275.0220864107570264, -4.372720440640867956 ) ) ;
#47687 = CARTESIAN_POINT ( 'NONE',  ( 149.7119746935222793, 271.3382486597900538, 12.05352563709836922 ) ) ;
#47688 = CARTESIAN_POINT ( 'NONE',  ( 177.2704016510258782, 269.4991140589317524, 16.10227469079067220 ) ) ;
#47689 = VECTOR ( 'NONE', #74949, 1000.000000000000000 ) ;
#47690 = CARTESIAN_POINT ( 'NONE',  ( 164.9103019330012216, 245.0139736909548560, 2.841678961959298810 ) ) ;
#47691 = CARTESIAN_POINT ( 'NONE',  ( 76.20055470335279324, 65.09253202017347917, 14.18943646504600054 ) ) ;
#47692 = CARTESIAN_POINT ( 'NONE',  ( 69.34698985851524355, 65.60308984842636448, -11.02141108540449288 ) ) ;
#47693 = CARTESIAN_POINT ( 'NONE',  ( -22.42236680055709641, 157.8615022471902591, 0.000000000000000000 ) ) ;
#47694 = CARTESIAN_POINT ( 'NONE',  ( 101.8248682511026573, 241.8464784336661353, 1.353441290958777327E-15 ) ) ;
#47695 = EDGE_LOOP ( 'NONE', ( #22423, #25473, #95941, #62358 ) ) ;
#47696 = CARTESIAN_POINT ( 'NONE',  ( 191.7247331938518187, 298.5700163710982338, -9.650650827884682315 ) ) ;
#47697 = CARTESIAN_POINT ( 'NONE',  ( 22.90194105960797089, 172.4824982072973967, 3.021315404115420679E-15 ) ) ;
#47698 = CARTESIAN_POINT ( 'NONE',  ( 154.9903553346911735, 262.1958252075976361, -18.39016733948542637 ) ) ;
#47699 = CARTESIAN_POINT ( 'NONE',  ( 182.8460422257451512, 285.5338780432256272, -15.29722646433579492 ) ) ;
#47700 = CARTESIAN_POINT ( 'NONE',  ( 83.83309058964263727, 51.93283190383716885, -14.92096955093740362 ) ) ;
#47701 = CARTESIAN_POINT ( 'NONE',  ( 174.9976167624121501, 253.1009688407763178, 5.034851627924513018 ) ) ;
#47702 = VERTEX_POINT ( 'NONE', #18155 ) ;
#47703 = CARTESIAN_POINT ( 'NONE',  ( 162.8223739550644211, 248.6303710312858186, -11.16939803179192658 ) ) ;
#47704 = CARTESIAN_POINT ( 'NONE',  ( 19.18375657693640335, 36.32959363016014720, 10.00000000000000000 ) ) ;
#47705 = CARTESIAN_POINT ( 'NONE',  ( 185.2286309111798914, 261.0640975966447286, 10.24933178681469137 ) ) ;
#47706 = CARTESIAN_POINT ( 'NONE',  ( 206.3426153068844542, 272.1430791857031295, 8.023365743556523100 ) ) ;
#47707 = CARTESIAN_POINT ( 'NONE',  ( 137.8467198073504107, 241.2048013555409796, 4.594050593750051981 ) ) ;
#47708 = CARTESIAN_POINT ( 'NONE',  ( 150.6916211261701619, 269.6414512649903941, -15.44346024757110847 ) ) ;
#47709 = FACE_OUTER_BOUND ( 'NONE', #84340, .T. ) ;
#47710 = CARTESIAN_POINT ( 'NONE',  ( 187.6813309808503050, 281.4444333665542217, -16.91448409808978326 ) ) ;
#47711 = LINE ( 'NONE', #9232, #30411 ) ;
#47712 = CARTESIAN_POINT ( 'NONE',  ( 43.28705038798948124, 204.9869531367911293, 4.594050593750046652 ) ) ;
#47713 = EDGE_CURVE ( 'NONE', #93369, #80464, #55623, .T. ) ;
#47714 = CARTESIAN_POINT ( 'NONE',  ( 75.96427205163369933, 60.71763398054469718, -16.06735551131085060 ) ) ;
#47715 = ORIENTED_EDGE ( 'NONE', *, *, #89381, .F. ) ;
#47716 = CARTESIAN_POINT ( 'NONE',  ( 71.84021079141780319, 65.98448790626392224, 11.99618737985939987 ) ) ;
#47717 = DIRECTION ( 'NONE',  ( -0.8660254037844384856, -0.5000000000000002220, 0.000000000000000000 ) ) ;
#47718 = CARTESIAN_POINT ( 'NONE',  ( 68.49446975927493497, 70.11123478153655242, -1.325469564123312516 ) ) ;
#47719 = CARTESIAN_POINT ( 'NONE',  ( 171.9522100717342710, 260.0157765023859042, 15.50740241267492969 ) ) ;
#47720 = CARTESIAN_POINT ( 'NONE',  ( 151.3906727466529389, 278.2750905898312794, -1.659020316575751330 ) ) ;
#47721 = VECTOR ( 'NONE', #54377, 1000.000000000000114 ) ;
#47722 = EDGE_CURVE ( 'NONE', #45441, #95521, #56126, .T. ) ;
#47723 = CARTESIAN_POINT ( 'NONE',  ( 203.5555343017997529, 278.0784677578903370, -15.71723084798551362 ) ) ;
#47724 = CARTESIAN_POINT ( 'NONE',  ( 181.7766938514437243, 262.7534622773716819, 12.50707551241419324 ) ) ;
#47725 = CARTESIAN_POINT ( 'NONE',  ( 125.9386101817166974, 233.5177522451417929, 5.000000000000051514 ) ) ;
#47726 = B_SPLINE_SURFACE_WITH_KNOTS ( 'NONE', 3, 1, ( 
 ( #68172, #37764 ),
 ( #21111, #29195 ),
 ( #82928, #84909 ),
 ( #83925, #60063 ),
 ( #59565, #51989 ),
 ( #76301, #13988 ),
 ( #30682, #68666 ),
 ( #99590, #30174 ),
 ( #91026, #99099 ),
 ( #45850, #44865 ),
 ( #61061, #6389 ),
 ( #60556, #29683 ),
 ( #53464, #84414 ),
 ( #44373, #76773 ),
 ( #7366, #15451 ),
 ( #69166, #61562 ),
 ( #92509, #53953 ),
 ( #46350, #77274 ),
 ( #7885, #28681 ),
 ( #31651, #86940 ),
 ( #38762, #79326 ),
 ( #17472, #17991 ),
 ( #33175, #93512 ),
 ( #31157, #24565 ),
 ( #63070, #39735 ),
 ( #87459, #56469 ),
 ( #54444, #92999 ),
 ( #69666, #25066 ),
 ( #55448, #9377 ),
 ( #95020, #70155 ),
 ( #77794, #48382 ),
 ( #15968, #94512 ),
 ( #40752, #62549 ),
 ( #62046, #8379 ) ),
 .UNSPECIFIED., .T., .F., .F.,
 ( 4, 2, 2, 2, 2, 2, 2, 2, 2, 2, 2, 2, 2, 2, 2, 2, 4 ),
 ( 2, 2 ),
 ( 0.000000000000000000, 0.06250000000000000000, 0.1250000000000000000, 0.1875000000000000000, 0.2500000000000000000, 0.3125000000000000000, 0.3750000000000000000, 0.4375000000000000000, 0.5000000000000000000, 0.5625000000000000000, 0.6250000000000000000, 0.6875000000000000000, 0.7500000000000000000, 0.8125000000000000000, 0.8750000000000000000, 0.9375000000000000000, 1.000000000000000000 ),
 ( 0.000000000000000000, 1.000000000000000000 ),
 .UNSPECIFIED. ) ;
#47727 = CARTESIAN_POINT ( 'NONE',  ( 55.77019854693759271, 214.5530062829863311, -4.648177544792955347E-16 ) ) ;
#47728 = ORIENTED_EDGE ( 'NONE', *, *, #24516, .T. ) ;
#47729 = EDGE_CURVE ( 'NONE', #18043, #98408, #59782, .T. ) ;
#47730 = CARTESIAN_POINT ( 'NONE',  ( 203.0337691736598629, 278.9821914694464340, 16.08167820133810011 ) ) ;
#47731 = FACE_OUTER_BOUND ( 'NONE', #75, .T. ) ;
#47732 = CARTESIAN_POINT ( 'NONE',  ( 23.17945691357580529, 178.0643266524160424, -9.188101187500093303 ) ) ;
#47733 = CARTESIAN_POINT ( 'NONE',  ( 16.19390013444010279, 21.30066082961420904, -10.00000000000000533 ) ) ;
#47734 = CARTESIAN_POINT ( 'NONE',  ( 188.8691947583266426, 290.7266936548607532, -15.09369555602670587 ) ) ;
#47735 = CARTESIAN_POINT ( 'NONE',  ( -1.712471552152344811, 43.16833485791677560, 59.99999999999999289 ) ) ;
#47737 = CARTESIAN_POINT ( 'NONE',  ( 57.52260328274599033, 204.0177522451418497, -10.00000000000009592 ) ) ;
#47736 = CARTESIAN_POINT ( 'NONE',  ( 198.0902711536284357, 277.7603059513703556, -15.87033955601944690 ) ) ;
#47738 = CARTESIAN_POINT ( 'NONE',  ( 174.4148835039708274, 289.3800151988198195, 7.905235673531343821 ) ) ;
#47739 = LINE ( 'NONE', #24948, #99096 ) ;
#47740 = CARTESIAN_POINT ( 'NONE',  ( 157.8811243250769110, 257.1888664433053009, -17.39256699147873064 ) ) ;
#47741 = CARTESIAN_POINT ( 'NONE',  ( 162.2469855708762054, 251.8525454486305648, -12.98361378634216123 ) ) ;
#47742 = VERTEX_POINT ( 'NONE', #49054 ) ;
#47743 = B_SPLINE_CURVE_WITH_KNOTS ( 'NONE', 3,
 ( #66310, #82561, #13125, #26814, #34410, #80558 ),
 .UNSPECIFIED., .F., .F.,
 ( 4, 2, 4 ),
 ( 0.02004572608914358123, 0.02459847040748617750, 0.02915121472582877377 ),
 .UNSPECIFIED. ) ;
#47744 = CARTESIAN_POINT ( 'NONE',  ( 31.27120823407814854, 178.8615022471902023, 5.000000000000051514 ) ) ;
#47745 = CARTESIAN_POINT ( 'NONE',  ( 140.4712518949831974, 264.1589784336661637, -6.496448406907675876E-16 ) ) ;
#47746 = CARTESIAN_POINT ( 'NONE',  ( 202.2576150004249200, 280.3265299319959354, 16.24828394350762295 ) ) ;
#47747 = CARTESIAN_POINT ( 'NONE',  ( -11.70556275232237908, 173.2369531367911293, -4.594050593750048428 ) ) ;
#47748 = CARTESIAN_POINT ( 'NONE',  ( 27.19903172117837542, 31.10171378149920329, 9.188101187500008038 ) ) ;
#47750 = FACE_OUTER_BOUND ( 'NONE', #2706, .T. ) ;
#47749 = DIRECTION ( 'NONE',  ( 0.5000000000000014433, -0.8660254037844378194, 0.000000000000000000 ) ) ;
#47751 = CARTESIAN_POINT ( 'NONE',  ( 186.1518260931114526, 260.7827538074319023, 6.339317543960328649 ) ) ;
#47752 = CARTESIAN_POINT ( 'NONE',  ( 164.7762319088960794, 245.2461897844768828, 2.994040459560653122 ) ) ;
#47753 = CARTESIAN_POINT ( 'NONE',  ( -20.65464553008482795, 23.07220643578491348, 10.00000000000000000 ) ) ;
#47754 = CARTESIAN_POINT ( 'NONE',  ( 65.84451031894835182, 68.99484999965710585, 2.058805951153825031 ) ) ;
#47755 = VERTEX_POINT ( 'NONE', #41433 ) ;
#47756 = CARTESIAN_POINT ( 'NONE',  ( 150.5287101026835330, 271.9236214347867531, -12.89083132144543775 ) ) ;
#47757 = CARTESIAN_POINT ( 'NONE',  ( 178.6565837683001519, 285.5687190954733410, 13.02810775182850911 ) ) ;
#47758 = CARTESIAN_POINT ( 'NONE',  ( 168.7068454911210438, 288.1994200320167465, 0.5267417468238662082 ) ) ;
#47759 = CARTESIAN_POINT ( 'NONE',  ( 16.72130706672766109, 10.44966523072493025, -2.296566073217252530E-15 ) ) ;
#47760 = CARTESIAN_POINT ( 'NONE',  ( 160.5489464122825325, 252.5680630427104063, 14.85483651643795788 ) ) ;
#47761 = VECTOR ( 'NONE', #24306, 1000.000000000000114 ) ;
#47762 = CARTESIAN_POINT ( 'NONE',  ( 159.2394649670193303, 254.8361514374751664, -16.43133403737800791 ) ) ;
#47763 = ADVANCED_FACE ( 'NONE', ( #64759 ), #80495, .F. ) ;
#47764 = CARTESIAN_POINT ( 'NONE',  ( 192.0331311261993790, 298.0358554833232461, 11.82583305898340953 ) ) ;
#47765 = DIRECTION ( 'NONE',  ( 0.8599083858334037878, -0.5104483989331242144, 0.000000000000000000 ) ) ;
#47766 = CARTESIAN_POINT ( 'NONE',  ( -105.0000000000000000, 4.999999999999999112, 14.21260523776214235 ) ) ;
#47767 = CARTESIAN_POINT ( 'NONE',  ( 87.66117359288392663, 45.35348716220470067, 6.484875789303244709 ) ) ;
#47768 = CARTESIAN_POINT ( 'NONE',  ( 15.77038241084232517, 34.14663330942826747, -10.00000000000000000 ) ) ;
#47769 = ORIENTED_EDGE ( 'NONE', *, *, #26141, .F. ) ;
#47770 = ORIENTED_EDGE ( 'NONE', *, *, #33012, .F. ) ;
#47771 = B_SPLINE_CURVE_WITH_KNOTS ( 'NONE', 3,
 ( #89414, #50842, #81792, #56944, #87930, #89890, #12369, #74175, #35649, #66549, #97479, #28044, #80300, #51339, #82306, #43735, #15313, #30541, #45719, #5254, #83275, #92379, #74678, #98961 ),
 .UNSPECIFIED., .F., .F.,
 ( 4, 2, 2, 2, 2, 2, 2, 2, 2, 2, 2, 4 ),
 ( 0.000000000000000000, 0.1249999999999878153, 0.2499999999999756306, 0.3749999999999634737, 0.4374999999999670819, 0.4999999999999706901, 0.5624999999999743538, 0.6249999999999780176, 0.6874999999999816813, 0.7499999999999853451, 0.8749999999999926725, 1.000000000000000000 ),
 .UNSPECIFIED. ) ;
#47772 = CARTESIAN_POINT ( 'NONE',  ( 48.61286661847091040, 84.94359857078811160, 10.00000000000000000 ) ) ;
#47773 = CARTESIAN_POINT ( 'NONE',  ( 86.45558908622700756, 47.52558151742778847, 10.49075240043499591 ) ) ;
#47774 = EDGE_LOOP ( 'NONE', ( #5907, #73676, #3706, #7669 ) ) ;
#47776 = ADVANCED_FACE ( 'NONE', ( #51028 ), #11565, .T. ) ;
#47775 = CARTESIAN_POINT ( 'NONE',  ( 6.522775935009023307, 186.1199935810940644, 2.679491924311251605 ) ) ;
#47777 = DIRECTION ( 'NONE',  ( 0.000000000000000000, 0.000000000000000000, 1.000000000000000000 ) ) ;
#47778 = EDGE_LOOP ( 'NONE', ( #73882, #85603, #7289, #68193 ) ) ;
#47780 = ADVANCED_FACE ( 'NONE', ( #51539 ), #50048, .F. ) ;
#47779 = DIRECTION ( 'NONE',  ( -1.000000000000000000, 0.000000000000000000, 0.000000000000000000 ) ) ;
#47781 = CARTESIAN_POINT ( 'NONE',  ( 78.98660877947106940, 59.42842565914681785, -16.52762269555201868 ) ) ;
#47782 = CARTESIAN_POINT ( 'NONE',  ( 83.56140931445644071, 47.55900624907771856, -12.50891871133917199 ) ) ;
#47783 = CARTESIAN_POINT ( 'NONE',  ( 3.722289961109204626, 27.08330320443190331, 10.00000000000000000 ) ) ;
#47784 = ORIENTED_EDGE ( 'NONE', *, *, #34499, .F. ) ;
#47785 = CARTESIAN_POINT ( 'NONE',  ( 200.1444820856229967, 283.9865835035790269, 17.93386694781497326 ) ) ;
#47786 = CARTESIAN_POINT ( 'NONE',  ( 93.96857342517718337, -8.000000000000000000, 14.21260523776213347 ) ) ;
#47787 = CARTESIAN_POINT ( 'NONE',  ( 161.0515428782683500, 277.3244187559503189, -13.42420650014866368 ) ) ;
#47788 = CARTESIAN_POINT ( 'NONE',  ( -115.0954152546898257, 78.37593066204033221, -30.52142883766498116 ) ) ;
#47789 = ORIENTED_EDGE ( 'NONE', *, *, #33747, .T. ) ;
#47790 = CARTESIAN_POINT ( 'NONE',  ( 170.8211178702818529, 255.2134001104743390, -11.38359876985272301 ) ) ;
#47791 = ORIENTED_EDGE ( 'NONE', *, *, #42677, .T. ) ;
#47792 = ORIENTED_EDGE ( 'NONE', *, *, #73326, .T. ) ;
#47793 = CARTESIAN_POINT ( 'NONE',  ( 80.20973102464937199, 46.09908331049562236, 12.23914068923185461 ) ) ;
#47794 = VECTOR ( 'NONE', #8117, 1000.000000000000000 ) ;
#47795 = ORIENTED_EDGE ( 'NONE', *, *, #23524, .F. ) ;
#47796 = CARTESIAN_POINT ( 'NONE',  ( 186.0400780920065529, 271.7087950812899066, 16.90619359840448510 ) ) ;
#47797 = ORIENTED_EDGE ( 'NONE', *, *, #355, .T. ) ;
#47798 =( BOUNDED_CURVE ( )  B_SPLINE_CURVE ( 2, ( #41161, #80735, #72098, #18392, #49287, #86338, #80223, #3213, #34097 ),
 .UNSPECIFIED., .F., .T. ) 
 B_SPLINE_CURVE_WITH_KNOTS ( ( 3, 2, 2, 2, 3 ),
 ( 0.5282258064516128782, 0.5295698924731182533, 0.5322580645161290036, 0.5349462365591397539, 0.5362903225806451291 ),
 .UNSPECIFIED. ) 
 CURVE ( )  GEOMETRIC_REPRESENTATION_ITEM ( )  RATIONAL_B_SPLINE_CURVE ( ( 0.9330127018922194093, 0.9330127018922194093, 1.000000000000000000, 0.8660254037844387076, 1.000000000000000000, 0.8660254037844387076, 1.000000000000000000, 0.9330127018922194093, 0.9330127018922194093 ) ) 
 REPRESENTATION_ITEM ( '' )  );
#47799 = DIRECTION ( 'NONE',  ( -0.8660254037844387076, -0.4999999999999998890, -0.000000000000000000 ) ) ;
#47800 = CARTESIAN_POINT ( 'NONE',  ( 162.9148809972199672, 269.1323162226891554, 17.43693885807998001 ) ) ;
#47801 = CARTESIAN_POINT ( 'NONE',  ( 147.8308140999695866, 274.5965143850199865, -7.866624397492971710 ) ) ;
#47802 = CARTESIAN_POINT ( 'NONE',  ( 82.44970526080962259, 53.47733151612504088, -15.75145310647262065 ) ) ;
#47803 = DIRECTION ( 'NONE',  ( 0.4999999999999998890, -0.8660254037844385966, 0.000000000000000000 ) ) ;
#47804 = CARTESIAN_POINT ( 'NONE',  ( -64.74139798177010618, 41.16849083240310847, -10.00000000000000000 ) ) ;
#47805 = B_SPLINE_CURVE_WITH_KNOTS ( 'NONE', 3,
 ( #23172, #60661, #29789, #68281 ),
 .UNSPECIFIED., .F., .F.,
 ( 4, 4 ),
 ( 0.002207507469835296148, 0.004300347803759868928 ),
 .UNSPECIFIED. ) ;
#47806 = CARTESIAN_POINT ( 'NONE',  ( 23.96105869301208813, 16.76004757982090254, 5.678558825948272215 ) ) ;
#47807 = CARTESIAN_POINT ( 'NONE',  ( 205.7829192689729325, 274.2205238267313234, 11.21202327925415254 ) ) ;
#47808 = CARTESIAN_POINT ( 'NONE',  ( 206.0691053506789387, 273.7248349927971844, 11.70564474658248422 ) ) ;
#47810 = ORIENTED_EDGE ( 'NONE', *, *, #87678, .F. ) ;
#47809 = CARTESIAN_POINT ( 'NONE',  ( 197.9552487813401456, 287.7784468162186613, 17.26493623863614602 ) ) ;
#47811 = DIRECTION ( 'NONE',  ( 1.000000000000000000, 1.804112415015878984E-15, 0.000000000000000000 ) ) ;
#47812 = CARTESIAN_POINT ( 'NONE',  ( 64.35513503747660025, 196.4155109091896350, 2.679491924311254714 ) ) ;
#47813 = CARTESIAN_POINT ( 'NONE',  ( 159.9647205790309101, 253.5799718689968927, -16.48298384325780219 ) ) ;
#47814 = CARTESIAN_POINT ( 'NONE',  ( 159.3773945546513460, 271.5416235043197162, -16.14591210334819849 ) ) ;
#47815 = CARTESIAN_POINT ( 'NONE',  ( 161.6673510627899191, 250.6309293646106653, 13.01175935005004192 ) ) ;
#47816 = CARTESIAN_POINT ( 'NONE',  ( 190.7952227603998665, 261.9688979877246311, -0.5812294033076593758 ) ) ;
#47817 = ORIENTED_EDGE ( 'NONE', *, *, #97395, .T. ) ;
#47818 = CARTESIAN_POINT ( 'NONE',  ( 185.8626946602280441, 259.3471889805154547, 7.308832903665572367 ) ) ;
#47819 = CARTESIAN_POINT ( 'NONE',  ( 131.5677753063155251, 246.7677522451418497, 10.00000000000009592 ) ) ;
#47820 = CARTESIAN_POINT ( 'NONE',  ( 194.9499559406243918, 279.5747724307917679, 17.51673600049429780 ) ) ;
#47821 = CARTESIAN_POINT ( 'NONE',  ( 8.953011887168695893, 182.6427522451419350, 10.00000000000009237 ) ) ;
#47822 = CARTESIAN_POINT ( 'NONE',  ( 91.08134800299070832, 214.2048013555409796, 4.594050593750051981 ) ) ;
#47823 = CARTESIAN_POINT ( 'NONE',  ( 82.21221196657927521, 40.84058624180994457, -1.181054413250449464 ) ) ;
#47824 = CARTESIAN_POINT ( 'NONE',  ( 7.026152882275393807, 27.55466486950697913, -1.111400068045478839E-16 ) ) ;
#47825 = CARTESIAN_POINT ( 'NONE',  ( 169.7087038524299771, 280.0432160542959537, -13.57890784763611336 ) ) ;
#47827 = CARTESIAN_POINT ( 'NONE',  ( 75.87952572578419108, 65.59853847594877152, 13.85574643265811723 ) ) ;
#47826 = CARTESIAN_POINT ( 'NONE',  ( 3.531332017333847606, 172.8458772461660828, 9.188101187500095079 ) ) ;
#47829 = EDGE_CURVE ( 'NONE', #4560, #5926, #70511, .T. ) ;
#47828 = AXIS2_PLACEMENT_3D ( 'NONE', #46042, #7558, #76976 ) ;
#47830 = CARTESIAN_POINT ( 'NONE',  ( 200.4775477985258760, 283.4096967665721536, 16.80647240730505487 ) ) ;
#47831 = ORIENTED_EDGE ( 'NONE', *, *, #100099, .F. ) ;
#47832 = VERTEX_POINT ( 'NONE', #50530 ) ;
#47833 = CARTESIAN_POINT ( 'NONE',  ( 200.6160348301466456, 267.6256034195902203, -2.850748744823686565 ) ) ;
#47834 = EDGE_CURVE ( 'NONE', #98025, #87101, #35338, .T. ) ;
#47835 = CYLINDRICAL_SURFACE ( 'NONE', #34047, 16.60714546451156792 ) ;
#47836 = CARTESIAN_POINT ( 'NONE',  ( 82.19874836290229325, 41.39239848049727755, 4.139731784179837781 ) ) ;
#47837 = LINE ( 'NONE', #47351, #73787 ) ;
#47838 = CARTESIAN_POINT ( 'NONE',  ( 185.5962948356213360, 286.5636094107885015, 15.98812411951390544 ) ) ;
#47839 = CARTESIAN_POINT ( 'NONE',  ( 164.7647380297938184, 248.9862001899016946, 10.10785415616959071 ) ) ;
#47840 = CARTESIAN_POINT ( 'NONE',  ( 39.87759600423577666, 184.6423013555410080, -4.594050593750043987 ) ) ;
#47841 = CARTESIAN_POINT ( 'NONE',  ( 78.30721297357251842, 216.0177522451418497, -10.00000000000009592 ) ) ;
#47842 = CARTESIAN_POINT ( 'NONE',  ( 195.8878223364301050, 275.2230923960996165, 15.66255634890894832 ) ) ;
#47843 = ORIENTED_EDGE ( 'NONE', *, *, #25564, .T. ) ;
#47844 = EDGE_CURVE ( 'NONE', #56530, #59778, #46296, .T. ) ;
#47845 = FACE_OUTER_BOUND ( 'NONE', #42210, .T. ) ;
#47846 = CARTESIAN_POINT ( 'NONE',  ( 175.1702272577395263, 281.4177487094669345, -14.21329840767373121 ) ) ;
#47847 = CARTESIAN_POINT ( 'NONE',  ( -14.60124842228533915, 168.5024278399160949, 9.188101187500095079 ) ) ;
#47848 = CARTESIAN_POINT ( 'NONE',  ( 157.0935036675524827, 258.5530654392286465, 17.32636058289560665 ) ) ;
#47849 = CARTESIAN_POINT ( 'NONE',  ( 68.59598715216472442, 64.19765338651440345, -12.48679878568064971 ) ) ;
#47850 = CARTESIAN_POINT ( 'NONE',  ( 198.8157103782086210, 286.2880836124806478, -18.60729372713428020 ) ) ;
#47851 = CIRCLE ( 'NONE', #28486, 0.1418229129681557177 ) ;
#47852 = CIRCLE ( 'NONE', #21986, 70.00000000000001421 ) ;
#47853 = DIRECTION ( 'NONE',  ( 1.000000000000000000, 0.000000000000000000, -0.000000000000000000 ) ) ;
#47854 = CARTESIAN_POINT ( 'NONE',  ( 194.8708600166808651, 293.1207648669033006, -14.79199694356877970 ) ) ;
#47855 = CARTESIAN_POINT ( 'NONE',  ( 192.5555981258711995, 265.1457337795512785, 7.710077344952797063 ) ) ;
#47856 = CARTESIAN_POINT ( 'NONE',  ( 204.5730103890532519, 276.3161474792809145, 14.88139715235883109 ) ) ;
#47857 = CARTESIAN_POINT ( 'NONE',  ( 70.17018262072913615, 217.9865022471902876, 10.00000000000009415 ) ) ;
#47858 = CARTESIAN_POINT ( 'NONE',  ( 148.3930300673291640, 273.6227277647267897, 8.375036249079425232 ) ) ;
#47859 = EDGE_CURVE ( 'NONE', #38166, #53063, #8818, .T. ) ;
#47860 = EDGE_LOOP ( 'NONE', ( #10968, #53445, #96163, #79611 ) ) ;
#47861 = AXIS2_PLACEMENT_3D ( 'NONE', #8367, #92496, #91014 ) ;
#47862 = CARTESIAN_POINT ( 'NONE',  ( 152.9502192050138660, 266.8376656511403553, -16.03576590126549561 ) ) ;
#47863 = FACE_OUTER_BOUND ( 'NONE', #91826, .T. ) ;
#47864 = CARTESIAN_POINT ( 'NONE',  ( 117.3868696429430258, 229.3923013555409796, 4.594050593750050204 ) ) ;
#47865 = CARTESIAN_POINT ( 'NONE',  ( 15.97197434310064601, 12.14754757982088940, -5.678558825948276656 ) ) ;
#47867 = CARTESIAN_POINT ( 'NONE',  ( 70.81316579126399802, 61.41551742065354347, -14.85192641751565468 ) ) ;
#47866 = PRODUCT_DEFINITION_FORMATION_WITH_SPECIFIED_SOURCE ( 'ANY', '', #29009, .NOT_KNOWN. ) ;
#47868 = CARTESIAN_POINT ( 'NONE',  ( 0.4893710859096792598, 78.77562236714182120, 59.97499999999998721 ) ) ;
#47870 = CARTESIAN_POINT ( 'NONE',  ( -19.69202633138669967, 92.92865703790650400, 59.99999999999999289 ) ) ;
#47869 = DIRECTION ( 'NONE',  ( 0.5000000000000001110, -0.8660254037844385966, 0.000000000000000000 ) ) ;
#47871 = CARTESIAN_POINT ( 'NONE',  ( 190.8775532225699862, 300.0373751245133462, -6.456187174708069243 ) ) ;
#47872 = CARTESIAN_POINT ( 'NONE',  ( 21.45610022030931674, 34.16126292948896293, -6.180339887498951690 ) ) ;
#47873 = CARTESIAN_POINT ( 'NONE',  ( 149.6890529486499872, 271.3779502865075983, -12.51465682618088593 ) ) ;
#47874 = CARTESIAN_POINT ( 'NONE',  ( 91.79731502344390037, 212.2592609112380444, 2.679491924311254714 ) ) ;
#47875 = CARTESIAN_POINT ( 'NONE',  ( 173.1586067699058162, 289.7215660399545527, -1.264861486351297248 ) ) ;
#47876 = DIRECTION ( 'NONE',  ( 0.000000000000000000, 0.000000000000000000, 1.000000000000000000 ) ) ;
#47877 = ORIENTED_EDGE ( 'NONE', *, *, #55877, .T. ) ;
#47878 = CARTESIAN_POINT ( 'NONE',  ( 15.54467260552930341, 34.00295985972733348, 10.00000000000000000 ) ) ;
#47879 = CARTESIAN_POINT ( 'NONE',  ( 175.1138237960793447, 279.3531053840294476, 15.84073920059228158 ) ) ;
#47880 = CARTESIAN_POINT ( 'NONE',  ( 199.6627426296996930, 270.0018726912092006, 9.250069944390398646 ) ) ;
#47881 = EDGE_CURVE ( 'NONE', #8972, #56753, #5245, .T. ) ;
#47882 = VERTEX_POINT ( 'NONE', #93050 ) ;
#47883 = CARTESIAN_POINT ( 'NONE',  ( 85.57885443703831641, 45.56984769523893419, 9.424717718146821355 ) ) ;
#47884 = CARTESIAN_POINT ( 'NONE',  ( 185.1790142135946837, 260.5378326486920741, -9.806357480331048038 ) ) ;
#47885 = CARTESIAN_POINT ( 'NONE',  ( 191.7967966825411850, 283.9693557995756805, 17.70397221340040161 ) ) ;
#47886 = CARTESIAN_POINT ( 'NONE',  ( 192.7944000592152634, 296.7172990131160759, 11.44860011299869740 ) ) ;
#47887 = EDGE_CURVE ( 'NONE', #12886, #7039, #30014, .T. ) ;
#47888 = VERTEX_POINT ( 'NONE', #44917 ) ;
#47889 = CARTESIAN_POINT ( 'NONE',  ( 190.7357586861858749, 280.8065426626702106, 16.64018919219373061 ) ) ;
#47890 = CARTESIAN_POINT ( 'NONE',  ( 36.96107555259132482, 29.84335787977765619, 9.188101187500006262 ) ) ;
#47891 = LINE ( 'NONE', #7037, #11004 ) ;
#47892 = VERTEX_POINT ( 'NONE', #30231 ) ;
#47893 = CARTESIAN_POINT ( 'NONE',  ( 167.5344527987841730, 280.9027864911226402, 11.65609303130555574 ) ) ;
#47894 = CYLINDRICAL_SURFACE ( 'NONE', #14361, 17.82106496071139645 ) ;
#47895 = CARTESIAN_POINT ( 'NONE',  ( 164.4854433269806577, 246.2060377238486808, -1.879056492287135116 ) ) ;
#47896 = VERTEX_POINT ( 'NONE', #83473 ) ;
#47898 = ADVANCED_FACE ( 'NONE', ( #45903 ), #60112, .T. ) ;
#47897 = DIRECTION ( 'NONE',  ( 0.6123724356958143433, 0.3535533905932691234, -0.7071067811865326957 ) ) ;
#47899 = CARTESIAN_POINT ( 'NONE',  ( 162.8756881843043516, 250.5380280774768949, 12.81046238701583029 ) ) ;
#47900 = CARTESIAN_POINT ( 'NONE',  ( 192.4380962356868281, 295.3344353383980661, 13.50754959408193656 ) ) ;
#47901 = CARTESIAN_POINT ( 'NONE',  ( 86.16957357854950317, 44.43129735356627208, -7.220647133741227464 ) ) ;
#47902 = CYLINDRICAL_SURFACE ( 'NONE', #33501, 14.21260523776213347 ) ;
#47903 = AXIS2_PLACEMENT_3D ( 'NONE', #20532, #81857, #50907 ) ;
#47904 = CARTESIAN_POINT ( 'NONE',  ( 85.97422890462554790, 44.88503902940634305, -8.159254893437074330 ) ) ;
#47905 = VECTOR ( 'NONE', #5965, 1000.000000000000000 ) ;
#47906 = CARTESIAN_POINT ( 'NONE',  ( 203.4696564630250464, 278.2272125378923988, -16.38980782817167636 ) ) ;
#47907 = EDGE_CURVE ( 'NONE', #98060, #75682, #86206, .T. ) ;
#47908 = ORIENTED_EDGE ( 'NONE', *, *, #12722, .T. ) ;
#47909 = ORIENTED_EDGE ( 'NONE', *, *, #26316, .F. ) ;
#47911 = VECTOR ( 'NONE', #20054, 1000.000000000000114 ) ;
#47910 = CARTESIAN_POINT ( 'NONE',  ( 177.9882410936357928, 260.8588164829307630, 12.21663056129005120 ) ) ;
#47912 = ORIENTED_EDGE ( 'NONE', *, *, #82703, .F. ) ;
#47913 = CARTESIAN_POINT ( 'NONE',  ( 81.17432035541970947, 55.57579169957366361, 16.36820043613993292 ) ) ;
#47914 = B_SPLINE_CURVE_WITH_KNOTS ( 'NONE', 3,
 ( #8075, #465, #46541, #62745 ),
 .UNSPECIFIED., .F., .F.,
 ( 4, 4 ),
 ( 0.008817850388587639837, 0.01395074355647914210 ),
 .UNSPECIFIED. ) ;
#47915 = ORIENTED_EDGE ( 'NONE', *, *, #36778, .F. ) ;
#47916 = DIRECTION ( 'NONE',  ( -0.5000000000000011102, -0.8660254037844380415, -0.000000000000000000 ) ) ;
#47917 = CARTESIAN_POINT ( 'NONE',  ( -19.65312891409015350, 9.999999999999801048, -54.99999999999999289 ) ) ;
#47918 = ORIENTED_EDGE ( 'NONE', *, *, #95424, .T. ) ;
#47919 = CARTESIAN_POINT ( 'NONE',  ( 182.7138520656610012, 280.2226620527670775, -16.11794820187313704 ) ) ;
#47920 = CARTESIAN_POINT ( 'NONE',  ( 165.0477436618537865, 244.7759176335020186, -2.027991469056170448 ) ) ;
#47921 = CARTESIAN_POINT ( 'NONE',  ( 190.0146931831988013, 301.5318925525250506, 2.191471318341308372 ) ) ;
#47922 = CARTESIAN_POINT ( 'NONE',  ( 179.4722142099873565, 269.7276464518548096, -17.35046799866735157 ) ) ;
#47923 = CARTESIAN_POINT ( 'NONE',  ( 82.54798078747610646, 40.46213573055935342, 0.9004448831076741211 ) ) ;
#47924 = CARTESIAN_POINT ( 'NONE',  ( 170.9484186264854770, 250.8673865788455544, -5.551388615809983662 ) ) ;
#47925 = CARTESIAN_POINT ( 'NONE',  ( 196.8708119716154954, 268.3476497963631573, -11.07389558091716708 ) ) ;
#47926 = CARTESIAN_POINT ( 'NONE',  ( 153.8479027513132280, 279.7076740674982034, 2.196726205667342668 ) ) ;
#47927 = CARTESIAN_POINT ( 'NONE',  ( 127.4808708382166316, 256.6589784336661637, -6.496448406907675876E-16 ) ) ;
#47928 = VERTEX_POINT ( 'NONE', #53023 ) ;
#47929 = CARTESIAN_POINT ( 'NONE',  ( 186.6466788774901602, 262.7990401948939621, -9.116086771617830209 ) ) ;
#47930 = VERTEX_POINT ( 'NONE', #45418 ) ;
#47932 = ORIENTED_EDGE ( 'NONE', *, *, #96726, .F. ) ;
#47931 = CARTESIAN_POINT ( 'NONE',  ( 85.68734770396230260, 48.85621462398719217, -12.54449143327925498 ) ) ;
#47933 = VECTOR ( 'NONE', #48997, 1000.000000000000227 ) ;
#47934 = CARTESIAN_POINT ( 'NONE',  ( 201.8235137129046279, 275.1765603161098284, 13.33099703020108073 ) ) ;
#47935 = CARTESIAN_POINT ( 'NONE',  ( 180.9179439205437916, 256.0455442330405731, 0.7724379216420866889 ) ) ;
#47936 = CARTESIAN_POINT ( 'NONE',  ( 32.41152252715882298, 42.21091486745863364, 7.012934429366973338E-14 ) ) ;
#47937 = CARTESIAN_POINT ( 'NONE',  ( 192.0467657490588351, 298.0122396237888438, 11.75052100010666045 ) ) ;
#47938 = CARTESIAN_POINT ( 'NONE',  ( 71.52353591355296203, 59.88240882867724224, 15.08427714274043829 ) ) ;
#47939 = CARTESIAN_POINT ( 'NONE',  ( -19.65312891409030271, 93.06504152958497400, -10.00000000000000888 ) ) ;
#47940 = CARTESIAN_POINT ( 'NONE',  ( 173.4000888393750017, 287.4655024987716843, -9.837467039034411442 ) ) ;
#47941 = VECTOR ( 'NONE', #49560, 1000.000000000000114 ) ;
#47942 = CARTESIAN_POINT ( 'NONE',  ( 174.9461632972169696, 282.2965899055037085, 14.42753729772996252 ) ) ;
#47943 = CARTESIAN_POINT ( 'NONE',  ( 177.2261086063719517, 256.1163090582663244, -7.433373391858083323 ) ) ;
#47944 = VERTEX_POINT ( 'NONE', #38814 ) ;
#47945 = CARTESIAN_POINT ( 'NONE',  ( 147.6884207308302450, 274.8431469350302336, -8.096293592099874203 ) ) ;
#47946 = CARTESIAN_POINT ( 'NONE',  ( 66.00531965145684410, 68.68482112325794731, -0.3732326179758673756 ) ) ;
#47947 = ORIENTED_EDGE ( 'NONE', *, *, #1027, .T. ) ;
#47948 = DIRECTION ( 'NONE',  ( 0.000000000000000000, -0.000000000000000000, 1.000000000000000000 ) ) ;
#47949 = CARTESIAN_POINT ( 'NONE',  ( 157.1454194340104209, 276.7041856997979039, 10.24769222078917608 ) ) ;
#47950 = CARTESIAN_POINT ( 'NONE',  ( 192.1068185053286754, 297.9082251987945824, -9.660304852024209410 ) ) ;
#47951 = CARTESIAN_POINT ( 'NONE',  ( 58.72569090598248920, 179.3089433639326842, 17.97570218321541446 ) ) ;
#47952 = CARTESIAN_POINT ( 'NONE',  ( 162.8996025780091941, 248.4966071325470125, 11.23567065566008516 ) ) ;
#47954 = CARTESIAN_POINT ( 'NONE',  ( 151.5066875197445597, 274.9073607968387023, -8.887479126886400849 ) ) ;
#47953 = CARTESIAN_POINT ( 'NONE',  ( 153.1401327494902773, 270.1234001006548624, 14.03976522339925381 ) ) ;
#47955 = CARTESIAN_POINT ( 'NONE',  ( 200.7694952279801157, 282.9040289856181403, -17.94628235092568502 ) ) ;
#47956 = B_SPLINE_CURVE_WITH_KNOTS ( 'NONE', 3,
 ( #28282, #81533, #80545, #59158, #27799, #74910, #5494, #12105, #42964, #34883 ),
 .UNSPECIFIED., .F., .F.,
 ( 4, 2, 2, 2, 4 ),
 ( 0.000000000000000000, 0.0002622400424272329066, 0.0005244800848544658133, 0.0007867201272816987199, 0.001048960169708931627 ),
 .UNSPECIFIED. ) ;
#47957 = EDGE_LOOP ( 'NONE', ( #8932, #1487, #13971, #18952 ) ) ;
#47958 = CARTESIAN_POINT ( 'NONE',  ( 147.1199024702499969, 275.8278494473859723, 5.224467159276165340 ) ) ;
#47959 = CARTESIAN_POINT ( 'NONE',  ( 186.8442235758623156, 262.5257503668073582, -8.765433223893147385 ) ) ;
#47960 = CARTESIAN_POINT ( 'NONE',  ( 193.5216815486326425, 276.1393389031752577, -16.40952103877357970 ) ) ;
#47961 = DIRECTION ( 'NONE',  ( 0.5000000000000048850, -0.8660254037844358210, 0.000000000000000000 ) ) ;
#47962 = CARTESIAN_POINT ( 'NONE',  ( 184.5612557885503975, 296.9796338933509219, -4.430542032517011286 ) ) ;
#47963 = CARTESIAN_POINT ( 'NONE',  ( 192.0645969571214096, 297.9813550654635605, 11.46542907566974812 ) ) ;
#47964 = CARTESIAN_POINT ( 'NONE',  ( 16.98334746987259791, 25.50829794293879615, -10.00000000000000355 ) ) ;
#47965 = CARTESIAN_POINT ( 'NONE',  ( 74.06759120418938380, 68.62503282117260994, 10.93070749243084450 ) ) ;
#47966 = CARTESIAN_POINT ( 'NONE',  ( 68.39103212955656375, 70.07216116922043625, 1.057113424849359662 ) ) ;
#47967 = CARTESIAN_POINT ( 'NONE',  ( -6.807019788225388446, 173.0024278399160949, 9.188101187500095079 ) ) ;
#47968 = CARTESIAN_POINT ( 'NONE',  ( 92.65049840370248546, 233.4869531367911293, 4.594050593750046652 ) ) ;
#47969 = CARTESIAN_POINT ( 'NONE',  ( 34.80747863286459420, 184.2365022471901739, 10.00000000000009948 ) ) ;
#47970 = CARTESIAN_POINT ( 'NONE',  ( 180.2468139727683649, 280.2236653090821505, -17.21193327238699666 ) ) ;
#47971 = LINE ( 'NONE', #32282, #47933 ) ;
#47972 = ADVANCED_FACE ( 'NONE', ( #61111 ), #92086, .T. ) ;
#47973 = CARTESIAN_POINT ( 'NONE',  ( 202.8151641853381477, 279.3608264160075692, -16.28741359973609448 ) ) ;
#47974 = CIRCLE ( 'NONE', #51224, 9.999999999999998224 ) ;
#47975 = CARTESIAN_POINT ( 'NONE',  ( 77.82957106945204373, 53.72413217592595203, 15.93988384268166669 ) ) ;
#47976 = LINE ( 'NONE', #31284, #65927 ) ;
#47977 = VECTOR ( 'NONE', #28751, 1000.000000000000227 ) ;
#47978 = CARTESIAN_POINT ( 'NONE',  ( 77.58957552442460326, 61.75793702469097468, 15.67560070342385892 ) ) ;
#47980 = CARTESIAN_POINT ( 'NONE',  ( 162.7070706717508699, 248.8300821762643693, -9.986337079333621247 ) ) ;
#47979 = CARTESIAN_POINT ( 'NONE',  ( 190.4469008128301653, 300.3948906649509922, -0.6521089053012534276 ) ) ;
#47981 = CARTESIAN_POINT ( 'NONE',  ( 207.6250539976609275, 271.0298528822568187, 4.860623598087060238 ) ) ;
#47982 = EDGE_CURVE ( 'NONE', #89109, #88625, #6442, .T. ) ;
#47983 = CARTESIAN_POINT ( 'NONE',  ( -9.181706736895311138, 177.0530062829863027, -4.648177544792955347E-16 ) ) ;
#47984 = DIRECTION ( 'NONE',  ( 0.4999999999999998890, -0.8660254037844385966, 0.000000000000000000 ) ) ;
#47985 = CARTESIAN_POINT ( 'NONE',  ( 157.0957870390718369, 258.5491105237443321, 17.69218919045495397 ) ) ;
#47986 = TOROIDAL_SURFACE ( 'NONE', #10774, 15.10714546451156970, 0.5000000000000000000 ) ;
#47987 = CARTESIAN_POINT ( 'NONE',  ( -7.357133217438179607, 159.8927522451417929, -10.00000000000009237 ) ) ;
#47988 = EDGE_CURVE ( 'NONE', #49571, #81157, #38093, .T. ) ;
#47989 = B_SPLINE_CURVE_WITH_KNOTS ( 'NONE', 3,
 ( #92726, #76983, #22292, #38976, #21795, #37969, #76026, #7085, #495, #6603, #53192, #23276, #14693, #45576, #46070, #76504, #92246, #22796, #16192, #84629, #69881, #85130, #85649, #6096, #36991, #10331, #34611, #27026, #25522, #58400, #79767, #33630, #57910, #19929, #95967, #17936, #81259, #88889, #42692, #73623 ),
 .UNSPECIFIED., .F., .F.,
 ( 4, 2, 2, 2, 2, 2, 2, 2, 2, 2, 2, 2, 2, 2, 2, 2, 2, 2, 2, 4 ),
 ( 0.003159330915503282683, 0.003354433587230957418, 0.003549536258958632586, 0.003647087594822461497, 0.003744638930686289974, 0.003939741602413947795, 0.004329946945869263437, 0.004720152289324578213, 0.005500562976235209497, 0.006280973663145839915, 0.007061384350056471200, 0.007841795036967101618, 0.007939346372830951779, 0.008036897708694801939, 0.008085673376626687989, 0.008134449044558574038, 0.008232000380422342667, 0.008622205723877195138, 0.009012411067332047609, 0.009402616410786900081 ),
 .UNSPECIFIED. ) ;
#47990 = CARTESIAN_POINT ( 'NONE',  ( 207.8575108622103755, 270.6272257822888037, -6.381720258959569847 ) ) ;
#47991 = CARTESIAN_POINT ( 'NONE',  ( 36.87296296726972855, 204.3464784336661637, 1.353441290958777327E-15 ) ) ;
#47992 = B_SPLINE_CURVE_WITH_KNOTS ( 'NONE', 3,
 ( #26201, #47979, #71816, #33816, #10497, #86555, #55571, #78924, #79938, #49488, #72828, #32291 ),
 .UNSPECIFIED., .F., .F.,
 ( 4, 2, 2, 2, 2, 4 ),
 ( 0.001378329982659087533, 0.001584756524673330271, 0.001791183066687573010, 0.002204036150716021623, 0.002616889234744470237, 0.003029742318772918417 ),
 .UNSPECIFIED. ) ;
#47993 = CARTESIAN_POINT ( 'NONE',  ( 62.85372508080289577, 219.3464784336661637, 1.353441290958777327E-15 ) ) ;
#47994 = CARTESIAN_POINT ( 'NONE',  ( 164.4708158012598460, 246.8356330233726794, -5.687495631043780087 ) ) ;
#47995 = DIRECTION ( 'NONE',  ( -0.7905172007421654712, 0.000000000000000000, 0.6124398381316900064 ) ) ;
#47996 = CARTESIAN_POINT ( 'NONE',  ( 166.9993039719644230, 259.7585743740527278, 15.88680828586103821 ) ) ;
#47998 = CARTESIAN_POINT ( 'NONE',  ( 79.19548930461120051, 59.90515312544787463, -16.13566294680263624 ) ) ;
#47997 = CARTESIAN_POINT ( 'NONE',  ( 44.18794977381974576, 118.5901545549086791, -10.00000000000000000 ) ) ;
#47999 = B_SPLINE_CURVE_WITH_KNOTS ( 'NONE', 3,
 ( #5465, #35857, #53044, #43942, #52058, #59127, #14563, #66751, #14059, #68742, #20668, #44443, #21178, #5959, #36850, #90611 ),
 .UNSPECIFIED., .F., .F.,
 ( 4, 2, 2, 2, 2, 2, 2, 4 ),
 ( 8.673617379884035472E-19, 0.0003786681000627550929, 0.0007573362001255093184, 0.001136004300188263490, 0.001514672400251017769, 0.001893340500313771832, 0.002272008600376526112, 0.003029344800502178654 ),
 .UNSPECIFIED. ) ;
#48000 = CARTESIAN_POINT ( 'NONE',  ( 25.90481151690805106, 33.14336893147756768, 7.433330006724141015 ) ) ;
#48001 = AXIS2_PLACEMENT_3D ( 'NONE', #97602, #49982, #11506 ) ;
#48002 = CARTESIAN_POINT ( 'NONE',  ( 198.4782858197754649, 286.8725200914082620, -17.44895083299520522 ) ) ;
#48003 = CARTESIAN_POINT ( 'NONE',  ( 196.3507576896697344, 290.5575069072837664, -17.68249398312240928 ) ) ;
#48004 = ORIENTED_EDGE ( 'NONE', *, *, #57294, .F. ) ;
#48005 = CARTESIAN_POINT ( 'NONE',  ( 19.63753723929501760, 13.19860640527291551, 2.839279412974134775 ) ) ;
#48006 = CARTESIAN_POINT ( 'NONE',  ( 63.28708487846012076, 207.3458772461660544, 9.188101187500095079 ) ) ;
#48007 = CARTESIAN_POINT ( 'NONE',  ( 76.62859868508415673, 63.47930858090246176, 15.36151106740648409 ) ) ;
#48008 = CARTESIAN_POINT ( 'NONE',  ( 94.51141663858166453, 213.8262482093457493, 3.021315404115420679E-15 ) ) ;
#48009 = VECTOR ( 'NONE', #96334, 999.9999999999998863 ) ;
#48010 = CARTESIAN_POINT ( 'NONE',  ( 159.9307118030769175, 253.6388767968520881, 16.60600887889890487 ) ) ;
#48011 = CARTESIAN_POINT ( 'NONE',  ( -67.83107014231842413, 42.28230845022618922, 10.00000000000000000 ) ) ;
#48012 = CARTESIAN_POINT ( 'NONE',  ( 153.5280555550942267, 264.7286027217564879, 16.61052749018010388 ) ) ;
#48013 = CIRCLE ( 'NONE', #22136, 70.00000000000001421 ) ;
#48014 = DIRECTION ( 'NONE',  ( -0.7715546603183375263, -0.6361630342459823062, 0.000000000000000000 ) ) ;
#48015 = CARTESIAN_POINT ( 'NONE',  ( 125.7401460302306759, 236.7365022471902023, 10.00000000000009592 ) ) ;
#48016 = CYLINDRICAL_SURFACE ( 'NONE', #6809, 15.50000000000000000 ) ;
#48017 = ADVANCED_FACE ( 'NONE', ( #93559 ), #63123, .F. ) ;
#48018 = CARTESIAN_POINT ( 'NONE',  ( 207.6508796976096107, 270.9851214578045528, 6.713685698622268383 ) ) ;
#48019 = ORIENTED_EDGE ( 'NONE', *, *, #57729, .T. ) ;
#48020 = CARTESIAN_POINT ( 'NONE',  ( 86.25434633476642432, 46.76098024266752873, 9.759940948247864512 ) ) ;
#48021 = CARTESIAN_POINT ( 'NONE',  ( 82.29966782571446515, 53.62663270485408162, 15.81823675489985703 ) ) ;
#48022 = ORIENTED_EDGE ( 'NONE', *, *, #92557, .F. ) ;
#48023 = CARTESIAN_POINT ( 'NONE',  ( 159.9997000813754084, 253.5193855937126841, -16.28798248637880519 ) ) ;
#48024 = CARTESIAN_POINT ( 'NONE',  ( 207.3206384775119488, 270.4334275325076646, -0.2364287663163220921 ) ) ;
#48025 = CARTESIAN_POINT ( 'NONE',  ( 70.46465484163427107, 68.90236690406180742, -7.952911809055608572 ) ) ;
#48026 = VERTEX_POINT ( 'NONE', #94067 ) ;
#48028 = EDGE_CURVE ( 'NONE', #40468, #39976, #24618, .T. ) ;
#48027 = CARTESIAN_POINT ( 'NONE',  ( 50.30020549591841927, 90.50945844122861672, -10.00000000000000000 ) ) ;
#48029 = ORIENTED_EDGE ( 'NONE', *, *, #51816, .T. ) ;
#48031 = EDGE_CURVE ( 'NONE', #40710, #21425, #96666, .T. ) ;
#48030 = CARTESIAN_POINT ( 'NONE',  ( 79.14312167556931854, 57.64441083166269664, 0.000000000000000000 ) ) ;
#48032 = CARTESIAN_POINT ( 'NONE',  ( 170.3389527966260175, 250.2486659550142178, 3.410583519328374003 ) ) ;
#48033 = CARTESIAN_POINT ( 'NONE',  ( 148.4796866745341219, 273.9119512061620298, 7.990242866642934594 ) ) ;
#48034 = EDGE_LOOP ( 'NONE', ( #18496, #7180, #79371, #54784 ) ) ;
#48035 = CARTESIAN_POINT ( 'NONE',  ( 27.77157046966360809, 18.96004757982091249, -5.678558825948275768 ) ) ;
#48036 = CARTESIAN_POINT ( 'NONE',  ( 75.14516343145004384, 66.38879684927510993, -13.15419235483435045 ) ) ;
#48037 = CARTESIAN_POINT ( 'NONE',  ( 82.20012801274769743, 48.57593112100128252, -13.18042320071303664 ) ) ;
#48038 = ADVANCED_FACE ( 'NONE', ( #1335 ), #3647, .F. ) ;
#48039 = ADVANCED_FACE ( 'NONE', ( #85053 ), #39891, .T. ) ;
#48040 = VERTEX_POINT ( 'NONE', #48008 ) ;
#48041 = CARTESIAN_POINT ( 'NONE',  ( 81.56753329430793542, 59.44520672954722329, 0.3596699001693225983 ) ) ;
#48042 = CARTESIAN_POINT ( 'NONE',  ( -32.30932376655839988, 25.48519649537502119, -10.00000000000000000 ) ) ;
#48043 = ORIENTED_EDGE ( 'NONE', *, *, #75358, .T. ) ;
#48044 = ORIENTED_EDGE ( 'NONE', *, *, #3015, .F. ) ;
#48045 = CARTESIAN_POINT ( 'NONE',  ( 192.1943038168404314, 277.1473907896511264, 17.36549850453357635 ) ) ;
#48047 = CARTESIAN_POINT ( 'NONE',  ( 194.8598199529639317, 293.1398868181796615, -15.91766051364927570 ) ) ;
#48046 = CARTESIAN_POINT ( 'NONE',  ( 67.67694934082794589, 65.73157130137430215, 10.65708354426730864 ) ) ;
#48048 = CARTESIAN_POINT ( 'NONE',  ( 81.74146036984987518, 55.29309318191306488, -15.92173512836979654 ) ) ;
#48049 = CARTESIAN_POINT ( 'NONE',  ( 155.6276701977099890, 261.0919634844306643, 17.49722577287685255 ) ) ;
#48050 = CARTESIAN_POINT ( 'NONE',  ( 186.2639079497381545, 293.1677061230143977, -10.74393367941972244 ) ) ;
#48051 = CARTESIAN_POINT ( 'NONE',  ( 157.1850763439666139, 258.3944569110938687, -16.98181238659443437 ) ) ;
#48052 = CARTESIAN_POINT ( 'NONE',  ( 142.9371257517045137, 259.7655487066560340, -7.305945665944389766 ) ) ;
#48053 = CARTESIAN_POINT ( 'NONE',  ( 74.90858141719442642, 61.82407377426982009, -15.58808111368598048 ) ) ;
#48054 = CARTESIAN_POINT ( 'NONE',  ( 79.53039288183295241, 59.52037319582147035, 16.54552321433123652 ) ) ;
#48055 = CARTESIAN_POINT ( 'NONE',  ( 84.85626976964255164, 228.9869531367911293, 4.594050593750046652 ) ) ;
#48056 = ORIENTED_EDGE ( 'NONE', *, *, #34182, .T. ) ;
#48057 = CARTESIAN_POINT ( 'NONE',  ( 151.3883635558152321, 268.4346579770563608, 15.44343517165679103 ) ) ;
#48058 = DIRECTION ( 'NONE',  ( -0.8660254037844377084, -0.5000000000000015543, -3.252519625699478541E-16 ) ) ;
#48059 = CIRCLE ( 'NONE', #4385, 70.00000000000001421 ) ;
#48060 = ORIENTED_EDGE ( 'NONE', *, *, #92636, .T. ) ;
#48061 = CARTESIAN_POINT ( 'NONE',  ( 195.9660570498024299, 291.2238279612380438, -17.10029777481811308 ) ) ;
#48062 = VECTOR ( 'NONE', #87336, 1000.000000000000227 ) ;
#48063 = ORIENTED_EDGE ( 'NONE', *, *, #3118, .T. ) ;
#48064 = CARTESIAN_POINT ( 'NONE',  ( 80.39210556992956924, 44.73937495152041777, -11.68521036719157458 ) ) ;
#48065 = DIRECTION ( 'NONE',  ( -1.000000000000000000, 0.000000000000000000, 0.000000000000000000 ) ) ;
#48067 = B_SPLINE_SURFACE_WITH_KNOTS ( 'NONE', 3, 1, ( 
 ( #16366, #665 ),
 ( #17360, #48779 ),
 ( #62439, #15856 ),
 ( #23954, #93406 ),
 ( #40648, #1685 ),
 ( #40144, #41144 ),
 ( #79711, #33064 ),
 ( #70558, #10274 ),
 ( #71586, #47257 ),
 ( #24465, #94900 ),
 ( #16859, #32048 ),
 ( #47746, #71086 ),
 ( #63958, #77689 ),
 ( #78178, #1175 ),
 ( #78683, #32570 ),
 ( #94402, #24956 ),
 ( #2181, #25463 ),
 ( #56351, #87352 ),
 ( #72082, #2683 ),
 ( #64468, #25982 ),
 ( #74582, #65459 ),
 ( #49272, #43132 ),
 ( #95916, #42640 ),
 ( #5161, #36040 ),
 ( #27478, #41652 ),
 ( #26970, #12778 ),
 ( #11292, #58346 ),
 ( #50255, #35049 ),
 ( #73086, #57852 ),
 ( #80209, #81208 ),
 ( #35555, #19876 ),
 ( #72593, #19396 ),
 ( #18377, #10777 ),
 ( #26476, #3199 ) ),
 .UNSPECIFIED., .T., .F., .F.,
 ( 4, 2, 2, 2, 2, 2, 2, 2, 2, 2, 2, 2, 2, 2, 2, 2, 4 ),
 ( 2, 2 ),
 ( 0.000000000000000000, 0.06250000000000000000, 0.1250000000000000000, 0.1875000000000000000, 0.2500000000000000000, 0.3125000000000000000, 0.3750000000000000000, 0.4375000000000000000, 0.5000000000000000000, 0.5625000000000000000, 0.6250000000000000000, 0.6875000000000000000, 0.7500000000000000000, 0.8125000000000000000, 0.8750000000000000000, 0.9375000000000000000, 1.000000000000000000 ),
 ( 0.000000000000000000, 1.000000000000000000 ),
 .UNSPECIFIED. ) ;
#48066 = CARTESIAN_POINT ( 'NONE',  ( -5.101858724868291617, 167.8615022471904012, 2.586156800657061008E-14 ) ) ;
#48068 = CARTESIAN_POINT ( 'NONE',  ( 164.0723032761492846, 249.9223654822971241, 10.21660028793007058 ) ) ;
#48069 = CARTESIAN_POINT ( 'NONE',  ( 84.80231054593309636, 47.28878989737494720, -11.15588628155341056 ) ) ;
#48070 = CARTESIAN_POINT ( 'NONE',  ( 207.8018416422513894, 270.7236476996756664, 1.610379135119299754 ) ) ;
#48071 = CARTESIAN_POINT ( 'NONE',  ( 86.99453030705913648, 221.0333772461660544, 9.188101187500095079 ) ) ;
#48072 = ORIENTED_EDGE ( 'NONE', *, *, #21324, .F. ) ;
#48073 = AXIS2_PLACEMENT_3D ( 'NONE', #97578, #80916, #65647 ) ;
#48074 = EDGE_LOOP ( 'NONE', ( #51583, #96177, #10935, #57918 ) ) ;
#48075 = CARTESIAN_POINT ( 'NONE',  ( 163.3723087697842971, 247.6778559913402091, -10.08585062664141319 ) ) ;
#48076 = ORIENTED_EDGE ( 'NONE', *, *, #81302, .F. ) ;
#48077 = EDGE_CURVE ( 'NONE', #89630, #96180, #62198, .T. ) ;
#48078 = CYLINDRICAL_SURFACE ( 'NONE', #75698, 17.82106496071139645 ) ;
#48079 = CARTESIAN_POINT ( 'NONE',  ( 164.7750468393942072, 284.9269967741507799, 0.5039332410673107443 ) ) ;
#48080 = DIRECTION ( 'NONE',  ( -0.5000000000000006661, 0.8660254037844382635, -1.877843081442120958E-16 ) ) ;
#48081 = CARTESIAN_POINT ( 'NONE',  ( 87.56490573087398843, 44.61754441107329683, 4.959165031671988189 ) ) ;
#48082 = EDGE_LOOP ( 'NONE', ( #83349, #8406, #6432, #87597 ) ) ;
#48083 = AXIS2_PLACEMENT_3D ( 'NONE', #93738, #9096, #7090 ) ;
#48084 = CARTESIAN_POINT ( 'NONE',  ( 84.25039669599603087, 43.70795126229808147, -6.896957926195620203 ) ) ;
#48085 = CARTESIAN_POINT ( 'NONE',  ( 160.7116691410181204, 275.5603374970829691, 13.86191725030325905 ) ) ;
#48086 = CARTESIAN_POINT ( 'NONE',  ( 159.2651917302844993, 254.7915913763855258, -16.53922207549818424 ) ) ;
#48087 = CARTESIAN_POINT ( 'NONE',  ( 155.9304167309410616, 262.0567994629158193, -16.96786909722664660 ) ) ;
#48088 = CARTESIAN_POINT ( 'NONE',  ( 174.7346703842556224, 283.9960318526788114, 13.82134370946545943 ) ) ;
#48089 = CARTESIAN_POINT ( 'NONE',  ( 198.6444633007815810, 284.5846922512318997, -17.80363864581810418 ) ) ;
#48090 = CARTESIAN_POINT ( 'NONE',  ( 195.5147172610062967, 279.6304477706623857, -17.34193691489010902 ) ) ;
#48091 = EDGE_LOOP ( 'NONE', ( #22006, #53496, #47300, #53256 ) ) ;
#48092 = CARTESIAN_POINT ( 'NONE',  ( 8.658876260137789771, 164.2592609112380160, 2.679491924311254714 ) ) ;
#48093 =( BOUNDED_CURVE ( )  B_SPLINE_CURVE ( 2, ( #11503, #95634, #27184, #64684, #42356, #26182, #52954, #61544, #61037 ),
 .UNSPECIFIED., .F., .F. ) 
 B_SPLINE_CURVE_WITH_KNOTS ( ( 3, 2, 2, 2, 3 ),
 ( 0.4637096774193548154, 0.4650537634408601906, 0.4677419354838709409, 0.4704301075268817467, 0.4717741935483871218 ),
 .UNSPECIFIED. ) 
 CURVE ( )  GEOMETRIC_REPRESENTATION_ITEM ( )  RATIONAL_B_SPLINE_CURVE ( ( 0.9330127018922194093, 0.9330127018922194093, 1.000000000000000000, 0.8660254037844387076, 1.000000000000000000, 0.8660254037844387076, 1.000000000000000000, 0.9330127018922194093, 0.9330127018922194093 ) ) 
 REPRESENTATION_ITEM ( '' )  );
#48094 = CARTESIAN_POINT ( 'NONE',  ( 200.1444820856229967, 283.9865835035790269, 17.93386694781497326 ) ) ;
#48095 = AXIS2_PLACEMENT_3D ( 'NONE', #52732, #83695, #68439 ) ;
#48096 = FACE_OUTER_BOUND ( 'NONE', #75086, .T. ) ;
#48097 = CARTESIAN_POINT ( 'NONE',  ( 187.9089654282127526, 266.1749911718636099, -11.87902348831128485 ) ) ;
#48098 = CARTESIAN_POINT ( 'NONE',  ( 78.01910789048406514, 61.79390329888819622, 16.07883194446994679 ) ) ;
#48099 = CARTESIAN_POINT ( 'NONE',  ( 175.1301202802792432, 290.1368936646978227, -6.315612267206111241 ) ) ;
#48100 = CARTESIAN_POINT ( 'NONE',  ( 156.9309300460126906, 272.6596396618500080, 14.48126528928379031 ) ) ;
#48101 = EDGE_LOOP ( 'NONE', ( #61807, #48546, #22777, #707 ) ) ;
#48102 = EDGE_CURVE ( 'NONE', #5362, #28497, #62702, .T. ) ;
#48103 = CARTESIAN_POINT ( 'NONE',  ( 207.1059763530604698, 271.9289217357780899, 6.370907250589925575 ) ) ;
#48105 = CARTESIAN_POINT ( 'NONE',  ( 73.83712343681983725, 55.22609035296176927, 16.12121283296830399 ) ) ;
#48104 = CARTESIAN_POINT ( 'NONE',  ( 180.6081384992149594, 267.0382346236909825, -16.05224082202179403 ) ) ;
#48106 = CARTESIAN_POINT ( 'NONE',  ( 199.4400349757259789, 281.3072289442092142, -16.75105224125054448 ) ) ;
#48107 = ADVANCED_FACE ( 'NONE', ( #24712 ), #39394, .F. ) ;
#48108 = CARTESIAN_POINT ( 'NONE',  ( 27.87997788293534285, 34.83478043621390441, -8.090169943749479842 ) ) ;
#48109 = DIRECTION ( 'NONE',  ( -0.000000000000000000, -0.000000000000000000, -1.000000000000000000 ) ) ;
#48110 = CARTESIAN_POINT ( 'NONE',  ( 169.2488921996751401, 273.1503855280286643, 15.96805902338648409 ) ) ;
#48111 =( BOUNDED_CURVE ( )  B_SPLINE_CURVE ( 2, ( #40924, #94685, #48557, #80497, #34832, #96191, #2984, #1957, #71871 ),
 .UNSPECIFIED., .F., .T. ) 
 B_SPLINE_CURVE_WITH_KNOTS ( ( 3, 2, 2, 2, 3 ),
 ( 0.5846774193548387455, 0.5860215053763441206, 0.5887096774193548709, 0.5913978494623656212, 0.5927419354838709964 ),
 .UNSPECIFIED. ) 
 CURVE ( )  GEOMETRIC_REPRESENTATION_ITEM ( )  RATIONAL_B_SPLINE_CURVE ( ( 0.9330127018922194093, 0.9330127018922194093, 1.000000000000000000, 0.8660254037844387076, 1.000000000000000000, 0.8660254037844387076, 1.000000000000000000, 0.9330127018922194093, 0.9330127018922194093 ) ) 
 REPRESENTATION_ITEM ( '' )  );
#48112 = CARTESIAN_POINT ( 'NONE',  ( 181.2820369676599910, 273.4109893422450455, 17.60600081488427193 ) ) ;
#48113 = CARTESIAN_POINT ( 'NONE',  ( 196.4164021072083983, 270.5621661862001019, 13.33908636140236936 ) ) ;
#48114 = CARTESIAN_POINT ( 'NONE',  ( 205.8889072768004951, 273.5716727396786041, -9.812782715980612025 ) ) ;
#48115 = EDGE_CURVE ( 'NONE', #77592, #91230, #25214, .T. ) ;
#48116 = CARTESIAN_POINT ( 'NONE',  ( 190.5526305594705434, 299.9695577504274979, -4.324655322867677398 ) ) ;
#48117 = CARTESIAN_POINT ( 'NONE',  ( -1.610867365518755978, 176.0024278399160949, 9.188101187500095079 ) ) ;
#48118 = CARTESIAN_POINT ( 'NONE',  ( 83.13520543127567919, 52.15262426605146118, 14.79738518802719049 ) ) ;
#48119 = ORIENTED_EDGE ( 'NONE', *, *, #28818, .T. ) ;
#48120 = CARTESIAN_POINT ( 'NONE',  ( 175.0080295257186265, 255.0607892082682895, 9.260279940284284805 ) ) ;
#48121 = CARTESIAN_POINT ( 'NONE',  ( 35.05457148360284236, 21.20801979619930933, -3.090169943749474069 ) ) ;
#48122 = CARTESIAN_POINT ( 'NONE',  ( 72.13088006912725803, 72.32200972276189077, -1.116376892176975000 ) ) ;
#48123 = CARTESIAN_POINT ( 'NONE',  ( 15.76359375002403596, 192.1589784336661637, -6.496448406907676862E-16 ) ) ;
#48124 = VECTOR ( 'NONE', #21441, 1000.000000000000114 ) ;
#48125 = CARTESIAN_POINT ( 'NONE',  ( 181.7217459927706216, 276.2532386564253670, -17.70126685545563916 ) ) ;
#48126 = CARTESIAN_POINT ( 'NONE',  ( 33.51440821012886317, 31.30066082961424456, -10.00000000000000533 ) ) ;
#48127 = DIRECTION ( 'NONE',  ( -0.8660254037844369313, -0.5000000000000029976, 0.000000000000000000 ) ) ;
#48128 = CARTESIAN_POINT ( 'NONE',  ( 147.2405539530007559, 275.6188749492528132, 0.4306668706573002492 ) ) ;
#48129 = VECTOR ( 'NONE', #19560, 1000.000000000000227 ) ;
#48130 = CARTESIAN_POINT ( 'NONE',  ( 196.3189437186685211, 290.6126103214480167, 17.40845986800375300 ) ) ;
#48131 = CARTESIAN_POINT ( 'NONE',  ( 73.29578800698439522, 66.59928693814347866, 12.71955346165220568 ) ) ;
#48132 = CARTESIAN_POINT ( 'NONE',  ( -22.42236680055709641, 157.8615022471902591, 0.000000000000000000 ) ) ;
#48133 = CARTESIAN_POINT ( 'NONE',  ( 156.6812872898450735, 261.2670451491295012, 0.000000000000000000 ) ) ;
#48134 = PLANE ( 'NONE',  #67878 ) ;
#48135 = AXIS2_PLACEMENT_3D ( 'NONE', #84778, #29546, #144 ) ;
#48136 = CARTESIAN_POINT ( 'NONE',  ( 77.09838585100470709, 201.9865022471901739, 1.119607411625061291E-15 ) ) ;
#48137 = CARTESIAN_POINT ( 'NONE',  ( 76.77731254116881132, 64.09355814141257213, -15.16545583891343263 ) ) ;
#48138 = DIRECTION ( 'NONE',  ( 1.000000000000000000, 0.000000000000000000, 0.000000000000000000 ) ) ;
#48139 = EDGE_CURVE ( 'NONE', #41560, #83225, #71648, .T. ) ;
#48140 = CARTESIAN_POINT ( 'NONE',  ( -22.42236680055709641, 157.8615022471902591, 0.000000000000000000 ) ) ;
#48141 = CARTESIAN_POINT ( 'NONE',  ( 34.35668405510998724, 181.4548013555409796, -4.594050593750042211 ) ) ;
#48142 = CARTESIAN_POINT ( 'NONE',  ( 197.9552487813401456, 287.7784468162186613, 17.26493623863614602 ) ) ;
#48143 = CARTESIAN_POINT ( 'NONE',  ( 69.37632600059342280, 210.8615022471902591, -10.00000000000009592 ) ) ;
#48144 = CARTESIAN_POINT ( 'NONE',  ( 171.3928239984006723, 250.3015599828365509, -5.796133048607560845 ) ) ;
#48145 = FACE_OUTER_BOUND ( 'NONE', #14549, .T. ) ;
#48146 = VERTEX_POINT ( 'NONE', #21563 ) ;
#48147 = CARTESIAN_POINT ( 'NONE',  ( 66.31687960855757069, 69.41545726844323383, 0.05603871075114778139 ) ) ;
#48148 = LINE ( 'NONE', #69076, #92757 ) ;
#48149 = DIRECTION ( 'NONE',  ( -0.8660254037844387076, -0.4999999999999998890, -0.000000000000000000 ) ) ;
#48150 = CARTESIAN_POINT ( 'NONE',  ( -19.65312891409030271, 93.06504152958497400, 59.99999999999999289 ) ) ;
#48151 = CARTESIAN_POINT ( 'NONE',  ( 28.38260615371904905, 22.10170272979928185, -7.433330006724141015 ) ) ;
#48152 = CARTESIAN_POINT ( 'NONE',  ( 163.1014434023538513, 248.1470085697407058, 9.692260209037655727 ) ) ;
#48153 = CARTESIAN_POINT ( 'NONE',  ( 196.8363552541316324, 289.7164272536036265, -17.80258609350122967 ) ) ;
#48154 = CARTESIAN_POINT ( 'NONE',  ( 185.8051906529039172, 267.9722644852660096, -14.39617185440305747 ) ) ;
#48155 = EDGE_LOOP ( 'NONE', ( #67861, #17065, #99149, #43197 ) ) ;
#48156 = VECTOR ( 'NONE', #76833, 1000.000000000000227 ) ;
#48157 = CARTESIAN_POINT ( 'NONE',  ( 185.4481162553822173, 290.9827097585334741, 13.29153407209991755 ) ) ;
#48158 = CARTESIAN_POINT ( 'NONE',  ( 6.089662503932698812, 18.91421378149916421, 9.188101187500008038 ) ) ;
#48159 = CARTESIAN_POINT ( 'NONE',  ( 76.39671315866488044, 58.77431009255887062, -16.02812391186772700 ) ) ;
#48160 = CARTESIAN_POINT ( 'NONE',  ( 71.59149729713742261, 72.39908022291972145, -1.330894502438451754 ) ) ;
#48161 = EDGE_CURVE ( 'NONE', #29721, #70849, #60531, .T. ) ;
#48162 = ORIENTED_EDGE ( 'NONE', *, *, #28815, .F. ) ;
#48163 = CARTESIAN_POINT ( 'NONE',  ( 182.0338464029501040, 278.3680066549227945, 17.69288446120480174 ) ) ;
#48164 = CARTESIAN_POINT ( 'NONE',  ( 72.11718761729461846, 71.53392678631075796, -5.852761162471809442 ) ) ;
#48165 = CARTESIAN_POINT ( 'NONE',  ( 85.34302531380257051, 49.09540806577671646, 12.42140015106420847 ) ) ;
#48166 = LINE ( 'NONE', #79107, #50107 ) ;
#48167 = CARTESIAN_POINT ( 'NONE',  ( 149.7128599965862463, 271.3367152699035501, 12.33532264622322394 ) ) ;
#48168 = ORIENTED_EDGE ( 'NONE', *, *, #3849, .F. ) ;
#48169 = VERTEX_POINT ( 'NONE', #91000 ) ;
#48171 = PRESENTATION_STYLE_ASSIGNMENT (( #17268 ) ) ;
#48170 = CARTESIAN_POINT ( 'NONE',  ( 189.5591655548766425, 274.6138781789617838, -16.86315132615974832 ) ) ;
#48172 = ORIENTED_EDGE ( 'NONE', *, *, #52238, .T. ) ;
#48173 = CARTESIAN_POINT ( 'NONE',  ( 152.6621968174709991, 266.2283140474973493, -17.02835521334403168 ) ) ;
#48174 = CARTESIAN_POINT ( 'NONE',  ( -13.76211276271269668, 162.8615022471902591, 0.000000000000000000 ) ) ;
#48175 = CARTESIAN_POINT ( 'NONE',  ( 72.77847538495844049, 57.31112570069235090, -15.86834930776232255 ) ) ;
#48176 = DIRECTION ( 'NONE',  ( 0.000000000000000000, 0.000000000000000000, -1.000000000000000000 ) ) ;
#48177 = FACE_OUTER_BOUND ( 'NONE', #60044, .T. ) ;
#48178 = CARTESIAN_POINT ( 'NONE',  ( 100.3364738622893810, 237.9244531367911009, -4.594050593750046652 ) ) ;
#48179 = CARTESIAN_POINT ( 'NONE',  ( 196.3174919959537306, 290.6151247789487684, -17.61248417473235151 ) ) ;
#48180 = EDGE_CURVE ( 'NONE', #33184, #40534, #79017, .T. ) ;
#48181 = CARTESIAN_POINT ( 'NONE',  ( 184.1766470405371194, 288.8506743398048684, -13.13675576434501835 ) ) ;
#48182 = ORIENTED_EDGE ( 'NONE', *, *, #9124, .T. ) ;
#48183 = CARTESIAN_POINT ( 'NONE',  ( 208.1876422586379647, 270.0554214305024630, 3.377638779759113863 ) ) ;
#48184 = VERTEX_POINT ( 'NONE', #79303 ) ;
#48185 = CARTESIAN_POINT ( 'NONE',  ( 30.18562306610639112, 29.37878583063842441, 9.188101187500006262 ) ) ;
#48186 = CARTESIAN_POINT ( 'NONE',  ( 198.2819808855875863, 287.2125302111982705, 18.53535247371401695 ) ) ;
#48187 = CARTESIAN_POINT ( 'NONE',  ( 78.29597207138884585, 47.82683086104820092, -14.50971761538352744 ) ) ;
#48188 = CARTESIAN_POINT ( 'NONE',  ( 53.21953955946602122, 201.5333772461660544, 9.188101187500095079 ) ) ;
#48189 = CARTESIAN_POINT ( 'NONE',  ( 73.85129109314340212, 68.53037146055885387, 11.40305250113368629 ) ) ;
#48190 = CARTESIAN_POINT ( 'NONE',  ( 151.0778907302193943, 268.9724126853576536, 15.84769371787143832 ) ) ;
#48191 = CARTESIAN_POINT ( 'NONE',  ( 150.2950809960438221, 270.3282789176094525, 14.12607625385173193 ) ) ;
#48192 = CARTESIAN_POINT ( 'NONE',  ( 173.0661364776218818, 271.2294764343828319, 16.42400051025034458 ) ) ;
#48193 = ORIENTED_EDGE ( 'NONE', *, *, #66082, .F. ) ;
#48194 = DIRECTION ( 'NONE',  ( 0.06115825522547522347, -0.9981280818701454560, -0.000000000000000000 ) ) ;
#48195 = CARTESIAN_POINT ( 'NONE',  ( 177.5535686395006962, 288.9327453076302277, 11.22957305193713928 ) ) ;
#48196 = CARTESIAN_POINT ( 'NONE',  ( 77.08943580299947484, 49.61595851769168064, 15.51385818994994459 ) ) ;
#48197 = VECTOR ( 'NONE', #97503, 1000.000000000000000 ) ;
#48198 = ORIENTED_EDGE ( 'NONE', *, *, #46124, .F. ) ;
#48199 = LINE ( 'NONE', #79146, #43128 ) ;
#48200 = CARTESIAN_POINT ( 'NONE',  ( 71.05045428464670465, 69.84340204859232415, -6.994201869904678404 ) ) ;
#48201 = B_SPLINE_CURVE_WITH_KNOTS ( 'NONE', 3,
 ( #81677, #90284, #83670, #14233, #5140, #96885, #89774, #89301, #19854, #50722, #43108, #74052, #26977, #3206, #80726, #89803, #19883, #12787, #27955, #18890, #42159, #73095, #90310, #58836, #97878, #35056, #43650, #3687, #41659, #34566, #82215, #43139, #74589, #82712, #20882, #51247, #65468, #81215, #26484, #4160, #96409, #72603, #57859, #88840, #19403, #96914, #89330, #50262, #11789, #11301, #5167, #59330 ),
 .UNSPECIFIED., .F., .F.,
 ( 4, 2, 2, 2, 2, 2, 2, 2, 2, 2, 2, 2, 2, 2, 2, 2, 2, 2, 2, 2, 2, 2, 2, 2, 2, 4 ),
 ( 0.0001359809603122414388, 0.0006282668108888124145, 0.001120552661465383255, 0.001366695586753668675, 0.001612838512041954312, 0.001735909974686074362, 0.001858981437330194629, 0.001982052899974314896, 0.002105124362618435163, 0.002597410213194750132, 0.003089696063771064666, 0.004074267764923540647, 0.005058839466076017928, 0.005551125316652261339, 0.005797268241940383912, 0.005920339704584443898, 0.006043411167228504750, 0.006104946898550515227, 0.006166482629872525704, 0.006289554092516613445, 0.006535697017804746427, 0.006781839943092880275, 0.007027982868381014124, 0.007274125793669147105, 0.007520268718957280087, 0.008012554569533536508 ),
 .UNSPECIFIED. ) ;
#48202 = CARTESIAN_POINT ( 'NONE',  ( -22.42236680055709641, 157.8615022471902591, 0.000000000000000000 ) ) ;
#48203 = CARTESIAN_POINT ( 'NONE',  ( 192.4743214706506365, 297.2716913909250707, -12.17804856100553046 ) ) ;
#48204 = CARTESIAN_POINT ( 'NONE',  ( 149.2511585606875428, 272.1364056148075292, 11.40684181024752242 ) ) ;
#48205 = B_SPLINE_CURVE_WITH_KNOTS ( 'NONE', 3,
 ( #855, #62637, #93593, #24160, #1868, #94100, #55045, #86026, #70758, #24652, #86519, #47942, #32752, #34747, #66157, #89039, #49454, #42830, #2379, #48968, #48466, #96103, #41344, #11970, #80409, #19586, #3387, #33258, #34259, #95619, #42340, #79902, #73765, #26167, #71780, #57045, #64159, #33785, #95109, #88026, #4356, #58056, #10467, #72797, #50450, #2889, #72285, #64670, #18576, #10979 ),
 .UNSPECIFIED., .F., .F.,
 ( 4, 2, 2, 2, 2, 2, 2, 2, 2, 2, 2, 2, 2, 2, 2, 2, 2, 2, 2, 2, 2, 2, 2, 2, 4 ),
 ( 0.0001777596983279888224, 0.001185089187328521899, 0.001688753931828796068, 0.001940586304078896181, 0.002066502490203914362, 0.002192418676328932326, 0.002318334862453950290, 0.002444251048578967821, 0.002696083420829005917, 0.003199748165329127213, 0.004207077654329402332, 0.005214407143329677016, 0.005718071887829815660, 0.005969904260079806485, 0.006221736632329797310, 0.006284694725392295234, 0.006347652818454793157, 0.006410610911517290213, 0.006473569004579788136, 0.006725401376829856157, 0.006977233749079924177, 0.007229066121329991330, 0.007480898493580059351, 0.007732730865830127372, 0.008236395610330311118 ),
 .UNSPECIFIED. ) ;
#48206 = AXIS2_PLACEMENT_3D ( 'NONE', #26786, #17176, #57168 ) ;
#48207 = CARTESIAN_POINT ( 'NONE',  ( 180.8410963975274228, 271.3820433072099263, 16.71430284973371627 ) ) ;
#48208 = CARTESIAN_POINT ( 'NONE',  ( 83.13810225994288317, 42.45549248814388932, -6.801163518002313779 ) ) ;
#48209 = CARTESIAN_POINT ( 'NONE',  ( 76.04328680567357424, 65.50720358278793753, 13.94868768647875612 ) ) ;
#48210 = CARTESIAN_POINT ( 'NONE',  ( 72.69105027424014054, 65.04613689808410015, -12.99582216046819205 ) ) ;
#48211 = DIRECTION ( 'NONE',  ( 0.000000000000000000, 0.000000000000000000, 1.000000000000000000 ) ) ;
#48212 = VECTOR ( 'NONE', #44803, 1000.000000000000000 ) ;
#48213 = CARTESIAN_POINT ( 'NONE',  ( 116.7102005222951817, 232.0643266524159856, -9.188101187500093303 ) ) ;
#48214 = ORIENTED_EDGE ( 'NONE', *, *, #97235, .T. ) ;
#48215 = CARTESIAN_POINT ( 'NONE',  ( 146.8637854207107409, 276.2714571898724216, 0.7988785540157756770 ) ) ;
#48216 = CARTESIAN_POINT ( 'NONE',  ( 86.13879346367242817, 46.95025718893440825, -10.63009676298479356 ) ) ;
#48217 = CARTESIAN_POINT ( 'NONE',  ( 204.1780753366177237, 277.0001950557890495, 14.05599973203924158 ) ) ;
#48218 = CARTESIAN_POINT ( 'NONE',  ( 83.81598819787330967, 51.53879304665028371, -14.37095643376077092 ) ) ;
#48219 = CARTESIAN_POINT ( 'NONE',  ( 175.3791991197070672, 252.5596894157395980, 5.239567693004966387 ) ) ;
#48220 = VERTEX_POINT ( 'NONE', #71169 ) ;
#48221 = CARTESIAN_POINT ( 'NONE',  ( 174.7762878479638857, 265.7456530501560792, -17.06323711782486541 ) ) ;
#48222 = VECTOR ( 'NONE', #100101, 999.9999999999998863 ) ;
#48223 = CARTESIAN_POINT ( 'NONE',  ( 155.9194312736545385, 273.7031741143842964, -12.76921509093127050 ) ) ;
#48224 = CARTESIAN_POINT ( 'NONE',  ( 181.9855612025720575, 260.5135956200978740, 9.640126796794145747 ) ) ;
#48225 = CARTESIAN_POINT ( 'NONE',  ( 164.9825360643182535, 244.8888605054729624, -1.157747536866345461 ) ) ;
#48226 = CARTESIAN_POINT ( 'NONE',  ( 123.8274129399422918, 251.4869531367911577, 4.594050593750046652 ) ) ;
#48227 = CARTESIAN_POINT ( 'NONE',  ( 190.5153763745130675, 294.7680481657044993, -12.25754067625421229 ) ) ;
#48228 = AXIS2_PLACEMENT_3D ( 'NONE', #9309, #40183, #71123 ) ;
#48229 = CYLINDRICAL_SURFACE ( 'NONE', #33611, 10.00000000000010658 ) ;
#48230 = CARTESIAN_POINT ( 'NONE',  ( 133.7124848875370731, 259.5530062829863596, -4.648177544792955347E-16 ) ) ;
#48231 = CARTESIAN_POINT ( 'NONE',  ( 53.65289935712325331, 189.5327760586659451, 1.948934522072303157E-15 ) ) ;
#48232 = B_SPLINE_CURVE_WITH_KNOTS ( 'NONE', 3,
 ( #56727, #10644, #94764, #57713, #87710, #25327, #49139, #88192, #50130, #2039, #80073, #81082, #11648, #72462, #42508, #82076, #82580, #4523, #67827, #20239, #35424, #98242, #13632, #50612, #89199, #91155, #44506, #75953, #43516, #45007, #6529, #81566, #52112, #65812, #5526, #75435, #60195, #28828, #73937, #51628, #5035, #36410, #74942, #12137, #74455, #42999, #6019, #89678, #13143, #44000 ),
 .UNSPECIFIED., .F., .F.,
 ( 4, 2, 2, 2, 2, 2, 2, 2, 2, 2, 2, 2, 2, 2, 2, 2, 2, 2, 2, 2, 2, 2, 2, 2, 4 ),
 ( 0.002843746976746490841, 0.003047737582608842262, 0.003251728188471194117, 0.003353723491402369611, 0.003455718794333545105, 0.003557714097264720165, 0.003659709400195895659, 0.003863700006058367210, 0.004067690611920839194, 0.004475671823645782296, 0.005291634247095621663, 0.006107596670545461029, 0.006923559093995300395, 0.007739521517445139762, 0.007841516820376355154, 0.007892514471841962850, 0.007943512123307570547, 0.007994509774773178243, 0.008045507426238784204, 0.008147502729170008270, 0.008555483940894892392, 0.008759474546757333585, 0.008963465152619774778, 0.009167455758482215972, 0.009371446364344657165 ),
 .UNSPECIFIED. ) ;
#48233 = CARTESIAN_POINT ( 'NONE',  ( 85.33699565288863198, 48.33901173460943568, -12.30238903177782817 ) ) ;
#48234 = CARTESIAN_POINT ( 'NONE',  ( 205.2941531242069857, 275.0670916224857478, -13.92605142593109058 ) ) ;
#48235 = CARTESIAN_POINT ( 'NONE',  ( 185.9427433571077586, 257.7868782628476083, -2.501399907045548598 ) ) ;
#48236 = ADVANCED_FACE ( 'NONE', ( #79796 ), #70127, .F. ) ;
#48237 = CARTESIAN_POINT ( 'NONE',  ( 171.6037788498051953, 259.8733260417915290, 15.41710503213636763 ) ) ;
#48238 = DIRECTION ( 'NONE',  ( -0.8660254037844378194, -0.5000000000000014433, -0.000000000000000000 ) ) ;
#48239 = CARTESIAN_POINT ( 'NONE',  ( 178.8732274734658745, 291.7255955964181453, -6.546936884515894839 ) ) ;
#48240 = CARTESIAN_POINT ( 'NONE',  ( 155.5211745099813356, 261.2764194263634749, -17.18163098020766810 ) ) ;
#48241 = ADVANCED_FACE ( 'NONE', ( #17969 ), #88636, .T. ) ;
#48242 = CARTESIAN_POINT ( 'NONE',  ( 178.9139577745172858, 261.4084931650070871, 12.21660760478297370 ) ) ;
#48243 = VECTOR ( 'NONE', #84289, 1000.000000000000000 ) ;
#48244 = CARTESIAN_POINT ( 'NONE',  ( 120.6702889753613022, 247.1427522451419065, 10.00000000000009237 ) ) ;
#48245 = EDGE_CURVE ( 'NONE', #7074, #18151, #99448, .T. ) ;
#48246 = CARTESIAN_POINT ( 'NONE',  ( 75.36487073175837281, 53.53173320265494084, -16.04382577248123809 ) ) ;
#48247 = VERTEX_POINT ( 'NONE', #81291 ) ;
#48248 = ADVANCED_FACE ( 'NONE', ( #3275 ), #81783, .T. ) ;
#48249 = CARTESIAN_POINT ( 'NONE',  ( 147.7978300115112233, 274.6536445020713018, 7.902890709649431855 ) ) ;
#48250 = CARTESIAN_POINT ( 'NONE',  ( 88.03824807523534446, 44.69492972130227315, 4.342143822040329226 ) ) ;
#48251 = CARTESIAN_POINT ( 'NONE',  ( 24.99226373304320958, 194.4244531367911293, -4.594050593750046652 ) ) ;
#48252 = CARTESIAN_POINT ( 'NONE',  ( 12.20045371381521626, 28.81751292744055704, -6.180339887498951690 ) ) ;
#48253 = CARTESIAN_POINT ( 'NONE',  ( 68.45344762042827824, 64.57392882346940155, 12.12708197196866600 ) ) ;
#48254 = CARTESIAN_POINT ( 'NONE',  ( 31.25085430583858681, 200.3967562850347122, -4.648177544792955347E-16 ) ) ;
#48255 = CARTESIAN_POINT ( 'NONE',  ( 72.28203645621837836, 72.07279491845184793, 3.271428334514307590 ) ) ;
#48257 = CARTESIAN_POINT ( 'NONE',  ( 57.45043449909725553, 210.6427522451419634, -10.00000000000009415 ) ) ;
#48256 = PLANE ( 'NONE',  #59006 ) ;
#48258 = CARTESIAN_POINT ( 'NONE',  ( 35.21268636174862365, 20.73415679381824006, 1.333680081654574804E-15 ) ) ;
#48259 = CARTESIAN_POINT ( 'NONE',  ( 47.72569090598238972, 198.3615022471903728, 4.570193772333722408E-14 ) ) ;
#48260 = CARTESIAN_POINT ( 'NONE',  ( -52.01928280585847375, 85.51831290684647513, -10.00000000000000000 ) ) ;
#48261 = DIRECTION ( 'NONE',  ( -0.5000000000000082157, 0.8660254037844338226, 0.000000000000000000 ) ) ;
#48262 = EDGE_LOOP ( 'NONE', ( #48790, #93328, #18202, #96936 ) ) ;
#48263 = CARTESIAN_POINT ( 'NONE',  ( 161.9103913065419249, 267.1972571684306104, 16.48826679605286216 ) ) ;
#48264 = CARTESIAN_POINT ( 'NONE',  ( 29.61132621015795863, 181.2365022471902307, 10.00000000000009592 ) ) ;
#48265 = CARTESIAN_POINT ( 'NONE',  ( 66.85524610400479162, 67.34209505064850987, -6.990925417236247164 ) ) ;
#48266 = CARTESIAN_POINT ( 'NONE',  ( 74.56414817410227158, 187.8759306620403322, 17.47570218321535762 ) ) ;
#48267 = AXIS2_PLACEMENT_3D ( 'NONE', #26417, #34992, #74020 ) ;
#48268 = CARTESIAN_POINT ( 'NONE',  ( -12.81524457486244550, 175.6589784336661353, -6.496448406907675876E-16 ) ) ;
#48269 = CARTESIAN_POINT ( 'NONE',  ( 33.97448420766330202, 31.56628583063843152, 9.188101187500006262 ) ) ;
#48272 = CYLINDRICAL_SURFACE ( 'NONE', #53241, 70.00000000000002842 ) ;
#48271 = PLANE ( 'NONE',  #31389 ) ;
#48270 = B_SPLINE_CURVE_WITH_KNOTS ( 'NONE', 3,
 ( #62480, #1213, #71124, #55872 ),
 .UNSPECIFIED., .F., .F.,
 ( 4, 4 ),
 ( 0.008820457929765233851, 0.01706750817050696478 ),
 .UNSPECIFIED. ) ;
#48273 = CARTESIAN_POINT ( 'NONE',  ( 153.4619471835925708, 264.8431057800031567, 16.95044998314351758 ) ) ;
#48274 = CARTESIAN_POINT ( 'NONE',  ( 31.05045217176252237, 26.43085787977764767, -9.188101187500008038 ) ) ;
#48275 = DIRECTION ( 'NONE',  ( -0.7082622432767082810, -0.7059494278973847958, 0.000000000000000000 ) ) ;
#48277 = VECTOR ( 'NONE', #68823, 1000.000000000000000 ) ;
#48276 = CARTESIAN_POINT ( 'NONE',  ( 184.4794126637048066, 258.5029335018122083, -2.309405192791472938 ) ) ;
#48278 = CARTESIAN_POINT ( 'NONE',  ( 66.10780414051451714, 68.63670250712272036, 1.777645618418522533 ) ) ;
#48279 = VERTEX_POINT ( 'NONE', #20455 ) ;
#48280 = CARTESIAN_POINT ( 'NONE',  ( 149.6230451358742926, 271.4922791719315001, -12.72565967355361671 ) ) ;
#48281 = CARTESIAN_POINT ( 'NONE',  ( 160.1795347027651815, 282.8633239002924711, 5.491715875156680582 ) ) ;
#48282 =( NAMED_UNIT ( * ) PLANE_ANGLE_UNIT ( ) SI_UNIT ( $, .RADIAN. ) );
#48283 = AXIS2_PLACEMENT_3D ( 'NONE', #26934, #43612, #96872 ) ;
#48284 = CARTESIAN_POINT ( 'NONE',  ( 11.13306418284875576, 18.37878583063839244, 9.188101187500006262 ) ) ;
#48285 = CARTESIAN_POINT ( 'NONE',  ( -110.0000000000000000, 15.00000000000000000, 59.99999999999999289 ) ) ;
#48286 = CARTESIAN_POINT ( 'NONE',  ( 20.65814732634927609, 20.43085787977763346, -9.188101187500008038 ) ) ;
#48287 = DIRECTION ( 'NONE',  ( -1.000000000000000000, 0.000000000000000000, 0.000000000000000000 ) ) ;
#48288 = VECTOR ( 'NONE', #59373, 1000.000000000000000 ) ;
#48289 = PLANE ( 'NONE',  #63162 ) ;
#48290 = CARTESIAN_POINT ( 'NONE',  ( 88.03317622032373890, 44.09547299458050418, -1.704834311733967711 ) ) ;
#48291 = ORIENTED_EDGE ( 'NONE', *, *, #73168, .F. ) ;
#48292 = CARTESIAN_POINT ( 'NONE',  ( 32.88524308553003550, 19.39040679176984838, -6.890680421881970419E-14 ) ) ;
#48293 = CARTESIAN_POINT ( 'NONE',  ( 164.8329445879545290, 245.1479605429143760, -2.955380775890217304 ) ) ;
#48294 = FACE_OUTER_BOUND ( 'NONE', #71440, .T. ) ;
#48295 = CARTESIAN_POINT ( 'NONE',  ( 87.66085752470290515, 45.43799534522830896, 6.661108708518598043 ) ) ;
#48296 = LINE ( 'NONE', #32591, #98558 ) ;
#48297 = VERTEX_POINT ( 'NONE', #12358 ) ;
#48298 = VECTOR ( 'NONE', #53290, 1000.000000000000000 ) ;
#48299 = VERTEX_POINT ( 'NONE', #88413 ) ;
#48300 = CARTESIAN_POINT ( 'NONE',  ( 156.0847645221770392, 276.9562993373755830, -10.16876128128424561 ) ) ;
#48301 = CARTESIAN_POINT ( 'NONE',  ( 86.47146563682314024, 47.48338690922361138, 10.43545430509261607 ) ) ;
#48302 = ORIENTED_EDGE ( 'NONE', *, *, #23596, .T. ) ;
#48303 = LINE ( 'NONE', #40681, #9541 ) ;
#48304 = CARTESIAN_POINT ( 'NONE',  ( -70.89022602266994966, 47.22876919346843749, -10.00000000000000000 ) ) ;
#48305 = ORIENTED_EDGE ( 'NONE', *, *, #85127, .F. ) ;
#48306 = CARTESIAN_POINT ( 'NONE',  ( 78.33236083551435058, 61.59332569120734036, -15.80201694036198745 ) ) ;
#48307 = CARTESIAN_POINT ( 'NONE',  ( 78.94155721643029722, 59.44305089757030913, -16.52414004995257457 ) ) ;
#48308 = EDGE_CURVE ( 'NONE', #42896, #55151, #30528, .T. ) ;
#48309 = EDGE_CURVE ( 'NONE', #34164, #71353, #76476, .T. ) ;
#48310 = VERTEX_POINT ( 'NONE', #29052 ) ;
#48311 = CARTESIAN_POINT ( 'NONE',  ( 173.6791921498279692, 267.2095749298062515, 16.87208145038420781 ) ) ;
#48312 = CARTESIAN_POINT ( 'NONE',  ( -32.89710813242851373, 94.50490555674265636, 43.90259609869470125 ) ) ;
#48313 = CARTESIAN_POINT ( 'NONE',  ( 151.2057546125658973, 268.7509459446807227, 15.78031848731319187 ) ) ;
#48314 = B_SPLINE_SURFACE_WITH_KNOTS ( 'NONE', 3, 1, ( 
 ( #85075, #70333 ),
 ( #24245, #15622 ),
 ( #8054, #69338 ),
 ( #76456, #29842 ),
 ( #45525, #23228 ),
 ( #38927, #22236 ),
 ( #86108, #54616 ),
 ( #7036, #62219 ),
 ( #93171, #85600 ),
 ( #16635, #38423 ),
 ( #8544, #93680 ),
 ( #55122, #46014 ),
 ( #69832, #47531 ),
 ( #78459, #39416 ),
 ( #37424, #62723 ),
 ( #61228, #84094 ),
 ( #53137, #31334 ),
 ( #46521, #37917 ),
 ( #16140, #53626 ),
 ( #100259, #77458 ),
 ( #92193, #7532 ),
 ( #68828, #443 ),
 ( #99257, #47038 ),
 ( #77955, #68332 ),
 ( #945, #60712 ),
 ( #14646, #31821 ),
 ( #91674, #99754 ),
 ( #76930, #30339 ),
 ( #22746, #84581 ),
 ( #15120, #30842 ),
 ( #61727, #92675 ),
 ( #54116, #23722 ),
 ( #24732, #18149 ),
 ( #64239, #71357 ) ),
 .UNSPECIFIED., .T., .F., .F.,
 ( 4, 2, 2, 2, 2, 2, 2, 2, 2, 2, 2, 2, 2, 2, 2, 2, 4 ),
 ( 2, 2 ),
 ( 0.000000000000000000, 0.06250000000000000000, 0.1250000000000000000, 0.1875000000000000000, 0.2500000000000000000, 0.3125000000000000000, 0.3750000000000000000, 0.4375000000000000000, 0.5000000000000000000, 0.5625000000000000000, 0.6250000000000000000, 0.6875000000000000000, 0.7500000000000000000, 0.8125000000000000000, 0.8750000000000000000, 0.9375000000000000000, 1.000000000000000000 ),
 ( 0.000000000000000000, 1.000000000000000000 ),
 .UNSPECIFIED. ) ;
#48315 = ORIENTED_EDGE ( 'NONE', *, *, #5426, .F. ) ;
#48316 = CARTESIAN_POINT ( 'NONE',  ( 170.6575497776124166, 255.5351817509920522, -11.56051450327723451 ) ) ;
#48317 = DIRECTION ( 'NONE',  ( -0.1577859398657163181, 0.9874733399847778204, 0.000000000000000000 ) ) ;
#48318 = VERTEX_POINT ( 'NONE', #75644 ) ;
#48319 = ORIENTED_EDGE ( 'NONE', *, *, #3280, .T. ) ;
#48320 = CARTESIAN_POINT ( 'NONE',  ( 72.60116808109883380, 58.01589515306911693, 15.73743885619152394 ) ) ;
#48321 = ORIENTED_EDGE ( 'NONE', *, *, #65995, .F. ) ;
#48322 = CARTESIAN_POINT ( 'NONE',  ( 35.52150138090271980, 110.7651959890790039, 59.99999999999999289 ) ) ;
#48323 = EDGE_LOOP ( 'NONE', ( #64831, #18545, #29249, #44325 ) ) ;
#48324 = CARTESIAN_POINT ( 'NONE',  ( 82.29696812179142285, 46.31306431584521732, 11.46503684240460963 ) ) ;
#48326 = ADVANCED_FACE ( 'NONE', ( #22917 ), #76161, .T. ) ;
#48325 = CARTESIAN_POINT ( 'NONE',  ( -13.35616335646270691, 163.0958772461660544, -9.188101187500095079 ) ) ;
#48327 = CARTESIAN_POINT ( 'NONE',  ( 152.6757560589063303, 266.2048287524194166, 16.73757896668104195 ) ) ;
#48328 = LINE ( 'NONE', #40199, #45086 ) ;
#48329 = CARTESIAN_POINT ( 'NONE',  ( 11.72935026791635416, 51.93958514983272323, 59.99999999999999289 ) ) ;
#48330 = ORIENTED_EDGE ( 'NONE', *, *, #51647, .T. ) ;
#48331 = CARTESIAN_POINT ( 'NONE',  ( 75.98104421109889017, 51.53574906954565193, 16.18761828508177558 ) ) ;
#48332 = CARTESIAN_POINT ( 'NONE',  ( 27.97303175072023151, 18.01110640527293327, 2.839279412974134775 ) ) ;
#48333 = VECTOR ( 'NONE', #75797, 1000.000000000000227 ) ;
#48334 = CARTESIAN_POINT ( 'NONE',  ( 205.7576124508049418, 274.2643565215761328, 10.88614016733041545 ) ) ;
#48335 = DIRECTION ( 'NONE',  ( -0.7911563084720434347, -0.6116140086401625764, 0.000000000000000000 ) ) ;
#48337 = EDGE_LOOP ( 'NONE', ( #73896, #51139, #72639, #8691 ) ) ;
#48336 = CARTESIAN_POINT ( 'NONE',  ( 198.2489255580726422, 287.2697837179150042, 18.53597557040773225 ) ) ;
#48338 = ORIENTED_EDGE ( 'NONE', *, *, #46993, .F. ) ;
#48339 = CARTESIAN_POINT ( 'NONE',  ( 191.0989310468112308, 299.6539374852582114, 5.701794864544876162 ) ) ;
#48340 = PLANE ( 'NONE',  #12528 ) ;
#48341 = CARTESIAN_POINT ( 'NONE',  ( 206.1615484827472358, 273.5647187912443314, -9.556459874778100883 ) ) ;
#48342 = DIRECTION ( 'NONE',  ( 1.000000000000000000, 0.000000000000000000, 0.000000000000000000 ) ) ;
#48343 = CARTESIAN_POINT ( 'NONE',  ( 161.4469036912142599, 251.0127554125742222, 12.93933463576739307 ) ) ;
#48344 = CARTESIAN_POINT ( 'NONE',  ( 190.8693101975414947, 262.0387244596780079, -0.7334896453799415461 ) ) ;
#48345 = ORIENTED_EDGE ( 'NONE', *, *, #34475, .F. ) ;
#48346 = CARTESIAN_POINT ( 'NONE',  ( 175.3932935011599170, 269.2958584618301643, -17.65833184418574930 ) ) ;
#48347 = CARTESIAN_POINT ( 'NONE',  ( 14.42807667092211865, 8.734156793818204534, -7.779800476318352071E-15 ) ) ;
#48348 = CARTESIAN_POINT ( 'NONE',  ( 74.82458239918587140, 66.79921256097770765, -13.19236156228706847 ) ) ;
#48349 = AXIS2_PLACEMENT_3D ( 'NONE', #60644, #91600, #53064 ) ;
#48350 = CARTESIAN_POINT ( 'NONE',  ( 164.6649740431187183, 245.4388940607451843, -1.430729255012818557 ) ) ;
#48351 = CARTESIAN_POINT ( 'NONE',  ( 21.22170510744829741, 176.3927522451418213, -10.00000000000009059 ) ) ;
#48352 = CARTESIAN_POINT ( 'NONE',  ( 86.39896429407481548, 226.8149278399160664, 9.188101187500093303 ) ) ;
#48353 = CARTESIAN_POINT ( 'NONE',  ( 82.09771067107622855, 40.75407999355962119, -0.9479713174774019313 ) ) ;
#48354 = VECTOR ( 'NONE', #5273, 1000.000000000000227 ) ;
#48355 = CARTESIAN_POINT ( 'NONE',  ( 81.30975366074838462, 56.24313983998633404, -16.44754541364717326 ) ) ;
#48356 = CARTESIAN_POINT ( 'NONE',  ( 163.0682440866927720, 248.2045114712421423, 11.63988583931958942 ) ) ;
#48357 = AXIS2_PLACEMENT_3D ( 'NONE', #32362, #49556, #33362 ) ;
#48359 = CARTESIAN_POINT ( 'NONE',  ( 75.51323141522172477, 65.35427051582675517, 13.87231131232226922 ) ) ;
#48358 = CARTESIAN_POINT ( 'NONE',  ( 4.830370123010505168, 173.5958772461660828, -9.188101187500095079 ) ) ;
#48360 = CARTESIAN_POINT ( 'NONE',  ( 200.2631011806900005, 283.7811292041749311, 18.23377125296567058 ) ) ;
#48361 = EDGE_LOOP ( 'NONE', ( #79135, #41071, #10553, #49089, #63987 ) ) ;
#48362 = VECTOR ( 'NONE', #64749, 1000.000000000000114 ) ;
#48364 = ORIENTED_EDGE ( 'NONE', *, *, #30122, .T. ) ;
#48363 = UNCERTAINTY_MEASURE_WITH_UNIT (LENGTH_MEASURE( 1.000000000000000082E-05 ), #53726, 'distance_accuracy_value', 'NONE');
#48365 = CARTESIAN_POINT ( 'NONE',  ( 197.7405121978164289, 265.0121665675080749, -2.992171231212423343 ) ) ;
#48366 = CARTESIAN_POINT ( 'NONE',  ( 80.25009607139122636, 47.00733110321809960, -12.86902101113169294 ) ) ;
#48367 = CARTESIAN_POINT ( 'NONE',  ( 83.72222592155259235, 43.16924363288482880, 6.458418534604592587 ) ) ;
#48368 = DIRECTION ( 'NONE',  ( -0.4996954135095461047, 0.8654978445076770832, -0.03489949670251103753 ) ) ;
#48369 = CARTESIAN_POINT ( 'NONE',  ( 94.51141663858166453, 213.8262482093457493, 3.021315404115420679E-15 ) ) ;
#48370 = CARTESIAN_POINT ( 'NONE',  ( 74.40386970632725649, 67.99584678604389865, -11.66886300729125914 ) ) ;
#48371 = CARTESIAN_POINT ( 'NONE',  ( 24.99226373304320958, 194.4244531367911293, -4.594050593750046652 ) ) ;
#48372 = CARTESIAN_POINT ( 'NONE',  ( 82.20432729060253507, 208.2677522451417929, -5.000000000000041744 ) ) ;
#48373 = B_SPLINE_CURVE_WITH_KNOTS ( 'NONE', 3,
 ( #42243, #88425, #49855, #65552, #13367, #44231, #89892, #5744, #51342, #36634 ),
 .UNSPECIFIED., .F., .F.,
 ( 4, 2, 2, 2, 4 ),
 ( 0.000000000000000000, 0.0002622400424273647456, 0.0005244800848547294912, 0.0007867201272820942368, 0.001048960169709458982 ),
 .UNSPECIFIED. ) ;
#48374 = DIRECTION ( 'NONE',  ( -1.000000000000000000, 0.000000000000000000, 0.000000000000000000 ) ) ;
#48375 = VERTEX_POINT ( 'NONE', #14335 ) ;
#48376 = CARTESIAN_POINT ( 'NONE',  ( 84.55105187355179908, 49.10534814802225867, 12.70480211847229235 ) ) ;
#48377 = EDGE_CURVE ( 'NONE', #5980, #26753, #83774, .T. ) ;
#48378 = CARTESIAN_POINT ( 'NONE',  ( 173.9008529106967558, 272.4049662731551962, -17.79092985220220058 ) ) ;
#48379 = VECTOR ( 'NONE', #26569, 1000.000000000000000 ) ;
#48380 = CARTESIAN_POINT ( 'NONE',  ( -3.180017766230537557, 156.7202760586659736, -5.415160957724236172E-17 ) ) ;
#48381 = FACE_OUTER_BOUND ( 'NONE', #76933, .T. ) ;
#48382 = CARTESIAN_POINT ( 'NONE',  ( 161.8408514536557163, 250.3304178724980318, -14.12919723462510646 ) ) ;
#48383 = LINE ( 'NONE', #32671, #12786 ) ;
#48384 = CARTESIAN_POINT ( 'NONE',  ( 148.3625667886952044, 273.6754917110858401, -8.960758510948144462 ) ) ;
#48385 = CARTESIAN_POINT ( 'NONE',  ( 72.54275072821182846, 68.03364687615834328, -11.16216900646165122 ) ) ;
#48386 = CARTESIAN_POINT ( 'NONE',  ( 204.2457645315488719, 276.8829539310449945, 14.53406579917280261 ) ) ;
#48387 = CARTESIAN_POINT ( 'NONE',  ( 191.8232488616404225, 298.3993822291468518, -9.342381338555176384 ) ) ;
#48388 = CARTESIAN_POINT ( 'NONE',  ( 147.6857584380539095, 274.8477581613835810, 8.112022437684441201 ) ) ;
#48389 = VERTEX_POINT ( 'NONE', #68032 ) ;
#48390 = CARTESIAN_POINT ( 'NONE',  ( 143.8748646542946972, 242.3262482093457777, 3.021315404115420679E-15 ) ) ;
#48391 = CARTESIAN_POINT ( 'NONE',  ( 115.5733686319456126, 237.5333772461660544, 9.188101187500095079 ) ) ;
#48392 = CARTESIAN_POINT ( 'NONE',  ( 15.60392711327956761, 29.98502408145592213, -5.678558825948271327 ) ) ;
#48393 = CARTESIAN_POINT ( 'NONE',  ( 74.80730538133219909, 67.19677535317899242, 12.47566025441376603 ) ) ;
#48394 = CARTESIAN_POINT ( 'NONE',  ( 79.14312167556931854, 57.64441083166269664, 0.000000000000000000 ) ) ;
#48396 = DIRECTION ( 'NONE',  ( 0.000000000000000000, 0.000000000000000000, 1.000000000000000000 ) ) ;
#48395 = CARTESIAN_POINT ( 'NONE',  ( 157.3412122618683497, 258.1240215684019290, 16.75554199904894048 ) ) ;
#48397 = CARTESIAN_POINT ( 'NONE',  ( 204.6823371430232896, 272.9704135290961062, -9.754921121218281144 ) ) ;
#48398 = CARTESIAN_POINT ( 'NONE',  ( 189.7180314725545713, 261.4674912868679257, -4.463871536367752135 ) ) ;
#48399 = CARTESIAN_POINT ( 'NONE',  ( 196.2421909983451940, 290.7455499326673021, -17.31908925000307065 ) ) ;
#48400 = CARTESIAN_POINT ( 'NONE',  ( 45.79150443358504674, 28.29860640527296667, -2.839279412974138328 ) ) ;
#48401 = CARTESIAN_POINT ( 'NONE',  ( 172.5371125453617935, 290.7831369524994329, -1.769056789171790101 ) ) ;
#48402 = DIRECTION ( 'NONE',  ( 0.000000000000000000, 0.000000000000000000, 1.000000000000000000 ) ) ;
#48403 = ORIENTED_EDGE ( 'NONE', *, *, #90823, .T. ) ;
#48404 = CARTESIAN_POINT ( 'NONE',  ( 49.06003799288187395, 95.45573527953635562, -10.00000000000000000 ) ) ;
#48405 = CARTESIAN_POINT ( 'NONE',  ( 194.4390729088694627, 266.5749947481197069, -10.67130533956043692 ) ) ;
#48406 = VERTEX_POINT ( 'NONE', #99945 ) ;
#48407 = CARTESIAN_POINT ( 'NONE',  ( 72.12922596056051816, 72.33235173570187726, 1.011742168054688307 ) ) ;
#48408 = CARTESIAN_POINT ( 'NONE',  ( 78.56719005003022005, 47.98515344134877836, 13.96283253221395704 ) ) ;
#48409 = CARTESIAN_POINT ( 'NONE',  ( -11.87431992379006651, 23.49859753039504540, 177.5919119679930134 ) ) ;
#48410 = CARTESIAN_POINT ( 'NONE',  ( 166.8083734521890449, 257.5796782931630560, -15.79284703031436798 ) ) ;
#48411 = CARTESIAN_POINT ( 'NONE',  ( 74.96609828305089707, 53.12645705097258997, -16.02874109550557336 ) ) ;
#48412 = CARTESIAN_POINT ( 'NONE',  ( 192.1640094933931096, 297.8091675017319062, 12.36911124822534447 ) ) ;
#48413 = EDGE_LOOP ( 'NONE', ( #9831, #1736, #37212, #62057 ) ) ;
#48414 = CARTESIAN_POINT ( 'NONE',  ( 162.2577960498091443, 259.6413045848935894, 17.32708210747303212 ) ) ;
#48415 = CARTESIAN_POINT ( 'NONE',  ( 32.22500930073565684, 40.64646525600392835, -2.839279412974133887 ) ) ;
#48416 = CARTESIAN_POINT ( 'NONE',  ( 173.7814884173456846, 272.7086687150770103, -16.36263896858758926 ) ) ;
#48417 = VERTEX_POINT ( 'NONE', #44711 ) ;
#48418 = CARTESIAN_POINT ( 'NONE',  ( 167.7924589794888561, 280.8658978846934247, 11.87785029710499707 ) ) ;
#48419 = DIRECTION ( 'NONE',  ( 0.000000000000000000, 0.000000000000000000, 1.000000000000000000 ) ) ;
#48420 = CARTESIAN_POINT ( 'NONE',  ( 112.0822037211656266, 235.5177522451418781, -10.00000000000009592 ) ) ;
#48421 = EDGE_LOOP ( 'NONE', ( #21150, #10706, #43897 ) ) ;
#48422 = AXIS2_PLACEMENT_3D ( 'NONE', #12313, #7554, #15645 ) ;
#48423 = CARTESIAN_POINT ( 'NONE',  ( 79.36969597941133259, 59.79870839543468009, 16.16250099277175067 ) ) ;
#48424 = CARTESIAN_POINT ( 'NONE',  ( 188.5582800777447687, 293.2501195853826061, 12.57055310508630441 ) ) ;
#48425 = ADVANCED_FACE ( 'NONE', ( #45223 ), #6117, .F. ) ;
#48426 = VECTOR ( 'NONE', #76282, 999.9999999999998863 ) ;
#48427 = FACE_OUTER_BOUND ( 'NONE', #42835, .T. ) ;
#48428 = CARTESIAN_POINT ( 'NONE',  ( 84.76617582037141574, 50.00026310130547813, -13.66906362199170921 ) ) ;
#48429 = CARTESIAN_POINT ( 'NONE',  ( 154.9792334219179679, 262.2150889255981951, -17.21325849938693153 ) ) ;
#48430 = EDGE_LOOP ( 'NONE', ( #40454, #83505, #22016, #69839 ) ) ;
#48431 = B_SPLINE_CURVE_WITH_KNOTS ( 'NONE', 3,
 ( #33254, #49451, #50448, #97102, #34745, #58537, #48965, #11968, #64155, #27669, #3861, #19584, #89512, #56551, #41340, #25670, #35249, #79899, #72280, #58054, #2885, #66155, #27166, #64667, #33782, #50943, #18572, #73762, #10464, #81892, #40831, #95616, #4354, #42338, #26164, #65646, #57041, #96603, #73268, #88023, #80405, #19081, #10975, #71777 ),
 .UNSPECIFIED., .F., .F.,
 ( 4, 2, 2, 2, 2, 2, 2, 2, 2, 2, 2, 2, 2, 2, 2, 2, 2, 2, 2, 2, 2, 4 ),
 ( 0.002539959018451169899, 0.002952063888789773112, 0.003158116323959076887, 0.003261142541543766288, 0.003364168759128455689, 0.003467194976713144656, 0.003570221194297834057, 0.003776273629467117449, 0.004188378499805755356, 0.005012588240482921884, 0.005836797981160088411, 0.006661007721837254938, 0.007485217462514421466, 0.007588243680099037575, 0.007639756788891345629, 0.007691269897683653683, 0.007742783006475961738, 0.007794296115268268925, 0.007897322332852958759, 0.008309427203191686873, 0.008721532073530414986, 0.009133636943869143099 ),
 .UNSPECIFIED. ) ;
#48432 = CARTESIAN_POINT ( 'NONE',  ( 178.2670323550805449, 261.0171416467691756, 12.20401725416360250 ) ) ;
#48433 = ORIENTED_EDGE ( 'NONE', *, *, #9358, .F. ) ;
#48434 = CARTESIAN_POINT ( 'NONE',  ( 77.14493030857452993, 49.40685365668701934, -15.43250326293851415 ) ) ;
#48435 = ORIENTED_EDGE ( 'NONE', *, *, #67698, .F. ) ;
#48436 = CARTESIAN_POINT ( 'NONE',  ( 88.36122950843017065, 44.19684974305501157, -0.04416232360327642520 ) ) ;
#48438 = CARTESIAN_POINT ( 'NONE',  ( 155.6535436963908694, 261.0471492701456668, -17.87366571046205976 ) ) ;
#48437 = VECTOR ( 'NONE', #78073, 999.9999999999998863 ) ;
#48439 = ORIENTED_EDGE ( 'NONE', *, *, #49194, .T. ) ;
#48440 = CARTESIAN_POINT ( 'NONE',  ( 186.0992327883404300, 282.4869563496903311, -17.09887767567498074 ) ) ;
#48441 = CARTESIAN_POINT ( 'NONE',  ( 29.20513097723256024, 32.56454794089043503, 10.00000000000000355 ) ) ;
#48442 = CARTESIAN_POINT ( 'NONE',  ( 190.7010893771977464, 300.3430194703970528, 2.893802326194260033 ) ) ;
#48443 = CARTESIAN_POINT ( 'NONE',  ( 70.62434185772895034, 62.04354964908118575, -13.98456736824397062 ) ) ;
#48444 = CARTESIAN_POINT ( 'NONE',  ( 192.5143468344189728, 297.2023654272867361, -12.06830393602581530 ) ) ;
#48446 = EDGE_CURVE ( 'NONE', #50800, #69971, #81363, .T. ) ;
#48445 = CARTESIAN_POINT ( 'NONE',  ( 201.2139346379346705, 282.1342373466909521, -16.65315141107179286 ) ) ;
#48447 = CARTESIAN_POINT ( 'NONE',  ( 55.42424806449747621, 191.2592609112379876, 2.679491924311254714 ) ) ;
#48448 = CARTESIAN_POINT ( 'NONE',  ( 157.9540493922656879, 280.9862137877769328, 2.136681455221008274 ) ) ;
#48449 = CARTESIAN_POINT ( 'NONE',  ( 118.1982478153434357, 248.2369531367911293, -4.594050593750048428 ) ) ;
#48450 = ORIENTED_EDGE ( 'NONE', *, *, #49270, .T. ) ;
#48451 = CARTESIAN_POINT ( 'NONE',  ( 70.58921092982998857, 61.38955905053295936, -14.80681037022087132 ) ) ;
#48452 = B_SPLINE_CURVE_WITH_KNOTS ( 'NONE', 3,
 ( #89462, #3815, #10923, #3334 ),
 .UNSPECIFIED., .F., .F.,
 ( 4, 4 ),
 ( 0.02347114592376520203, 0.03270413735196970456 ),
 .UNSPECIFIED. ) ;
#48453 = CARTESIAN_POINT ( 'NONE',  ( 36.73494696561986217, 42.18502408145594984, 5.678558825948277544 ) ) ;
#48454 = ORIENTED_EDGE ( 'NONE', *, *, #16743, .F. ) ;
#48455 = AXIS2_PLACEMENT_3D ( 'NONE', #85959, #70174, #70683 ) ;
#48457 = VERTEX_POINT ( 'NONE', #41108 ) ;
#48456 = CARTESIAN_POINT ( 'NONE',  ( 83.61754957953866096, 52.24592005514148951, -14.70745080183156972 ) ) ;
#48458 = CARTESIAN_POINT ( 'NONE',  ( 203.5976937514409428, 276.3333535462982695, 13.44459927773758423 ) ) ;
#48459 = CARTESIAN_POINT ( 'NONE',  ( 177.6622601390721172, 253.8114938525349942, 1.357533546181270534 ) ) ;
#48460 = CARTESIAN_POINT ( 'NONE',  ( 171.4551282591434926, 287.9808904575950237, -4.629812407206613578 ) ) ;
#48461 = CARTESIAN_POINT ( 'NONE',  ( 192.7841353343293065, 296.7350780381442519, 12.22624134270118290 ) ) ;
#48462 = CARTESIAN_POINT ( 'NONE',  ( 73.01840184697886116, 65.54798808777084673, 12.82851028372286706 ) ) ;
#48463 = CARTESIAN_POINT ( 'NONE',  ( 200.9061540366740246, 282.6673289856585143, -18.13083321883407351 ) ) ;
#48464 = CARTESIAN_POINT ( 'NONE',  ( 173.9627241292350277, 288.0875699508326875, -10.01394112541635728 ) ) ;
#48465 = EDGE_CURVE ( 'NONE', #94679, #78204, #70014, .T. ) ;
#48466 = CARTESIAN_POINT ( 'NONE',  ( 173.7260703337255734, 281.2931294367136843, 14.01478156921193552 ) ) ;
#48467 = PLANE ( 'NONE',  #10925 ) ;
#48468 = VERTEX_POINT ( 'NONE', #31510 ) ;
#48469 = CARTESIAN_POINT ( 'NONE',  ( 194.9819925439454664, 292.9282776833073285, -15.33279721168237586 ) ) ;
#48470 = CARTESIAN_POINT ( 'NONE',  ( 152.8781682389868877, 273.7668382822124045, 12.04242711029878876 ) ) ;
#48471 = ORIENTED_EDGE ( 'NONE', *, *, #30619, .T. ) ;
#48473 = CARTESIAN_POINT ( 'NONE',  ( 164.0056900153536503, 278.2207161265373543, 13.42382243837776912 ) ) ;
#48472 = B_SPLINE_CURVE_WITH_KNOTS ( 'NONE', 3,
 ( #52606, #92176, #22726, #36915 ),
 .UNSPECIFIED., .F., .F.,
 ( 4, 4 ),
 ( 1.636534854170084423E-17, 0.0005839710162101579682 ),
 .UNSPECIFIED. ) ;
#48474 = CARTESIAN_POINT ( 'NONE',  ( 160.1198091476357206, 278.7610481921645942, 10.47921716862936670 ) ) ;
#48475 = CARTESIAN_POINT ( 'NONE',  ( 191.8691792395926825, 298.3198284809228085, -9.399504496626216010 ) ) ;
#48476 = CARTESIAN_POINT ( 'NONE',  ( 190.0445576990143195, 301.4801656937889902, 4.140328216824785912 ) ) ;
#48477 = CARTESIAN_POINT ( 'NONE',  ( 202.3425522658138505, 280.1794142728863903, 15.86053073629060961 ) ) ;
#48479 = CARTESIAN_POINT ( 'NONE',  ( 160.8888607722415998, 281.5892145363297914, 5.729030087643299574 ) ) ;
#48478 = CARTESIAN_POINT ( 'NONE',  ( 153.4232513496498598, 270.1086993216917449, 15.21047082690287588 ) ) ;
#48480 = CARTESIAN_POINT ( 'NONE',  ( 200.0474988174100872, 267.3471589286638164, 6.283709695813487706 ) ) ;
#48481 = VERTEX_POINT ( 'NONE', #62405 ) ;
#48482 = CARTESIAN_POINT ( 'NONE',  ( 164.2922989826749358, 280.8236579903888241, -11.68724490838191699 ) ) ;
#48483 = EDGE_CURVE ( 'NONE', #81472, #83009, #54291, .T. ) ;
#48484 = CARTESIAN_POINT ( 'NONE',  ( 164.1447795365461957, 247.4481183885314692, -7.445268063671048431 ) ) ;
#48485 = LINE ( 'NONE', #86045, #60937 ) ;
#48486 = CARTESIAN_POINT ( 'NONE',  ( 79.60625107924917643, 216.7677522451418497, 10.00000000000009592 ) ) ;
#48487 = CARTESIAN_POINT ( 'NONE',  ( 165.1645208897747352, 286.5721895103531551, -2.307774008256134657 ) ) ;
#48488 = CARTESIAN_POINT ( 'NONE',  ( 192.0332533962074706, 298.0356437054567778, 11.70630383928353346 ) ) ;
#48489 = CARTESIAN_POINT ( 'NONE',  ( 74.13497556468038852, 68.62018799133311120, 11.47049235834077408 ) ) ;
#48490 = EDGE_CURVE ( 'NONE', #34739, #28157, #17072, .T. ) ;
#48491 = CARTESIAN_POINT ( 'NONE',  ( 19.39999966495784989, 36.48715600906564305, 10.00000000000000000 ) ) ;
#48492 = DIRECTION ( 'NONE',  ( 0.4999999999999998890, -0.8660254037844385966, 0.000000000000000000 ) ) ;
#48493 = CARTESIAN_POINT ( 'NONE',  ( -2.124636079309504488, 160.3923013555410080, 4.594050593750050204 ) ) ;
#48494 = CARTESIAN_POINT ( 'NONE',  ( 88.91628449352961638, 212.9548013555409796, -4.594050593750042211 ) ) ;
#48495 = CARTESIAN_POINT ( 'NONE',  ( 154.8833801513861772, 262.3811116602312268, -17.49275566389638215 ) ) ;
#48496 = CARTESIAN_POINT ( 'NONE',  ( 146.9422184197532317, 276.1356072505412840, -5.063317562214876943 ) ) ;
#48497 = CARTESIAN_POINT ( 'NONE',  ( 7.330671393470725050, 16.18347333012629008, -9.594050593750004907 ) ) ;
#48498 = EDGE_CURVE ( 'NONE', #11106, #41237, #60823, .T. ) ;
#48499 = VECTOR ( 'NONE', #2242, 1000.000000000000000 ) ;
#48500 = EDGE_CURVE ( 'NONE', #95263, #24773, #11739, .T. ) ;
#48501 = AXIS2_PLACEMENT_3D ( 'NONE', #80064, #64322, #49615 ) ;
#48502 = CARTESIAN_POINT ( 'NONE',  ( 78.23645445329486847, 55.98478834354698819, 16.17353624429016534 ) ) ;
#48503 = CARTESIAN_POINT ( 'NONE',  ( 77.80179017151976950, 62.02139351241540766, 15.64422485472365487 ) ) ;
#48505 = CARTESIAN_POINT ( 'NONE',  ( 163.3473224498206093, 247.7211335670114352, -10.00320358166632850 ) ) ;
#48504 = CARTESIAN_POINT ( 'NONE',  ( 67.27848795683267724, 66.89052574399529760, 9.026760262957274961 ) ) ;
#48506 = EDGE_CURVE ( 'NONE', #24288, #17132, #95897, .T. ) ;
#48507 = CARTESIAN_POINT ( 'NONE',  ( 177.9544788665398869, 290.2550896080946359, 9.853009586926770424 ) ) ;
#48508 = EDGE_CURVE ( 'NONE', #89517, #22170, #77742, .T. ) ;
#48509 = CARTESIAN_POINT ( 'NONE',  ( 156.6168467568483891, 276.9391697405689001, 11.51099842983860633 ) ) ;
#48510 = CARTESIAN_POINT ( 'NONE',  ( -19.65312891409030271, 93.06504152958497400, -10.00000000000000888 ) ) ;
#48511 = LINE ( 'NONE', #7493, #99740 ) ;
#48512 = CARTESIAN_POINT ( 'NONE',  ( 207.8232941427535536, 270.6864908788566026, -6.505149060073906142 ) ) ;
#48513 = CARTESIAN_POINT ( 'NONE',  ( 73.43001404989733771, 69.84121715231802341, 9.192346335135486157 ) ) ;
#48514 = CIRCLE ( 'NONE', #21054, 17.82106496071138935 ) ;
#48515 = CARTESIAN_POINT ( 'NONE',  ( 44.12627281972940807, 196.2833772461660828, -9.188101187500095079 ) ) ;
#48516 = CARTESIAN_POINT ( 'NONE',  ( 175.2923730233647177, 264.8622459507627127, -16.64663378418118356 ) ) ;
#48517 = CARTESIAN_POINT ( 'NONE',  ( 73.65258675182887771, 204.1423013555409796, -4.594050593750043987 ) ) ;
#48518 = CYLINDRICAL_SURFACE ( 'NONE', #69261, 70.00000000000002842 ) ;
#48519 = CARTESIAN_POINT ( 'NONE',  ( 88.46984543095399545, 43.85297569260386297, 0.05479058522690674615 ) ) ;
#48520 = CARTESIAN_POINT ( 'NONE',  ( 166.0372674191381179, 259.3140289393645617, 15.65118634594625568 ) ) ;
#48522 = CARTESIAN_POINT ( 'NONE',  ( -22.42236680055709641, 157.8615022471902591, 0.000000000000000000 ) ) ;
#48521 = CARTESIAN_POINT ( 'NONE',  ( 197.6960670654980561, 286.6464179233946652, -17.55001329891280548 ) ) ;
#48523 = CARTESIAN_POINT ( 'NONE',  ( 176.7533145580467249, 270.1659372832907593, -17.11952259541214261 ) ) ;
#48524 = CARTESIAN_POINT ( 'NONE',  ( 26.34264212020660167, 36.18502408145594273, 5.678558825948276656 ) ) ;
#48525 = CARTESIAN_POINT ( 'NONE',  ( -105.0000000000000000, 0.000000000000000000, -14.21260523776211215 ) ) ;
#48526 = CARTESIAN_POINT ( 'NONE',  ( 80.80681612256114477, 47.51855870693373163, -12.98719063757217107 ) ) ;
#48527 = EDGE_LOOP ( 'NONE', ( #63980, #15669, #82737, #23238 ) ) ;
#48528 = CARTESIAN_POINT ( 'NONE',  ( 20.82171660429349203, 14.94754757982089366, 5.678558825948272215 ) ) ;
#48529 = CARTESIAN_POINT ( 'NONE',  ( 78.87554214658000262, 216.3458772461660544, 9.188101187500095079 ) ) ;
#48530 = DIRECTION ( 'NONE',  ( -0.06958655048002569676, 0.1205274409548614395, -0.9902680687415721383 ) ) ;
#48531 = CARTESIAN_POINT ( 'NONE',  ( 169.1442752176298256, 288.3456522438739285, -1.115561018949916328 ) ) ;
#48532 = CARTESIAN_POINT ( 'NONE',  ( 3.722289961109204626, 27.08330320443190331, -10.00000000000000000 ) ) ;
#48533 = CARTESIAN_POINT ( 'NONE',  ( 154.0399853174704958, 263.8419143634142756, 17.78904985960463847 ) ) ;
#48534 = LINE ( 'NONE', #25219, #81018 ) ;
#48535 = CARTESIAN_POINT ( 'NONE',  ( 123.8637576553643953, 228.9865022471901455, 1.119607411625061291E-15 ) ) ;
#48536 = CARTESIAN_POINT ( 'NONE',  ( 13.28313890609088865, 185.1427522451419350, -10.00000000000009592 ) ) ;
#48537 = CARTESIAN_POINT ( 'NONE',  ( 75.28764074951533303, 53.10663795412859400, 16.48602496812178941 ) ) ;
#48538 = ORIENTED_EDGE ( 'NONE', *, *, #73168, .T. ) ;
#48539 = CARTESIAN_POINT ( 'NONE',  ( 82.36618331495026268, 53.78214551141626742, 15.85029956610786783 ) ) ;
#48540 = ORIENTED_EDGE ( 'NONE', *, *, #54062, .T. ) ;
#48541 = CARTESIAN_POINT ( 'NONE',  ( 163.4260108471723640, 247.5848412648317662, 10.45113099391573108 ) ) ;
#48542 = CARTESIAN_POINT ( 'NONE',  ( 25.96864935082048831, 154.0458036431183189, 22.50000000000001421 ) ) ;
#48543 = CARTESIAN_POINT ( 'NONE',  ( 67.16135865072904210, 68.50708211668059278, -4.823428580958654344 ) ) ;
#48544 = ORIENTED_EDGE ( 'NONE', *, *, #457, .F. ) ;
#48545 = CARTESIAN_POINT ( 'NONE',  ( 173.3736115051062256, 251.7241798402721713, -0.2400946007419621497 ) ) ;
#48546 = ORIENTED_EDGE ( 'NONE', *, *, #8589, .F. ) ;
#48547 = CARTESIAN_POINT ( 'NONE',  ( 72.38244233070295763, 71.76593646792086645, 5.668245152086862859 ) ) ;
#48548 = CARTESIAN_POINT ( 'NONE',  ( 170.9648869844012893, 249.9305383690098097, 2.790804180076797092 ) ) ;
#48549 = CARTESIAN_POINT ( 'NONE',  ( 110.0000000000000000, 0.000000000000000000, -59.99999999999999289 ) ) ;
#48550 = ORIENTED_EDGE ( 'NONE', *, *, #17115, .T. ) ;
#48551 = ADVANCED_FACE ( 'NONE', ( #15694, #55678, #93752 ), #54682, .F. ) ;
#48552 = CARTESIAN_POINT ( 'NONE',  ( 29.87828763904599683, 19.11110640527293469, -2.839279412974138328 ) ) ;
#48553 = CARTESIAN_POINT ( 'NONE',  ( 75.00762831775020345, 66.90256318391985246, -13.19391308334217783 ) ) ;
#48554 = DIRECTION ( 'NONE',  ( -0.8660254037844378194, -0.5000000000000014433, -0.000000000000000000 ) ) ;
#48555 = ADVANCED_FACE ( 'NONE', ( #40492 ), #63805, .T. ) ;
#48556 = CARTESIAN_POINT ( 'NONE',  ( -19.65312891409030271, 93.06504152958497400, 59.99999999999999289 ) ) ;
#48557 = CARTESIAN_POINT ( 'NONE',  ( 76.30452923086889427, 224.8615022471903160, 5.000000000000046185 ) ) ;
#48558 = ORIENTED_EDGE ( 'NONE', *, *, #45383, .T. ) ;
#48559 = ORIENTED_EDGE ( 'NONE', *, *, #46075, .T. ) ;
#48560 = CARTESIAN_POINT ( 'NONE',  ( 183.2720146765236677, 295.8373939426455763, 1.008183942803973832 ) ) ;
#48562 = CARTESIAN_POINT ( 'NONE',  ( 148.3625667886952044, 273.6754917110858401, -8.960758510948144462 ) ) ;
#48561 = CARTESIAN_POINT ( 'NONE',  ( 163.2164407651493150, 283.9037165268248941, -2.742087382082966318 ) ) ;
#48563 = CARTESIAN_POINT ( 'NONE',  ( 163.3939361803663246, 247.6403962173759226, -10.78041711314006790 ) ) ;
#48564 = CARTESIAN_POINT ( 'NONE',  ( 193.7706395672514645, 295.0264025848412075, 15.16938698680137065 ) ) ;
#48565 = CARTESIAN_POINT ( 'NONE',  ( 186.9117901887487960, 293.6123360585760906, -10.79420932501841790 ) ) ;
#48566 = CARTESIAN_POINT ( 'NONE',  ( 204.6149525604204769, 276.2435015074934199, -13.22810747389629960 ) ) ;
#48568 = EDGE_CURVE ( 'NONE', #83607, #5345, #56189, .T. ) ;
#48567 = CARTESIAN_POINT ( 'NONE',  ( 164.7274214590310351, 245.3307319635834176, 4.681956269261704051 ) ) ;
#48569 = VECTOR ( 'NONE', #15505, 999.9999999999998863 ) ;
#48570 = DIRECTION ( 'NONE',  ( 0.5000000000000001110, -0.8660254037844384856, -0.000000000000000000 ) ) ;
#48571 = CARTESIAN_POINT ( 'NONE',  ( 73.07159975088246995, 72.16059528448882077, 0.000000000000000000 ) ) ;
#48572 = CARTESIAN_POINT ( 'NONE',  ( 79.22710464504368133, 225.7369531367911293, -4.594050593750048428 ) ) ;
#48573 = ORIENTED_EDGE ( 'NONE', *, *, #45048, .T. ) ;
#48574 = CARTESIAN_POINT ( 'NONE',  ( 190.9061255863007318, 299.9878863388391892, 7.497146773253707153 ) ) ;
#48575 = CARTESIAN_POINT ( 'NONE',  ( -12.95261720355844126, 24.63757726406876714, -10.00000000000000000 ) ) ;
#48576 = CARTESIAN_POINT ( 'NONE',  ( 77.91028351001615704, 61.39461664896379034, -16.15133184208620420 ) ) ;
#48577 = VERTEX_POINT ( 'NONE', #16704 ) ;
#48578 = CARTESIAN_POINT ( 'NONE',  ( 164.8309217477579409, 264.8793071284783878, -16.66214786874606446 ) ) ;
#48579 = VERTEX_POINT ( 'NONE', #47596 ) ;
#48580 = CARTESIAN_POINT ( 'NONE',  ( 80.32560484147226987, 44.93948968179056180, -11.21518412823304445 ) ) ;
#48581 = ADVANCED_FACE ( 'NONE', ( #509 ), #31397, .F. ) ;
#48582 = CARTESIAN_POINT ( 'NONE',  ( 146.5157004908022031, 276.8743579738231233, -0.1877253132609108255 ) ) ;
#48583 = CARTESIAN_POINT ( 'NONE',  ( 84.53427811226562483, 42.13127511552543325, -0.9647912365454934802 ) ) ;
#48584 = CARTESIAN_POINT ( 'NONE',  ( 81.01193622735327438, 48.21211403554050179, -13.36836587503643159 ) ) ;
#48585 = CARTESIAN_POINT ( 'NONE',  ( 162.7894281526998839, 248.6874348348773651, 10.21811719309735622 ) ) ;
#48586 = EDGE_CURVE ( 'NONE', #99538, #80312, #74165, .T. ) ;
#48587 = CARTESIAN_POINT ( 'NONE',  ( 103.3411068992554362, 218.2202760586659736, -5.415160957724236172E-17 ) ) ;
#48588 = ORIENTED_EDGE ( 'NONE', *, *, #14495, .F. ) ;
#48589 = VECTOR ( 'NONE', #47091, 1000.000000000000114 ) ;
#48590 = VERTEX_POINT ( 'NONE', #67670 ) ;
#48591 = CARTESIAN_POINT ( 'NONE',  ( 113.8142545287344802, 246.5177522451419065, 5.000000000000046185 ) ) ;
#48592 = B_SPLINE_SURFACE_WITH_KNOTS ( 'NONE', 3, 1, ( 
 ( #14487, #99589 ),
 ( #29194, #92030 ),
 ( #5394, #44864 ),
 ( #67177, #36774 ),
 ( #82927, #67682 ),
 ( #28183, #43377 ),
 ( #28680, #13503 ),
 ( #30173, #91025 ),
 ( #98101, #44372 ),
 ( #35787, #75804 ),
 ( #6388, #4904 ),
 ( #68171, #99098 ),
 ( #66682, #59055 ),
 ( #45366, #29682 ),
 ( #60555, #39244 ),
 ( #30681, #55447 ),
 ( #31650, #69165 ),
 ( #32669, #94511 ),
 ( #23550, #84413 ),
 ( #31156, #61561 ),
 ( #92508, #62045 ),
 ( #100096, #23054 ),
 ( #54443, #53952 ),
 ( #271, #84908 ),
 ( #24564, #86434 ),
 ( #76772, #62548 ),
 ( #8869, #39734 ),
 ( #15450, #8378 ),
 ( #93511, #7884 ),
 ( #24068, #85940 ),
 ( #46349, #85420 ),
 ( #15967, #77273 ),
 ( #9376, #92998 ),
 ( #46869, #16960 ) ),
 .UNSPECIFIED., .T., .F., .F.,
 ( 4, 2, 2, 2, 2, 2, 2, 2, 2, 2, 2, 2, 2, 2, 2, 2, 4 ),
 ( 2, 2 ),
 ( 0.000000000000000000, 0.06250000000000000000, 0.1250000000000000000, 0.1875000000000000000, 0.2500000000000000000, 0.3125000000000000000, 0.3750000000000000000, 0.4375000000000000000, 0.5000000000000000000, 0.5625000000000000000, 0.6250000000000000000, 0.6875000000000000000, 0.7500000000000000000, 0.8125000000000000000, 0.8750000000000000000, 0.9375000000000000000, 1.000000000000000000 ),
 ( 0.000000000000000000, 1.000000000000000000 ),
 .UNSPECIFIED. ) ;
#48593 = CARTESIAN_POINT ( 'NONE',  ( 208.1303168694798273, 270.1547119170880364, -0.9257663487928086132 ) ) ;
#48594 = EDGE_LOOP ( 'NONE', ( #72116, #64531, #72413, #57282 ) ) ;
#48595 = B_SPLINE_CURVE_WITH_KNOTS ( 'NONE', 3,
 ( #26882, #32967, #19308, #25898, #18293, #41563, #57263, #80625, #3593, #11201 ),
 .UNSPECIFIED., .F., .F.,
 ( 4, 2, 2, 2, 4 ),
 ( 0.3240010727220205000, 0.6620005363610115268, 0.7465004022707594222, 0.8310002681805074287, 1.000000000000000000 ),
 .UNSPECIFIED. ) ;
#48596 = B_SPLINE_CURVE_WITH_KNOTS ( 'NONE', 3,
 ( #18330, #64417, #2632, #42104, #11728, #4106, #65410, #10725, #41600, #11241, #26919, #82158, #42590, #56805, #58299, #41093, #74025, #72029, #80159, #57798, #64922, #87790, #72544, #3149, #95866, #65901, #88275, #96857, #27424, #66407, #18825, #58783, #50695, #57304, #81650, #49708, #19347, #50209, #4613, #20321, #67904, #21798, #44082, #12733, #45095, #60275 ),
 .UNSPECIFIED., .F., .F.,
 ( 4, 1, 2, 2, 1, 2, 2, 1, 1, 2, 2, 1, 1, 2, 2, 1, 1, 2, 2, 1, 1, 1, 2, 2, 1, 1, 1, 2, 2, 4 ),
 ( 0.000000000000000000, 0.06249999999999407418, 0.09374999999999257538, 0.1249999999999910905, 0.1874999999999910905, 0.2187499999999912015, 0.2499999999999912847, 0.3124999999999945599, 0.3437499999999963363, 0.3593749999999957256, 0.3749999999999951150, 0.4374999999999903966, 0.4687499999999894529, 0.4843749999999891198, 0.4999999999999887867, 0.5624999999999840128, 0.5937499999999800160, 0.6093749999999782396, 0.6249999999999763522, 0.6874999999999722444, 0.7187499999999702460, 0.7343749999999693578, 0.7421874999999686917, 0.7499999999999680256, 0.8124999999999780176, 0.8437499999999812372, 0.8593749999999812372, 0.8671874999999825695, 0.8749999999999840128, 1.000000000000000000 ),
 .UNSPECIFIED. ) ;
#48597 = CARTESIAN_POINT ( 'NONE',  ( -107.5954152546898257, 65.38554960527383741, -36.50000000000000000 ) ) ;
#48598 = CARTESIAN_POINT ( 'NONE',  ( 73.16146949562005375, 69.20639639887286876, -9.765445885128082537 ) ) ;
#48599 = CARTESIAN_POINT ( 'NONE',  ( -6.635445380951201955, 173.6427522451419065, 10.00000000000009237 ) ) ;
#48600 = CARTESIAN_POINT ( 'NONE',  ( 87.95873400847938228, 44.36334681983743877, 4.762736470890962082 ) ) ;
#48601 = VERTEX_POINT ( 'NONE', #50105 ) ;
#48602 = CARTESIAN_POINT ( 'NONE',  ( 157.2470923712064348, 258.2870420010311250, 16.90933983342926439 ) ) ;
#48603 = CARTESIAN_POINT ( 'NONE',  ( 158.9004676769321236, 274.8003366604523876, 12.92727430671328470 ) ) ;
#48604 = EDGE_CURVE ( 'NONE', #76243, #23143, #7376, .T. ) ;
#48605 = CARTESIAN_POINT ( 'NONE',  ( 159.6288139302610887, 254.1617792512662675, -15.32287760493869477 ) ) ;
#48606 = CARTESIAN_POINT ( 'NONE',  ( -28.04097607764120781, 24.82386083235215679, -10.00000000000000000 ) ) ;
#48607 = CARTESIAN_POINT ( 'NONE',  ( 174.9634400046559790, 284.2171181662870367, 13.92180131362537310 ) ) ;
#48608 = CARTESIAN_POINT ( 'NONE',  ( 198.9875272090999374, 285.4391185361790804, -17.09544516096110911 ) ) ;
#48609 = LINE ( 'NONE', #41481, #11438 ) ;
#48610 = ORIENTED_EDGE ( 'NONE', *, *, #28692, .F. ) ;
#48611 = CARTESIAN_POINT ( 'NONE',  ( 203.5838568433318301, 277.5370308791458456, -14.27138230751178050 ) ) ;
#48612 = EDGE_CURVE ( 'NONE', #24001, #86729, #27312, .T. ) ;
#48613 = CARTESIAN_POINT ( 'NONE',  ( 161.5504728662519369, 250.8333683393111926, 12.94300825113363373 ) ) ;
#48614 = CARTESIAN_POINT ( 'NONE',  ( 83.45685042842153223, 41.88942480781632582, 3.373892084012322989 ) ) ;
#48615 = CARTESIAN_POINT ( 'NONE',  ( 169.0039380441634478, 250.7158015086602347, 6.952515250780078482 ) ) ;
#48616 = CARTESIAN_POINT ( 'NONE',  ( 78.41424692880730163, 61.43889907920149795, 16.20108440401020999 ) ) ;
#48617 = CARTESIAN_POINT ( 'NONE',  ( 176.4148488556422762, 290.5001664222085651, -6.184015662434656946 ) ) ;
#48618 = CARTESIAN_POINT ( 'NONE',  ( -4.429217378738782962, 26.01694505731172313, 10.00000000000000000 ) ) ;
#48619 = EDGE_LOOP ( 'NONE', ( #5203, #8095, #47407, #21770 ) ) ;
#48620 = DIRECTION ( 'NONE',  ( -1.000000000000000000, 0.000000000000000000, 0.000000000000000000 ) ) ;
#48621 = EDGE_CURVE ( 'NONE', #36836, #17411, #15462, .T. ) ;
#48622 = ADVANCED_FACE ( 'NONE', ( #41491 ), #40978, .F. ) ;
#48623 = CARTESIAN_POINT ( 'NONE',  ( 164.5867587387928950, 245.5743669417666126, -3.022048486790635202 ) ) ;
#48625 = CARTESIAN_POINT ( 'NONE',  ( 74.25213553829982516, 55.44843064055443449, 16.12155446884580812 ) ) ;
#48624 = CARTESIAN_POINT ( 'NONE',  ( 180.6308739683319402, 266.9664207081152085, -14.83175007465150408 ) ) ;
#48626 = CARTESIAN_POINT ( 'NONE',  ( 79.98875348938439345, 57.15387458570124579, 16.58871383043193859 ) ) ;
#48627 = CARTESIAN_POINT ( 'NONE',  ( 36.02478613032081967, 22.92755873383628540, 6.180339887498953466 ) ) ;
#48628 = CARTESIAN_POINT ( 'NONE',  ( 189.3423859142968695, 300.6963629005612120, 0.4146017780601669589 ) ) ;
#48629 = CARTESIAN_POINT ( 'NONE',  ( 168.7143801906630358, 273.0201647186528362, 15.94736956477383139 ) ) ;
#48630 = DIRECTION ( 'NONE',  ( 0.3301025504114431519, 0.9439450758449140499, 0.000000000000000000 ) ) ;
#48632 = CARTESIAN_POINT ( 'NONE',  ( 50.40832357593285451, 87.79023373031367328, 10.00000000000000000 ) ) ;
#48631 = B_SPLINE_CURVE_WITH_KNOTS ( 'NONE', 3,
 ( #6996, #901, #92157, #1414, #99715, #77411, #55083, #62177, #76424, #32295, #39869, #8504 ),
 .UNSPECIFIED., .F., .F.,
 ( 4, 2, 2, 2, 2, 4 ),
 ( 0.000000000000000000, 0.0004508590478066377321, 0.0009017180956132754641, 0.001352577143419913088, 0.001578006667323285242, 0.001803436191226657397 ),
 .UNSPECIFIED. ) ;
#48633 = CARTESIAN_POINT ( 'NONE',  ( 188.2908577371792092, 260.7054629446816421, 3.471952975698951338 ) ) ;
#48634 = CARTESIAN_POINT ( 'NONE',  ( 161.4143265314674522, 251.0691807084224365, -12.94469757303959234 ) ) ;
#48635 = CARTESIAN_POINT ( 'NONE',  ( 0.4734401320438119676, 161.8923013555410080, 4.594050593750050204 ) ) ;
#48636 = FACE_OUTER_BOUND ( 'NONE', #46796, .T. ) ;
#48637 = ORIENTED_EDGE ( 'NONE', *, *, #50435, .T. ) ;
#48638 = CARTESIAN_POINT ( 'NONE',  ( 178.8556401556461140, 256.8010837051114663, 8.596802396966896964 ) ) ;
#48639 = CARTESIAN_POINT ( 'NONE',  ( -19.65312891409030271, 93.06504152958497400, 59.99999999999999289 ) ) ;
#48640 = CARTESIAN_POINT ( 'NONE',  ( -20.01211276271284945, 173.6868197944959036, 22.50000000000001421 ) ) ;
#48641 = CARTESIAN_POINT ( 'NONE',  ( 17.30628827445631401, 189.9869531367911293, 4.594050593750046652 ) ) ;
#48642 = CARTESIAN_POINT ( 'NONE',  ( 161.1990332043106946, 251.4420796895884394, 14.26998817770995487 ) ) ;
#48643 = LINE ( 'NONE', #86686, #3795 ) ;
#48644 = CARTESIAN_POINT ( 'NONE',  ( 36.13333420750807079, 36.56454794089044924, 10.00000000000000355 ) ) ;
#48645 = CARTESIAN_POINT ( 'NONE',  ( 181.4912298780635922, 293.8245865419322627, 6.251483007042555329 ) ) ;
#48646 = CARTESIAN_POINT ( 'NONE',  ( 173.6199058471797230, 272.8469020441871180, -16.35875967547425347 ) ) ;
#48647 = CARTESIAN_POINT ( 'NONE',  ( 149.7585222076137654, 271.2576260004179289, 12.47083832704270989 ) ) ;
#48648 = CARTESIAN_POINT ( 'NONE',  ( 81.69294868133339094, 55.63836673252024667, 15.97022168499915828 ) ) ;
#48649 = CARTESIAN_POINT ( 'NONE',  ( 11.84292332949202020, 15.03677371833800080, 10.00000000000000533 ) ) ;
#48650 = DIRECTION ( 'NONE',  ( -0.8450603975019799208, 0.5346708562974007428, 0.000000000000000000 ) ) ;
#48651 = PLANE ( 'NONE',  #40372 ) ;
#48652 = B_SPLINE_CURVE_WITH_KNOTS ( 'NONE', 3,
 ( #17593, #18099, #8010, #47484, #23672, #93121, #17084, #38882, #40868, #16090, #32784, #46995, #25185, #64191, #70281, #79440, #77909, #48502, #8497, #892, #78920, #70797, #1407, #32288, #63189, #93628, #24195, #94131, #47975, #71814, #2411, #33289, #71311, #63692, #94628, #34293, #4387, #27705, #80442, #88058, #34778, #27201, #65680, #26694, #97615, #57580 ),
 .UNSPECIFIED., .F., .F.,
 ( 4, 1, 2, 2, 1, 2, 2, 1, 1, 2, 2, 1, 1, 2, 2, 1, 1, 2, 2, 1, 1, 1, 2, 2, 1, 1, 1, 2, 2, 4 ),
 ( 0.000000000000000000, 0.06250000000000137390, 0.09375000000000205391, 0.1250000000000027478, 0.1875000000000019984, 0.2187500000000013878, 0.2500000000000007772, 0.3124999999999995559, 0.3437499999999978906, 0.3593749999999973910, 0.3749999999999968914, 0.4374999999999915623, 0.4687499999999882316, 0.4843749999999878431, 0.4999999999999874545, 0.5624999999999912292, 0.5937499999999941158, 0.6093749999999962252, 0.6249999999999983347, 0.6875000000000041078, 0.7187500000000061062, 0.7343750000000067724, 0.7421875000000062172, 0.7500000000000055511, 0.8125000000000018874, 0.8437500000000003331, 0.8593750000000000000, 0.8671874999999997780, 0.8749999999999994449, 1.000000000000000000 ),
 .UNSPECIFIED. ) ;
#48653 = VECTOR ( 'NONE', #10302, 1000.000000000000000 ) ;
#48654 = CARTESIAN_POINT ( 'NONE',  ( 85.75863988884901801, 226.9865022471902876, 10.00000000000009237 ) ) ;
#48655 = DIRECTION ( 'NONE',  ( -0.4827766168686586923, -0.5834231310750570554, -0.6531035050674809384 ) ) ;
#48656 = CARTESIAN_POINT ( 'NONE',  ( 203.4484836655096274, 270.1063680826336508, 6.027198966828741789 ) ) ;
#48657 = CARTESIAN_POINT ( 'NONE',  ( 51.05482314576993730, 188.0327760586659451, 1.948934522072303157E-15 ) ) ;
#48658 = CARTESIAN_POINT ( 'NONE',  ( 198.2819808855875863, 287.2125302111982705, 18.53535247371401695 ) ) ;
#48659 = EDGE_LOOP ( 'NONE', ( #58390, #40890, #18534 ) ) ;
#48660 = CARTESIAN_POINT ( 'NONE',  ( 162.8796071693688532, 263.4516756011302618, 17.10221866870684337 ) ) ;
#48661 = DIRECTION ( 'NONE',  ( -0.9820299053580079374, -0.1887253692075927247, 0.000000000000000000 ) ) ;
#48662 = DIRECTION ( 'NONE',  ( -0.8660254037844378194, -0.5000000000000014433, -0.000000000000000000 ) ) ;
#48663 = ORIENTED_EDGE ( 'NONE', *, *, #73450, .T. ) ;
#48664 = CARTESIAN_POINT ( 'NONE',  ( 82.63281508726200286, 40.94328431233920895, -3.617117793111280122 ) ) ;
#48665 = LINE ( 'NONE', #2570, #97614 ) ;
#48666 = CARTESIAN_POINT ( 'NONE',  ( -22.42236680055709641, 157.8615022471902591, 0.000000000000000000 ) ) ;
#48667 = B_SPLINE_CURVE_WITH_KNOTS ( 'NONE', 3,
 ( #93539, #93025, #77307, #23086, #61088, #15999, #100123, #84936, #6900, #92058, #38789, #99623, #1310, #83950, #69695, #53492 ),
 .UNSPECIFIED., .F., .F.,
 ( 4, 1, 2, 2, 2, 1, 2, 2, 4 ),
 ( 0.000000000000000000, 0.1249999999999935607, 0.1874999999999922839, 0.2499999999999910072, 0.4999999999999943379, 0.6249999999999965583, 0.6874999999999971134, 0.7499999999999976685, 1.000000000000000000 ),
 .UNSPECIFIED. ) ;
#48668 = DIRECTION ( 'NONE',  ( -0.3986482622784180974, -0.9171038997749370036, 0.000000000000000000 ) ) ;
#48669 = CARTESIAN_POINT ( 'NONE',  ( 26.18145187173165311, 30.51421378149920116, -9.188101187500004485 ) ) ;
#48670 = CARTESIAN_POINT ( 'NONE',  ( 163.2919429874875448, 247.8170536094679903, 9.876785378511263147 ) ) ;
#48671 = CARTESIAN_POINT ( 'NONE',  ( 196.4242782546697015, 290.4301655533025155, -16.42402868779123537 ) ) ;
#48672 = DIRECTION ( 'NONE',  ( -0.8660254037844378194, -0.5000000000000013323, -0.000000000000000000 ) ) ;
#48673 = ORIENTED_EDGE ( 'NONE', *, *, #47144, .T. ) ;
#48674 = CARTESIAN_POINT ( 'NONE',  ( 11.13306418284875576, 18.37878583063839244, 9.188101187500006262 ) ) ;
#48675 = LINE ( 'NONE', #18275, #20567 ) ;
#48676 = CARTESIAN_POINT ( 'NONE',  ( 23.90999230191042102, 174.6115022471901739, -5.000000000000041744 ) ) ;
#48677 = DIRECTION ( 'NONE',  ( -0.2588190451024967587, -0.9659258262890746405, 0.000000000000000000 ) ) ;
#48678 = ORIENTED_EDGE ( 'NONE', *, *, #30491, .F. ) ;
#48679 = CARTESIAN_POINT ( 'NONE',  ( 72.20607312672656519, 71.10925155450907198, -5.972286613955676948 ) ) ;
#48680 = CARTESIAN_POINT ( 'NONE',  ( 190.7851866479434761, 300.1973587246873194, 7.931162401707728016 ) ) ;
#48681 = CARTESIAN_POINT ( 'NONE',  ( 177.9642817169934688, 254.8723555480702601, -7.199370876740468717 ) ) ;
#48682 = CARTESIAN_POINT ( 'NONE',  ( 190.0601721553029222, 300.2863949309033842, 3.228815124723532382 ) ) ;
#48683 = ORIENTED_EDGE ( 'NONE', *, *, #1707, .F. ) ;
#48684 = ORIENTED_EDGE ( 'NONE', *, *, #46220, .T. ) ;
#48686 = DIRECTION ( 'NONE',  ( -0.9922852870422786964, 0.1239754375649568807, 0.000000000000000000 ) ) ;
#48685 = CARTESIAN_POINT ( 'NONE',  ( 69.36140278139266968, 71.17324983025980600, 0.8027048792421369594 ) ) ;
#48687 = ORIENTED_EDGE ( 'NONE', *, *, #99963, .T. ) ;
#48688 = CARTESIAN_POINT ( 'NONE',  ( 153.1983976505312626, 265.2995869615763809, -17.69657798691567763 ) ) ;
#48689 = CARTESIAN_POINT ( 'NONE',  ( 170.4745685060332221, 252.4510253584002442, 10.32956013645375570 ) ) ;
#48690 = CARTESIAN_POINT ( 'NONE',  ( 72.63904040253795813, 57.48289066996441932, -16.31294606514927636 ) ) ;
#48691 = CARTESIAN_POINT ( 'NONE',  ( 77.16076033720362659, 63.58031483167507503, 15.43380074518343825 ) ) ;
#48692 = CARTESIAN_POINT ( 'NONE',  ( 72.21491844529387549, 53.64441083166271085, 0.000000000000000000 ) ) ;
#48694 = ADVANCED_FACE ( 'NONE', ( #11130 ), #95262, .T. ) ;
#48693 = CARTESIAN_POINT ( 'NONE',  ( 88.83448719433606300, 234.3464784336661637, 1.353441290958777525E-15 ) ) ;
#48695 = CARTESIAN_POINT ( 'NONE',  ( 200.4958402305064737, 266.0993451409080421, 1.904533336957719536 ) ) ;
#48696 = ORIENTED_EDGE ( 'NONE', *, *, #97601, .T. ) ;
#48697 = CARTESIAN_POINT ( 'NONE',  ( 208.3135187673106543, 269.8373969220020285, 2.829653198597726682 ) ) ;
#48698 = ORIENTED_EDGE ( 'NONE', *, *, #32566, .F. ) ;
#48699 = CARTESIAN_POINT ( 'NONE',  ( 33.57875857642567752, 25.10170272979928896, -7.433330006724141015 ) ) ;
#48700 = CARTESIAN_POINT ( 'NONE',  ( 198.1300353965528984, 287.4757075181870505, 18.48278456664528946 ) ) ;
#48701 = CARTESIAN_POINT ( 'NONE',  ( 78.24399414866135771, 47.91685926408410268, -14.02064381479976340 ) ) ;
#48702 = CARTESIAN_POINT ( 'NONE',  ( 59.20026718252854891, 214.1744531367911293, 4.594050593750047540 ) ) ;
#48703 = EDGE_CURVE ( 'NONE', #19180, #57417, #56704, .T. ) ;
#48704 = CARTESIAN_POINT ( 'NONE',  ( 74.07459009150333884, 68.62600853808264389, 11.43350474783684767 ) ) ;
#48705 = CARTESIAN_POINT ( 'NONE',  ( 151.3560786774222322, 268.4905770267490652, 15.54402364351346932 ) ) ;
#48706 = CARTESIAN_POINT ( 'NONE',  ( 182.4179874479192165, 295.3930394561857042, 6.267308984944027550 ) ) ;
#48707 = CARTESIAN_POINT ( 'NONE',  ( 173.0033714575370425, 271.2342936761517649, 16.42547438483588351 ) ) ;
#48708 = EDGE_CURVE ( 'NONE', #22737, #61085, #19725, .T. ) ;
#48709 = CARTESIAN_POINT ( 'NONE',  ( 87.79538347886169447, 45.10662587206184071, 6.725936807544243834 ) ) ;
#48710 = ORIENTED_EDGE ( 'NONE', *, *, #24538, .T. ) ;
#48711 =( BOUNDED_CURVE ( )  B_SPLINE_CURVE ( 2, ( #845, #24642, #94585, #2370, #32245, #48959, #18062, #62628, #93584, #8949, #10458, #2879, #41334 ),
 .UNSPECIFIED., .F., .T. ) 
 B_SPLINE_CURVE_WITH_KNOTS ( ( 3, 2, 2, 2, 2, 2, 3 ),
 ( 0.5125000000000000666, 0.5150000000000000133, 0.5200000000000000178, 0.5250000000000000222, 0.5300000000000000266, 0.5350000000000000311, 0.5375000000000000888 ),
 .UNSPECIFIED. ) 
 CURVE ( )  GEOMETRIC_REPRESENTATION_ITEM ( )  RATIONAL_B_SPLINE_CURVE ( ( 0.9755282581475767101, 0.9755282581475772652, 1.000000000000000000, 0.9510565162951535312, 1.000000000000000000, 0.9510565162951535312, 1.000000000000000000, 0.9510565162951535312, 1.000000000000000000, 0.9510565162951535312, 1.000000000000000000, 0.9755282581475761550, 0.9755282581475767101 ) ) 
 REPRESENTATION_ITEM ( '' )  );
#48712 = CARTESIAN_POINT ( 'NONE',  ( 74.46650544198260491, 58.60527373928128725, -15.83729253052527319 ) ) ;
#48713 = CARTESIAN_POINT ( 'NONE',  ( 178.0374733479650615, 288.7981423944819994, 10.93213786509874907 ) ) ;
#48714 = CARTESIAN_POINT ( 'NONE',  ( 78.65816961274913410, 57.55682543410598839, 16.60711249658122668 ) ) ;
#48715 = EDGE_LOOP ( 'NONE', ( #30871, #30567, #46562, #29530 ) ) ;
#48716 = CARTESIAN_POINT ( 'NONE',  ( 172.1715872173708135, 258.5563651535738927, -14.06291902901496371 ) ) ;
#48717 = CARTESIAN_POINT ( 'NONE',  ( 173.8466962506738867, 278.0501108023409529, -16.19608603001420732 ) ) ;
#48718 = CARTESIAN_POINT ( 'NONE',  ( 207.2337123599961899, 271.7076764818092443, -5.443417788256701861 ) ) ;
#48719 = CARTESIAN_POINT ( 'NONE',  ( 206.4767859350078254, 270.5991797036530784, 2.338462165877995158 ) ) ;
#48721 = CARTESIAN_POINT ( 'NONE',  ( 190.3572031550745294, 300.9386478791372497, 3.093832330100951378 ) ) ;
#48720 = B_SPLINE_CURVE_WITH_KNOTS ( 'NONE', 3,
 ( #63266, #971, #16663, #47558, #9073, #70877, #71387, #1483, #32366, #94206, #16167, #62244, #40941, #71887, #24761, #32861, #40451, #55640, #2484, #25262, #17675, #86626, #47065, #33366, #23750, #48576, #25786, #77980, #17160, #56663, #87647 ),
 .UNSPECIFIED., .F., .F.,
 ( 4, 3, 3, 3, 3, 3, 3, 3, 3, 3, 4 ),
 ( 0.000000000000000000, 0.1333490885032390105, 0.3007194338854328186, 0.4699862290245252483, 0.5844252810809424936, 0.6686540514502805621, 0.7354980260655528124, 0.8028463152565618044, 0.8633854507757205976, 0.9437142632667329112, 1.000000000000000000 ),
 .UNSPECIFIED. ) ;
#48722 = CARTESIAN_POINT ( 'NONE',  ( 180.9066661141190764, 271.3944185450963573, 16.82689088922535348 ) ) ;
#48723 = CARTESIAN_POINT ( 'NONE',  ( 164.8849641302980444, 245.0578600525887794, 2.884140591399200648 ) ) ;
#48724 = CARTESIAN_POINT ( 'NONE',  ( 67.40908756201770302, 66.96761179404961695, 9.024507661442916273 ) ) ;
#48725 = CARTESIAN_POINT ( 'NONE',  ( 164.7391251265351571, 254.6380307246101040, 14.05658276553760722 ) ) ;
#48726 = DIRECTION ( 'NONE',  ( 0.4999999999999998890, -0.8660254037844385966, 0.000000000000000000 ) ) ;
#48727 = CARTESIAN_POINT ( 'NONE',  ( 112.7044859340271472, 242.0024278399160949, 9.188101187500095079 ) ) ;
#48728 = ORIENTED_EDGE ( 'NONE', *, *, #16187, .F. ) ;
#48729 = CARTESIAN_POINT ( 'NONE',  ( 149.0000156265528517, 272.5713979366907438, -11.96939414408693025 ) ) ;
#48730 = CARTESIAN_POINT ( 'NONE',  ( 84.28294931125054745, 42.37490528802118206, 3.413621673734357209 ) ) ;
#48731 = CARTESIAN_POINT ( 'NONE',  ( 155.0619429961492983, 262.0718317407570339, -17.08853361476647592 ) ) ;
#48732 = CARTESIAN_POINT ( 'NONE',  ( 183.2273280905530441, 284.5979244485508843, -14.99588714064362094 ) ) ;
#48733 = CARTESIAN_POINT ( 'NONE',  ( 83.77043784194415821, 51.50489687730897259, -14.36765084287526406 ) ) ;
#48734 = AXIS2_PLACEMENT_3D ( 'NONE', #52490, #61581, #31180 ) ;
#48735 = CARTESIAN_POINT ( 'NONE',  ( 176.9774428127479950, 254.7512675880996369, 4.897130350530210841 ) ) ;
#48736 = VERTEX_POINT ( 'NONE', #48618 ) ;
#48737 = CARTESIAN_POINT ( 'NONE',  ( 80.41065583177754661, 57.49148768039361812, -16.58946210043120217 ) ) ;
#48738 = EDGE_CURVE ( 'NONE', #61424, #37421, #89178, .T. ) ;
#48739 = CARTESIAN_POINT ( 'NONE',  ( 154.8737640171889609, 273.3615094271205521, -13.02948580469064943 ) ) ;
#48741 = LINE ( 'NONE', #79171, #100133 ) ;
#48740 = CARTESIAN_POINT ( 'NONE',  ( 72.99786219007800980, 70.75108751906873295, 8.232086053012798388 ) ) ;
#48742 = CARTESIAN_POINT ( 'NONE',  ( 205.9736828131439097, 273.8901116759951719, -10.08879389214638778 ) ) ;
#48743 = CARTESIAN_POINT ( 'NONE',  ( 143.0428722300570143, 244.2048013555409511, 4.594050593750051981 ) ) ;
#48744 = CARTESIAN_POINT ( 'NONE',  ( 192.3947792546893254, 295.6933971515595090, -12.11733834305915103 ) ) ;
#48745 = CARTESIAN_POINT ( 'NONE',  ( 185.6688052473205630, 297.0996414484710044, 4.161359448325653965 ) ) ;
#48746 = EDGE_CURVE ( 'NONE', #36428, #90703, #73418, .T. ) ;
#48747 = CARTESIAN_POINT ( 'NONE',  ( 83.90596095485256001, 41.21795184261720379, -1.108148245180562033E-06 ) ) ;
#48748 = CARTESIAN_POINT ( 'NONE',  ( 58.87550765610937731, 213.9869531367911009, 4.594050593750046652 ) ) ;
#48749 = CARTESIAN_POINT ( 'NONE',  ( 72.82155047740585019, 61.75947611529039705, -15.18569844785497480 ) ) ;
#48750 = CARTESIAN_POINT ( 'NONE',  ( 171.1295603993285965, 249.6517061031812545, 4.344809613321301889 ) ) ;
#48751 = ADVANCED_FACE ( 'NONE', ( #80049 ), #26282, .F. ) ;
#48752 = SURFACE_STYLE_FILL_AREA ( #79181 ) ;
#48753 = CARTESIAN_POINT ( 'NONE',  ( 171.1201963583744146, 259.8845004021682712, 14.96928189076699844 ) ) ;
#48754 = CARTESIAN_POINT ( 'NONE',  ( 152.3741921479031589, 278.3847345969097660, -1.620820812214976758 ) ) ;
#48755 = DIRECTION ( 'NONE',  ( 0.000000000000000000, 0.000000000000000000, 1.000000000000000000 ) ) ;
#48756 = CARTESIAN_POINT ( 'NONE',  ( 155.5322964227545413, 261.2571557083629159, -18.35853982030605280 ) ) ;
#48757 = PLANE ( 'NONE',  #28900 ) ;
#48758 = CARTESIAN_POINT ( 'NONE',  ( 126.3716228836088646, 243.7677522451418497, 10.00000000000009592 ) ) ;
#48759 = CARTESIAN_POINT ( 'NONE',  ( 80.20189741304909603, 52.03696804570480339, -15.25587582201593229 ) ) ;
#48760 = ORIENTED_EDGE ( 'NONE', *, *, #56597, .T. ) ;
#48761 = CARTESIAN_POINT ( 'NONE',  ( 190.1063449786324213, 301.3731469862293011, 0.2163967485516588019 ) ) ;
#48762 = CARTESIAN_POINT ( 'NONE',  ( 87.83617351001007023, 44.77714871921288875, 4.967881908888847953 ) ) ;
#48763 = CARTESIAN_POINT ( 'NONE',  ( 48.29419362332453858, 192.5643266524160140, 9.188101187500095079 ) ) ;
#48764 = CARTESIAN_POINT ( 'NONE',  ( 15.16022976130349065, 27.49103043416548431, -8.090169943749479842 ) ) ;
#48765 = CARTESIAN_POINT ( 'NONE',  ( 44.73065482718367747, 120.5373619841236774, -10.00000000000000000 ) ) ;
#48766 = CARTESIAN_POINT ( 'NONE',  ( 77.96183350652215438, 50.52624373792482970, -15.65746755701282211 ) ) ;
#48767 = CARTESIAN_POINT ( 'NONE',  ( 147.5177358149801421, 275.1387818813681179, 4.867883209065928085 ) ) ;
#48768 = CARTESIAN_POINT ( 'NONE',  ( 72.02410375280403798, 72.02863993979345025, 2.848237292894958639 ) ) ;
#48770 = CARTESIAN_POINT ( 'NONE',  ( 58.82164138842265544, 204.7677522451418781, 10.00000000000009592 ) ) ;
#48769 = CARTESIAN_POINT ( 'NONE',  ( 198.1468175574237591, 277.6623963789502909, -16.51117061083609983 ) ) ;
#48771 = CARTESIAN_POINT ( 'NONE',  ( -4.429217378738782962, 26.01694505731172313, -10.00000000000000000 ) ) ;
#48772 = CARTESIAN_POINT ( 'NONE',  ( 180.9078741482798307, 256.3374541303720662, 1.332084592654648070 ) ) ;
#48773 = CARTESIAN_POINT ( 'NONE',  ( 205.3943609285979051, 274.8935266139653777, -13.14270440534009943 ) ) ;
#48774 = CARTESIAN_POINT ( 'NONE',  ( -19.65312891409030271, 93.06504152958497400, 177.5919119679930134 ) ) ;
#48775 = EDGE_LOOP ( 'NONE', ( #40969, #42429, #69647, #2986 ) ) ;
#48776 = EDGE_CURVE ( 'NONE', #43534, #75541, #7552, .T. ) ;
#48777 = CARTESIAN_POINT ( 'NONE',  ( 38.27158024800235836, 186.2365022471901739, -10.00000000000009059 ) ) ;
#48778 = CARTESIAN_POINT ( 'NONE',  ( 184.8129517241381734, 294.4172780608702737, 9.971149335153635107 ) ) ;
#48779 = CARTESIAN_POINT ( 'NONE',  ( 163.0683798854284703, 248.2042762609320903, 11.26611642476872710 ) ) ;
#48780 = CARTESIAN_POINT ( 'NONE',  ( 9.864316330390064280, 170.3768266524160140, -9.188101187500091527 ) ) ;
#48781 = CARTESIAN_POINT ( 'NONE',  ( 29.25887229277395463, 38.93396525600392266, 2.839279412974139660 ) ) ;
#48784 = ADVANCED_FACE ( 'NONE', ( #30670 ), #61550, .F. ) ;
#48783 = CARTESIAN_POINT ( 'NONE',  ( 47.54560441532652959, 78.55524412553474178, -10.00000000000000000 ) ) ;
#48782 = LINE ( 'NONE', #10780, #94566 ) ;
#48785 = CARTESIAN_POINT ( 'NONE',  ( 192.6773196027083372, 296.9200883123592689, 11.15745042875121484 ) ) ;
#48786 = CARTESIAN_POINT ( 'NONE',  ( 29.97031301328857467, 32.70171378149920827, -9.188101187500004485 ) ) ;
#48787 = CARTESIAN_POINT ( 'NONE',  ( 155.6179570493757183, 261.5041650582481338, -17.00304691045595362 ) ) ;
#48788 = DIRECTION ( 'NONE',  ( 0.000000000000000000, 0.000000000000000000, 1.000000000000000000 ) ) ;
#48789 = CARTESIAN_POINT ( 'NONE',  ( -22.20871200244593169, 23.11170711957623070, 177.5919119679930134 ) ) ;
#48790 = ORIENTED_EDGE ( 'NONE', *, *, #45472, .F. ) ;
#48791 = CARTESIAN_POINT ( 'NONE',  ( 75.43850382708453139, 204.3615022471901739, 5.000000000000051514 ) ) ;
#48792 = CARTESIAN_POINT ( 'NONE',  ( 88.40853095561152486, 233.3967562850347122, -4.648177544792955347E-16 ) ) ;
#48793 = CARTESIAN_POINT ( 'NONE',  ( 6.244247187202517146, 25.64646525600388216, -2.839279412974133887 ) ) ;
#48794 = CARTESIAN_POINT ( 'NONE',  ( 168.4882224088831890, 287.4185086114543424, 0.5096248658197195525 ) ) ;
#48795 = CARTESIAN_POINT ( 'NONE',  ( 14.92192532440567199, 20.56628583063839955, 9.188101187500006262 ) ) ;
#48796 = CYLINDRICAL_SURFACE ( 'NONE', #23051, 70.00000000000002842 ) ;
#48797 = CARTESIAN_POINT ( 'NONE',  ( 152.8006295377938386, 275.0191557585933424, 10.80676033415724646 ) ) ;
#48798 = CARTESIAN_POINT ( 'NONE',  ( 87.90399932408934092, 44.03024641107109005, -1.767293127319844670 ) ) ;
#48799 = ORIENTED_EDGE ( 'NONE', *, *, #4660, .T. ) ;
#48800 = CARTESIAN_POINT ( 'NONE',  ( 26.78025984663613812, 31.16454794089042579, -10.00000000000000355 ) ) ;
#48801 = CARTESIAN_POINT ( 'NONE',  ( 207.6900289502458179, 270.9173129631602706, 7.178327969100043227 ) ) ;
#48802 = CARTESIAN_POINT ( 'NONE',  ( 102.3574601280508176, 223.2365022471902023, 10.00000000000009948 ) ) ;
#48803 = CARTESIAN_POINT ( 'NONE',  ( 87.45543461181301836, 45.01664465679169780, 6.930016242323781661 ) ) ;
#48804 = VECTOR ( 'NONE', #87978, 1000.000000000000000 ) ;
#48805 = CARTESIAN_POINT ( 'NONE',  ( 155.0303156110108489, 262.1266119787277944, 17.11986653161320859 ) ) ;
#48806 = ORIENTED_EDGE ( 'NONE', *, *, #44451, .F. ) ;
#48807 = ORIENTED_EDGE ( 'NONE', *, *, #71091, .T. ) ;
#48808 = CARTESIAN_POINT ( 'NONE',  ( 198.2505066714982149, 285.2670451491296149, 0.000000000000000000 ) ) ;
#48809 = CARTESIAN_POINT ( 'NONE',  ( 86.72009611066519597, 47.05274629621921889, 10.38319007345879541 ) ) ;
#48810 = VERTEX_POINT ( 'NONE', #15438 ) ;
#48811 = CARTESIAN_POINT ( 'NONE',  ( 192.7874605187217014, 292.5376213369709149, 15.36506066506490598 ) ) ;
#48812 = CARTESIAN_POINT ( 'NONE',  ( 155.3625719195318027, 262.1439356272904888, -17.05869219998719899 ) ) ;
#48813 = ORIENTED_EDGE ( 'NONE', *, *, #95752, .F. ) ;
#48814 = CARTESIAN_POINT ( 'NONE',  ( 78.38473537823422532, 61.45169569177851088, -15.84070094600075684 ) ) ;
#48815 = CARTESIAN_POINT ( 'NONE',  ( 85.19897760540997922, 48.35682075688382042, -11.91179608430785208 ) ) ;
#48816 = CARTESIAN_POINT ( 'NONE',  ( 77.38344707992527560, 49.10671604805792612, -15.27628165681131200 ) ) ;
#48817 = CARTESIAN_POINT ( 'NONE',  ( -23.73952538801239598, 24.43184193311135743, -10.00000000000000000 ) ) ;
#48818 = ORIENTED_EDGE ( 'NONE', *, *, #60201, .F. ) ;
#48819 = CARTESIAN_POINT ( 'NONE',  ( 200.8769374536528858, 282.7179335918746688, 17.26928237494566787 ) ) ;
#48820 = CARTESIAN_POINT ( 'NONE',  ( 169.0831179322903495, 276.3545926343148267, -16.16093963830661551 ) ) ;
#48821 = CARTESIAN_POINT ( 'NONE',  ( 111.7912168577913974, 246.8967562850347122, -4.648177544792955347E-16 ) ) ;
#48822 = CARTESIAN_POINT ( 'NONE',  ( 40.07751882555258049, 24.10801979619931501, 3.090169943749476733 ) ) ;
#48823 = ORIENTED_EDGE ( 'NONE', *, *, #52628, .T. ) ;
#48824 = CARTESIAN_POINT ( 'NONE',  ( 171.8094870316595291, 256.2585101260063993, -11.60869940165414427 ) ) ;
#48825 = CARTESIAN_POINT ( 'NONE',  ( 33.16502987395432456, 42.08080186712595605, -3.090169943749475845 ) ) ;
#48826 = EDGE_LOOP ( 'NONE', ( #24024, #12661, #31005, #62111 ) ) ;
#48827 = EDGE_CURVE ( 'NONE', #329, #7306, #46337, .T. ) ;
#48828 = ORIENTED_EDGE ( 'NONE', *, *, #76516, .F. ) ;
#48829 = CARTESIAN_POINT ( 'NONE',  ( 160.2388368888874197, 268.7474976419025552, -16.58833657477884671 ) ) ;
#48830 = VERTEX_POINT ( 'NONE', #7870 ) ;
#48831 = ADVANCED_FACE ( 'NONE', ( #62033 ), #57635, .F. ) ;
#48832 = CARTESIAN_POINT ( 'NONE',  ( 67.71970704014216835, 67.69221244699392059, 7.277574328431961170 ) ) ;
#48833 = VERTEX_POINT ( 'NONE', #44852 ) ;
#48834 = EDGE_CURVE ( 'NONE', #54113, #79361, #47837, .T. ) ;
#48835 = CARTESIAN_POINT ( 'NONE',  ( 194.0772601196179039, 294.4953202094977769, 14.03104165446852214 ) ) ;
#48836 = CARTESIAN_POINT ( 'NONE',  ( 190.8422792407884003, 275.9516057710682162, 17.28259784732214399 ) ) ;
#48837 = CARTESIAN_POINT ( 'NONE',  ( 71.17403661793173342, 68.90151599838424090, 8.574984275677001833 ) ) ;
#48838 = EDGE_CURVE ( 'NONE', #16838, #35245, #6678, .T. ) ;
#48839 = CARTESIAN_POINT ( 'NONE',  ( -42.72532191160158987, 28.29708160126036987, 10.00000000000000000 ) ) ;
#48840 = CARTESIAN_POINT ( 'NONE',  ( 82.41797270617800564, 53.48512899883142779, -15.75897339677477937 ) ) ;
#48841 = LINE ( 'NONE', #63521, #98210 ) ;
#48842 = VERTEX_POINT ( 'NONE', #33675 ) ;
#48843 = CARTESIAN_POINT ( 'NONE',  ( 185.4203654054929871, 257.3861754496879257, 1.843076797948306034 ) ) ;
#48844 = CARTESIAN_POINT ( 'NONE',  ( 24.68213521633936836, 16.11110640527292759, -2.839279412974138328 ) ) ;
#48845 = CARTESIAN_POINT ( 'NONE',  ( 164.4261001824251878, 245.8526357240660900, 1.583002802772015549 ) ) ;
#48846 = DIRECTION ( 'NONE',  ( 0.000000000000000000, 0.000000000000000000, 1.000000000000000000 ) ) ;
#48848 = ORIENTED_EDGE ( 'NONE', *, *, #68274, .F. ) ;
#48847 = CARTESIAN_POINT ( 'NONE',  ( 197.8822014719394531, 287.9049684674569676, 17.88172308374019792 ) ) ;
#48849 = VERTEX_POINT ( 'NONE', #2282 ) ;
#48850 = CARTESIAN_POINT ( 'NONE',  ( 171.4323342072972025, 259.3649984363102021, -13.88167851551672349 ) ) ;
#48851 = CARTESIAN_POINT ( 'NONE',  ( 36.03373902044236132, 43.73705186507757503, -3.090169943749475845 ) ) ;
#48852 = DIRECTION ( 'NONE',  ( -0.9956898167541080591, 0.09274582908234035861, 0.000000000000000000 ) ) ;
#48853 = B_SPLINE_CURVE_WITH_KNOTS ( 'NONE', 3,
 ( #30814, #13135, #37397, #6012, #90669, #36905, #91643, #43993, #99726, #74935, #22210, #84064, #37890, #100228, #29320, #68798, #61694, #91148, #30312, #61198, #14618, #83553, #14118, #5518, #75944, #6521, #68302, #99225, #45497, #92646, #23195, #7003, #92166, #22717, #53596, #85041, #9528, #32805, #85565, #93139, #39880, #32305, #70816, #31789, #2430, #62691 ),
 .UNSPECIFIED., .F., .F.,
 ( 4, 1, 1, 1, 2, 2, 1, 1, 1, 2, 2, 1, 1, 2, 2, 1, 1, 2, 2, 1, 1, 2, 2, 1, 2, 2, 1, 2, 2, 4 ),
 ( 0.000000000000000000, 0.06249999999998029354, 0.09374999999997235545, 0.1093749999999686084, 0.1171874999999683725, 0.1249999999999681366, 0.1874999999999587830, 0.2187499999999538425, 0.2343749999999514277, 0.2421874999999502343, 0.2499999999999490408, 0.3124999999999495404, 0.3437499999999494849, 0.3593749999999494293, 0.3749999999999493183, 0.4374999999999565903, 0.4687499999999620304, 0.4843749999999648059, 0.4999999999999675815, 0.5624999999999735767, 0.5937499999999764633, 0.6093749999999774625, 0.6249999999999785727, 0.6874999999999792388, 0.7187499999999815703, 0.7499999999999837907, 0.8124999999999882316, 0.8437499999999902300, 0.8749999999999921174, 1.000000000000000000 ),
 .UNSPECIFIED. ) ;
#48854 = CARTESIAN_POINT ( 'NONE',  ( 161.7587802986029999, 250.4725692828850754, 14.33336164792646450 ) ) ;
#48855 = CARTESIAN_POINT ( 'NONE',  ( 103.9969882237314351, 242.3967562850347122, -4.648177544792955347E-16 ) ) ;
#48856 = ORIENTED_EDGE ( 'NONE', *, *, #22761, .F. ) ;
#48857 = LINE ( 'NONE', #56435, #36488 ) ;
#48858 = CARTESIAN_POINT ( 'NONE',  ( 5.294102074706517058, 26.55466486950697558, -1.111400068045478839E-16 ) ) ;
#48859 = EDGE_CURVE ( 'NONE', #32616, #73603, #40240, .T. ) ;
#48860 = CARTESIAN_POINT ( 'NONE',  ( 52.03546399666511491, 212.3967562850347122, -4.648177544792955347E-16 ) ) ;
#48861 = CARTESIAN_POINT ( 'NONE',  ( -1.617403181491035902, 158.3262482093458061, 3.021315404115420679E-15 ) ) ;
#48862 = CARTESIAN_POINT ( 'NONE',  ( 21.14953632379956616, 183.0177522451418497, -10.00000000000009592 ) ) ;
#48863 = CARTESIAN_POINT ( 'NONE',  ( 100.4447270377624477, 237.9869531367911293, 4.594050593750046652 ) ) ;
#48864 = CARTESIAN_POINT ( 'NONE',  ( 82.10501726141201573, 40.76148666933337239, -0.9869235838961029073 ) ) ;
#48865 = CARTESIAN_POINT ( 'NONE',  ( 95.19470834736908671, 225.7677522451418497, 10.00000000000009592 ) ) ;
#48866 = CARTESIAN_POINT ( 'NONE',  ( 167.3689703329816325, 278.5095797815824312, -13.36534151890726285 ) ) ;
#48867 = CARTESIAN_POINT ( 'NONE',  ( 23.53136650780448491, 175.2048013555409796, 4.594050593750051981 ) ) ;
#48868 = CARTESIAN_POINT ( 'NONE',  ( 200.6800100461949228, 283.0590218669948399, 18.32402613046234308 ) ) ;
#48869 = VERTEX_POINT ( 'NONE', #25568 ) ;
#48870 = ORIENTED_EDGE ( 'NONE', *, *, #59504, .F. ) ;
#48871 = CARTESIAN_POINT ( 'NONE',  ( 201.0556664636881408, 267.5442616503679005, -3.613160940470883098 ) ) ;
#48872 = CARTESIAN_POINT ( 'NONE',  ( 68.21128839155480250, 69.77371198540542707, 2.434279403033834388 ) ) ;
#48873 = CARTESIAN_POINT ( 'NONE',  ( 82.63815169587347498, 41.85270833316975825, 4.777311450696864803 ) ) ;
#48874 = CYLINDRICAL_SURFACE ( 'NONE', #33727, 14.82106496071141066 ) ;
#48875 = CARTESIAN_POINT ( 'NONE',  ( 161.8882824960653579, 250.2482648971885340, -13.83574485983625557 ) ) ;
#48876 = CARTESIAN_POINT ( 'NONE',  ( 184.9465927238675818, 285.7743050737326485, 15.21868303762837016 ) ) ;
#48877 = CARTESIAN_POINT ( 'NONE',  ( 73.98570270871888965, 68.92876820612471533, -11.10152750440661684 ) ) ;
#48878 = CARTESIAN_POINT ( 'NONE',  ( 38.76791418169571557, 187.0643266524159856, -9.188101187500093303 ) ) ;
#48879 = ORIENTED_EDGE ( 'NONE', *, *, #20933, .F. ) ;
#48880 = CARTESIAN_POINT ( 'NONE',  ( 84.41763424635644242, 48.60878372575622564, 12.39659109532091641 ) ) ;
#48881 = CARTESIAN_POINT ( 'NONE',  ( -6.833909532437232315, 176.8615022471903160, 5.000000000000046185 ) ) ;
#48882 = EDGE_CURVE ( 'NONE', #90329, #14068, #94496, .T. ) ;
#48883 = CARTESIAN_POINT ( 'NONE',  ( -2.801305199957352166, 163.0643266524159571, -9.188101187500093303 ) ) ;
#48884 = CARTESIAN_POINT ( 'NONE',  ( 68.87871463239315517, 64.28074856791785407, -11.90835882824521796 ) ) ;
#48885 = CARTESIAN_POINT ( 'NONE',  ( 198.8533049117289977, 286.2229679703367538, -18.60939981449148561 ) ) ;
#48886 = CARTESIAN_POINT ( 'NONE',  ( 186.6343157368956156, 282.6707309082632378, 16.18028840507778199 ) ) ;
#48887 = CARTESIAN_POINT ( 'NONE',  ( 193.1569697810063531, 296.0893098336876506, -13.02398914535779539 ) ) ;
#48888 = LINE ( 'NONE', #64587, #34588 ) ;
#48889 = CARTESIAN_POINT ( 'NONE',  ( 204.1780753366177237, 277.0001950557890495, 14.05599973203924158 ) ) ;
#48890 = CARTESIAN_POINT ( 'NONE',  ( 191.8210230231139803, 298.4032374945642232, -8.800268167321144475 ) ) ;
#48891 = CARTESIAN_POINT ( 'NONE',  ( 164.2578067403839555, 246.1441285162624126, -2.322300236470859591 ) ) ;
#48892 = ORIENTED_EDGE ( 'NONE', *, *, #11399, .F. ) ;
#48893 = CARTESIAN_POINT ( 'NONE',  ( -8.565960340006073537, 165.8615022471902591, -10.00000000000009592 ) ) ;
#48894 = CARTESIAN_POINT ( 'NONE',  ( 142.1946287021350201, 246.2365022471901739, -10.00000000000009237 ) ) ;
#48895 = CARTESIAN_POINT ( 'NONE',  ( 112.9752924205922824, 236.0333772461660544, 9.188101187500095079 ) ) ;
#48896 = CARTESIAN_POINT ( 'NONE',  ( 21.77916244986271366, 18.28920272979926764, -7.433330006724141015 ) ) ;
#48897 = DIRECTION ( 'NONE',  ( 0.5607300124661794838, -0.8279987035736700030, 0.000000000000000000 ) ) ;
#48898 = CARTESIAN_POINT ( 'NONE',  ( 151.3011447763744570, 269.1990464485573966, 14.21186556778774168 ) ) ;
#48900 = CARTESIAN_POINT ( 'NONE',  ( 150.2076754159204484, 245.9824982072973683, 3.021315404115420679E-15 ) ) ;
#48899 = CARTESIAN_POINT ( 'NONE',  ( 195.7291850945597957, 291.6341022226063160, 17.08310330964873813 ) ) ;
#48901 = CARTESIAN_POINT ( 'NONE',  ( 150.7880176790500855, 269.4744875377281232, -15.26825497096394280 ) ) ;
#48902 = B_SPLINE_CURVE_WITH_KNOTS ( 'NONE', 3,
 ( #27926, #49737, #11265, #27449 ),
 .UNSPECIFIED., .F., .F.,
 ( 4, 4 ),
 ( 0.003021277710772510023, 0.003024111843000437151 ),
 .UNSPECIFIED. ) ;
#48903 = VERTEX_POINT ( 'NONE', #95008 ) ;
#48904 = CARTESIAN_POINT ( 'NONE',  ( 192.9053747558651821, 263.8457269808281467, -4.439418679438619009 ) ) ;
#48905 = CARTESIAN_POINT ( 'NONE',  ( 148.9322735291567597, 272.6887306911919495, -12.40988026045598858 ) ) ;
#48906 = CARTESIAN_POINT ( 'NONE',  ( 184.6885808911535207, 260.6528513612950064, 10.31057805081157852 ) ) ;
#48907 = CARTESIAN_POINT ( 'NONE',  ( 173.9194055806650283, 290.1763249296482172, -1.066906480392311174 ) ) ;
#48908 = CARTESIAN_POINT ( 'NONE',  ( 81.64224228150362705, 55.84784712173523502, -16.01176111343366770 ) ) ;
#48909 = VERTEX_POINT ( 'NONE', #41244 ) ;
#48910 = CARTESIAN_POINT ( 'NONE',  ( 72.87137282294411023, 65.35262256510435463, -13.40290358551061445 ) ) ;
#48911 = AXIS2_PLACEMENT_3D ( 'NONE', #35577, #58366, #20897 ) ;
#48912 = CARTESIAN_POINT ( 'NONE',  ( 175.7290542241515539, 278.6131925542825343, 15.45880334531811151 ) ) ;
#48913 = CARTESIAN_POINT ( 'NONE',  ( 165.6255258425915429, 269.1894970381998178, -17.38843227986124518 ) ) ;
#48914 = B_SPLINE_SURFACE_WITH_KNOTS ( 'NONE', 3, 1, ( 
 ( #40726, #24535 ),
 ( #94479, #86401 ),
 ( #2771, #65047 ),
 ( #16933, #73167 ),
 ( #55913, #78758 ),
 ( #95510, #41225 ),
 ( #72166, #48350 ),
 ( #95996, #41734 ),
 ( #79299, #26557 ),
 ( #71671, #33144 ),
 ( #26057, #87918 ),
 ( #18461, #72678 ),
 ( #43220, #28032 ),
 ( #20962, #59408 ),
 ( #67025, #11860 ),
 ( #96990, #89877 ),
 ( #44708, #19953 ),
 ( #97952, #43722 ),
 ( #36122, #58426 ),
 ( #51845, #90887 ),
 ( #27561, #65537 ),
 ( #88919, #12863 ),
 ( #28524, #5729 ),
 ( #50829, #21435 ),
 ( #52322, #82785 ),
 ( #74665, #57936 ),
 ( #74162, #29048 ),
 ( #4753, #81779 ),
 ( #35133, #42717 ),
 ( #20452, #5242 ),
 ( #51325, #19479 ),
 ( #83264, #97465 ),
 ( #50336, #82292 ),
 ( #90387, #13350 ) ),
 .UNSPECIFIED., .T., .F., .F.,
 ( 4, 2, 2, 2, 2, 2, 2, 2, 2, 2, 2, 2, 2, 2, 2, 2, 4 ),
 ( 2, 2 ),
 ( 0.000000000000000000, 0.06250000000000000000, 0.1250000000000000000, 0.1875000000000000000, 0.2500000000000000000, 0.3125000000000000000, 0.3750000000000000000, 0.4375000000000000000, 0.5000000000000000000, 0.5625000000000000000, 0.6250000000000000000, 0.6875000000000000000, 0.7500000000000000000, 0.8125000000000000000, 0.8750000000000000000, 0.9375000000000000000, 1.000000000000000000 ),
 ( 0.000000000000000000, 1.000000000000000000 ),
 .UNSPECIFIED. ) ;
#48915 = CARTESIAN_POINT ( 'NONE',  ( 79.80408092812572818, 52.66049817665187760, 15.49629232015225000 ) ) ;
#48916 = CARTESIAN_POINT ( 'NONE',  ( 156.6493444904068895, 261.1156140128878178, 17.71731464056091454 ) ) ;
#48917 = CARTESIAN_POINT ( 'NONE',  ( 72.37288529989473318, 71.73372848700918780, -5.731447342215284735 ) ) ;
#48918 = CARTESIAN_POINT ( 'NONE',  ( 153.4619471835925708, 264.8431057800031567, 16.95044998314351758 ) ) ;
#48919 = ORIENTED_EDGE ( 'NONE', *, *, #82936, .F. ) ;
#48920 = LINE ( 'NONE', #40287, #82822 ) ;
#48921 = CARTESIAN_POINT ( 'NONE',  ( 6.591042624459347188, 19.50829794293877839, -10.00000000000000355 ) ) ;
#48922 = CARTESIAN_POINT ( 'NONE',  ( 195.2858898497755433, 290.2585894125917321, -16.56900025010267896 ) ) ;
#48923 = ORIENTED_EDGE ( 'NONE', *, *, #87995, .F. ) ;
#48924 = CARTESIAN_POINT ( 'NONE',  ( 77.98425798866018965, 61.79443237021894930, 16.07418881765924823 ) ) ;
#48925 = CARTESIAN_POINT ( 'NONE',  ( 147.8505793332463725, 274.5622799967613332, -9.317516487097901035 ) ) ;
#48926 = CARTESIAN_POINT ( 'NONE',  ( 85.63227550969774882, 43.97216078338577461, -6.976400197485735255 ) ) ;
#48927 = ORIENTED_EDGE ( 'NONE', *, *, #88252, .T. ) ;
#48928 = CYLINDRICAL_SURFACE ( 'NONE', #11907, 17.82106496071139645 ) ;
#48929 = CARTESIAN_POINT ( 'NONE',  ( 188.5410240070633563, 293.7196559869043426, 13.01390607220156248 ) ) ;
#48930 = CARTESIAN_POINT ( 'NONE',  ( 150.7254409736883645, 269.5828735707850683, 14.54962197351449049 ) ) ;
#48931 = FACE_OUTER_BOUND ( 'NONE', #92309, .T. ) ;
#48932 = CARTESIAN_POINT ( 'NONE',  ( 80.49435834713268889, 44.43729004761577528, 11.36066671759673241 ) ) ;
#48933 = CARTESIAN_POINT ( 'NONE',  ( 84.74798064930895691, 49.97902072749974423, -13.66263633214625806 ) ) ;
#48934 = CARTESIAN_POINT ( 'NONE',  ( 155.6048174803203210, 261.1315455520403361, -17.38645169541727498 ) ) ;
#48935 = ORIENTED_EDGE ( 'NONE', *, *, #60007, .T. ) ;
#48936 = ORIENTED_EDGE ( 'NONE', *, *, #53380, .T. ) ;
#48937 = EDGE_CURVE ( 'NONE', #5335, #709, #24553, .T. ) ;
#48938 = FACE_OUTER_BOUND ( 'NONE', #50167, .T. ) ;
#48939 = VERTEX_POINT ( 'NONE', #32657 ) ;
#48940 = CARTESIAN_POINT ( 'NONE',  ( 46.85966550219794868, 197.8615022471903444, 4.537668576076728569E-14 ) ) ;
#48941 = EDGE_LOOP ( 'NONE', ( #23357, #22363, #80757, #19937 ) ) ;
#48942 = ADVANCED_FACE ( 'NONE', ( #39725 ), #73219, .F. ) ;
#48943 = DIRECTION ( 'NONE',  ( 0.4999999999999992784, -0.8660254037844390407, 0.000000000000000000 ) ) ;
#48944 = CARTESIAN_POINT ( 'NONE',  ( 78.63153613502940686, 50.56850472993508561, 15.05419567323381536 ) ) ;
#48945 = VERTEX_POINT ( 'NONE', #80823 ) ;
#48946 = CARTESIAN_POINT ( 'NONE',  ( 186.1983351278354633, 282.4945498714998280, -16.89931508121779657 ) ) ;
#48947 = CARTESIAN_POINT ( 'NONE',  ( 78.75297625639956323, 47.66336229257158408, 14.29739783539338482 ) ) ;
#48948 = CARTESIAN_POINT ( 'NONE',  ( 147.8889855101223532, 274.4957585470872914, -6.229723215998690833 ) ) ;
#48949 = CARTESIAN_POINT ( 'NONE',  ( 161.7379161894558024, 277.5265442474504312, -13.23162672871571033 ) ) ;
#48950 = CARTESIAN_POINT ( 'NONE',  ( 193.0142717932987182, 296.3364699985351081, -13.30037542329744937 ) ) ;
#48951 = DIRECTION ( 'NONE',  ( -0.6056412518070772855, -0.7957378174433814566, 0.000000000000000000 ) ) ;
#48952 = ADVANCED_FACE ( 'NONE', ( #89894 ), #3773, .T. ) ;
#48953 = CARTESIAN_POINT ( 'NONE',  ( 84.18924544147772338, 41.92290757784675748, -3.949398286619972165 ) ) ;
#48954 = CARTESIAN_POINT ( 'NONE',  ( 157.9162940790990604, 280.9685295036878756, 2.104535951830800222 ) ) ;
#48955 = CARTESIAN_POINT ( 'NONE',  ( 128.9971094863694532, 233.0327760586659451, 1.948934522072303157E-15 ) ) ;
#48956 = ORIENTED_EDGE ( 'NONE', *, *, #23587, .T. ) ;
#48957 = CARTESIAN_POINT ( 'NONE',  ( 70.79161049076395784, 61.41985499215619626, -14.84464568873325518 ) ) ;
#48958 = ORIENTED_EDGE ( 'NONE', *, *, #29889, .F. ) ;
#48960 = ORIENTED_EDGE ( 'NONE', *, *, #59559, .T. ) ;
#48959 = CARTESIAN_POINT ( 'NONE',  ( 24.00897855452593888, 29.56454794089042082, 10.00000000000000355 ) ) ;
#48961 = CARTESIAN_POINT ( 'NONE',  ( 203.5231681107415511, 276.4626886777189156, 14.22114972371920416 ) ) ;
#48962 = CARTESIAN_POINT ( 'NONE',  ( 180.1475770660277647, 255.8711682511834340, 1.311453321043420051 ) ) ;
#48963 = CARTESIAN_POINT ( 'NONE',  ( 171.1366801964148578, 287.7825823751429652, -4.654478872985349014 ) ) ;
#48964 = CARTESIAN_POINT ( 'NONE',  ( 48.29091023345864642, 82.53782597618220507, -10.00000000000000000 ) ) ;
#48965 = CARTESIAN_POINT ( 'NONE',  ( 156.7136391252028602, 279.5216684332963837, 7.468001664478725488 ) ) ;
#48966 = PLANE ( 'NONE',  #5991 ) ;
#48967 = CARTESIAN_POINT ( 'NONE',  ( 77.95436975687957215, 48.11784896437988834, 14.20357318872344621 ) ) ;
#48968 = CARTESIAN_POINT ( 'NONE',  ( 174.0035762054535269, 281.4834410953270094, 14.05709486446668244 ) ) ;
#48969 = CARTESIAN_POINT ( 'NONE',  ( 177.2141887958173072, 256.0616080229310114, -7.313315655081018996 ) ) ;
#48970 = ORIENTED_EDGE ( 'NONE', *, *, #76953, .T. ) ;
#48971 = DIRECTION ( 'NONE',  ( 1.000000000000000000, -1.084449990124929494E-13, 0.000000000000000000 ) ) ;
#48972 = CARTESIAN_POINT ( 'NONE',  ( 65.73886374032248625, 69.08165079949409915, -0.06455758818544669875 ) ) ;
#48973 = ORIENTED_EDGE ( 'NONE', *, *, #6421, .F. ) ;
#48974 = LINE ( 'NONE', #73278, #11199 ) ;
#48975 = B_SPLINE_CURVE_WITH_KNOTS ( 'NONE', 3,
 ( #58029, #19563, #50422, #42802 ),
 .UNSPECIFIED., .F., .F.,
 ( 4, 4 ),
 ( 0.01114209618785225175, 0.01956799148668745755 ),
 .UNSPECIFIED. ) ;
#48976 = CARTESIAN_POINT ( 'NONE',  ( 156.6716504413620896, 276.8562130845049296, 9.991782109645525267 ) ) ;
#48977 = CARTESIAN_POINT ( 'NONE',  ( 192.2053377076082086, 297.7375849349253940, -10.11643020772709534 ) ) ;
#48978 = CARTESIAN_POINT ( 'NONE',  ( 190.8153366230912411, 300.1451374358846920, 3.771947273125533684 ) ) ;
#48980 = AXIS2_PLACEMENT_3D ( 'NONE', #87592, #81448, #88078 ) ;
#48979 = CARTESIAN_POINT ( 'NONE',  ( 202.6560281492536717, 279.6364581158209717, 17.15553667345918853 ) ) ;
#48982 = CARTESIAN_POINT ( 'NONE',  ( 151.5115963269173562, 274.8992243283395283, -8.951992038018516951 ) ) ;
#48981 = CARTESIAN_POINT ( 'NONE',  ( 164.0880046841931517, 283.2396324619593884, -6.684692064823180679 ) ) ;
#48983 = AXIS2_PLACEMENT_3D ( 'NONE', #31564, #45278, #23463 ) ;
#48984 = CARTESIAN_POINT ( 'NONE',  ( 157.7632566947985708, 282.3764601569879460, -1.694678876849560645 ) ) ;
#48985 = ORIENTED_EDGE ( 'NONE', *, *, #62049, .T. ) ;
#48986 = CARTESIAN_POINT ( 'NONE',  ( 76.45572749640668064, 51.64231386250387601, -16.15369532800221819 ) ) ;
#48987 = FACE_OUTER_BOUND ( 'NONE', #64538, .T. ) ;
#48988 = VECTOR ( 'NONE', #22365, 1000.000000000000000 ) ;
#48989 = CARTESIAN_POINT ( 'NONE',  ( 75.87525401958798454, 64.72722897157592570, -14.29033900848947169 ) ) ;
#48990 = CARTESIAN_POINT ( 'NONE',  ( 187.0645750985391373, 267.3865546210132038, 14.82880848505713800 ) ) ;
#48991 = CARTESIAN_POINT ( 'NONE',  ( 80.75774510745969792, 43.20856077877414236, -9.122087061355482973 ) ) ;
#48992 = CARTESIAN_POINT ( 'NONE',  ( 45.19716250472275476, 70.24742367233086782, 10.00000000000000000 ) ) ;
#48993 = CARTESIAN_POINT ( 'NONE',  ( -1.069254392388470976, 164.0643266524160140, 9.188101187500095079 ) ) ;
#48994 = CARTESIAN_POINT ( 'NONE',  ( 90.05242219234915524, 231.9869531367911293, 4.594050593750046652 ) ) ;
#48995 = CARTESIAN_POINT ( 'NONE',  ( 155.4661767250933622, 261.3716783840932294, -17.10192542004562810 ) ) ;
#48996 = CARTESIAN_POINT ( 'NONE',  ( 88.19817206715259772, 44.49282453600611831, -4.737833512016797144 ) ) ;
#48997 = DIRECTION ( 'NONE',  ( -0.8660254037844384856, -0.5000000000000002220, 0.000000000000000000 ) ) ;
#48998 = DIRECTION ( 'NONE',  ( -0.000000000000000000, 0.000000000000000000, 1.000000000000000000 ) ) ;
#48999 = CIRCLE ( 'NONE', #86208, 70.00000000000001421 ) ;
#49000 = EDGE_CURVE ( 'NONE', #31328, #65871, #66059, .T. ) ;
#49001 = DIRECTION ( 'NONE',  ( 0.7071067811865465735, 0.000000000000000000, 0.7071067811865484609 ) ) ;
#49002 = DIRECTION ( 'NONE',  ( -0.000000000000000000, -0.000000000000000000, -1.000000000000000000 ) ) ;
#49003 = CARTESIAN_POINT ( 'NONE',  ( 163.6926455977765897, 284.3758010234985818, 5.960030555855258427 ) ) ;
#49005 = CARTESIAN_POINT ( 'NONE',  ( 207.6837091943624785, 270.9282591014416539, -1.156610046911421552 ) ) ;
#49004 = DIRECTION ( 'NONE',  ( -0.000000000000000000, 1.000000000000000000, -0.000000000000000000 ) ) ;
#49006 = CARTESIAN_POINT ( 'NONE',  ( 178.6423073663378602, 290.9544255387157818, 10.03153667033594765 ) ) ;
#49007 = CARTESIAN_POINT ( 'NONE',  ( 164.1493212971148807, 246.3320308158860144, -5.698338322471421691 ) ) ;
#49008 = CARTESIAN_POINT ( 'NONE',  ( 77.99682093914630343, 55.11119047563809659, -16.10778797222130621 ) ) ;
#49009 = CYLINDRICAL_SURFACE ( 'NONE', #33420, 16.60714546451156792 ) ;
#49010 = EDGE_CURVE ( 'NONE', #69987, #14298, #72697, .T. ) ;
#49011 = CARTESIAN_POINT ( 'NONE',  ( 73.64088816139484095, 69.63733386616164012, 10.15931356738738423 ) ) ;
#49012 = CARTESIAN_POINT ( 'NONE',  ( 52.08270766911643079, 207.0024278399160664, -9.188101187500093303 ) ) ;
#49013 = DIRECTION ( 'NONE',  ( -0.8660254037844382635, -0.5000000000000004441, 0.000000000000000000 ) ) ;
#49014 = ADVANCED_FACE ( 'NONE', ( #13369 ), #19498, .F. ) ;
#49015 = CARTESIAN_POINT ( 'NONE',  ( 70.26924114858965709, 217.5024278399160664, -9.188101187500093303 ) ) ;
#49016 = CARTESIAN_POINT ( 'NONE',  ( 161.6127771116929921, 250.7254542206800352, -12.96229604595372464 ) ) ;
#49017 = DIRECTION ( 'NONE',  ( -0.1032265479692855564, 0.9946578707245747886, 0.000000000000000000 ) ) ;
#49018 = CARTESIAN_POINT ( 'NONE',  ( -22.42236680055709641, 157.8615022471902591, 0.000000000000000000 ) ) ;
#49020 = DIRECTION ( 'NONE',  ( -0.8615733660689098850, -0.5076330711061763923, 0.000000000000000000 ) ) ;
#49019 = CARTESIAN_POINT ( 'NONE',  ( -43.64404709005470551, 40.32064712455566990, 59.99999999999999289 ) ) ;
#49021 = CARTESIAN_POINT ( 'NONE',  ( 175.9592805506638626, 269.6404646308017163, -17.54410699522518868 ) ) ;
#49022 = CARTESIAN_POINT ( 'NONE',  ( 26.97895004263468266, 38.68290643055188838, 3.479690158560446702E-15 ) ) ;
#49023 = CARTESIAN_POINT ( 'NONE',  ( 82.34816312114848813, 49.74663056318024701, 14.30763284621803244 ) ) ;
#49024 = CARTESIAN_POINT ( 'NONE',  ( 84.83591964108416050, 46.74628741325042114, -10.57126189487417633 ) ) ;
#49025 = ORIENTED_EDGE ( 'NONE', *, *, #71457, .F. ) ;
#49026 = CARTESIAN_POINT ( 'NONE',  ( 82.61045024828291616, 212.3768266524159856, -9.188101187500093303 ) ) ;
#49027 = LINE ( 'NONE', #35684, #85350 ) ;
#49028 = CARTESIAN_POINT ( 'NONE',  ( 170.3290958195750022, 289.6815776661216546, -1.151831906498994140 ) ) ;
#49029 = CARTESIAN_POINT ( 'NONE',  ( -32.89006047420026135, 94.48531712824750173, 10.45786326575769998 ) ) ;
#49030 = CARTESIAN_POINT ( 'NONE',  ( 202.0097953763375358, 280.7557661120279136, 17.59517121574885579 ) ) ;
#49031 = ORIENTED_EDGE ( 'NONE', *, *, #81679, .T. ) ;
#49032 = CARTESIAN_POINT ( 'NONE',  ( 24.19030146973739193, 38.49624447322263165, 177.5919119679930134 ) ) ;
#49033 = DIRECTION ( 'NONE',  ( 0.8660254037844380415, 0.5000000000000011102, 0.000000000000000000 ) ) ;
#49034 = DIRECTION ( 'NONE',  ( 0.000000000000000000, 0.000000000000000000, 1.000000000000000000 ) ) ;
#49035 = CARTESIAN_POINT ( 'NONE',  ( 87.53367671268780725, 44.88112536278567433, -6.578546970659244764 ) ) ;
#49036 = CARTESIAN_POINT ( 'NONE',  ( 116.0695290213043620, 244.4865022471903444, -10.00000000000009415 ) ) ;
#49037 = CARTESIAN_POINT ( 'NONE',  ( 74.82952949953238431, 53.40084132974138953, 16.53760015760405722 ) ) ;
#49038 = VERTEX_POINT ( 'NONE', #96011 ) ;
#49039 = CARTESIAN_POINT ( 'NONE',  ( 82.07496931413966479, 54.01582194328672415, 15.59905118150530967 ) ) ;
#49040 = ORIENTED_EDGE ( 'NONE', *, *, #69955, .F. ) ;
#49041 = CARTESIAN_POINT ( 'NONE',  ( 202.9685995779611858, 279.0950685203052899, 16.84977534244423580 ) ) ;
#49042 = CARTESIAN_POINT ( 'NONE',  ( -64.94778771796556782, 41.33875607593970614, -10.00000000000000000 ) ) ;
#49043 = CARTESIAN_POINT ( 'NONE',  ( 73.00396795756827828, 57.62093675928252878, -16.32480838619500219 ) ) ;
#49044 = ORIENTED_EDGE ( 'NONE', *, *, #17486, .T. ) ;
#49045 = CARTESIAN_POINT ( 'NONE',  ( -24.63924516542739696, 141.7012482093459198, 1.426039447152360146E-13 ) ) ;
#49046 = VERTEX_POINT ( 'NONE', #26572 ) ;
#49047 = CARTESIAN_POINT ( 'NONE',  ( 189.1676533816863071, 290.3111667206173365, 14.33508402202939891 ) ) ;
#49048 = CARTESIAN_POINT ( 'NONE',  ( 170.5023504269580030, 250.3523026268861713, 3.405075941885475022 ) ) ;
#49049 = CARTESIAN_POINT ( 'NONE',  ( 180.8673497570526933, 284.8464743004457773, -15.75982562109706819 ) ) ;
#49050 = ORIENTED_EDGE ( 'NONE', *, *, #21817, .T. ) ;
#49051 = CARTESIAN_POINT ( 'NONE',  ( 30.86762485498029207, 38.79752408145594700, -5.678558825948271327 ) ) ;
#49052 = CARTESIAN_POINT ( 'NONE',  ( 80.14444365492592226, 44.30149127559567290, 11.42155680931026573 ) ) ;
#49053 = CARTESIAN_POINT ( 'NONE',  ( 84.88199885514633536, 50.20673742124042604, -13.33258340498515437 ) ) ;
#49054 = CARTESIAN_POINT ( 'NONE',  ( -23.29562891409031522, 78.77562236714182120, 52.49999999999999289 ) ) ;
#49055 = EDGE_CURVE ( 'NONE', #63052, #60481, #99462, .T. ) ;
#49056 = AXIS2_PLACEMENT_3D ( 'NONE', #52727, #33442, #64340 ) ;
#49057 = FACE_OUTER_BOUND ( 'NONE', #30099, .T. ) ;
#49058 = LINE ( 'NONE', #79992, #77207 ) ;
#49059 = EDGE_LOOP ( 'NONE', ( #51746, #32520, #28844, #3390 ) ) ;
#49060 = EDGE_LOOP ( 'NONE', ( #51663, #32754, #78592, #21335 ) ) ;
#49061 = CARTESIAN_POINT ( 'NONE',  ( 183.1375400018946777, 295.7571731117037643, 0.9692433187012515772 ) ) ;
#49063 = FACE_OUTER_BOUND ( 'NONE', #30214, .T. ) ;
#49062 = CARTESIAN_POINT ( 'NONE',  ( 204.5133713884061706, 276.4194452585140311, 14.87364779308245843 ) ) ;
#49064 = CARTESIAN_POINT ( 'NONE',  ( 81.45669997382150029, 55.98862135975878118, -16.04303691645969820 ) ) ;
#49065 = CARTESIAN_POINT ( 'NONE',  ( 155.5660013421004919, 261.1987770755905558, 17.28709111629370199 ) ) ;
#49066 = CARTESIAN_POINT ( 'NONE',  ( 121.6084831627943998, 251.0177522451418781, 5.000000000000046185 ) ) ;
#49067 = CARTESIAN_POINT ( 'NONE',  ( 70.34454795188869980, 61.29844696716961749, 14.78467410895967760 ) ) ;
#49068 = CARTESIAN_POINT ( 'NONE',  ( 207.5461847957217003, 271.1664583471679748, -5.063772443593253847 ) ) ;
#49069 = EDGE_CURVE ( 'NONE', #63771, #2846, #30039, .T. ) ;
#49070 = CARTESIAN_POINT ( 'NONE',  ( 166.2346546936187508, 265.4583583427066742, 16.55353420763369954 ) ) ;
#49071 = AXIS2_PLACEMENT_3D ( 'NONE', #32336, #8543, #31820 ) ;
#49072 = FACE_OUTER_BOUND ( 'NONE', #99676, .T. ) ;
#49073 = CARTESIAN_POINT ( 'NONE',  ( 75.51934661115029712, 226.6589784336661637, -6.496448406907675876E-16 ) ) ;
#49074 = VERTEX_POINT ( 'NONE', #77137 ) ;
#49075 = CARTESIAN_POINT ( 'NONE',  ( 150.5780525126727980, 271.8381578737140103, 12.98431582152410968 ) ) ;
#49076 = CARTESIAN_POINT ( 'NONE',  ( 74.62401959271109320, 66.89443057110609914, 13.05059976691390311 ) ) ;
#49077 = ORIENTED_EDGE ( 'NONE', *, *, #3947, .T. ) ;
#49078 = CARTESIAN_POINT ( 'NONE',  ( 157.0907897361001631, 258.5577661063921937, -18.43739762333529342 ) ) ;
#49079 = ORIENTED_EDGE ( 'NONE', *, *, #68382, .T. ) ;
#49080 = CARTESIAN_POINT ( 'NONE',  ( 80.42297664653236211, 44.73783946406587830, -11.66823080374195420 ) ) ;
#49081 = FACE_OUTER_BOUND ( 'NONE', #12674, .T. ) ;
#49082 = PLANE ( 'NONE',  #2924 ) ;
#49083 = CARTESIAN_POINT ( 'NONE',  ( 83.90325127553046514, 41.85121661673234428, -1.721470070664741225 ) ) ;
#49084 = CARTESIAN_POINT ( 'NONE',  ( 159.3237119419271437, 254.6902313965507858, -15.56765445935501191 ) ) ;
#49085 = CARTESIAN_POINT ( 'NONE',  ( 50.34596055286379368, 92.70800680107760172, 10.00000000000000000 ) ) ;
#49086 = CARTESIAN_POINT ( 'NONE',  ( 94.43719644265542001, 216.1423013555410080, -4.594050593750043987 ) ) ;
#49087 = ORIENTED_EDGE ( 'NONE', *, *, #34396, .F. ) ;
#49088 = FACE_OUTER_BOUND ( 'NONE', #48715, .T. ) ;
#49089 = ORIENTED_EDGE ( 'NONE', *, *, #83276, .F. ) ;
#49090 = B_SPLINE_CURVE_WITH_KNOTS ( 'NONE', 3,
 ( #83351, #59493, #98539, #90472 ),
 .UNSPECIFIED., .F., .F.,
 ( 4, 4 ),
 ( 0.03354936294194791474, 0.04243329031352276182 ),
 .UNSPECIFIED. ) ;
#49091 = CARTESIAN_POINT ( 'NONE',  ( 31.17504386912796477, 20.12755873383627758, -6.180339887498949025 ) ) ;
#49092 = CARTESIAN_POINT ( 'NONE',  ( 70.71923034029678945, 69.39805573920016002, -7.454743742243774562 ) ) ;
#49093 = CARTESIAN_POINT ( 'NONE',  ( 87.77567103309253582, 45.10408226285451150, -6.743331934586553444 ) ) ;
#49094 = CARTESIAN_POINT ( 'NONE',  ( -7.357133217438179607, 159.8927522451417929, -10.00000000000009059 ) ) ;
#49095 = CARTESIAN_POINT ( 'NONE',  ( 87.92412256492882250, 44.79819542341160599, 4.880203861778121599 ) ) ;
#49096 = VERTEX_POINT ( 'NONE', #92871 ) ;
#49097 = CARTESIAN_POINT ( 'NONE',  ( 157.1187995864133882, 258.5092516225370218, 18.42986330599266509 ) ) ;
#49098 = CARTESIAN_POINT ( 'NONE',  ( 160.6939490957829264, 275.5766803063729640, 12.96402070036174337 ) ) ;
#49099 = CARTESIAN_POINT ( 'NONE',  ( 81.96852851063667345, 40.98455881841368154, -3.062051805011598571 ) ) ;
#49100 = CARTESIAN_POINT ( 'NONE',  ( 188.9422029048082834, 269.7498099985592148, 14.56541238386251891 ) ) ;
#49101 = CYLINDRICAL_SURFACE ( 'NONE', #60833, 10.00000000000010658 ) ;
#49102 = DIRECTION ( 'NONE',  ( 0.000000000000000000, 0.000000000000000000, 1.000000000000000000 ) ) ;
#49103 = LINE ( 'NONE', #78012, #40463 ) ;
#49104 = VERTEX_POINT ( 'NONE', #68044 ) ;
#49105 = CARTESIAN_POINT ( 'NONE',  ( 148.9908051373835463, 274.2115824367425603, 8.962154046299646737 ) ) ;
#49106 = CARTESIAN_POINT ( 'NONE',  ( 175.6264801365410051, 290.2407708024952626, 8.598400420672549060 ) ) ;
#49107 = CARTESIAN_POINT ( 'NONE',  ( 84.37722046559913736, 42.81587621694462342, 4.768053884619589233 ) ) ;
#49108 = CARTESIAN_POINT ( 'NONE',  ( 24.77599400646307970, 14.70852965304480087, 1.583844403245364907 ) ) ;
#49109 = DIRECTION ( 'NONE',  ( -0.9055221650797476984, -0.4242989612870696758, 0.000000000000000000 ) ) ;
#49110 = CARTESIAN_POINT ( 'NONE',  ( 117.4407359106297974, 228.6115022471901739, -5.000000000000041744 ) ) ;
#49111 = CARTESIAN_POINT ( 'NONE',  ( 202.7288423927450651, 279.5103401465790398, -16.79777765389096800 ) ) ;
#49112 = VERTEX_POINT ( 'NONE', #60926 ) ;
#49113 = AXIS2_PLACEMENT_3D ( 'NONE', #43899, #43400, #5909 ) ;
#49114 = ADVANCED_FACE ( 'NONE', ( #46735 ), #54315, .T. ) ;
#49115 = CARTESIAN_POINT ( 'NONE',  ( 164.6460902696047128, 245.4716017159096566, -3.036414139157908476 ) ) ;
#49117 = CARTESIAN_POINT ( 'NONE',  ( 184.8290635382854248, 266.2232361729078889, 13.18960270750180008 ) ) ;
#49116 = CARTESIAN_POINT ( 'NONE',  ( 180.5854428321844978, 266.8285079129313999, -14.77326707302557196 ) ) ;
#49118 = CARTESIAN_POINT ( 'NONE',  ( 199.1207061629229429, 281.8795345183781365, -16.59791185551577186 ) ) ;
#49119 = EDGE_CURVE ( 'NONE', #83865, #8776, #46215, .T. ) ;
#49120 = B_SPLINE_CURVE_WITH_KNOTS ( 'NONE', 3,
 ( #17583, #55065, #1394, #93615 ),
 .UNSPECIFIED., .F., .F.,
 ( 4, 4 ),
 ( 2.797157557069881010E-17, 0.003963014350466228901 ),
 .UNSPECIFIED. ) ;
#49121 = CARTESIAN_POINT ( 'NONE',  ( 40.07751882555258049, 24.10801979619931501, 3.090169943749476733 ) ) ;
#49122 = CARTESIAN_POINT ( 'NONE',  ( 91.45997379709655206, 233.6115022471902876, -5.000000000000047962 ) ) ;
#49123 = CARTESIAN_POINT ( 'NONE',  ( 180.9931686530488548, 273.3540426091562381, 16.66408796176733276 ) ) ;
#49124 = CARTESIAN_POINT ( 'NONE',  ( 160.1418619798153600, 272.5460874529753710, -14.82127459029824124 ) ) ;
#49125 = PLANE ( 'NONE',  #7452 ) ;
#49126 = B_SPLINE_CURVE_WITH_KNOTS ( 'NONE', 3,
 ( #66627, #89966, #44312, #20546, #51424, #90973, #21533 ),
 .UNSPECIFIED., .F., .F.,
 ( 4, 3, 4 ),
 ( 0.001252835390139021452, 0.001498048275941827635, 0.002504222586275619590 ),
 .UNSPECIFIED. ) ;
#49127 = CARTESIAN_POINT ( 'NONE',  ( -5.074968980656518802, 174.0024278399160664, -9.188101187500093303 ) ) ;
#49128 = AXIS2_PLACEMENT_3D ( 'NONE', #38670, #54868, #24968 ) ;
#49129 = CARTESIAN_POINT ( 'NONE',  ( 81.36240293647936994, 45.51711427137305321, 11.23452077343203115 ) ) ;
#49130 = ORIENTED_EDGE ( 'NONE', *, *, #74800, .T. ) ;
#49131 = ADVANCED_FACE ( 'NONE', ( #98966 ), #38116, .F. ) ;
#49132 = CARTESIAN_POINT ( 'NONE',  ( 87.06988255670405863, 46.05766899987094831, 8.936389965629217613 ) ) ;
#49133 = CARTESIAN_POINT ( 'NONE',  ( 30.64569906364082641, 29.64441083166262558, -10.00000000000000533 ) ) ;
#49134 = CARTESIAN_POINT ( 'NONE',  ( 81.88434891954030093, 41.68080424094055303, 5.410084833112948743 ) ) ;
#49135 = CARTESIAN_POINT ( 'NONE',  ( 33.24700223256990483, 183.8768266524160140, -9.188101187500093303 ) ) ;
#49136 = FACE_OUTER_BOUND ( 'NONE', #60416, .T. ) ;
#49137 = CARTESIAN_POINT ( 'NONE',  ( 70.67536410627012344, 201.6115022471901739, -5.000000000000041744 ) ) ;
#49138 = CARTESIAN_POINT ( 'NONE',  ( 39.48212635690286021, 23.76426979415093044, 3.090169943749476733 ) ) ;
#49139 = CARTESIAN_POINT ( 'NONE',  ( 199.6646305490404814, 267.3205410694829425, -6.722116363147288887 ) ) ;
#49140 = CARTESIAN_POINT ( 'NONE',  ( 191.1747001918821525, 299.5227014763493116, -9.654804683100723040 ) ) ;
#49141 = CARTESIAN_POINT ( 'NONE',  ( 196.2972863317696692, 290.6501220159163381, 17.07231422512514740 ) ) ;
#49142 = CARTESIAN_POINT ( 'NONE',  ( 182.5462621144656907, 280.4176611228211300, -16.08232872008645487 ) ) ;
#49143 = CARTESIAN_POINT ( 'NONE',  ( -19.53599293563658179, 93.14499714974044764, 59.99999999999999289 ) ) ;
#49144 = B_SPLINE_SURFACE_WITH_KNOTS ( 'NONE', 3, 1, ( 
 ( #85772, #94343 ),
 ( #62896, #47195 ),
 ( #86260, #61882 ),
 ( #55281, #9208 ),
 ( #55773, #16800 ),
 ( #85247, #46179 ),
 ( #78621, #40081 ),
 ( #1626, #605 ),
 ( #2116, #71026 ),
 ( #1112, #7701 ),
 ( #32999, #31489 ),
 ( #63900, #47686 ),
 ( #32512, #15792 ),
 ( #8209, #16301 ),
 ( #63404, #94839 ),
 ( #24897, #69499 ),
 ( #25401, #78117 ),
 ( #23388, #24405 ),
 ( #87287, #8706 ),
 ( #54793, #54278 ),
 ( #93851, #79149 ),
 ( #86765, #77099 ),
 ( #113, #38594 ),
 ( #39574, #30997 ),
 ( #46698, #70497 ),
 ( #40585, #17299 ),
 ( #48203, #9732 ),
 ( #77625, #39079 ),
 ( #23892, #69991 ),
 ( #31990, #62381 ),
 ( #93338, #95856 ),
 ( #74015, #57788 ),
 ( #49217, #58775 ),
 ( #27896, #50200 ) ),
 .UNSPECIFIED., .T., .F., .F.,
 ( 4, 2, 2, 2, 2, 2, 2, 2, 2, 2, 2, 2, 2, 2, 2, 2, 4 ),
 ( 2, 2 ),
 ( 0.000000000000000000, 0.06250000000000000000, 0.1250000000000000000, 0.1875000000000000000, 0.2500000000000000000, 0.3125000000000000000, 0.3750000000000000000, 0.4375000000000000000, 0.5000000000000000000, 0.5625000000000000000, 0.6250000000000000000, 0.6875000000000000000, 0.7500000000000000000, 0.8125000000000000000, 0.8750000000000000000, 0.9375000000000000000, 1.000000000000000000 ),
 ( 0.000000000000000000, 1.000000000000000000 ),
 .UNSPECIFIED. ) ;
#49145 = CARTESIAN_POINT ( 'NONE',  ( 187.3763302972169242, 296.2500356619865443, -7.707757652183316210 ) ) ;
#49146 = ADVANCED_FACE ( 'NONE', ( #91890 ), #22442, .T. ) ;
#49147 = CARTESIAN_POINT ( 'NONE',  ( 83.78171082742430542, 51.97306301863909539, 14.95037678041454932 ) ) ;
#49148 = EDGE_CURVE ( 'NONE', #14885, #72252, #85285, .T. ) ;
#49149 = CARTESIAN_POINT ( 'NONE',  ( 87.56285948006663489, 221.3615022471902591, -10.00000000000009592 ) ) ;
#49150 = CARTESIAN_POINT ( 'NONE',  ( 164.8620696960021519, 246.0477266191988406, 0.9441760987540538386 ) ) ;
#49151 = CARTESIAN_POINT ( 'NONE',  ( 77.93017357788673394, 184.0458036431182052, 21.50000000000000000 ) ) ;
#49152 = CARTESIAN_POINT ( 'NONE',  ( 50.29670382169353360, 199.8458772461660260, 9.188101187500095079 ) ) ;
#49153 = CARTESIAN_POINT ( 'NONE',  ( 197.8822014719394531, 287.9049684674569676, 17.88172308374019792 ) ) ;
#49154 = ORIENTED_EDGE ( 'NONE', *, *, #42120, .F. ) ;
#49155 = DIRECTION ( 'NONE',  ( 0.8660254037844373753, 0.5000000000000021094, 0.000000000000000000 ) ) ;
#49156 = CARTESIAN_POINT ( 'NONE',  ( 150.9115585710837877, 269.2605084359132093, -15.80434701481532578 ) ) ;
#49157 = CARTESIAN_POINT ( 'NONE',  ( 67.23736956560070155, 67.19511859228909145, -8.571709603932553989 ) ) ;
#49158 = VERTEX_POINT ( 'NONE', #21942 ) ;
#49159 = CARTESIAN_POINT ( 'NONE',  ( 169.7025245114118945, 285.7301650108328772, 7.496735491984821920 ) ) ;
#49160 = CARTESIAN_POINT ( 'NONE',  ( 168.0788774586240493, 281.7893607645295333, -11.63581643431726320 ) ) ;
#49161 = DIRECTION ( 'NONE',  ( -0.8660254037844377084, -0.5000000000000015543, -3.252519625699478541E-16 ) ) ;
#49162 = CARTESIAN_POINT ( 'NONE',  ( 72.12749769884386808, 68.75288622073954059, 10.17241042758247183 ) ) ;
#49163 = CARTESIAN_POINT ( 'NONE',  ( 31.43713336585798146, 20.01110640527293683, 2.839279412974134775 ) ) ;
#49164 = CARTESIAN_POINT ( 'NONE',  ( 202.9685995779611858, 279.0950685203052899, 16.84977534244423580 ) ) ;
#49165 = CARTESIAN_POINT ( 'NONE',  ( 196.5806080813426888, 290.1593943507663766, -16.31912166233602690 ) ) ;
#49166 = CARTESIAN_POINT ( 'NONE',  ( 175.0827542836768771, 257.3802440988434910, 11.53455802463486712 ) ) ;
#49167 = ORIENTED_EDGE ( 'NONE', *, *, #77601, .T. ) ;
#49168 = CARTESIAN_POINT ( 'NONE',  ( 21.04482852044473162, 14.01110640527291906, 2.839279412974134775 ) ) ;
#49169 = B_SPLINE_CURVE_WITH_KNOTS ( 'NONE', 3,
 ( #25817, #80037, #4492, #27798, #58672, #89644, #51076, #56693, #82038, #12613 ),
 .UNSPECIFIED., .F., .F.,
 ( 4, 2, 2, 2, 4 ),
 ( 0.000000000000000000, 0.0002622400424273094513, 0.0005244800848546189026, 0.0007867201272819283539, 0.001048960169709237805 ),
 .UNSPECIFIED. ) ;
#49170 = LINE ( 'NONE', #10171, #30235 ) ;
#49171 = CARTESIAN_POINT ( 'NONE',  ( 171.6344159911060387, 252.4546017485605489, 8.684224258240840655 ) ) ;
#49172 = CARTESIAN_POINT ( 'NONE',  ( 77.56105267981615725, 49.72783448595330213, -15.46007777815280981 ) ) ;
#49173 = EDGE_CURVE ( 'NONE', #16631, #35859, #75660, .T. ) ;
#49174 = VERTEX_POINT ( 'NONE', #7743 ) ;
#49175 = CARTESIAN_POINT ( 'NONE',  ( 179.4321505992908214, 282.5710338533123718, 15.18541787117502118 ) ) ;
#49176 = CARTESIAN_POINT ( 'NONE',  ( 190.8264243556038195, 300.1259329198319961, 8.466983560044813117 ) ) ;
#49177 = CARTESIAN_POINT ( 'NONE',  ( 177.3128891232254318, 256.0384362114311898, -7.181690309295756691 ) ) ;
#49178 = CARTESIAN_POINT ( 'NONE',  ( 68.61392852225033323, 65.52134601779788170, -11.40821467630667563 ) ) ;
#49179 = ORIENTED_EDGE ( 'NONE', *, *, #11543, .F. ) ;
#49180 = EDGE_CURVE ( 'NONE', #85997, #6688, #69034, .T. ) ;
#49182 = CARTESIAN_POINT ( 'NONE',  ( 171.7624276866505113, 273.7583704609413076, 17.52529772748773595 ) ) ;
#49181 = CARTESIAN_POINT ( 'NONE',  ( 161.1747502674735415, 251.4841389699472529, -13.25152330924089839 ) ) ;
#49183 = CARTESIAN_POINT ( 'NONE',  ( 196.7823306783968746, 289.8100005636337073, -17.85370042640856170 ) ) ;
#49184 = ORIENTED_EDGE ( 'NONE', *, *, #5261, .F. ) ;
#49185 = CARTESIAN_POINT ( 'NONE',  ( 45.27367124825920541, 27.10801979619933277, 3.090169943749476733 ) ) ;
#49186 = LINE ( 'NONE', #41053, #25354 ) ;
#49187 = CARTESIAN_POINT ( 'NONE',  ( 73.06484434959700991, 57.43056366546561975, -15.87593782397910402 ) ) ;
#49188 = CARTESIAN_POINT ( 'NONE',  ( 77.99401760355904401, 61.40429962668400776, -16.15929906019731632 ) ) ;
#49189 = CARTESIAN_POINT ( 'NONE',  ( 166.8729799300310219, 285.2663129487913238, 8.463664631012395745 ) ) ;
#49190 = CARTESIAN_POINT ( 'NONE',  ( 115.8441751185107336, 231.5643266524159856, 9.188101187500095079 ) ) ;
#49191 = ADVANCED_FACE ( 'NONE', ( #53337 ), #52340, .T. ) ;
#49192 = CARTESIAN_POINT ( 'NONE',  ( 196.2293283710122012, 290.7678286567270902, -17.07152402978540096 ) ) ;
#49193 = CARTESIAN_POINT ( 'NONE',  ( 183.3879987404869496, 288.3258381666292394, -13.17223454804403993 ) ) ;
#49194 = EDGE_CURVE ( 'NONE', #77668, #79774, #84290, .T. ) ;
#49195 = EDGE_LOOP ( 'NONE', ( #69675, #23858, #20539, #73736 ) ) ;
#49196 = CARTESIAN_POINT ( 'NONE',  ( 208.0045976720423084, 270.3724639545367836, 2.002128742561712471 ) ) ;
#49197 = ORIENTED_EDGE ( 'NONE', *, *, #35698, .T. ) ;
#49198 = ADVANCED_FACE ( 'NONE', ( #15319 ), #86778, .T. ) ;
#49199 = CARTESIAN_POINT ( 'NONE',  ( 30.33837380989695731, 32.91421378149920685, 9.188101187500008038 ) ) ;
#49200 = CARTESIAN_POINT ( 'NONE',  ( 157.2590776934911787, 259.4042227141288208, 17.28571348683609088 ) ) ;
#49201 = CARTESIAN_POINT ( 'NONE',  ( 204.8682506193380561, 275.1723083338505376, -12.18470981274732701 ) ) ;
#49202 = EDGE_CURVE ( 'NONE', #59884, #55652, #29282, .T. ) ;
#49203 = CARTESIAN_POINT ( 'NONE',  ( 61.36533069198963375, 215.4244531367911293, -4.594050593750046652 ) ) ;
#49204 = CARTESIAN_POINT ( 'NONE',  ( 74.35260113823048300, 68.48135296369000002, 11.70560402319360449 ) ) ;
#49205 = CARTESIAN_POINT ( 'NONE',  ( 191.4685399627163633, 299.0137560639802814, 7.545791216288330716 ) ) ;
#49206 = LINE ( 'NONE', #93842, #83913 ) ;
#49207 = DIRECTION ( 'NONE',  ( 0.9997524133706775507, -0.02225111142181396620, 0.000000000000000000 ) ) ;
#49208 = ORIENTED_EDGE ( 'NONE', *, *, #9625, .T. ) ;
#49209 = AXIS2_PLACEMENT_3D ( 'NONE', #17786, #49663, #95827 ) ;
#49210 = CARTESIAN_POINT ( 'NONE',  ( 73.78529867857243119, 58.81232895305485187, -15.71900575702707847 ) ) ;
#49211 = CARTESIAN_POINT ( 'NONE',  ( 199.6683510264480788, 265.5076446645038573, 0.06738290090010203015 ) ) ;
#49212 = CARTESIAN_POINT ( 'NONE',  ( 186.7782727736096433, 295.3793828959698544, 10.37790068846201841 ) ) ;
#49213 = EDGE_LOOP ( 'NONE', ( #59418, #82569, #85994, #6596, #80340, #83853, #54476, #21965 ) ) ;
#49214 = CARTESIAN_POINT ( 'NONE',  ( 152.7607425496961184, 268.9805552238780137, -15.58657372067007074 ) ) ;
#49215 = CARTESIAN_POINT ( 'NONE',  ( 68.62755322380348844, 69.49084673843516669, -4.507018638050549697 ) ) ;
#49216 = CARTESIAN_POINT ( 'NONE',  ( 207.2683629543511756, 271.6476598918739001, -6.694388351944108528 ) ) ;
#49217 = CARTESIAN_POINT ( 'NONE',  ( 192.4867975473904949, 297.2500821921321972, -13.04960750009181325 ) ) ;
#49218 = VECTOR ( 'NONE', #7413, 1000.000000000000114 ) ;
#49219 = CARTESIAN_POINT ( 'NONE',  ( 149.7162292714551199, 271.3308795146458010, 12.12826134257344357 ) ) ;
#49220 = CARTESIAN_POINT ( 'NONE',  ( 164.4494343874829099, 245.8122196953522121, 2.922779519406129456 ) ) ;
#49221 = DIRECTION ( 'NONE',  ( 0.000000000000000000, 0.000000000000000000, 1.000000000000000000 ) ) ;
#49222 = LINE ( 'NONE', #72539, #64414 ) ;
#49223 = CARTESIAN_POINT ( 'NONE',  ( 164.3545367017254364, 245.9765873086048487, -5.942639963102972267 ) ) ;
#49224 = CARTESIAN_POINT ( 'NONE',  ( 123.3675972660055749, 242.0333772461660544, 9.188101187500095079 ) ) ;
#49225 = ORIENTED_EDGE ( 'NONE', *, *, #54762, .F. ) ;
#49226 = CARTESIAN_POINT ( 'NONE',  ( 191.0478321355427624, 299.7424433957868928, -9.006798842970001218 ) ) ;
#49227 = CARTESIAN_POINT ( 'NONE',  ( 84.46936203225826034, 42.55036768791385526, 3.687038961768065448 ) ) ;
#49228 = CARTESIAN_POINT ( 'NONE',  ( 167.4785370940337543, 280.2404111755776057, -13.99786577961182665 ) ) ;
#49229 = CARTESIAN_POINT ( 'NONE',  ( 79.45058217612400142, 59.65650951519399570, -16.18060345040571590 ) ) ;
#49230 = CARTESIAN_POINT ( 'NONE',  ( 73.91967031219644468, 56.99378804825083478, 16.01627465200614964 ) ) ;
#49231 = CARTESIAN_POINT ( 'NONE',  ( 174.9088318666119619, 252.9790288038798565, 5.053753844769934389 ) ) ;
#49232 = VERTEX_POINT ( 'NONE', #61430 ) ;
#49233 = CARTESIAN_POINT ( 'NONE',  ( 80.45778748667572700, 57.56998633490270123, -16.59146305250142817 ) ) ;
#49234 = CARTESIAN_POINT ( 'NONE',  ( 154.6388284336715628, 273.3529371992580081, -13.15606555357048713 ) ) ;
#49235 = CARTESIAN_POINT ( 'NONE',  ( 183.3396530472832637, 261.1613252051864720, 9.520234298542119333 ) ) ;
#49236 = CARTESIAN_POINT ( 'NONE',  ( 165.0817809681736037, 244.7169632896033136, -1.727194264083430131 ) ) ;
#49237 = FACE_OUTER_BOUND ( 'NONE', #35967, .T. ) ;
#49238 = CARTESIAN_POINT ( 'NONE',  ( 195.2593017302202156, 263.4723950921689379, 0.8603167340095838611 ) ) ;
#49239 = CARTESIAN_POINT ( 'NONE',  ( -46.49770490450613636, 29.77544742692501245, -10.00000000000000000 ) ) ;
#49240 = CARTESIAN_POINT ( 'NONE',  ( 68.18175421089479471, 69.02745595044970628, 5.050215709098530681 ) ) ;
#49241 = CARTESIAN_POINT ( 'NONE',  ( 69.62006919151632189, 204.8768266524160140, -9.188101187500091527 ) ) ;
#49242 = CARTESIAN_POINT ( 'NONE',  ( 170.7270849433730007, 250.4993316485856099, 3.429389635961456406 ) ) ;
#49243 = CARTESIAN_POINT ( 'NONE',  ( 171.3857937658397645, 260.1551371363238445, 14.78898683988441753 ) ) ;
#49244 = CARTESIAN_POINT ( 'NONE',  ( 155.1480735223870226, 280.2009427251024363, -0.8861822022151647493 ) ) ;
#49245 = CARTESIAN_POINT ( 'NONE',  ( 170.9511032993452204, 286.1488562452602764, -7.996916569637939176 ) ) ;
#49246 = CARTESIAN_POINT ( 'NONE',  ( 159.2111180226792726, 254.8852497853115722, 16.01057445397460910 ) ) ;
#49247 = CARTESIAN_POINT ( 'NONE',  ( 157.1316430727322881, 271.7231682581081600, -14.76758205110185074 ) ) ;
#49248 = CARTESIAN_POINT ( 'NONE',  ( 114.6081111488702078, 243.6427522451419065, -10.00000000000009415 ) ) ;
#49249 = CARTESIAN_POINT ( 'NONE',  ( 77.67544480499739734, 52.83525693180617111, -15.78147281318218198 ) ) ;
#49250 = EDGE_LOOP ( 'NONE', ( #79477, #44673, #87087, #5338 ) ) ;
#49251 = EDGE_CURVE ( 'NONE', #13449, #95124, #14726, .T. ) ;
#49252 = CARTESIAN_POINT ( 'NONE',  ( 147.6947327179224487, 274.8322142526899370, 9.090449717876689206 ) ) ;
#49253 = CARTESIAN_POINT ( 'NONE',  ( -9.459049039432731121, 165.3458772461660544, 9.188101187500095079 ) ) ;
#49254 = CARTESIAN_POINT ( 'NONE',  ( 37.98264478980979675, 201.9244531367911293, -4.594050593750046652 ) ) ;
#49255 = B_SPLINE_CURVE_WITH_KNOTS ( 'NONE', 3,
 ( #23551, #8870, #54962, #1788 ),
 .UNSPECIFIED., .F., .F.,
 ( 4, 4 ),
 ( 0.03266906780946862709, 0.04161376246641813881 ),
 .UNSPECIFIED. ) ;
#49256 = FACE_OUTER_BOUND ( 'NONE', #11387, .T. ) ;
#49257 = CARTESIAN_POINT ( 'NONE',  ( 17.74301629803562719, 32.01751292744057054, 6.180339887498949913 ) ) ;
#49258 = CARTESIAN_POINT ( 'NONE',  ( 85.69655150396907572, 48.70939609366209311, 11.94995701397517784 ) ) ;
#49259 = CARTESIAN_POINT ( 'NONE',  ( 66.14445876615877751, 69.31385697677988844, 0.2434306055318663509 ) ) ;
#49260 = CARTESIAN_POINT ( 'NONE',  ( 192.4852853123542786, 292.2780683445978980, -14.34739779062837783 ) ) ;
#49261 = CARTESIAN_POINT ( 'NONE',  ( 147.1199024702499969, 275.8278494473859723, 5.224467159276165340 ) ) ;
#49262 = CARTESIAN_POINT ( 'NONE',  ( 73.75732063271028949, 55.42083462481677003, -16.58942913474808734 ) ) ;
#49264 = CARTESIAN_POINT ( 'NONE',  ( 60.91453611423501968, 212.6427522451419065, 10.00000000000009237 ) ) ;
#49263 = CARTESIAN_POINT ( 'NONE',  ( 198.1023735320433445, 277.7417427054917312, -16.33290366355920398 ) ) ;
#49265 = DIRECTION ( 'NONE',  ( 0.000000000000000000, 0.000000000000000000, 1.000000000000000000 ) ) ;
#49266 = CARTESIAN_POINT ( 'NONE',  ( 180.8189091534864588, 256.2865937343618157, 1.394926522994340612 ) ) ;
#49267 = EDGE_CURVE ( 'NONE', #41296, #31700, #55795, .T. ) ;
#49268 = CARTESIAN_POINT ( 'NONE',  ( 157.2777284163744582, 258.2339788142568864, -16.82360006463426316 ) ) ;
#49269 = CARTESIAN_POINT ( 'NONE',  ( 88.45958475239287111, 43.85926912372239173, -0.5941283661710181629 ) ) ;
#49270 = EDGE_CURVE ( 'NONE', #59009, #47394, #26922, .T. ) ;
#49271 = CARTESIAN_POINT ( 'NONE',  ( 46.85966550219804816, 187.8615022471902023, 5.000000000000051514 ) ) ;
#49272 = CARTESIAN_POINT ( 'NONE',  ( 202.7599932440484451, 279.4563852894229967, 15.58249343055423353 ) ) ;
#49273 = CARTESIAN_POINT ( 'NONE',  ( 4.992576338337581632, 179.8149278399160949, -9.188101187500095079 ) ) ;
#49274 = CARTESIAN_POINT ( 'NONE',  ( 35.70653501523218409, 32.56628583063843507, 9.188101187500006262 ) ) ;
#49275 = CARTESIAN_POINT ( 'NONE',  ( 164.3408556225676875, 252.5018482456856646, 13.48875141561916635 ) ) ;
#49276 = CYLINDRICAL_SURFACE ( 'NONE', #84067, 10.00000000000001066 ) ;
#49277 = CARTESIAN_POINT ( 'NONE',  ( 27.52682148520507965, 37.93396525600392266, 2.839279412974139660 ) ) ;
#49278 = CARTESIAN_POINT ( 'NONE',  ( 206.5571822944673670, 272.8794609281530938, 10.95833005210827515 ) ) ;
#49279 = VECTOR ( 'NONE', #80893, 1000.000000000000000 ) ;
#49280 = CARTESIAN_POINT ( 'NONE',  ( -2.590881078880516331, 25.17631125121047475, 10.00000000000000000 ) ) ;
#49281 = CARTESIAN_POINT ( 'NONE',  ( 80.76024885531072073, 43.13123959331257851, -9.841151695238801622 ) ) ;
#49282 = CARTESIAN_POINT ( 'NONE',  ( 148.9194629746633893, 272.7109192224475009, -12.27648025871169679 ) ) ;
#49283 = FACE_OUTER_BOUND ( 'NONE', #5475, .T. ) ;
#49284 = CARTESIAN_POINT ( 'NONE',  ( 4.685401460390529849, 24.74646525600388003, 2.839279412974139660 ) ) ;
#49285 = CARTESIAN_POINT ( 'NONE',  ( 167.6610723016181623, 288.0491441363175227, 0.5383436845847213714 ) ) ;
#49286 = CARTESIAN_POINT ( 'NONE',  ( 10.40777469057294091, 26.98502408145591502, -5.678558825948271327 ) ) ;
#49287 = CARTESIAN_POINT ( 'NONE',  ( 71.97440221194672461, 212.3615022471902591, -10.00000000000009592 ) ) ;
#49288 = CARTESIAN_POINT ( 'NONE',  ( -27.77457187288642615, 24.79904599702366852, -10.00000000000000000 ) ) ;
#49289 = CARTESIAN_POINT ( 'NONE',  ( 84.46699969863880142, 49.90279977532637901, -13.71381277893580197 ) ) ;
#49290 = CARTESIAN_POINT ( 'NONE',  ( -22.42236680055709641, 157.8615022471902591, 0.000000000000000000 ) ) ;
#49291 = VERTEX_POINT ( 'NONE', #32025 ) ;
#49292 = CARTESIAN_POINT ( 'NONE',  ( 152.8036029408733043, 266.6878101728642037, 15.84078619445996416 ) ) ;
#49293 = CARTESIAN_POINT ( 'NONE',  ( 165.0387478276132072, 244.7914988754632191, -2.473354058663827626 ) ) ;
#49294 = CARTESIAN_POINT ( 'NONE',  ( 66.07429888242232607, 68.52750538357182108, 4.592745147667558037 ) ) ;
#49295 = CARTESIAN_POINT ( 'NONE',  ( 121.3378502276597288, 240.8615022471902591, -10.00000000000009592 ) ) ;
#49296 = CARTESIAN_POINT ( 'NONE',  ( 154.8989000222956349, 262.3542304552891551, 17.41779271305265908 ) ) ;
#49297 = VERTEX_POINT ( 'NONE', #16834 ) ;
#49298 =( BOUNDED_CURVE ( )  B_SPLINE_CURVE ( 2, ( #54177, #8607, #93235, #23794, #76518, #38488, #54678, #76994, #69404 ),
 .UNSPECIFIED., .F., .T. ) 
 B_SPLINE_CURVE_WITH_KNOTS ( ( 3, 2, 2, 2, 3 ),
 ( 0.2379032258064516236, 0.2392473118279569988, 0.2419354838709677491, 0.2446236559139784994, 0.2459677419354838745 ),
 .UNSPECIFIED. ) 
 CURVE ( )  GEOMETRIC_REPRESENTATION_ITEM ( )  RATIONAL_B_SPLINE_CURVE ( ( 0.9330127018922194093, 0.9330127018922194093, 1.000000000000000000, 0.8660254037844387076, 1.000000000000000000, 0.8660254037844387076, 1.000000000000000000, 0.9330127018922194093, 0.9330127018922194093 ) ) 
 REPRESENTATION_ITEM ( '' )  );
#49299 = ORIENTED_EDGE ( 'NONE', *, *, #6057, .F. ) ;
#49300 = EDGE_CURVE ( 'NONE', #68396, #34443, #78155, .T. ) ;
#49301 = CARTESIAN_POINT ( 'NONE',  ( 156.0175100402996407, 276.9512441243991248, -10.19015957619274459 ) ) ;
#49302 = CARTESIAN_POINT ( 'NONE',  ( 86.10592739760618031, 47.67974530001434630, 10.86095660826619813 ) ) ;
#49303 = EDGE_LOOP ( 'NONE', ( #2302, #23772, #82368, #98425 ) ) ;
#49304 = CARTESIAN_POINT ( 'NONE',  ( 78.22302278738825976, 60.67164067339659539, 15.94566782436302610 ) ) ;
#49305 = PLANE ( 'NONE',  #62958 ) ;
#49306 = VERTEX_POINT ( 'NONE', #62934 ) ;
#49307 = CARTESIAN_POINT ( 'NONE',  ( 79.35772302032123093, 59.09242961143867490, -16.22768995670567094 ) ) ;
#49308 = EDGE_CURVE ( 'NONE', #28514, #72111, #87322, .T. ) ;
#49309 = CARTESIAN_POINT ( 'NONE',  ( 80.75624902194448396, 43.07755972626095087, 9.780254146993412334 ) ) ;
#49310 = EDGE_LOOP ( 'NONE', ( #89155, #16405, #39783, #14285 ) ) ;
#49311 = CARTESIAN_POINT ( 'NONE',  ( 173.8168395337300467, 267.3393752366870331, 16.65285229048275184 ) ) ;
#49312 = CARTESIAN_POINT ( 'NONE',  ( 166.2812625422909889, 273.7011810638111342, -15.92596022500507580 ) ) ;
#49313 = CARTESIAN_POINT ( 'NONE',  ( 73.43553217956821300, 58.62768804998614769, 15.70915590920282945 ) ) ;
#49314 = ORIENTED_EDGE ( 'NONE', *, *, #63793, .F. ) ;
#49315 = EDGE_CURVE ( 'NONE', #81256, #34660, #21989, .T. ) ;
#49316 = CARTESIAN_POINT ( 'NONE',  ( 202.9093905060991005, 279.1976216410395182, 16.97070083370504179 ) ) ;
#49317 = ORIENTED_EDGE ( 'NONE', *, *, #10255, .T. ) ;
#49318 = EDGE_LOOP ( 'NONE', ( #34333, #5432, #46062, #82971 ) ) ;
#49319 = CARTESIAN_POINT ( 'NONE',  ( 160.3677668160452470, 268.8712655723239777, -16.73982956207869677 ) ) ;
#49320 = ORIENTED_EDGE ( 'NONE', *, *, #27017, .T. ) ;
#49321 = CARTESIAN_POINT ( 'NONE',  ( 161.0570922196022536, 271.1543799210750763, 16.37266413406176824 ) ) ;
#49322 = ORIENTED_EDGE ( 'NONE', *, *, #87113, .T. ) ;
#49323 = B_SPLINE_CURVE_WITH_KNOTS ( 'NONE', 3,
 ( #42675, #72630, #3232, #58866 ),
 .UNSPECIFIED., .F., .F.,
 ( 4, 4 ),
 ( 0.000000000000000000, 0.006095114798927191331 ),
 .UNSPECIFIED. ) ;
#49324 = DIRECTION ( 'NONE',  ( -0.1378186779084930869, 0.2387089523694814197, -0.9612616959383223358 ) ) ;
#49325 = CARTESIAN_POINT ( 'NONE',  ( 166.1760138177199622, 271.4483423397350066, 16.23974600030056337 ) ) ;
#49326 = CARTESIAN_POINT ( 'NONE',  ( 147.2962480419287772, 275.5224099575481773, 5.989900301663943161 ) ) ;
#49327 = CARTESIAN_POINT ( 'NONE',  ( 180.2055717995544910, 290.9255621863335932, -9.559994083472554749 ) ) ;
#49328 = CARTESIAN_POINT ( 'NONE',  ( 69.55475657562975300, 65.34938856974197563, 11.35858988098566513 ) ) ;
#49329 = DIRECTION ( 'NONE',  ( -0.000000000000000000, -1.000000000000000000, -0.000000000000000000 ) ) ;
#49330 = LINE ( 'NONE', #53779, #4676 ) ;
#49331 = CARTESIAN_POINT ( 'NONE',  ( 191.0862225170008628, 299.6759493045793192, -9.402218231374108726 ) ) ;
#49332 = VERTEX_POINT ( 'NONE', #24443 ) ;
#49333 = CARTESIAN_POINT ( 'NONE',  ( 18.13223351794271565, 28.65586893147756342, -7.433330006724137462 ) ) ;
#49334 = CARTESIAN_POINT ( 'NONE',  ( 164.5648480107187197, 245.6123174360222094, 3.015887571020871238 ) ) ;
#49336 = CARTESIAN_POINT ( 'NONE',  ( 164.2801755739368446, 246.1053845600426087, 2.518777461081745717 ) ) ;
#49335 = CARTESIAN_POINT ( 'NONE',  ( 77.38371485743755329, 49.76092087919086282, -14.99339166432857162 ) ) ;
#49338 = VERTEX_POINT ( 'NONE', #1661 ) ;
#49337 = DIRECTION ( 'NONE',  ( -0.2502735827033041316, -0.9681751565707789053, 0.000000000000000000 ) ) ;
#49339 = ORIENTED_EDGE ( 'NONE', *, *, #6733, .T. ) ;
#49340 = CARTESIAN_POINT ( 'NONE',  ( -55.56624327025929944, 44.99999999999998579, -59.99999999999999289 ) ) ;
#49341 = CARTESIAN_POINT ( 'NONE',  ( 69.35253854976203058, 63.01665765323906498, 13.58811665770852350 ) ) ;
#49342 = CARTESIAN_POINT ( 'NONE',  ( -35.11898741612374408, 42.34664502445047418, 59.99999999999999289 ) ) ;
#49343 = CARTESIAN_POINT ( 'NONE',  ( 78.90549422596571105, 46.47045305960070039, 12.99985401326297563 ) ) ;
#49344 = CARTESIAN_POINT ( 'NONE',  ( 200.3414094930810165, 283.6454952284590263, 16.87912319229835489 ) ) ;
#49345 = CARTESIAN_POINT ( 'NONE',  ( 190.2621123344814293, 301.1033500117378026, -1.456161902152197651 ) ) ;
#49346 = EDGE_LOOP ( 'NONE', ( #97799, #66281, #807, #50899, #88143, #9030, #6335, #78588, #72406, #13591, #20671, #31372, #80236, #8063, #22117, #52639, #31361, #5192, #94817, #352, #59258, #11609 ) ) ;
#49347 = CYLINDRICAL_SURFACE ( 'NONE', #26810, 17.82106496071139645 ) ;
#49348 = CARTESIAN_POINT ( 'NONE',  ( 25.96864935082048831, 154.0458036431183189, 30.52142883766506998 ) ) ;
#49349 = ADVANCED_FACE ( 'NONE', ( #9763 ), #99175, .F. ) ;
#49350 = CARTESIAN_POINT ( 'NONE',  ( 28.87159617421086821, 174.1427522451417644, 1.119607411625061291E-15 ) ) ;
#49351 = CARTESIAN_POINT ( 'NONE',  ( 96.30395630197683943, 238.6589784336661637, -6.496448406907676862E-16 ) ) ;
#49352 = CARTESIAN_POINT ( 'NONE',  ( 82.57385212973971989, 41.04541115053231692, -1.138833187496895549 ) ) ;
#49353 = DIRECTION ( 'NONE',  ( -0.5169068966820336009, 0.8560416229147678191, 0.000000000000000000 ) ) ;
#49354 = CARTESIAN_POINT ( 'NONE',  ( 163.2124973040920111, 247.9546575695509887, 10.85238219581215269 ) ) ;
#49355 = CARTESIAN_POINT ( 'NONE',  ( 29.78290061743214423, 181.8768266524160140, 9.188101187500098632 ) ) ;
#49356 = CARTESIAN_POINT ( 'NONE',  ( -22.42236680055709641, 157.8615022471902591, 0.000000000000000000 ) ) ;
#49357 = ORIENTED_EDGE ( 'NONE', *, *, #22281, .T. ) ;
#49358 = ORIENTED_EDGE ( 'NONE', *, *, #88321, .F. ) ;
#49359 = CARTESIAN_POINT ( 'NONE',  ( 188.5398260611945886, 261.4740634840828761, -5.959129374122240641 ) ) ;
#49360 = CARTESIAN_POINT ( 'NONE',  ( 67.40381412284057205, 69.04098650065962772, 3.573880184651055281 ) ) ;
#49361 = CARTESIAN_POINT ( 'NONE',  ( 82.81329010676300584, 42.04495716520958126, 5.036686735886401145 ) ) ;
#49362 = FACE_OUTER_BOUND ( 'NONE', #43548, .T. ) ;
#49363 = CARTESIAN_POINT ( 'NONE',  ( 161.7767236248226084, 250.4414905302161287, -13.15904643207033153 ) ) ;
#49364 = CARTESIAN_POINT ( 'NONE',  ( 182.4502648671029874, 284.2291850766257539, 14.94454483467801609 ) ) ;
#49365 = CARTESIAN_POINT ( 'NONE',  ( 166.8938901919198088, 251.4769634964625880, 10.27092145616306595 ) ) ;
#49366 = CARTESIAN_POINT ( 'NONE',  ( 41.69040282370317385, 201.0024278399160949, -9.188101187500093303 ) ) ;
#49367 = CARTESIAN_POINT ( 'NONE',  ( 71.81202244518919997, 222.2677522451419065, -5.000000000000047962 ) ) ;
#49368 = VERTEX_POINT ( 'NONE', #82182 ) ;
#49369 = CARTESIAN_POINT ( 'NONE',  ( 83.65721968253822638, 46.40063887978691781, 10.86318306393037503 ) ) ;
#49370 = EDGE_CURVE ( 'NONE', #93959, #23594, #36426, .T. ) ;
#49371 = CARTESIAN_POINT ( 'NONE',  ( 157.9059535858343111, 282.4144519034085192, -1.690885285080969025 ) ) ;
#49372 = CARTESIAN_POINT ( 'NONE',  ( -8.782727014549898570, 174.9244531367911293, -4.594050593750046652 ) ) ;
#49373 = CARTESIAN_POINT ( 'NONE',  ( 68.50152299929102639, 64.46762139964850746, -12.23471630616243822 ) ) ;
#49374 = CARTESIAN_POINT ( 'NONE',  ( 150.8247211172754589, 269.4109153179094278, -14.37608026040300402 ) ) ;
#49375 = CARTESIAN_POINT ( 'NONE',  ( -17.42236680055705023, 149.2012482093457777, 0.000000000000000000 ) ) ;
#49376 = CARTESIAN_POINT ( 'NONE',  ( 193.1169444172380167, 296.1586357973259283, -13.13373377033755318 ) ) ;
#49377 = CARTESIAN_POINT ( 'NONE',  ( 180.2008674086625888, 256.3788900776044102, -7.862092545524210330 ) ) ;
#49378 = CARTESIAN_POINT ( 'NONE',  ( 171.6625166626804457, 279.7479999435336140, 15.02938966302312984 ) ) ;
#49379 = EDGE_CURVE ( 'NONE', #85319, #52516, #25245, .T. ) ;
#49380 = CARTESIAN_POINT ( 'NONE',  ( 146.5689048584090699, 276.7822053059436485, -0.4306668706573002492 ) ) ;
#49381 = CARTESIAN_POINT ( 'NONE',  ( 207.2824254892180704, 271.6233028670009162, 6.274396967990798046 ) ) ;
#49382 = ORIENTED_EDGE ( 'NONE', *, *, #56085, .T. ) ;
#49383 = ADVANCED_FACE ( 'NONE', ( #43619 ), #74560, .T. ) ;
#49384 = CARTESIAN_POINT ( 'NONE',  ( -7.266922234329455499, 176.6115022471903160, -5.000000000000047962 ) ) ;
#49385 = CARTESIAN_POINT ( 'NONE',  ( 7.868168403658736487, 186.8967562850346837, -4.648177544792955347E-16 ) ) ;
#49386 = CARTESIAN_POINT ( 'NONE',  ( 124.5044291563551297, 236.5643266524159856, -9.188101187500093303 ) ) ;
#49387 = CARTESIAN_POINT ( 'NONE',  ( 14.21828646722447154, 29.18502408145591431, 5.678558825948277544 ) ) ;
#49388 = DIRECTION ( 'NONE',  ( -0.000000000000000000, 0.000000000000000000, -1.000000000000000000 ) ) ;
#49389 = CARTESIAN_POINT ( 'NONE',  ( 36.76746430747500938, 51.63176190406337440, 10.00000000000000000 ) ) ;
#49391 = CARTESIAN_POINT ( 'NONE',  ( 149.3212960838965557, 247.0177522451417644, 5.000000000000051514 ) ) ;
#49390 = CARTESIAN_POINT ( 'NONE',  ( 157.6673516573649181, 257.5591315650518141, 16.79781451397666103 ) ) ;
#49392 = CARTESIAN_POINT ( 'NONE',  ( 150.2464011702103335, 270.4125948492565499, -14.58086855962074857 ) ) ;
#49393 = VERTEX_POINT ( 'NONE', #81184 ) ;
#49394 = CARTESIAN_POINT ( 'NONE',  ( 192.9033750020381603, 263.8409475788059808, -4.418838240603300882 ) ) ;
#49395 = CARTESIAN_POINT ( 'NONE',  ( 196.4242782546697015, 290.4301655533025155, -16.42402868779123537 ) ) ;
#49396 = CARTESIAN_POINT ( 'NONE',  ( 75.75493378409400691, 65.86437009324527025, -14.07593894684413804 ) ) ;
#49397 = CARTESIAN_POINT ( 'NONE',  ( 176.3882048470632071, 292.4445974135971369, -1.112347119103176407 ) ) ;
#49398 = CARTESIAN_POINT ( 'NONE',  ( 81.49529596843051138, 56.10236560196279498, -16.41626961062114987 ) ) ;
#49399 = VERTEX_POINT ( 'NONE', #66919 ) ;
#49400 = CARTESIAN_POINT ( 'NONE',  ( -71.61465314115659453, 63.06504152958490295, 45.00000000000001421 ) ) ;
#49401 = CARTESIAN_POINT ( 'NONE',  ( 182.6925099381910513, 273.1766224467805841, 17.62059484408636933 ) ) ;
#49402 = CARTESIAN_POINT ( 'NONE',  ( 165.3945084580352329, 269.6251128436156250, -16.31137091215674317 ) ) ;
#49403 = CARTESIAN_POINT ( 'NONE',  ( 196.5709421020591776, 271.0089200914278535, 12.02914684137526358 ) ) ;
#49404 = VECTOR ( 'NONE', #91324, 1000.000000000000000 ) ;
#49405 = CARTESIAN_POINT ( 'NONE',  ( 83.66191979497145326, 52.22800872522471138, -14.69070669276292662 ) ) ;
#49406 = CARTESIAN_POINT ( 'NONE',  ( 72.18714191131631708, 71.56775394826222225, -5.867817691062866103 ) ) ;
#49407 = CARTESIAN_POINT ( 'NONE',  ( 192.5712965840290849, 297.1037255674836501, 11.03742858512898906 ) ) ;
#49408 = EDGE_CURVE ( 'NONE', #34337, #85402, #60643, .T. ) ;
#49409 = CARTESIAN_POINT ( 'NONE',  ( 199.4414920144331234, 281.2339203804377235, 17.34600695621782052 ) ) ;
#49410 = CARTESIAN_POINT ( 'NONE',  ( 6.214053113703209341, 25.36126292948893024, 6.180339887498949913 ) ) ;
#49411 = CARTESIAN_POINT ( 'NONE',  ( 191.8645708310420446, 287.9879281313274646, -15.85676223221169856 ) ) ;
#49412 = VERTEX_POINT ( 'NONE', #34534 ) ;
#49413 = CARTESIAN_POINT ( 'NONE',  ( 77.95656630038031665, 61.79485276963480089, 16.07049939491896495 ) ) ;
#49414 = CARTESIAN_POINT ( 'NONE',  ( 194.7900911235093133, 293.2606606935473792, -14.66228443412922999 ) ) ;
#49415 = CARTESIAN_POINT ( 'NONE',  ( 10.58227001879649620, 188.4637435831425023, 2.679491924311251605 ) ) ;
#49417 = ORIENTED_EDGE ( 'NONE', *, *, #48859, .T. ) ;
#49416 = AXIS2_PLACEMENT_3D ( 'NONE', #27487, #66466, #5171 ) ;
#49418 = CARTESIAN_POINT ( 'NONE',  ( 139.9899443387551230, 263.1772991869740395, 1.224646799147364892E-15 ) ) ;
#49419 = DIRECTION ( 'NONE',  ( -0.8660254037844387076, -0.4999999999999998890, -0.000000000000000000 ) ) ;
#49420 = CARTESIAN_POINT ( 'NONE',  ( 151.4025156491502742, 268.4101458323662541, 14.71049357081981235 ) ) ;
#49421 = CARTESIAN_POINT ( 'NONE',  ( 76.57758696453686298, 52.46645809405062266, -15.82665826843820867 ) ) ;
#49422 = CARTESIAN_POINT ( 'NONE',  ( -13.93676304270635136, 104.6887507934693105, 43.89948692389422291 ) ) ;
#49423 = CARTESIAN_POINT ( 'NONE',  ( 203.4682009197399566, 278.2297336128146412, -15.36039508894693206 ) ) ;
#49424 = VERTEX_POINT ( 'NONE', #65433 ) ;
#49425 = CARTESIAN_POINT ( 'NONE',  ( 94.85736712102178103, 237.1199935810940929, 2.679491924311251605 ) ) ;
#49426 = VERTEX_POINT ( 'NONE', #57825 ) ;
#49427 = CARTESIAN_POINT ( 'NONE',  ( 193.4652038833492611, 294.2243501988812682, 14.02643700387929648 ) ) ;
#49428 = EDGE_LOOP ( 'NONE', ( #59229, #97342, #69399, #90008, #6487, #52495 ) ) ;
#49429 = LINE ( 'NONE', #25125, #49279 ) ;
#49430 = CARTESIAN_POINT ( 'NONE',  ( 202.7676489560256528, 279.4431252073101746, -16.04062356091568020 ) ) ;
#49431 = EDGE_LOOP ( 'NONE', ( #78461, #55367, #53292, #72922 ) ) ;
#49432 = CARTESIAN_POINT ( 'NONE',  ( 184.0276249361047007, 281.0631757112061564, -16.18422146133542583 ) ) ;
#49433 = CARTESIAN_POINT ( 'NONE',  ( 82.43550774211716714, 40.72616915719758879, 3.190364828977913625 ) ) ;
#49434 = CARTESIAN_POINT ( 'NONE',  ( 147.1571408241294705, 275.7633507264765740, -6.825926678015840743 ) ) ;
#49435 = FACE_OUTER_BOUND ( 'NONE', #42416, .T. ) ;
#49436 = CARTESIAN_POINT ( 'NONE',  ( 146.8868584395697781, 276.2314935489248455, -3.891417269505058396 ) ) ;
#49437 = CARTESIAN_POINT ( 'NONE',  ( 201.4463813434794019, 281.7316278426353620, -17.16864527463587820 ) ) ;
#49438 = CARTESIAN_POINT ( 'NONE',  ( -4.294359489194460089, 63.59252496917286379, -10.00000000000000000 ) ) ;
#49439 = CARTESIAN_POINT ( 'NONE',  ( 183.5616576129386033, 284.3076914609734445, -16.02499936821387649 ) ) ;
#49440 = CARTESIAN_POINT ( 'NONE',  ( 142.3662031094091844, 246.8768266524159856, -9.188101187500091527 ) ) ;
#49441 = CARTESIAN_POINT ( 'NONE',  ( 70.41672140557730586, 61.20692221393646548, -14.84313828059261020 ) ) ;
#49442 = CARTESIAN_POINT ( 'NONE',  ( 43.88624854525928498, 27.19860640527296169, 2.839279412974134775 ) ) ;
#49443 = ADVANCED_FACE ( 'NONE', ( #19370 ), #44103, .F. ) ;
#49444 = ORIENTED_EDGE ( 'NONE', *, *, #88809, .T. ) ;
#49445 = AXIS2_PLACEMENT_3D ( 'NONE', #50949, #58061, #42345 ) ;
#49447 = ORIENTED_EDGE ( 'NONE', *, *, #42911, .T. ) ;
#49446 = CARTESIAN_POINT ( 'NONE',  ( 85.65412827366334625, 48.89905674914069067, -12.59087409094111543 ) ) ;
#49448 = CARTESIAN_POINT ( 'NONE',  ( 162.8042930031641049, 248.6616881586264469, 11.14389129512055554 ) ) ;
#49449 = CYLINDRICAL_SURFACE ( 'NONE', #36628, 60.00000000000002132 ) ;
#49450 = DIRECTION ( 'NONE',  ( -0.8660254037844387076, -0.4999999999999998890, -0.000000000000000000 ) ) ;
#49451 = CARTESIAN_POINT ( 'NONE',  ( 156.1835980877939960, 279.5352826047603685, 7.598597465648954774 ) ) ;
#49452 = CARTESIAN_POINT ( 'NONE',  ( -19.65312891409030271, 93.06504152958497400, 10.00000000000000000 ) ) ;
#49453 = CARTESIAN_POINT ( 'NONE',  ( -36.26652983198114555, 26.35523046909639788, -10.00000000000000000 ) ) ;
#49454 = CARTESIAN_POINT ( 'NONE',  ( 174.7165626157769509, 282.0434896912144040, 14.26103646697991678 ) ) ;
#49455 = CARTESIAN_POINT ( 'NONE',  ( 76.47316661484272515, 51.61210842333346704, -15.65491330287230376 ) ) ;
#49456 = CARTESIAN_POINT ( 'NONE',  ( 176.8882704868359781, 255.8434036686267348, -7.282961206419556355 ) ) ;
#49457 = ORIENTED_EDGE ( 'NONE', *, *, #72475, .F. ) ;
#49458 = CARTESIAN_POINT ( 'NONE',  ( 183.8301289239822722, 272.2411597453489662, -17.34995410509954183 ) ) ;
#49459 = CARTESIAN_POINT ( 'NONE',  ( 65.75045340966318008, 69.08842219619184277, 0.01581025732398740752 ) ) ;
#49460 = EDGE_LOOP ( 'NONE', ( #40904, #35759, #55968, #1201 ) ) ;
#49461 = LINE ( 'NONE', #71786, #85638 ) ;
#49462 = B_SPLINE_CURVE_WITH_KNOTS ( 'NONE', 3,
 ( #97104, #87027, #17559, #41850, #26661, #57545, #49961, #73270, #79407, #65649, #96606, #27168, #40834, #22039, #20568, #29157, #58539, #60028, #83888, #59021, #89992, #51446, #68136, #90504 ),
 .UNSPECIFIED., .F., .F.,
 ( 4, 2, 2, 2, 2, 2, 2, 2, 2, 2, 2, 4 ),
 ( 0.0002849336745323140284, 0.001954281156355254252, 0.002162949591583106668, 0.002267283809196996881, 0.002293367363600446775, 0.002319450918003896668, 0.002345534472407346128, 0.002371618026810796021, 0.002580286462039149773, 0.002788954897267503525, 0.003206291767724232713, 0.003623628638180961467 ),
 .UNSPECIFIED. ) ;
#49463 = CARTESIAN_POINT ( 'NONE',  ( 201.8725009077853656, 268.2699010817517546, -2.859759887887624252 ) ) ;
#49464 = CARTESIAN_POINT ( 'NONE',  ( 191.5817909860246573, 298.8175995376009837, -10.84987806275361422 ) ) ;
#49465 = CARTESIAN_POINT ( 'NONE',  ( 148.9719199701866899, 272.6200610409887872, 12.59512981512031438 ) ) ;
#49466 = CARTESIAN_POINT ( 'NONE',  ( 162.6264071486809542, 248.9697954965390920, 10.36322805486644683 ) ) ;
#49468 = CARTESIAN_POINT ( 'NONE',  ( 88.01292981757310940, 43.79437901572622849, 2.423352920943453892 ) ) ;
#49467 = LINE ( 'NONE', #96119, #20979 ) ;
#49469 = DIRECTION ( 'NONE',  ( -0.000000000000000000, -0.000000000000000000, 1.000000000000000000 ) ) ;
#49470 = VERTEX_POINT ( 'NONE', #99342 ) ;
#49471 = CARTESIAN_POINT ( 'NONE',  ( 76.63557502497172891, 60.94970092050591148, -15.67532736481255107 ) ) ;
#49472 = CARTESIAN_POINT ( 'NONE',  ( 190.2874339040999132, 273.3649718585393771, -16.54444726514628528 ) ) ;
#49473 = DIRECTION ( 'NONE',  ( -0.1548189829846212950, 0.9879428538673720173, 0.000000000000000000 ) ) ;
#49474 = AXIS2_PLACEMENT_3D ( 'NONE', #24312, #92739, #39477 ) ;
#49475 = CARTESIAN_POINT ( 'NONE',  ( 153.4578721839791342, 264.8501638863745029, 16.85421393845643223 ) ) ;
#49476 = CARTESIAN_POINT ( 'NONE',  ( 80.90448388914862221, 43.66277003455212480, -9.563369884905593921 ) ) ;
#49477 = CARTESIAN_POINT ( 'NONE',  ( -22.42236680055709641, 157.8615022471902591, 0.000000000000000000 ) ) ;
#49478 = CARTESIAN_POINT ( 'NONE',  ( 202.2576150004249200, 280.3265299319959354, 16.24828394350762295 ) ) ;
#49479 = CARTESIAN_POINT ( 'NONE',  ( 4.126898030318161936, 167.0643266524160140, 9.188101187500095079 ) ) ;
#49480 = CARTESIAN_POINT ( 'NONE',  ( 103.3950599391094443, 224.3768266524160140, -9.188101187500091527 ) ) ;
#49481 = CARTESIAN_POINT ( 'NONE',  ( 202.9881971861223917, 279.0611244672630278, -15.16231470264511927 ) ) ;
#49482 = CARTESIAN_POINT ( 'NONE',  ( 88.05604604623943032, 44.30204071979397185, -4.408624695025149087 ) ) ;
#49483 = CARTESIAN_POINT ( 'NONE',  ( 66.77752810875767864, 68.40544692769400115, 4.459354299965320401 ) ) ;
#49484 = CARTESIAN_POINT ( 'NONE',  ( 74.00414925029257063, 213.5333772461660544, 9.188101187500095079 ) ) ;
#49485 = FACE_OUTER_BOUND ( 'NONE', #36968, .T. ) ;
#49486 = CARTESIAN_POINT ( 'NONE',  ( 75.44349275752195183, 55.11585462790367984, -16.13645090372341073 ) ) ;
#49487 = CARTESIAN_POINT ( 'NONE',  ( 160.5082202113964058, 282.2950551440661684, 5.085134855888336247 ) ) ;
#49488 = CARTESIAN_POINT ( 'NONE',  ( 189.6418160314586601, 300.5678929089384042, -1.578015730609050093 ) ) ;
#49489 = CARTESIAN_POINT ( 'NONE',  ( 162.0470192796247488, 249.9733247230335280, 13.57526672572842408 ) ) ;
#49490 = CARTESIAN_POINT ( 'NONE',  ( 5.633247839328403117, 167.3927522451417929, -10.00000000000009237 ) ) ;
#49491 = EDGE_CURVE ( 'NONE', #51421, #1235, #91756, .T. ) ;
#49493 = CARTESIAN_POINT ( 'NONE',  ( 78.94459720937796021, 54.75824911672975759, -16.02467863901235390 ) ) ;
#49492 = B_SPLINE_CURVE_WITH_KNOTS ( 'NONE', 3,
 ( #89144, #3973, #35864, #58163 ),
 .UNSPECIFIED., .F., .F.,
 ( 4, 4 ),
 ( 0.006719243664021112145, 0.01482884518371295826 ),
 .UNSPECIFIED. ) ;
#49494 = CARTESIAN_POINT ( 'NONE',  ( 196.2350291401047571, 264.4780031501763347, 5.359379669934941859 ) ) ;
#49495 = ADVANCED_FACE ( 'NONE', ( #38505 ), #45603, .F. ) ;
#49497 = ADVANCED_FACE ( 'NONE', ( #75047 ), #69420, .T. ) ;
#49496 = CARTESIAN_POINT ( 'NONE',  ( 175.0296968597178306, 264.6864531019056699, -16.70299667166197466 ) ) ;
#49498 = EDGE_CURVE ( 'NONE', #59274, #72102, #86033, .T. ) ;
#49499 = CARTESIAN_POINT ( 'NONE',  ( 88.80803131805656392, 212.8923013555409796, 4.594050593750050204 ) ) ;
#49500 = CARTESIAN_POINT ( 'NONE',  ( 161.5757715694810770, 250.7895496999525449, -14.51803553215175135 ) ) ;
#49501 = CARTESIAN_POINT ( 'NONE',  ( 79.41912790878161843, 52.36421636274327085, -15.93798156132412380 ) ) ;
#49502 = CARTESIAN_POINT ( 'NONE',  ( 163.2515686412894240, 258.2197170105911823, 16.67045586147303027 ) ) ;
#49504 = CARTESIAN_POINT ( 'NONE',  ( 151.8693293926424133, 267.6016007109669204, 16.84127110976715969 ) ) ;
#49503 = DIRECTION ( 'NONE',  ( 0.06115825522547173321, -0.9981280818701455670, 0.000000000000000000 ) ) ;
#49505 = CARTESIAN_POINT ( 'NONE',  ( 173.4020954499399636, 268.3532267536930362, -16.29294589187022524 ) ) ;
#49506 = AXIS2_PLACEMENT_3D ( 'NONE', #14072, #83510, #23147 ) ;
#49507 = CARTESIAN_POINT ( 'NONE',  ( 31.10096393961467598, 36.14336893147757479, 7.433330006724141015 ) ) ;
#49508 = DIRECTION ( 'NONE',  ( 0.000000000000000000, 1.000000000000000000, 0.000000000000000000 ) ) ;
#49509 = CARTESIAN_POINT ( 'NONE',  ( 1.663964738649697406, 171.7677522451418781, 10.00000000000009592 ) ) ;
#49510 = ORIENTED_EDGE ( 'NONE', *, *, #54624, .F. ) ;
#49511 = CARTESIAN_POINT ( 'NONE',  ( 15.40246583222295129, 30.93396525600389424, 2.839279412974139660 ) ) ;
#49512 = CARTESIAN_POINT ( 'NONE',  ( 77.06204113558260360, 224.4869531367911293, 4.594050593750046652 ) ) ;
#49513 = DIRECTION ( 'NONE',  ( -1.136724945089119250E-16, 1.968865359125295083E-16, 1.000000000000000000 ) ) ;
#49514 = CARTESIAN_POINT ( 'NONE',  ( 169.8070512275697865, 289.2548177291374714, -1.145209284012313589 ) ) ;
#49515 = CARTESIAN_POINT ( 'NONE',  ( 146.9978162861947908, 276.0393089210717790, -5.134868500856280882 ) ) ;
#49516 = CARTESIAN_POINT ( 'NONE',  ( 201.5573355828420290, 281.5394494627441304, 17.77782387441517642 ) ) ;
#49517 = AXIS2_PLACEMENT_3D ( 'NONE', #16203, #38988, #22807 ) ;
#49518 = DIRECTION ( 'NONE',  ( -0.8660254037844378194, -0.5000000000000014433, -0.000000000000000000 ) ) ;
#49519 = CARTESIAN_POINT ( 'NONE',  ( 82.56047309644807797, 54.07683023134062239, -15.52634518316282630 ) ) ;
#49520 = CARTESIAN_POINT ( 'NONE',  ( 72.27728550995250600, 71.54023409894355723, 5.041877779019897865 ) ) ;
#49521 = CARTESIAN_POINT ( 'NONE',  ( 87.45985321408362267, 44.85427673109838764, -6.610136163016259836 ) ) ;
#49522 = CARTESIAN_POINT ( 'NONE',  ( 129.1320788617196911, 245.3615022471902591, -10.00000000000009592 ) ) ;
#49523 = CARTESIAN_POINT ( 'NONE',  ( 205.3465787480556344, 274.9762877783610406, -13.79319041940166279 ) ) ;
#49524 = CARTESIAN_POINT ( 'NONE',  ( 74.87825199367567564, 53.25176599458816185, 16.52284144418170797 ) ) ;
#49525 = VERTEX_POINT ( 'NONE', #78537 ) ;
#49526 = CARTESIAN_POINT ( 'NONE',  ( 85.26933297508705323, 45.86091332672160803, 9.343335550192509942 ) ) ;
#49527 = VERTEX_POINT ( 'NONE', #39489 ) ;
#49528 = CARTESIAN_POINT ( 'NONE',  ( 163.2919429874875448, 247.8170536094679903, 9.876785378511263147 ) ) ;
#49529 = CARTESIAN_POINT ( 'NONE',  ( 48.83428215874786815, 87.09189275153327969, 10.00000000000000000 ) ) ;
#49530 = CARTESIAN_POINT ( 'NONE',  ( 72.84093999290328725, 56.97456911652175648, -16.40692799624908815 ) ) ;
#49531 = ORIENTED_EDGE ( 'NONE', *, *, #10883, .T. ) ;
#49532 = CARTESIAN_POINT ( 'NONE',  ( 77.05346401475797791, 63.67418989607284630, -14.99496270919825136 ) ) ;
#49533 = EDGE_LOOP ( 'NONE', ( #39478, #94805, #76578, #98569 ) ) ;
#49534 = CARTESIAN_POINT ( 'NONE',  ( 192.8618517578005935, 292.5118789037293254, 15.26420307798650988 ) ) ;
#49535 = CARTESIAN_POINT ( 'NONE',  ( 168.9111548808109831, 249.2523013957518572, 3.445451539549450271 ) ) ;
#49536 = CARTESIAN_POINT ( 'NONE',  ( -2.330697855141256269, 26.52822386297705393, -10.00000000000000000 ) ) ;
#49537 = CARTESIAN_POINT ( 'NONE',  ( 201.4463813434794019, 281.7316278426353620, -17.16864527463587820 ) ) ;
#49538 = VERTEX_POINT ( 'NONE', #2539 ) ;
#49539 = CARTESIAN_POINT ( 'NONE',  ( 101.3989120123781191, 240.8967562850346837, -4.648177544792955347E-16 ) ) ;
#49540 = CARTESIAN_POINT ( 'NONE',  ( 30.25658917092484756, 35.65586893147758474, -7.433330006724137462 ) ) ;
#49541 = CARTESIAN_POINT ( 'NONE',  ( 86.30977306730703447, 47.58285218899635538, -10.62438056216880611 ) ) ;
#49542 = B_SPLINE_CURVE_WITH_KNOTS ( 'NONE', 3,
 ( #58659, #29285, #28268, #42461 ),
 .UNSPECIFIED., .F., .F.,
 ( 4, 4 ),
 ( 0.0004980378164629916185, 0.005738741390616254080 ),
 .UNSPECIFIED. ) ;
#49543 = DIRECTION ( 'NONE',  ( -0.9919084036772447543, 0.1269555777209495362, 0.000000000000000000 ) ) ;
#49544 = DIRECTION ( 'NONE',  ( 1.000000000000000000, 0.000000000000000000, 2.816764622163176999E-16 ) ) ;
#49545 = ORIENTED_EDGE ( 'NONE', *, *, #50238, .T. ) ;
#49546 = ORIENTED_EDGE ( 'NONE', *, *, #72238, .T. ) ;
#49547 = CARTESIAN_POINT ( 'NONE',  ( 189.5749590748330604, 276.2698024016027034, 17.49222575591110029 ) ) ;
#49549 = CARTESIAN_POINT ( 'NONE',  ( 194.9385458806846430, 293.0035295114944347, -15.70518692812489192 ) ) ;
#49548 = CARTESIAN_POINT ( 'NONE',  ( 204.2133777088835700, 276.9390495533970693, 13.75768580338462144 ) ) ;
#49550 = LINE ( 'NONE', #26264, #62605 ) ;
#49551 = LINE ( 'NONE', #11078, #53784 ) ;
#49552 = CARTESIAN_POINT ( 'NONE',  ( 49.06003799288187395, 95.45573527953635562, -10.00000000000000000 ) ) ;
#49553 = CARTESIAN_POINT ( 'NONE',  ( 187.4971950882544434, 291.4527388498394203, -14.03054952020046287 ) ) ;
#49554 = CARTESIAN_POINT ( 'NONE',  ( 163.9664443306652970, 246.6487830133108901, 5.061536945078034755 ) ) ;
#49555 = CARTESIAN_POINT ( 'NONE',  ( 169.6143685303033521, 267.3532035066224353, 16.95358291501599268 ) ) ;
#49556 = DIRECTION ( 'NONE',  ( -0.000000000000000000, -0.000000000000000000, 1.000000000000000000 ) ) ;
#49557 = CARTESIAN_POINT ( 'NONE',  ( 94.81556191316359161, 234.7369531367911009, -4.594050593750048428 ) ) ;
#49558 = VERTEX_POINT ( 'NONE', #62808 ) ;
#49559 = LINE ( 'NONE', #11087, #46311 ) ;
#49560 = DIRECTION ( 'NONE',  ( -0.5000000000000011102, -0.8660254037844380415, 0.000000000000000000 ) ) ;
#49561 = CARTESIAN_POINT ( 'NONE',  ( -11.23413608767113026, 23.57316747377392119, 10.00000000000000000 ) ) ;
#49562 = ADVANCED_FACE ( 'NONE', ( #24323 ), #54195, .F. ) ;
#49563 = VERTEX_POINT ( 'NONE', #39994 ) ;
#49564 = ORIENTED_EDGE ( 'NONE', *, *, #31210, .T. ) ;
#49565 = CARTESIAN_POINT ( 'NONE',  ( 80.22848430713953860, 44.69384781298665388, -11.72783283579514979 ) ) ;
#49566 = CARTESIAN_POINT ( 'NONE',  ( 197.0146455733971607, 286.4246647896720219, -17.74745810526840728 ) ) ;
#49567 = CARTESIAN_POINT ( 'NONE',  ( 38.03700799836438051, 22.36477965099642518, 1.583844403245330712 ) ) ;
#49568 = CARTESIAN_POINT ( 'NONE',  ( 159.2186641046529303, 254.8721795879351646, -15.96198087403305443 ) ) ;
#49569 = CARTESIAN_POINT ( 'NONE',  ( 207.0603918771781764, 270.3690891701808141, -3.414019917217335998 ) ) ;
#49570 = CARTESIAN_POINT ( 'NONE',  ( 93.65192705076950119, 231.0024278399160949, -9.188101187500093303 ) ) ;
#49571 = VERTEX_POINT ( 'NONE', #32421 ) ;
#49572 = ORIENTED_EDGE ( 'NONE', *, *, #37989, .T. ) ;
#49573 = CARTESIAN_POINT ( 'NONE',  ( 163.3939361803663246, 247.6403962173759226, -10.78041711314006790 ) ) ;
#49574 = ORIENTED_EDGE ( 'NONE', *, *, #65804, .T. ) ;
#49575 = EDGE_CURVE ( 'NONE', #23023, #2236, #19620, .T. ) ;
#49576 = CARTESIAN_POINT ( 'NONE',  ( 31.79297225648316427, 18.75978393459166682, -1.583844403245396437 ) ) ;
#49577 = CARTESIAN_POINT ( 'NONE',  ( 153.4689407916852701, 266.8309924954582470, 16.62268559038933091 ) ) ;
#49578 = CIRCLE ( 'NONE', #88486, 70.00000000000001421 ) ;
#49580 = DIRECTION ( 'NONE',  ( -1.000000000000000000, 0.000000000000000000, 1.082076799516502080E-16 ) ) ;
#49579 = CARTESIAN_POINT ( 'NONE',  ( 132.2983106946500982, 253.3149278399160949, -9.188101187500095079 ) ) ;
#49581 = CYLINDRICAL_SURFACE ( 'NONE', #13823, 45.00000000000000000 ) ;
#49582 = CARTESIAN_POINT ( 'NONE',  ( -1.387478102835363769, 181.5530062829863596, 2.649461200531984646E-14 ) ) ;
#49584 = CARTESIAN_POINT ( 'NONE',  ( 156.8572647664473152, 258.9622432186664014, 16.97926827742052325 ) ) ;
#49583 = VECTOR ( 'NONE', #12343, 1000.000000000000114 ) ;
#49585 = CARTESIAN_POINT ( 'NONE',  ( 81.24301197013335241, 47.20210463093496145, 12.61345882853937539 ) ) ;
#49586 = DIRECTION ( 'NONE',  ( 0.000000000000000000, 0.000000000000000000, 1.000000000000000000 ) ) ;
#49587 = CARTESIAN_POINT ( 'NONE',  ( -13.11024591527734451, 6.000000000000000000, -20.00000000000000000 ) ) ;
#49588 = CARTESIAN_POINT ( 'NONE',  ( 175.3476828388916715, 283.8530321168340151, 13.26393746783803884 ) ) ;
#49589 =( BOUNDED_CURVE ( )  B_SPLINE_CURVE ( 2, ( #73159, #28025, #74657, #27552, #88402, #11370, #28518, #26550, #12344 ),
 .UNSPECIFIED., .F., .T. ) 
 B_SPLINE_CURVE_WITH_KNOTS ( ( 3, 2, 2, 2, 3 ),
 ( 0.8346774193548387455, 0.8360215053763441206, 0.8387096774193548709, 0.8413978494623656212, 0.8427419354838709964 ),
 .UNSPECIFIED. ) 
 CURVE ( )  GEOMETRIC_REPRESENTATION_ITEM ( )  RATIONAL_B_SPLINE_CURVE ( ( 0.9330127018922194093, 0.9330127018922194093, 1.000000000000000000, 0.8660254037844387076, 1.000000000000000000, 0.8660254037844387076, 1.000000000000000000, 0.9330127018922194093, 0.9330127018922194093 ) ) 
 REPRESENTATION_ITEM ( '' )  );
#49590 = AXIS2_PLACEMENT_3D ( 'NONE', #47804, #9329, #40201 ) ;
#49591 = CARTESIAN_POINT ( 'NONE',  ( 22.87549206224920084, 39.05096577487528720, -10.00000000000000000 ) ) ;
#49592 = CARTESIAN_POINT ( 'NONE',  ( 197.3270082884988881, 280.8508283618238011, -16.59807545582490818 ) ) ;
#49593 = CARTESIAN_POINT ( 'NONE',  ( 148.9284654111854422, 274.1387509264121718, 8.943080486779532379 ) ) ;
#49594 = CARTESIAN_POINT ( 'NONE',  ( 200.9110265982630779, 282.6588894614233141, 17.52479721249226685 ) ) ;
#49595 = CARTESIAN_POINT ( 'NONE',  ( 82.65284874209399391, 41.20956459249614312, 2.251177775424070937 ) ) ;
#49596 = CARTESIAN_POINT ( 'NONE',  ( 167.7287655016564258, 249.9781926236658762, 6.962022607689601017 ) ) ;
#49597 = CARTESIAN_POINT ( 'NONE',  ( 78.43012671350176390, 61.37287260322700888, 16.21548333613125692 ) ) ;
#49598 = CARTESIAN_POINT ( 'NONE',  ( 175.2034740169264069, 290.8617031373823920, -6.552222927434346644 ) ) ;
#49599 = DIRECTION ( 'NONE',  ( 1.000000000000000000, 0.000000000000000000, 0.000000000000000000 ) ) ;
#49600 = AXIS2_PLACEMENT_3D ( 'NONE', #81806, #89901, #59434 ) ;
#49601 = CIRCLE ( 'NONE', #62532, 16.82106496071157764 ) ;
#49602 = CARTESIAN_POINT ( 'NONE',  ( 73.51359153202696461, 64.16502688528564136, -13.81845228444169926 ) ) ;
#49604 = CARTESIAN_POINT ( 'NONE',  ( 196.4287751515431921, 269.1031666285815618, -12.09581130873691279 ) ) ;
#49603 = CARTESIAN_POINT ( 'NONE',  ( 180.1950043829998265, 266.5822710862183840, -14.77280089193513390 ) ) ;
#49605 = DIRECTION ( 'NONE',  ( -0.1889875038809470387, -0.9819794923402672682, 0.000000000000000000 ) ) ;
#49606 = EDGE_CURVE ( 'NONE', #2096, #89824, #12630, .T. ) ;
#49607 = CARTESIAN_POINT ( 'NONE',  ( 33.07613030564196777, 37.83478043621391151, -8.090169943749479842 ) ) ;
#49608 = CARTESIAN_POINT ( 'NONE',  ( 43.53831125515428369, 65.97156238185917232, -10.00000000000000000 ) ) ;
#49609 = DIRECTION ( 'NONE',  ( 0.4999999999999992784, -0.8660254037844390407, 0.000000000000000000 ) ) ;
#49610 = CARTESIAN_POINT ( 'NONE',  ( 183.7008669673737700, 274.9450795675618338, 16.36284127036905289 ) ) ;
#49611 = CARTESIAN_POINT ( 'NONE',  ( 34.14357333472769085, 43.21091486745863364, 7.012934429366973338E-14 ) ) ;
#49612 = CIRCLE ( 'NONE', #44750, 9.212605237762131694 ) ;
#49613 = CARTESIAN_POINT ( 'NONE',  ( 52.35966550219797000, 188.3352228055615285, 4.537668576076727938E-14 ) ) ;
#49614 = CARTESIAN_POINT ( 'NONE',  ( 19.44454881187291662, 182.0333772461660544, 9.188101187500095079 ) ) ;
#49615 = DIRECTION ( 'NONE',  ( -1.000000000000000000, 0.000000000000000000, 0.000000000000000000 ) ) ;
#49616 = ORIENTED_EDGE ( 'NONE', *, *, #62643, .T. ) ;
#49617 = EDGE_CURVE ( 'NONE', #91729, #44705, #67844, .T. ) ;
#49618 = CARTESIAN_POINT ( 'NONE',  ( 86.65718700450617007, 46.39925006966746679, 9.083952274210956190 ) ) ;
#49619 = CARTESIAN_POINT ( 'NONE',  ( 17.08077532425043543, 25.56454794089041371, 10.00000000000000355 ) ) ;
#49620 = CARTESIAN_POINT ( 'NONE',  ( 82.00684797933710968, 41.19628710175830832, 5.481709446181254997 ) ) ;
#49621 = CARTESIAN_POINT ( 'NONE',  ( 34.43744006700849525, 196.8149278399161233, 9.188101187500093303 ) ) ;
#49622 = CARTESIAN_POINT ( 'NONE',  ( 87.37955803993382631, 45.91052472906853410, 8.478299845497456744 ) ) ;
#49623 = CARTESIAN_POINT ( 'NONE',  ( 190.8545714895799392, 300.0771806536980648, -5.516553996882049837 ) ) ;
#49624 = CARTESIAN_POINT ( 'NONE',  ( 37.84453522905105416, 33.80066082961425167, 10.00000000000000533 ) ) ;
#49625 = CARTESIAN_POINT ( 'NONE',  ( 180.2734563701938555, 292.7663661626478415, 6.129196057519468610 ) ) ;
#49626 = CARTESIAN_POINT ( 'NONE',  ( 191.0481192767711036, 299.7419460525905492, -9.103377665618040737 ) ) ;
#49627 = CARTESIAN_POINT ( 'NONE',  ( 181.8559320684326224, 273.7276056269956257, 17.73031764801637067 ) ) ;
#49628 = CARTESIAN_POINT ( 'NONE',  ( 163.1700791268402497, 270.5728986487383168, 17.16554465343218894 ) ) ;
#49629 = LINE ( 'NONE', #72965, #64633 ) ;
#49630 = ADVANCED_FACE ( 'NONE', ( #74441 ), #49125, .F. ) ;
#49631 = CARTESIAN_POINT ( 'NONE',  ( 81.06766895168337328, 207.6115022471902023, -5.000000000000041744 ) ) ;
#49632 = DIRECTION ( 'NONE',  ( -0.8660254037844379305, -0.5000000000000014433, -0.000000000000000000 ) ) ;
#49633 = CARTESIAN_POINT ( 'NONE',  ( 32.66923259237032084, 34.56454794089044213, 10.00000000000000355 ) ) ;
#49634 = CARTESIAN_POINT ( 'NONE',  ( 35.49282175392953320, 200.4869531367911293, 4.594050593750046652 ) ) ;
#49635 = ORIENTED_EDGE ( 'NONE', *, *, #28639, .T. ) ;
#49636 = CARTESIAN_POINT ( 'NONE',  ( -14.79927404260907231, 84.62610232342093752, 15.00661255959723483 ) ) ;
#49637 = CARTESIAN_POINT ( 'NONE',  ( 198.4344074287054696, 286.9485196940960918, -17.83642855442570152 ) ) ;
#49638 = DIRECTION ( 'NONE',  ( 0.8660254037844382635, 0.5000000000000005551, 0.000000000000000000 ) ) ;
#49639 = ORIENTED_EDGE ( 'NONE', *, *, #3307, .T. ) ;
#49640 = CARTESIAN_POINT ( 'NONE',  ( 170.8054577101068219, 287.4915981561377976, 8.526299399445241178 ) ) ;
#49641 = CARTESIAN_POINT ( 'NONE',  ( 164.4440639631384045, 245.8215215431751233, -2.910115319305802029 ) ) ;
#49642 = CARTESIAN_POINT ( 'NONE',  ( 193.4301016519987400, 295.6162315559625426, 13.49693599934615662 ) ) ;
#49643 = CARTESIAN_POINT ( 'NONE',  ( 31.98500480842837490, 19.26216523072496400, -2.296566073217252530E-15 ) ) ;
#49644 = DIRECTION ( 'NONE',  ( 3.755686162884237478E-16, 3.302728788975889054E-33, -1.000000000000000000 ) ) ;
#49645 = CARTESIAN_POINT ( 'NONE',  ( 86.41573892179229688, 47.05171444917584012, -10.02785938301615687 ) ) ;
#49646 = AXIS2_PLACEMENT_3D ( 'NONE', #9588, #39940, #8575 ) ;
#49647 = CARTESIAN_POINT ( 'NONE',  ( 171.3689516288318089, 255.6897779434656002, 12.22461471063935257 ) ) ;
#49648 = VERTEX_POINT ( 'NONE', #25839 ) ;
#49649 = CIRCLE ( 'NONE', #31853, 7.499999999999996447 ) ;
#49650 = CARTESIAN_POINT ( 'NONE',  ( 20.49695707787433463, 14.76004757982089188, 5.678558825948272215 ) ) ;
#49651 = DIRECTION ( 'NONE',  ( 0.3535533905932792265, -0.6123724356958031301, 0.7071067811865374697 ) ) ;
#49652 = CARTESIAN_POINT ( 'NONE',  ( 20.01287798488040437, 182.3615022471902591, -10.00000000000009592 ) ) ;
#49653 = CARTESIAN_POINT ( 'NONE',  ( 166.1070111784138703, 253.4115428555481344, -13.60050710122670559 ) ) ;
#49654 = ORIENTED_EDGE ( 'NONE', *, *, #93833, .T. ) ;
#49655 = CARTESIAN_POINT ( 'NONE',  ( 72.18714191131631708, 71.56775394826222225, -5.867817691062866103 ) ) ;
#49656 = CARTESIAN_POINT ( 'NONE',  ( 191.4941427383744781, 298.9694107557253346, 8.584406880462095657 ) ) ;
#49657 = DIRECTION ( 'NONE',  ( -0.9053220668578555452, -0.4247257412262889220, 0.000000000000000000 ) ) ;
#49658 = CARTESIAN_POINT ( 'NONE',  ( 32.61785165683025411, 46.50599740114042646, 177.5919119679930134 ) ) ;
#49659 = VERTEX_POINT ( 'NONE', #10630 ) ;
#49660 = ORIENTED_EDGE ( 'NONE', *, *, #26528, .F. ) ;
#49661 = AXIS2_PLACEMENT_3D ( 'NONE', #1866, #1368, #17557 ) ;
#49663 = DIRECTION ( 'NONE',  ( -0.000000000000000000, -0.000000000000000000, -1.000000000000000000 ) ) ;
#49662 = CARTESIAN_POINT ( 'NONE',  ( 207.2707369601997982, 271.6435479931266173, -5.381413637561199614 ) ) ;
#49664 = LINE ( 'NONE', #51153, #88584 ) ;
#49666 = ORIENTED_EDGE ( 'NONE', *, *, #93127, .F. ) ;
#49665 = CIRCLE ( 'NONE', #55324, 17.82106496071138224 ) ;
#49667 = CARTESIAN_POINT ( 'NONE',  ( 152.9607371460978129, 265.7112270302071124, -16.17698032818104537 ) ) ;
#49668 = CARTESIAN_POINT ( 'NONE',  ( 159.4889735931715222, 254.4039898200529706, 16.88104032092801887 ) ) ;
#49669 = CARTESIAN_POINT ( 'NONE',  ( 72.71298963066548993, 57.56606450374060557, -16.30620737163571476 ) ) ;
#49670 = CARTESIAN_POINT ( 'NONE',  ( 78.21587680839553514, 61.74396432438783222, -15.75068414206376843 ) ) ;
#49671 = CARTESIAN_POINT ( 'NONE',  ( 204.6149525604204769, 276.2435015074934199, -13.22810747389629960 ) ) ;
#49672 = CARTESIAN_POINT ( 'NONE',  ( 111.5140480995885639, 229.0643266524159856, -9.188101187500093303 ) ) ;
#49673 = CARTESIAN_POINT ( 'NONE',  ( 183.5953950971229744, 289.9057545191589043, -13.74357891376704544 ) ) ;
#49674 = EDGE_CURVE ( 'NONE', #52768, #26530, #14613, .T. ) ;
#49675 = ORIENTED_EDGE ( 'NONE', *, *, #88875, .T. ) ;
#49676 = AXIS2_PLACEMENT_3D ( 'NONE', #33779, #81397, #66645 ) ;
#49677 = CARTESIAN_POINT ( 'NONE',  ( 207.6590484093196096, 270.9709728340903894, 3.402057849327809524 ) ) ;
#49678 = VERTEX_POINT ( 'NONE', #28299 ) ;
#49679 = CARTESIAN_POINT ( 'NONE',  ( 35.22902474502244274, 28.84335787977765619, 9.188101187500006262 ) ) ;
#49680 = FACE_BOUND ( 'NONE', #26041, .T. ) ;
#49681 = CARTESIAN_POINT ( 'NONE',  ( 66.36121846479309738, 69.42315429199126697, -0.9703253544482470794 ) ) ;
#49682 = EDGE_CURVE ( 'NONE', #14203, #53284, #82566, .T. ) ;
#49683 = CARTESIAN_POINT ( 'NONE',  ( 65.07308872588301085, 214.5024278399160949, -9.188101187500093303 ) ) ;
#49684 = CARTESIAN_POINT ( 'NONE',  ( 73.76584831522593788, 68.38082682530667000, 10.99424229391076402 ) ) ;
#49685 = CARTESIAN_POINT ( 'NONE',  ( 151.0099717111976076, 269.0900518771037468, 15.84752309685681659 ) ) ;
#49686 = CARTESIAN_POINT ( 'NONE',  ( 150.5824154016292198, 269.8306011283729617, 15.30661888403989046 ) ) ;
#49687 = B_SPLINE_CURVE_WITH_KNOTS ( 'NONE', 3,
 ( #5298, #81833, #90940, #90444, #75207, #20508, #98512, #51896, #66593, #37180, #73705, #67580, #88974, #21015, #75700, #28583, #6287, #21491, #89930, #43776, #5784, #50389, #27109, #52381, #58958, #74222, #57993, #35187, #19529, #97043, #81341, #12410, #36177, #11915, #42771, #51383, #98003, #44277, #59462, #82837, #58477, #13406, #89450, #50885, #4811, #99500, #14872, #54869, #14391, #45761 ),
 .UNSPECIFIED., .F., .F.,
 ( 4, 2, 2, 2, 2, 2, 2, 2, 2, 2, 2, 2, 2, 2, 2, 2, 2, 2, 2, 2, 2, 2, 2, 2, 4 ),
 ( 0.0002878354312401214233, 0.0007598946772537885311, 0.001231953923267455585, 0.001467983546274291388, 0.001585998357777737696, 0.001704013169281184438, 0.001822027980784630746, 0.001940042792288077488, 0.002176072415294993522, 0.002648131661308826025, 0.003120190907322658094, 0.004064309399350322233, 0.005008427891377987239, 0.005480487137391740378, 0.005716516760398653377, 0.005834531571902066074, 0.005952546383405478772, 0.006011553789157129610, 0.006070561194908782182, 0.006188576006412259065, 0.006424605629419186809, 0.006896664875433114288, 0.007368724121447040899, 0.007604753744453974715, 0.007840783367460907663 ),
 .UNSPECIFIED. ) ;
#49688 = ORIENTED_EDGE ( 'NONE', *, *, #70437, .T. ) ;
#49689 = CARTESIAN_POINT ( 'NONE',  ( 78.87565597274867457, 57.06976691274630298, -16.20268086563066845 ) ) ;
#49690 = CIRCLE ( 'NONE', #85388, 70.00000000000001421 ) ;
#49691 = CARTESIAN_POINT ( 'NONE',  ( 83.98748035737914108, 42.88667253378446986, -5.474467086385531367 ) ) ;
#49692 = CARTESIAN_POINT ( 'NONE',  ( 78.14496247000307960, 54.23761980304868047, 16.42853692188513293 ) ) ;
#49693 = ORIENTED_EDGE ( 'NONE', *, *, #67444, .T. ) ;
#49694 = CARTESIAN_POINT ( 'NONE',  ( 172.3726553231756498, 259.9039163444838891, -13.86549437502850779 ) ) ;
#49695 = CARTESIAN_POINT ( 'NONE',  ( 68.13387999444950083, 69.36173196781918193, -3.979686392102562920 ) ) ;
#49696 = ADVANCED_FACE ( 'NONE', ( #99220 ), #68410, .T. ) ;
#49697 = CYLINDRICAL_SURFACE ( 'NONE', #82320, 10.00000000000001066 ) ;
#49698 = CARTESIAN_POINT ( 'NONE',  ( 207.1875246860671211, 270.9789124136162854, 2.454475744023529415 ) ) ;
#49699 = CARTESIAN_POINT ( 'NONE',  ( 149.4539134692060145, 271.7852238117696402, 12.95627816374690688 ) ) ;
#49700 = CARTESIAN_POINT ( 'NONE',  ( 31.25085430583858681, 200.3967562850347122, -4.648177544792955347E-16 ) ) ;
#49701 = CARTESIAN_POINT ( 'NONE',  ( 152.4039861250167576, 270.1776706740954523, -14.65162667463488511 ) ) ;
#49702 = DIRECTION ( 'NONE',  ( -0.7751245550734549017, -0.6318084552474576565, 0.000000000000000000 ) ) ;
#49703 = CARTESIAN_POINT ( 'NONE',  ( 164.2776907674634970, 254.2239456688865573, 14.24022417734382451 ) ) ;
#49704 = VERTEX_POINT ( 'NONE', #69794 ) ;
#49705 = CARTESIAN_POINT ( 'NONE',  ( 208.2555382576270233, 269.9378221106229034, 3.215405476967123199 ) ) ;
#49706 = CARTESIAN_POINT ( 'NONE',  ( 124.1257165900819359, 230.2202760586659736, -5.415160957724236172E-17 ) ) ;
#49707 = VERTEX_POINT ( 'NONE', #32795 ) ;
#49708 = CARTESIAN_POINT ( 'NONE',  ( 82.28868876057151738, 44.23413057205505794, -9.339634112966722412 ) ) ;
#49709 = CARTESIAN_POINT ( 'NONE',  ( 198.2505066714982149, 285.2670451491296149, 0.000000000000000000 ) ) ;
#49710 = CARTESIAN_POINT ( 'NONE',  ( 174.2379957965557651, 251.2590728793752248, 3.639292605338433795 ) ) ;
#49711 = ADVANCED_FACE ( 'NONE', ( #24205 ), #77917, .T. ) ;
#49712 = CARTESIAN_POINT ( 'NONE',  ( 163.8990931530087494, 246.7654386749614162, 5.873176884778091633 ) ) ;
#49713 = CARTESIAN_POINT ( 'NONE',  ( 0.09429369783835704621, 160.8615022471902023, 5.000000000000051514 ) ) ;
#49714 = CARTESIAN_POINT ( 'NONE',  ( 76.14472760179803856, 51.53489781101264100, -15.67783219047871235 ) ) ;
#49715 = ORIENTED_EDGE ( 'NONE', *, *, #12523, .F. ) ;
#49716 = CARTESIAN_POINT ( 'NONE',  ( 80.29526846451028632, 57.41841621455482425, -16.58920233904881414 ) ) ;
#49717 = CARTESIAN_POINT ( 'NONE',  ( 71.63453813518020752, 72.07236434383467838, 0.7172108931481352423 ) ) ;
#49719 = FACE_OUTER_BOUND ( 'NONE', #51527, .T. ) ;
#49718 = DIRECTION ( 'NONE',  ( 0.4999999999999992784, -0.8660254037844390407, 0.000000000000000000 ) ) ;
#49720 = CARTESIAN_POINT ( 'NONE',  ( 206.2880451275741223, 273.3456201754175368, -11.28869033117385534 ) ) ;
#49721 = CARTESIAN_POINT ( 'NONE',  ( 138.3604885211411215, 256.8149278399160949, 9.188101187500093303 ) ) ;
#49722 = CARTESIAN_POINT ( 'NONE',  ( 188.0737869051473012, 299.5124861214166572, -3.734995909225475863 ) ) ;
#49723 = CARTESIAN_POINT ( 'NONE',  ( 27.53018959221258655, 41.35687530090521591, -10.00000000000000000 ) ) ;
#49724 = CARTESIAN_POINT ( 'NONE',  ( 68.91580955978653833, 69.84068243732808412, 3.940511651554692740 ) ) ;
#49725 = CARTESIAN_POINT ( 'NONE',  ( 59.90443346675090908, 196.2048013555409796, 4.594050593750051981 ) ) ;
#49726 = VECTOR ( 'NONE', #70418, 1000.000000000000000 ) ;
#49727 = AXIS2_PLACEMENT_3D ( 'NONE', #76941, #30851, #61737 ) ;
#49728 = CARTESIAN_POINT ( 'NONE',  ( 191.7653887625562561, 297.2434025333955674, 10.91538051584371338 ) ) ;
#49729 = ADVANCED_FACE ( 'NONE', ( #23682 ), #31783, .F. ) ;
#49730 = EDGE_CURVE ( 'NONE', #92719, #15908, #18830, .T. ) ;
#49731 = B_SPLINE_SURFACE_WITH_KNOTS ( 'NONE', 3, 1, ( 
 ( #19740, #18733 ),
 ( #41511, #42499 ),
 ( #81074, #10636 ),
 ( #20230, #57209 ),
 ( #4514, #66321 ),
 ( #97254, #95779 ),
 ( #26332, #87702 ),
 ( #95283, #50605 ),
 ( #3545, #35908 ),
 ( #34422, #19255 ),
 ( #12127, #81559 ),
 ( #51101, #73928 ),
 ( #42991, #26827 ),
 ( #50121, #82067 ),
 ( #43507, #35413 ),
 ( #49132, #33946 ),
 ( #12636, #74446 ),
 ( #65805, #88684 ),
 ( #73435, #27331 ),
 ( #27819, #5027 ),
 ( #58213, #11640 ),
 ( #64833, #88186 ),
 ( #57706, #49618 ),
 ( #80571, #65323 ),
 ( #58695, #89191 ),
 ( #96260, #25845 ),
 ( #89669, #11149 ),
 ( #18236, #42018 ),
 ( #4021, #56720 ),
 ( #80066, #72453 ),
 ( #72952, #34904 ) ),
 .UNSPECIFIED., .F., .F., .F.,
 ( 4, 3, 3, 3, 3, 3, 3, 3, 3, 3, 4 ),
 ( 2, 2 ),
 ( 0.000000000000000000, 0.1333490885032313222, 0.3007194338854242699, 0.4699862290244929963, 0.5844252810809240639, 0.6686540514502682386, 0.7354980260655500368, 0.8028463152565734617, 0.8633854507757154906, 0.9437142632667211428, 1.000000000000000000 ),
 ( 0.000000000000000000, 1.000000000000000000 ),
 .UNSPECIFIED. ) ;
#49732 = CARTESIAN_POINT ( 'NONE',  ( 22.93021583062070690, 14.20801979619928623, -3.090169943749474069 ) ) ;
#49733 = CARTESIAN_POINT ( 'NONE',  ( 190.6094661480870798, 300.5017155583701083, 4.598210453186021951 ) ) ;
#49734 = CARTESIAN_POINT ( 'NONE',  ( 155.3771721686844955, 279.7991985491945002, -1.232760055725913961 ) ) ;
#49735 = CARTESIAN_POINT ( 'NONE',  ( 172.2711439251446848, 287.1981181489559276, -8.134297672120377243 ) ) ;
#49736 = CARTESIAN_POINT ( 'NONE',  ( 155.4495868485232108, 261.4004128932040203, -18.48326470492642315 ) ) ;
#49737 = CARTESIAN_POINT ( 'NONE',  ( 149.0239636976596955, 274.5272459498808644, 9.114559754079525788 ) ) ;
#49738 = EDGE_CURVE ( 'NONE', #71254, #63287, #62996, .T. ) ;
#49739 = CARTESIAN_POINT ( 'NONE',  ( 130.3409059842875024, 259.3927522451419918, 2.944929066748280225E-16 ) ) ;
#49740 = CARTESIAN_POINT ( 'NONE',  ( 81.87873318869407058, 51.48326241843163587, -14.75192784692151626 ) ) ;
#49741 = EDGE_LOOP ( 'NONE', ( #12479, #89055, #26118, #28256 ) ) ;
#49742 = EDGE_CURVE ( 'NONE', #42808, #76499, #72206, .T. ) ;
#49743 = CARTESIAN_POINT ( 'NONE',  ( 196.3341081413628899, 290.5863447708742342, 16.12390540996472410 ) ) ;
#49744 = FACE_OUTER_BOUND ( 'NONE', #2470, .T. ) ;
#49745 = CARTESIAN_POINT ( 'NONE',  ( -8.160010933756074891, 166.0958772461660544, -9.188101187500095079 ) ) ;
#49746 = CARTESIAN_POINT ( 'NONE',  ( 33.21950506899538880, 199.1744531367911293, 4.594050593750047540 ) ) ;
#49747 = CARTESIAN_POINT ( 'NONE',  ( 177.9283168337505856, 258.7219139204152611, -10.33080451080644835 ) ) ;
#49748 = CARTESIAN_POINT ( 'NONE',  ( 19.85205661636063468, 27.16454794089041869, -10.00000000000000355 ) ) ;
#49749 = CARTESIAN_POINT ( 'NONE',  ( 67.96946636730157820, 65.22418645040922058, -10.61429169278184759 ) ) ;
#49750 = VECTOR ( 'NONE', #23398, 1000.000000000000114 ) ;
#49751 = CARTESIAN_POINT ( 'NONE',  ( 205.2941531242069857, 275.0670916224857478, -13.92605142593109058 ) ) ;
#49752 = CARTESIAN_POINT ( 'NONE',  ( 72.30049733009887802, 72.04291962484111878, -3.432230885200083126 ) ) ;
#49753 = CARTESIAN_POINT ( 'NONE',  ( 146.9376205018946848, 276.1435710778808925, 5.066564108429441937 ) ) ;
#49754 = CARTESIAN_POINT ( 'NONE',  ( 74.22542230801622054, 55.48368813609693007, -16.11996396474174631 ) ) ;
#49755 = EDGE_CURVE ( 'NONE', #23113, #37415, #38387, .T. ) ;
#49757 = CARTESIAN_POINT ( 'NONE',  ( 60.04851071045058575, 212.1427522451419065, -10.00000000000009415 ) ) ;
#49756 = CARTESIAN_POINT ( 'NONE',  ( 171.4364905295525148, 258.3445811437964608, 14.25707489073475820 ) ) ;
#49758 = CARTESIAN_POINT ( 'NONE',  ( 75.00251594304947389, 67.18370992929050090, 12.56202059610710720 ) ) ;
#49759 = CARTESIAN_POINT ( 'NONE',  ( 6.176825452568912134, 162.8262482093457777, 3.021315404115420679E-15 ) ) ;
#49760 = CARTESIAN_POINT ( 'NONE',  ( 172.7217183343613272, 250.6623360901680826, 4.659671216799099902 ) ) ;
#49761 = CARTESIAN_POINT ( 'NONE',  ( 46.06580888206229929, 190.7365022471902023, -10.00000000000009059 ) ) ;
#49762 = DIRECTION ( 'NONE',  ( -0.8660254037844387076, -0.4999999999999998890, 0.000000000000000000 ) ) ;
#49763 = CARTESIAN_POINT ( 'NONE',  ( -18.88433730096684116, 34.39435382651002726, 59.99999999999999289 ) ) ;
#49764 = CARTESIAN_POINT ( 'NONE',  ( 2.232293911657190488, 172.0958772461660544, -9.188101187500095079 ) ) ;
#49765 = CARTESIAN_POINT ( 'NONE',  ( 38.30461122658549300, 34.06628583063844928, -9.188101187500006262 ) ) ;
#49766 = CARTESIAN_POINT ( 'NONE',  ( 164.3503491577412206, 246.9192647184853797, 5.874781936951689154 ) ) ;
#49767 = CARTESIAN_POINT ( 'NONE',  ( 192.0332533962074706, 298.0356437054567778, 11.70630383928353346 ) ) ;
#49768 = CARTESIAN_POINT ( 'NONE',  ( 32.31339950491288704, 36.84336893147758474, -7.433330006724137462 ) ) ;
#49769 = CARTESIAN_POINT ( 'NONE',  ( 27.64470315295111646, 16.36477965099641452, 1.583844403245364907 ) ) ;
#49770 = CARTESIAN_POINT ( 'NONE',  ( 207.3062152119541679, 271.5820978585240368, 7.879821064966149535 ) ) ;
#49771 = CARTESIAN_POINT ( 'NONE',  ( 37.34220537994157496, 54.61056725541210710, -10.00000000000000000 ) ) ;
#49772 = CARTESIAN_POINT ( 'NONE',  ( 196.3174919959537306, 290.6151247789487684, -17.61248417473235151 ) ) ;
#49773 = CARTESIAN_POINT ( 'NONE',  ( 176.4591198490730903, 260.2994120462323622, -13.48214217372917467 ) ) ;
#49774 = DIRECTION ( 'NONE',  ( 0.000000000000000000, 0.000000000000000000, 1.000000000000000000 ) ) ;
#49775 = CARTESIAN_POINT ( 'NONE',  ( 12.79414888559916719, 13.10170272979925166, -7.433330006724141015 ) ) ;
#49776 = CARTESIAN_POINT ( 'NONE',  ( 168.8659486881605858, 288.0201417398660624, 0.5198760491440675979 ) ) ;
#49777 = CARTESIAN_POINT ( 'NONE',  ( 19.43607595823839418, 14.14754757982089473, -5.678558825948275768 ) ) ;
#49778 = CARTESIAN_POINT ( 'NONE',  ( 158.9079007699492081, 259.3251291931981655, 16.70475046150345477 ) ) ;
#49779 = CARTESIAN_POINT ( 'NONE',  ( 153.1962011273530209, 277.8089822112107186, -4.949296756707812328 ) ) ;
#49780 = CARTESIAN_POINT ( 'NONE',  ( 156.6797689995629810, 276.8288829890643683, 11.48459988132798770 ) ) ;
#49781 = CARTESIAN_POINT ( 'NONE',  ( 159.2186641046529303, 254.8721795879351646, -15.96198087403305443 ) ) ;
#49782 = ORIENTED_EDGE ( 'NONE', *, *, #93081, .F. ) ;
#49783 = CARTESIAN_POINT ( 'NONE',  ( 152.6372694546979574, 266.7629011907697532, 15.66192084360741177 ) ) ;
#49784 = CARTESIAN_POINT ( 'NONE',  ( 164.5416088356626290, 245.6525688679454618, -1.463507744092769292 ) ) ;
#49785 = CARTESIAN_POINT ( 'NONE',  ( 87.50902739619012038, 45.51716134564335903, 6.992071084032383865 ) ) ;
#49786 = EDGE_LOOP ( 'NONE', ( #10098, #75736, #30648, #21861 ) ) ;
#49787 = ORIENTED_EDGE ( 'NONE', *, *, #21223, .F. ) ;
#49789 = CARTESIAN_POINT ( 'NONE',  ( -22.42236680055709641, 157.8615022471902591, 0.000000000000000000 ) ) ;
#49788 = DIRECTION ( 'NONE',  ( 0.4999999999999992784, -0.8660254037844390407, 0.000000000000000000 ) ) ;
#49790 = CARTESIAN_POINT ( 'NONE',  ( 86.32803123799460820, 47.24229282936711627, 10.81726845165080064 ) ) ;
#49791 = ORIENTED_EDGE ( 'NONE', *, *, #39597, .T. ) ;
#49792 = CARTESIAN_POINT ( 'NONE',  ( 77.34314915561620296, 55.31099856840221918, 16.12525396489078844 ) ) ;
#49793 = FACE_OUTER_BOUND ( 'NONE', #48101, .T. ) ;
#49794 = VERTEX_POINT ( 'NONE', #39376 ) ;
#49795 = CARTESIAN_POINT ( 'NONE',  ( 183.6215648671697522, 257.5753772875778509, -6.308267261209747012 ) ) ;
#49796 = CARTESIAN_POINT ( 'NONE',  ( 81.82315253837346347, 49.37544138376473768, -13.78991541157006750 ) ) ;
#49797 = CARTESIAN_POINT ( 'NONE',  ( 197.0313051377892748, 289.3787641501790517, -17.15509075150697882 ) ) ;
#49798 = AXIS2_PLACEMENT_3D ( 'NONE', #83537, #60668, #91627 ) ;
#49799 = CARTESIAN_POINT ( 'NONE',  ( 80.49441947199758829, 43.53112923038558790, 9.691460173197548045 ) ) ;
#49800 = EDGE_CURVE ( 'NONE', #47930, #4325, #43797, .T. ) ;
#49801 = ORIENTED_EDGE ( 'NONE', *, *, #85926, .T. ) ;
#49802 = CARTESIAN_POINT ( 'NONE',  ( 200.5621507313343557, 283.2631601884785368, 16.81037192529623425 ) ) ;
#49803 = CARTESIAN_POINT ( 'NONE',  ( 169.4682171067899219, 276.3332340018203581, -15.66424579517577698 ) ) ;
#49804 = CIRCLE ( 'NONE', #41694, 17.82106496071138935 ) ;
#49805 = DIRECTION ( 'NONE',  ( -0.000000000000000000, 0.000000000000000000, 1.000000000000000000 ) ) ;
#49806 = ORIENTED_EDGE ( 'NONE', *, *, #19856, .F. ) ;
#49807 = CARTESIAN_POINT ( 'NONE',  ( 170.6915967899095676, 255.4523109143232489, -11.49442897741288760 ) ) ;
#49808 = CARTESIAN_POINT ( 'NONE',  ( 42.14088959202413776, 24.73415679381825427, -6.890680421881970419E-14 ) ) ;
#49809 = EDGE_CURVE ( 'NONE', #82431, #69980, #15582, .T. ) ;
#49810 = ORIENTED_EDGE ( 'NONE', *, *, #55817, .F. ) ;
#49811 = CARTESIAN_POINT ( 'NONE',  ( -22.42236680055709641, 157.8615022471902591, 0.000000000000000000 ) ) ;
#49812 = ORIENTED_EDGE ( 'NONE', *, *, #91875, .T. ) ;
#49813 = CARTESIAN_POINT ( 'NONE',  ( 157.5163452712333481, 268.9055778063874413, 15.60794413863430030 ) ) ;
#49814 = ORIENTED_EDGE ( 'NONE', *, *, #57378, .F. ) ;
#49815 = CIRCLE ( 'NONE', #19108, 70.00000000000001421 ) ;
#49816 = CARTESIAN_POINT ( 'NONE',  ( 168.7855823332611749, 272.8000461963538896, 15.99225062755306404 ) ) ;
#49817 = CARTESIAN_POINT ( 'NONE',  ( 147.2424361040780525, 275.6156149679597434, 7.148024958481665081 ) ) ;
#49818 = CARTESIAN_POINT ( 'NONE',  ( 177.3637675892562697, 288.7201378008653023, -9.706580938851226747 ) ) ;
#49819 = CARTESIAN_POINT ( 'NONE',  ( 70.30547663914938994, 67.08293681328960645, 10.12933801363482544 ) ) ;
#49820 = CARTESIAN_POINT ( 'NONE',  ( 193.6538297768585153, 294.3106073703939387, 13.99927879369582406 ) ) ;
#49821 = ADVANCED_FACE ( 'NONE', ( #55086 ), #1024, .F. ) ;
#49822 = CARTESIAN_POINT ( 'NONE',  ( 178.5150000607630147, 291.6227694413174163, 6.743235598791427421 ) ) ;
#49823 = CARTESIAN_POINT ( 'NONE',  ( 158.7282104597116756, 255.7216702197306404, -17.63877974206365451 ) ) ;
#49824 = VECTOR ( 'NONE', #99268, 1000.000000000000000 ) ;
#49825 = ORIENTED_EDGE ( 'NONE', *, *, #4201, .F. ) ;
#49826 = CARTESIAN_POINT ( 'NONE',  ( 92.93017357788669131, 158.0650415295850735, -36.50000000000000000 ) ) ;
#49827 = CARTESIAN_POINT ( 'NONE',  ( 27.86299091144838869, 21.80170272979927404, 7.433330006724137462 ) ) ;
#49828 = CARTESIAN_POINT ( 'NONE',  ( 205.9642072045669465, 273.9065239114831911, 10.22128930895731536 ) ) ;
#49829 = PLANE ( 'NONE',  #91997 ) ;
#49830 = CARTESIAN_POINT ( 'NONE',  ( 159.9307118030769175, 253.6388767968520881, 16.60600887889890487 ) ) ;
#49831 = EDGE_LOOP ( 'NONE', ( #83219, #32191, #59604, #87303 ) ) ;
#49832 = CARTESIAN_POINT ( 'NONE',  ( 147.0341782662149512, 275.9763281242129551, -2.570835274536595438 ) ) ;
#49833 = CARTESIAN_POINT ( 'NONE',  ( 171.5796386137203910, 259.5337856624209962, -13.92799914495203772 ) ) ;
#49834 = CARTESIAN_POINT ( 'NONE',  ( 35.83123663242427170, 44.18528772668522464, -1.583844403245329602 ) ) ;
#49835 = EDGE_CURVE ( 'NONE', #68611, #51434, #47493, .T. ) ;
#49836 = DIRECTION ( 'NONE',  ( -1.000000000000000000, 0.000000000000000000, 0.000000000000000000 ) ) ;
#49837 = EDGE_CURVE ( 'NONE', #58518, #78498, #69402, .T. ) ;
#49838 = CARTESIAN_POINT ( 'NONE',  ( 160.6711157858514412, 252.3564594805604031, -15.48854669559399078 ) ) ;
#49839 = CARTESIAN_POINT ( 'NONE',  ( 190.5061062016229698, 300.6807402371136959, -0.1226455231808365465 ) ) ;
#49840 = ORIENTED_EDGE ( 'NONE', *, *, #28666, .F. ) ;
#49841 = DIRECTION ( 'NONE',  ( 0.000000000000000000, -0.000000000000000000, 1.000000000000000000 ) ) ;
#49842 = VECTOR ( 'NONE', #82311, 1000.000000000000114 ) ;
#49843 = DIRECTION ( 'NONE',  ( -0.8660254037844387076, -0.4999999999999998890, -0.000000000000000000 ) ) ;
#49844 = CARTESIAN_POINT ( 'NONE',  ( 186.6673878995319455, 276.5074556901925007, 17.73048906045012529 ) ) ;
#49845 = CARTESIAN_POINT ( 'NONE',  ( 34.93377400070185956, 197.6427522451419065, 10.00000000000009237 ) ) ;
#49846 = CARTESIAN_POINT ( 'NONE',  ( 100.9591899430832029, 229.0958772461660260, -9.188101187500095079 ) ) ;
#49847 = CARTESIAN_POINT ( 'NONE',  ( 180.9559662842916907, 294.1923438242872066, -2.650091675432668215 ) ) ;
#49848 = CARTESIAN_POINT ( 'NONE',  ( 23.04394319889420828, 13.70852965304479554, 1.583844403245364907 ) ) ;
#49849 = CARTESIAN_POINT ( 'NONE',  ( 162.6859166034911652, 248.8667220972772611, 10.26171246773997758 ) ) ;
#49850 = CARTESIAN_POINT ( 'NONE',  ( 19.11978928545374501, 181.8458772461660544, 9.188101187500095079 ) ) ;
#49851 = CARTESIAN_POINT ( 'NONE',  ( 177.5789271328089569, 256.9092084430625960, 10.75158368189463154 ) ) ;
#49852 = EDGE_LOOP ( 'NONE', ( #17758, #38041 ) ) ;
#49853 = CARTESIAN_POINT ( 'NONE',  ( 185.1442001806119890, 259.9352252026162091, -5.714739739034400579 ) ) ;
#49854 = CARTESIAN_POINT ( 'NONE',  ( 79.60765542401018990, 47.14190884193141784, -13.17992671574433317 ) ) ;
#49855 = CARTESIAN_POINT ( 'NONE',  ( 75.97349631671795578, 51.36067909666243025, 16.15326845647728149 ) ) ;
#49856 = CARTESIAN_POINT ( 'NONE',  ( 42.25626477193290498, 60.39660150822810891, -10.00000000000000000 ) ) ;
#49857 = CARTESIAN_POINT ( 'NONE',  ( 207.1158949475991164, 271.9117422260973740, -5.823035679195911918 ) ) ;
#49858 = CARTESIAN_POINT ( 'NONE',  ( 185.6362014350900722, 286.2933592875990030, 15.44405011100975855 ) ) ;
#49859 = CARTESIAN_POINT ( 'NONE',  ( 97.33941792859064890, 238.5530062829863027, -4.648177544792955347E-16 ) ) ;
#49860 = EDGE_CURVE ( 'NONE', #78822, #97187, #25193, .T. ) ;
#49861 = CARTESIAN_POINT ( 'NONE',  ( 50.89226983467786170, 194.0643266524160140, 9.188101187500095079 ) ) ;
#49862 = CARTESIAN_POINT ( 'NONE',  ( 83.43119661263041564, 225.6427522451419065, -10.00000000000009415 ) ) ;
#49863 = AXIS2_PLACEMENT_3D ( 'NONE', #9998, #77902, #24186 ) ;
#49864 = ORIENTED_EDGE ( 'NONE', *, *, #55999, .F. ) ;
#49865 = CARTESIAN_POINT ( 'NONE',  ( 84.80172950927561715, 50.19486025153374698, 13.34007759942641336 ) ) ;
#49866 = EDGE_CURVE ( 'NONE', #79979, #81112, #48511, .T. ) ;
#49867 = CARTESIAN_POINT ( 'NONE',  ( 158.6735398351655988, 282.4669076978136104, -1.658533933206339350 ) ) ;
#49868 = CIRCLE ( 'NONE', #11063, 50.00000000000000711 ) ;
#49869 = CARTESIAN_POINT ( 'NONE',  ( -12.49048504844327745, 175.8464784336661353, 1.353441290958777327E-15 ) ) ;
#49870 = AXIS2_PLACEMENT_3D ( 'NONE', #79264, #9837, #69610 ) ;
#49871 = EDGE_CURVE ( 'NONE', #87863, #45170, #34491, .T. ) ;
#49872 = CARTESIAN_POINT ( 'NONE',  ( 68.89679659267170564, 64.71313860959173780, -12.22090107332434528 ) ) ;
#49873 = CARTESIAN_POINT ( 'NONE',  ( 151.1230807375396807, 268.8941412966845519, -14.26613110909109849 ) ) ;
#49874 = CARTESIAN_POINT ( 'NONE',  ( 79.06615046322909279, 46.00065692319815724, -12.62335963921513837 ) ) ;
#49875 = CARTESIAN_POINT ( 'NONE',  ( 192.4743214706506365, 297.2716913909250707, -12.17804856100553046 ) ) ;
#49876 = DIRECTION ( 'NONE',  ( 0.000000000000000000, -0.000000000000000000, -1.000000000000000000 ) ) ;
#49877 = CARTESIAN_POINT ( 'NONE',  ( 204.9432097630379417, 275.6749433546094679, 13.74700047688257776 ) ) ;
#49878 = CARTESIAN_POINT ( 'NONE',  ( 68.51030059680894624, 220.3615022471903160, 5.000000000000046185 ) ) ;
#49879 = CARTESIAN_POINT ( 'NONE',  ( -5.362061845104283186, 24.53938646500536436, 177.5919119679930134 ) ) ;
#49880 = EDGE_LOOP ( 'NONE', ( #44823, #78526, #87029, #85212 ) ) ;
#49881 = VECTOR ( 'NONE', #41502, 1000.000000000000114 ) ;
#49882 =( BOUNDED_CURVE ( )  B_SPLINE_CURVE ( 2, ( #56290, #87288, #92121, #51185, #45940, #58776, #50686, #11719, #22674 ),
 .UNSPECIFIED., .F., .T. ) 
 B_SPLINE_CURVE_WITH_KNOTS ( ( 3, 2, 2, 2, 3 ),
 ( 0.4233870967741935609, 0.4247311827956989361, 0.4274193548387096864, 0.4301075268817204367, 0.4314516129032258118 ),
 .UNSPECIFIED. ) 
 CURVE ( )  GEOMETRIC_REPRESENTATION_ITEM ( )  RATIONAL_B_SPLINE_CURVE ( ( 0.9330127018922194093, 0.9330127018922194093, 1.000000000000000000, 0.8660254037844387076, 1.000000000000000000, 0.8660254037844387076, 1.000000000000000000, 0.9330127018922194093, 0.9330127018922194093 ) ) 
 REPRESENTATION_ITEM ( '' )  );
#49883 = CARTESIAN_POINT ( 'NONE',  ( -5.174027508517048624, 174.4865022471902876, 10.00000000000009237 ) ) ;
#49884 = DIRECTION ( 'NONE',  ( -0.9213551052231903071, 0.3887219701524006754, 0.000000000000000000 ) ) ;
#49885 = CARTESIAN_POINT ( 'NONE',  ( 118.1714448432989144, 239.0333772461660544, 9.188101187500095079 ) ) ;
#49886 = CARTESIAN_POINT ( 'NONE',  ( 16.72494223679300873, 27.84336893147755987, -7.433330006724137462 ) ) ;
#49887 = CARTESIAN_POINT ( 'NONE',  ( 75.19340432564982279, 67.01774300492178327, 13.18884388031393229 ) ) ;
#49888 = CARTESIAN_POINT ( 'NONE',  ( -15.51451749852110495, 173.3967562850347406, 6.972266317189433612E-15 ) ) ;
#49889 = CIRCLE ( 'NONE', #54705, 70.00000000000001421 ) ;
#49891 = CARTESIAN_POINT ( 'NONE',  ( 185.6268485153956362, 288.2895463531142468, 15.19883395034924156 ) ) ;
#49890 = DIRECTION ( 'NONE',  ( 0.000000000000000000, 0.000000000000000000, 1.000000000000000000 ) ) ;
#49892 = FACE_OUTER_BOUND ( 'NONE', #45160, .T. ) ;
#49893 = ORIENTED_EDGE ( 'NONE', *, *, #92162, .F. ) ;
#49894 = CARTESIAN_POINT ( 'NONE',  ( 191.4685399627163633, 299.0137560639802814, 7.545791216288330716 ) ) ;
#49895 = CARTESIAN_POINT ( 'NONE',  ( 149.0598351764325002, 272.4677874370131576, -11.59078276432863674 ) ) ;
#49896 = CARTESIAN_POINT ( 'NONE',  ( 190.2531537072969172, 300.2272130020738246, 3.269838540422708384 ) ) ;
#49897 = CARTESIAN_POINT ( 'NONE',  ( 176.3276157809688698, 292.5524778291284065, -1.120248480450068307 ) ) ;
#49898 = CARTESIAN_POINT ( 'NONE',  ( 81.63517289312954972, 55.69097578121159131, -16.34528168754147259 ) ) ;
#49899 = VERTEX_POINT ( 'NONE', #58094 ) ;
#49900 = CARTESIAN_POINT ( 'NONE',  ( 139.9313959742916325, 240.0494855054051584, -2.679491924311248496 ) ) ;
#49901 = CARTESIAN_POINT ( 'NONE',  ( 165.6308188219810802, 269.8697111906062673, -16.28193825780852677 ) ) ;
#49902 = CARTESIAN_POINT ( 'NONE',  ( 71.83275678050461011, 72.56239119006679061, 1.040614184235704842 ) ) ;
#49903 = CARTESIAN_POINT ( 'NONE',  ( 84.68632265823056571, 43.86313539936578110, 6.734552681056144685 ) ) ;
#49904 = CARTESIAN_POINT ( 'NONE',  ( 200.2698671084199304, 272.3682649667838405, 12.72613294923287164 ) ) ;
#49905 = CARTESIAN_POINT ( 'NONE',  ( 156.0412994658168202, 261.1582083806645755, 17.21098171226111262 ) ) ;
#49906 = CARTESIAN_POINT ( 'NONE',  ( 72.03955433498997252, 71.50824183410490775, -5.808600603169774779 ) ) ;
#49907 = CARTESIAN_POINT ( 'NONE',  ( 152.9489295551198893, 265.7316783776963121, 17.71675637597311237 ) ) ;
#49908 = VECTOR ( 'NONE', #73543, 1000.000000000000000 ) ;
#49909 = ORIENTED_EDGE ( 'NONE', *, *, #58548, .T. ) ;
#49910 = CARTESIAN_POINT ( 'NONE',  ( 194.4672199338309895, 282.9685410809637460, 17.39323676395655127 ) ) ;
#49911 = CARTESIAN_POINT ( 'NONE',  ( 5.551812139918021138, 18.90829794293878408, 10.00000000000000355 ) ) ;
#49912 = CARTESIAN_POINT ( 'NONE',  ( 174.2161637736558646, 273.0081352261942698, -16.36149965205150636 ) ) ;
#49913 = ORIENTED_EDGE ( 'NONE', *, *, #12347, .F. ) ;
#49914 = CARTESIAN_POINT ( 'NONE',  ( 164.3041378677445437, 280.0744590447591804, 12.54842942910348391 ) ) ;
#49915 = ADVANCED_FACE ( 'NONE', ( #81440 ), #59279, .T. ) ;
#49916 = CARTESIAN_POINT ( 'NONE',  ( 194.2900850603946310, 294.1266965989547657, -15.88613936555681505 ) ) ;
#49917 = CARTESIAN_POINT ( 'NONE',  ( 159.7390991980013268, 264.1538480117934569, -17.57393616107441758 ) ) ;
#49918 = EDGE_LOOP ( 'NONE', ( #33166, #87744, #94855, #71388 ) ) ;
#49919 = CARTESIAN_POINT ( 'NONE',  ( 79.15819921557465477, 59.82093924937031204, 16.50069780760282256 ) ) ;
#49920 = CARTESIAN_POINT ( 'NONE',  ( -19.65312891409030271, 93.06504152958497400, 177.5919119679930134 ) ) ;
#49921 = LINE ( 'NONE', #17012, #35075 ) ;
#49922 = AXIS2_PLACEMENT_3D ( 'NONE', #14099, #13607, #60169 ) ;
#49923 = ORIENTED_EDGE ( 'NONE', *, *, #97779, .T. ) ;
#49924 = CARTESIAN_POINT ( 'NONE',  ( -63.08903959183645327, 39.77784189046417396, -10.00000000000000000 ) ) ;
#49925 = CARTESIAN_POINT ( 'NONE',  ( 84.70734284140858961, 49.82661628013787691, -13.16822936550296319 ) ) ;
#49926 = CARTESIAN_POINT ( 'NONE',  ( 185.3516594888635041, 259.5148316134143442, -6.839491391714221713 ) ) ;
#49927 = ORIENTED_EDGE ( 'NONE', *, *, #72657, .T. ) ;
#49928 = ORIENTED_EDGE ( 'NONE', *, *, #46192, .T. ) ;
#49929 = CARTESIAN_POINT ( 'NONE',  ( 179.0457787397059235, 259.9863029104557199, 12.57728703070772980 ) ) ;
#49930 = VERTEX_POINT ( 'NONE', #49494 ) ;
#49931 = CARTESIAN_POINT ( 'NONE',  ( 77.32261477357617707, 49.49473738394384270, 14.91239470638691422 ) ) ;
#49932 = ORIENTED_EDGE ( 'NONE', *, *, #72532, .T. ) ;
#49933 = CARTESIAN_POINT ( 'NONE',  ( 74.82759778890250857, 57.94603759221541850, 15.96911003232950499 ) ) ;
#49934 = CARTESIAN_POINT ( 'NONE',  ( 203.5080190724872011, 278.1607665491929993, -15.47044080916498743 ) ) ;
#49935 = ORIENTED_EDGE ( 'NONE', *, *, #46143, .T. ) ;
#49936 = B_SPLINE_CURVE_WITH_KNOTS ( 'NONE', 3,
 ( #6588, #14680, #21293, #76490 ),
 .UNSPECIFIED., .F., .F.,
 ( 4, 4 ),
 ( 0.02883180965995480252, 0.03048461901537222879 ),
 .UNSPECIFIED. ) ;
#49937 = CARTESIAN_POINT ( 'NONE',  ( 151.3011447763744570, 269.1990464485573966, 14.21186556778774168 ) ) ;
#49938 = CARTESIAN_POINT ( 'NONE',  ( 162.0143107678314607, 277.5073529415977873, -13.05376659552506347 ) ) ;
#49939 = CARTESIAN_POINT ( 'NONE',  ( 147.3715240516018810, 275.3920280842035595, -3.728968767617475866 ) ) ;
#49940 = VECTOR ( 'NONE', #97935, 999.9999999999998863 ) ;
#49941 = CARTESIAN_POINT ( 'NONE',  ( 201.2535035105529744, 282.0657020489176716, -18.08976065250591958 ) ) ;
#49942 = CARTESIAN_POINT ( 'NONE',  ( 84.63373551891548630, 42.05073026052070162, -3.462570873098485436 ) ) ;
#49943 = ADVANCED_FACE ( 'NONE', ( #73313 ), #49009, .T. ) ;
#49945 = CARTESIAN_POINT ( 'NONE',  ( 73.28532805263516536, 68.06995479673437899, -11.00005841506875370 ) ) ;
#49944 = CIRCLE ( 'NONE', #71000, 17.82106496071138935 ) ;
#49946 = CARTESIAN_POINT ( 'NONE',  ( 137.1700506867025808, 243.8768266524160140, -9.188101187500091527 ) ) ;
#49947 = CARTESIAN_POINT ( 'NONE',  ( 88.05115470054576576, 43.61122574602664059, 0.03890336903546996739 ) ) ;
#49948 = CARTESIAN_POINT ( 'NONE',  ( 6.527493107231251201, 21.95586893147753216, 7.433330006724141015 ) ) ;
#49949 = VECTOR ( 'NONE', #12209, 1000.000000000000000 ) ;
#49950 = ORIENTED_EDGE ( 'NONE', *, *, #3463, .F. ) ;
#49951 = VECTOR ( 'NONE', #71236, 1000.000000000000114 ) ;
#49953 = ORIENTED_EDGE ( 'NONE', *, *, #93081, .T. ) ;
#49952 = CARTESIAN_POINT ( 'NONE',  ( 200.0230348527707918, 270.2077458102232299, 9.270856234837108190 ) ) ;
#49954 = CARTESIAN_POINT ( 'NONE',  ( -13.91626742945881468, 104.6355682312461113, 10.45771055378636660 ) ) ;
#49955 = CARTESIAN_POINT ( 'NONE',  ( 181.4712052382458012, 255.0843802102731956, 0.8439431145092127773 ) ) ;
#49956 = CARTESIAN_POINT ( 'NONE',  ( 171.0331961513450381, 287.8115977397300753, -5.235742780808191554 ) ) ;
#49957 = CARTESIAN_POINT ( 'NONE',  ( 157.4266892601732764, 279.9775888384338600, -6.903949925214651451 ) ) ;
#49958 = EDGE_CURVE ( 'NONE', #37182, #18761, #52220, .T. ) ;
#49959 = CARTESIAN_POINT ( 'NONE',  ( 78.71005434030972481, 51.00076188309252956, -15.65772236519125826 ) ) ;
#49961 = CARTESIAN_POINT ( 'NONE',  ( 192.7136452730116787, 292.4147829832277807, -14.35829535037222549 ) ) ;
#49960 = B_SPLINE_CURVE_WITH_KNOTS ( 'NONE', 3,
 ( #29255, #28749, #83990, #44435 ),
 .UNSPECIFIED., .F., .F.,
 ( 4, 4 ),
 ( 0.000000000000000000, 0.0002315650517813498070 ),
 .UNSPECIFIED. ) ;
#49962 = EDGE_CURVE ( 'NONE', #69383, #14295, #18108, .T. ) ;
#49963 = CARTESIAN_POINT ( 'NONE',  ( 85.96821334696042527, 43.30321141303308963, 3.387204527858681313 ) ) ;
#49964 = CARTESIAN_POINT ( 'NONE',  ( 88.45040933577318754, 44.05593677119288287, -2.476488480078137933 ) ) ;
#49965 = AXIS2_PLACEMENT_3D ( 'NONE', #68237, #82513, #44438 ) ;
#49966 = ORIENTED_EDGE ( 'NONE', *, *, #8219, .F. ) ;
#49967 = CARTESIAN_POINT ( 'NONE',  ( 147.7467138384290308, 274.7421803109381813, -9.190172068879620682 ) ) ;
#49968 = CARTESIAN_POINT ( 'NONE',  ( 66.05101471070410923, 68.71202625984970780, 0.004290391756236853690 ) ) ;
#49969 = ORIENTED_EDGE ( 'NONE', *, *, #81979, .F. ) ;
#49970 = CARTESIAN_POINT ( 'NONE',  ( 163.3780808840420207, 277.4266273750775440, 12.96822648644490350 ) ) ;
#49971 = CARTESIAN_POINT ( 'NONE',  ( 156.1857201963304362, 277.6936791020598889, 10.39727624116721749 ) ) ;
#49972 = DIRECTION ( 'NONE',  ( -0.9133924323370958831, 0.1624253398589842745, 0.3732723851572966600 ) ) ;
#49973 = CARTESIAN_POINT ( 'NONE',  ( 190.4841013044967042, 300.7188538369516095, 4.682298117523464143 ) ) ;
#49974 = CARTESIAN_POINT ( 'NONE',  ( 203.0535368433499457, 278.9479528611958585, 16.46202213522710167 ) ) ;
#49976 = CARTESIAN_POINT ( 'NONE',  ( 88.42017002704760387, 43.92753743058676719, 1.721442031696310382 ) ) ;
#49975 = CARTESIAN_POINT ( 'NONE',  ( 161.2233037901852697, 281.7567412870793078, -7.606728900846287722 ) ) ;
#49977 = CIRCLE ( 'NONE', #41869, 45.00000000000000000 ) ;
#49978 = CARTESIAN_POINT ( 'NONE',  ( 161.5295548613449625, 262.2726132182542642, 17.75576853186118598 ) ) ;
#49979 = ORIENTED_EDGE ( 'NONE', *, *, #80889, .T. ) ;
#49980 = PRODUCT ( 'MAS-322', 'MAS-322', '', ( #35060 ) ) ;
#49981 = CARTESIAN_POINT ( 'NONE',  ( 74.66876074730942037, 61.62064187642321400, -15.14846027550216867 ) ) ;
#49982 = DIRECTION ( 'NONE',  ( 0.000000000000000000, 0.000000000000000000, 1.000000000000000000 ) ) ;
#49983 = DIRECTION ( 'NONE',  ( 0.2702110370271901263, 0.9515975153008180420, -0.1464519181916028867 ) ) ;
#49984 = DIRECTION ( 'NONE',  ( -0.4493970231495795775, 0.7783784768652820540, -0.4383711467890876734 ) ) ;
#49985 = CARTESIAN_POINT ( 'NONE',  ( 81.05143020228690887, 43.40825155421170223, -9.967878382272422400 ) ) ;
#49986 = PLANE ( 'NONE',  #91913 ) ;
#49987 = EDGE_CURVE ( 'NONE', #62487, #10212, #38946, .T. ) ;
#49988 = CARTESIAN_POINT ( 'NONE',  ( 9.323050453024791295, 170.0643266524160140, 9.188101187500095079 ) ) ;
#49989 = CARTESIAN_POINT ( 'NONE',  ( 113.4086522182495145, 224.0327760586659451, 1.948934522072303157E-15 ) ) ;
#49990 = CARTESIAN_POINT ( 'NONE',  ( 154.9792334219179679, 262.2150889255981951, -17.21325849938693153 ) ) ;
#49991 = CARTESIAN_POINT ( 'NONE',  ( 88.09812594050896450, 44.33653194584124435, -4.440584375772049341 ) ) ;
#49992 = CARTESIAN_POINT ( 'NONE',  ( 184.6829044896801690, 294.7002800362207608, -7.708189250272898363 ) ) ;
#49993 = DIRECTION ( 'NONE',  ( 0.5000000000000013323, -0.8660254037844378194, 0.000000000000000000 ) ) ;
#49994 = LINE ( 'NONE', #96137, #58710 ) ;
#49995 = DIRECTION ( 'NONE',  ( 1.000000000000000000, 0.000000000000000000, -5.984665299743594308E-16 ) ) ;
#49996 = CARTESIAN_POINT ( 'NONE',  ( 147.9311236323648870, 274.4227731784279172, -7.799459659034405412 ) ) ;
#49997 = CARTESIAN_POINT ( 'NONE',  ( 181.8064089908095013, 291.5401130331068771, 9.400625256126808438 ) ) ;
#49998 = EDGE_CURVE ( 'NONE', #1644, #75140, #68985, .T. ) ;
#49999 = CARTESIAN_POINT ( 'NONE',  ( 180.4232100707751840, 278.0586175385776642, -17.62785496320838519 ) ) ;
#50000 = CARTESIAN_POINT ( 'NONE',  ( 168.8221748259757931, 288.8596753763678180, 0.1258535561669744951 ) ) ;
#50001 = CARTESIAN_POINT ( 'NONE',  ( 75.59167736239344038, 55.94695640115752866, -16.15688945000958299 ) ) ;
#50002 = CARTESIAN_POINT ( 'NONE',  ( 166.1124712730374711, 253.7145057436913191, -13.29400677092769101 ) ) ;
#50003 = CARTESIAN_POINT ( 'NONE',  ( 176.1427204184975039, 265.6242702382210723, -16.01709430928111288 ) ) ;
#50004 = CIRCLE ( 'NONE', #41895, 14.99999999999968026 ) ;
#50005 = CARTESIAN_POINT ( 'NONE',  ( 87.75264963113552596, 209.2202760586659167, -5.415160957724236172E-17 ) ) ;
#50006 = CARTESIAN_POINT ( 'NONE',  ( 207.1019571622349815, 271.9358831784929293, -5.989975140547304733 ) ) ;
#50007 = CARTESIAN_POINT ( 'NONE',  ( 73.13476967714908028, 57.39438153525127007, 15.88807208273858684 ) ) ;
#50008 = CARTESIAN_POINT ( 'NONE',  ( -16.70556162152145774, 103.8144583182831298, 12.73413235864565785 ) ) ;
#50010 = CARTESIAN_POINT ( 'NONE',  ( 151.8386188729356547, 267.6547928914259842, 15.62558980430495126 ) ) ;
#50009 = LINE ( 'NONE', #94648, #53321 ) ;
#50011 = CIRCLE ( 'NONE', #11207, 4.999999999999993783 ) ;
#50012 = CARTESIAN_POINT ( 'NONE',  ( 75.94843506473843320, 65.47918399976401815, 14.33637728062728200 ) ) ;
#50013 = CARTESIAN_POINT ( 'NONE',  ( 176.4203288667277718, 270.0400164863470991, -16.69789413301970882 ) ) ;
#50014 = CARTESIAN_POINT ( 'NONE',  ( 31.70236382085744964, 33.70171378149921537, -9.188101187500004485 ) ) ;
#50015 = DIRECTION ( 'NONE',  ( 0.3693965786901518555, -0.9292718480896806632, 0.000000000000000000 ) ) ;
#50016 = CARTESIAN_POINT ( 'NONE',  ( 76.03008165241378435, 63.51276889911483181, 15.23596077392240211 ) ) ;
#50017 = ORIENTED_EDGE ( 'NONE', *, *, #59102, .F. ) ;
#50018 = CARTESIAN_POINT ( 'NONE',  ( 17.52000153575897912, 22.06628583063841020, -9.188101187500006262 ) ) ;
#50019 = CARTESIAN_POINT ( 'NONE',  ( 76.27746593522670082, 214.8458772461660544, 9.188101187500095079 ) ) ;
#50020 = CARTESIAN_POINT ( 'NONE',  ( 172.6419814482584059, 289.4122052211230880, -1.058254457564594464 ) ) ;
#50021 = CARTESIAN_POINT ( 'NONE',  ( -30.12762649812272997, 94.39323202455672401, 12.42295412654578435 ) ) ;
#50022 = CARTESIAN_POINT ( 'NONE',  ( 188.6147648084645425, 286.2025555478231809, -16.06153253298101902 ) ) ;
#50023 = CARTESIAN_POINT ( 'NONE',  ( 84.14312167556933275, 48.98415679381830756, 0.000000000000000000 ) ) ;
#50025 = EDGE_CURVE ( 'NONE', #759, #66266, #11173, .T. ) ;
#50024 = CARTESIAN_POINT ( 'NONE',  ( 193.4694490986788082, 288.4501677614762229, 16.06150681008983483 ) ) ;
#50026 = CARTESIAN_POINT ( 'NONE',  ( 72.34554419998197261, 71.56729737182827478, 5.072265668445069764 ) ) ;
#50027 = CIRCLE ( 'NONE', #6354, 0.5000000000000004441 ) ;
#50028 = CARTESIAN_POINT ( 'NONE',  ( 125.2349645446897455, 233.1115022471901739, -5.000000000000041744 ) ) ;
#50029 = FACE_BOUND ( 'NONE', #74095, .T. ) ;
#50030 = CARTESIAN_POINT ( 'NONE',  ( 19.72404941274043466, 33.16126292948895582, -6.180339887498951690 ) ) ;
#50031 = VERTEX_POINT ( 'NONE', #6880 ) ;
#50032 = CARTESIAN_POINT ( 'NONE',  ( 169.3476482064008337, 248.6764527704247882, -1.911158280328731474 ) ) ;
#50033 = ORIENTED_EDGE ( 'NONE', *, *, #74187, .T. ) ;
#50034 = CARTESIAN_POINT ( 'NONE',  ( 162.6476498368881494, 248.9330020812748785, 10.75824100428386743 ) ) ;
#50035 = CARTESIAN_POINT ( 'NONE',  ( 154.8332767207531901, 280.7459370637686220, -0.9958211956073632631 ) ) ;
#50036 = EDGE_CURVE ( 'NONE', #69871, #38097, #17637, .T. ) ;
#50037 = CARTESIAN_POINT ( 'NONE',  ( 72.68453300703816922, 57.05733065325770781, -16.38297471568555252 ) ) ;
#50038 = ORIENTED_EDGE ( 'NONE', *, *, #19988, .F. ) ;
#50039 = CARTESIAN_POINT ( 'NONE',  ( 77.25136647710282034, 63.46566284268146063, -15.11586214491885194 ) ) ;
#50040 = VERTEX_POINT ( 'NONE', #35792 ) ;
#50041 = CARTESIAN_POINT ( 'NONE',  ( 189.0767208543637139, 290.4732453595815969, 14.36254912788081839 ) ) ;
#50042 = CARTESIAN_POINT ( 'NONE',  ( 51.36475398071000598, 188.9155109091896065, 2.679491924311254714 ) ) ;
#50043 = CARTESIAN_POINT ( 'NONE',  ( 143.0153750664825054, 259.5024278399160949, -9.188101187500093303 ) ) ;
#50044 = CARTESIAN_POINT ( 'NONE',  ( 201.2535035105529744, 282.0657020489176716, -18.08976065250591958 ) ) ;
#50045 = AXIS2_PLACEMENT_3D ( 'NONE', #56484, #80334, #72725 ) ;
#50046 = CARTESIAN_POINT ( 'NONE',  ( 112.5819247142704427, 224.2592609112379876, 2.679491924311254714 ) ) ;
#50047 = CARTESIAN_POINT ( 'NONE',  ( 28.52453836335597614, 34.65586893147758474, -7.433330006724137462 ) ) ;
#50048 = CYLINDRICAL_SURFACE ( 'NONE', #86695, 1.449999999999993072 ) ;
#50049 = CARTESIAN_POINT ( 'NONE',  ( 164.1286765816565207, 275.3158857940874782, 15.02251480813967888 ) ) ;
#50050 = CARTESIAN_POINT ( 'NONE',  ( -22.42236680055709641, 157.8615022471902591, 0.000000000000000000 ) ) ;
#50051 = ORIENTED_EDGE ( 'NONE', *, *, #54053, .T. ) ;
#50052 = VERTEX_POINT ( 'NONE', #91518 ) ;
#50053 = CARTESIAN_POINT ( 'NONE',  ( 184.6801771164089416, 296.8040060832889253, 1.022975585509389163 ) ) ;
#50055 = CARTESIAN_POINT ( 'NONE',  ( -63.34358462235559273, 38.37368864812747660, -10.00000000000000000 ) ) ;
#50054 = CARTESIAN_POINT ( 'NONE',  ( 204.5831314780710954, 276.2986172388744421, 13.28075685133257089 ) ) ;
#50056 = CARTESIAN_POINT ( 'NONE',  ( 150.0694502760089222, 271.4680435213315945, -12.17790201236558545 ) ) ;
#50057 = DIRECTION ( 'NONE',  ( -1.110223024625156343E-15, 1.000000000000000000, 0.000000000000000000 ) ) ;
#50058 = CARTESIAN_POINT ( 'NONE',  ( 161.9775247817796924, 252.0936927241524472, 14.33142805341373283 ) ) ;
#50059 = CARTESIAN_POINT ( 'NONE',  ( 161.2535912560966551, 263.0844709175967182, -17.80682751047658030 ) ) ;
#50060 = CARTESIAN_POINT ( 'NONE',  ( 164.7389676833716976, 245.3107333163898716, 5.284562706098457241 ) ) ;
#50061 = CARTESIAN_POINT ( 'NONE',  ( 196.0587100571994483, 289.0633482449420626, -17.27351923437598913 ) ) ;
#50062 = CARTESIAN_POINT ( 'NONE',  ( 22.45462004596304695, 37.14601545153949047, -10.00000000000000000 ) ) ;
#50063 = CARTESIAN_POINT ( 'NONE',  ( 102.2582280487598609, 229.8458772461660544, 9.188101187500095079 ) ) ;
#50064 = ORIENTED_EDGE ( 'NONE', *, *, #60232, .F. ) ;
#50065 = CARTESIAN_POINT ( 'NONE',  ( 150.0102862277170743, 271.3788846064419999, 12.09021458032355056 ) ) ;
#50066 = CARTESIAN_POINT ( 'NONE',  ( 117.3505249275209934, 231.8927522451417360, -10.00000000000009237 ) ) ;
#50067 = ORIENTED_EDGE ( 'NONE', *, *, #76967, .T. ) ;
#50068 = EDGE_LOOP ( 'NONE', ( #74101, #84007, #27503, #84947 ) ) ;
#50069 = CARTESIAN_POINT ( 'NONE',  ( 182.3292780454827096, 296.5739854331435481, -1.651664298513513041 ) ) ;
#50070 = DIRECTION ( 'NONE',  ( -0.8660254037844387076, -0.4999999999999998890, -0.000000000000000000 ) ) ;
#50071 = FACE_OUTER_BOUND ( 'NONE', #55909, .T. ) ;
#50072 = ADVANCED_FACE ( 'NONE', ( #37770 ), #29201, .T. ) ;
#50073 = CARTESIAN_POINT ( 'NONE',  ( 206.9942764641839688, 270.1223916185117560, -3.431663675821580828 ) ) ;
#50074 = CARTESIAN_POINT ( 'NONE',  ( 96.25000326212280299, 232.5024278399160664, -9.188101187500093303 ) ) ;
#50075 = VERTEX_POINT ( 'NONE', #37281 ) ;
#50076 = EDGE_CURVE ( 'NONE', #53637, #52411, #47378, .T. ) ;
#50077 = ORIENTED_EDGE ( 'NONE', *, *, #19912, .T. ) ;
#50079 = ADVANCED_FACE ( 'NONE', ( #280 ), #15978, .F. ) ;
#50078 = CARTESIAN_POINT ( 'NONE',  ( 208.2124092825819162, 270.0125236866795149, -2.339659020816897694 ) ) ;
#50080 = ORIENTED_EDGE ( 'NONE', *, *, #72324, .T. ) ;
#50081 = EDGE_CURVE ( 'NONE', #99571, #97906, #6307, .T. ) ;
#50082 = VECTOR ( 'NONE', #77676, 1000.000000000000000 ) ;
#50083 = CARTESIAN_POINT ( 'NONE',  ( 194.6143112939460309, 266.3039560675284179, -7.756514573897542064 ) ) ;
#50084 = CARTESIAN_POINT ( 'NONE',  ( 70.68033699063239794, 69.39733653096790533, -7.416591401506187786 ) ) ;
#50086 = CARTESIAN_POINT ( 'NONE',  ( 69.76031522910172100, 62.75377154243565059, -13.30659298224870746 ) ) ;
#50085 = CARTESIAN_POINT ( 'NONE',  ( 129.7002344832967538, 251.8149278399160949, -9.188101187500095079 ) ) ;
#50087 = LINE ( 'NONE', #81044, #57424 ) ;
#50088 = DIRECTION ( 'NONE',  ( -0.5000000000000006661, 0.8660254037844382635, -1.877843081442121204E-16 ) ) ;
#50089 = CIRCLE ( 'NONE', #84125, 10.00000000000000711 ) ;
#50090 = ORIENTED_EDGE ( 'NONE', *, *, #24910, .F. ) ;
#50091 = CARTESIAN_POINT ( 'NONE',  ( 204.9214210856886496, 275.7126824508080176, 13.23219655298346709 ) ) ;
#50092 = CARTESIAN_POINT ( 'NONE',  ( 160.6921517183488390, 275.5961185789591354, 13.91821361452047334 ) ) ;
#50093 = LINE ( 'NONE', #64804, #4765 ) ;
#50094 = DIRECTION ( 'NONE',  ( -0.9825427565607363078, 0.1860369090530953895, 0.000000000000000000 ) ) ;
#50095 = FACE_OUTER_BOUND ( 'NONE', #48430, .T. ) ;
#50096 = PLANE ( 'NONE',  #98564 ) ;
#50097 = LINE ( 'NONE', #81053, #14595 ) ;
#50098 = DIRECTION ( 'NONE',  ( -0.8660254037844387076, -0.4999999999999998890, -0.000000000000000000 ) ) ;
#50099 = VECTOR ( 'NONE', #564, 1000.000000000000000 ) ;
#50100 = CARTESIAN_POINT ( 'NONE',  ( 172.7264208856190919, 290.8582626858774347, 2.771863430787652849 ) ) ;
#50101 = CARTESIAN_POINT ( 'NONE',  ( 68.62498439451977106, 69.99363476994645339, -2.580443242845753549 ) ) ;
#50102 = CARTESIAN_POINT ( 'NONE',  ( 159.9531724557437826, 253.5999738052623229, -15.71074128491364874 ) ) ;
#50103 = CARTESIAN_POINT ( 'NONE',  ( 83.15922154792146159, 52.24841325804966630, 14.83149234656706561 ) ) ;
#50104 = CARTESIAN_POINT ( 'NONE',  ( -12.91644128716779072, 174.8967562850347690, 1.347971487989956912E-14 ) ) ;
#50105 = CARTESIAN_POINT ( 'NONE',  ( -50.66096862766640641, 31.69950886434491721, 10.00000000000000000 ) ) ;
#50106 = CARTESIAN_POINT ( 'NONE',  ( 189.8375740044709801, 294.2633537128526768, 13.17988706671251720 ) ) ;
#50107 = VECTOR ( 'NONE', #9690, 1000.000000000000000 ) ;
#50108 = CARTESIAN_POINT ( 'NONE',  ( 71.65393590783921240, 64.63887889010254639, -12.86708473997534341 ) ) ;
#50109 = CARTESIAN_POINT ( 'NONE',  ( 74.31667694623762088, 55.31426079121899164, 16.60244124719878300 ) ) ;
#50110 = CARTESIAN_POINT ( 'NONE',  ( 162.9203612012105111, 256.0174525517487609, 16.09041223595896852 ) ) ;
#50111 = AXIS2_PLACEMENT_3D ( 'NONE', #1538, #40502, #84656 ) ;
#50112 = CARTESIAN_POINT ( 'NONE',  ( 33.59574554791263523, 38.13478043621391578, 8.090169943749478065 ) ) ;
#50113 = CARTESIAN_POINT ( 'NONE',  ( 78.54208217020030247, 47.90658315326027861, 13.93004184109306287 ) ) ;
#50114 = CARTESIAN_POINT ( 'NONE',  ( 203.3041373168503299, 278.5139001086923827, -16.61929732091214973 ) ) ;
#50115 = CARTESIAN_POINT ( 'NONE',  ( 157.6418352378513816, 271.0230738774055226, -14.72348240588997825 ) ) ;
#50116 = CARTESIAN_POINT ( 'NONE',  ( 85.67990461644461675, 43.48540777662389445, -4.634265786033663126 ) ) ;
#50117 = CARTESIAN_POINT ( 'NONE',  ( 161.1061647010182583, 251.6029326557136585, -13.56144933775657613 ) ) ;
#50118 = CARTESIAN_POINT ( 'NONE',  ( 19.09298631340924501, 172.6423013555409796, -4.594050593750043987 ) ) ;
#50119 = CARTESIAN_POINT ( 'NONE',  ( 207.3594494688759085, 271.0859767844725638, 2.519715249304678828 ) ) ;
#50120 = ORIENTED_EDGE ( 'NONE', *, *, #55892, .F. ) ;
#50121 = CARTESIAN_POINT ( 'NONE',  ( 87.13039101863441260, 46.06611145402069241, 8.900391155234917306 ) ) ;
#50122 = CARTESIAN_POINT ( 'NONE',  ( 21.90410768801267949, 17.81029122506294726, 8.090169943749479842 ) ) ;
#50123 = CARTESIAN_POINT ( 'NONE',  ( 164.2647213391612979, 246.1321520798662164, -5.830872732487307530 ) ) ;
#50124 = CARTESIAN_POINT ( 'NONE',  ( 71.89122079532039322, 72.62093029633255981, -0.6100853850958146696 ) ) ;
#50125 = CARTESIAN_POINT ( 'NONE',  ( 33.40920844789697952, 190.0958772461660544, -9.188101187500095079 ) ) ;
#50126 = ADVANCED_FACE ( 'NONE', ( #25970 ), #16477, .T. ) ;
#50127 = CARTESIAN_POINT ( 'NONE',  ( 87.04534585051717954, 46.05262481000475105, 8.948764308993935046 ) ) ;
#50128 = CARTESIAN_POINT ( 'NONE',  ( 147.1199024702499969, 275.8278494473859723, 5.224467159276165340 ) ) ;
#50129 = CARTESIAN_POINT ( 'NONE',  ( 29.27874087092374111, 39.83705186507756224, 3.090169943749475401 ) ) ;
#50130 = CARTESIAN_POINT ( 'NONE',  ( 199.5733002173658690, 267.3584479166742653, -6.689480323808837170 ) ) ;
#50131 = CARTESIAN_POINT ( 'NONE',  ( 178.2475648503018704, 293.8761651525964567, 2.747118326088546336 ) ) ;
#50132 = CARTESIAN_POINT ( 'NONE',  ( 179.5554748665543059, 278.7501255867640566, -17.25862896719455009 ) ) ;
#50133 = CARTESIAN_POINT ( 'NONE',  ( 72.54776654123371316, 67.64497073380857728, -10.93401973738937549 ) ) ;
#50134 = CARTESIAN_POINT ( 'NONE',  ( -56.06787742410712383, 34.75406423768147590, -10.00000000000000000 ) ) ;
#50135 = DIRECTION ( 'NONE',  ( -0.8218955677251095215, -0.5696381972391070247, 0.000000000000000000 ) ) ;
#50136 = B_SPLINE_CURVE_WITH_KNOTS ( 'NONE', 3,
 ( #15554, #77387, #43802, #22004 ),
 .UNSPECIFIED., .F., .F.,
 ( 4, 4 ),
 ( 0.03394374891021562091, 0.04279985253772465581 ),
 .UNSPECIFIED. ) ;
#50137 = CARTESIAN_POINT ( 'NONE',  ( 84.96478326871331888, 219.8615022471902591, -10.00000000000009592 ) ) ;
#50138 = CARTESIAN_POINT ( 'NONE',  ( 19.16720650933548953, 170.3262482093457777, 3.021315404115420679E-15 ) ) ;
#50139 = CARTESIAN_POINT ( 'NONE',  ( 176.6775373737683879, 280.6285440243045741, 16.49000606930484736 ) ) ;
#50140 = CARTESIAN_POINT ( 'NONE',  ( 44.31597619863101301, 187.2048013555409796, 4.594050593750051981 ) ) ;
#50141 = EDGE_LOOP ( 'NONE', ( #59375, #92, #97771, #65261, #70489 ) ) ;
#50142 = CARTESIAN_POINT ( 'NONE',  ( 162.6641061006424138, 263.2818470139165470, 17.66040242672044869 ) ) ;
#50143 = CARTESIAN_POINT ( 'NONE',  ( 146.9324727656309335, 276.1524872186338371, 3.813717745456558728 ) ) ;
#50145 = CARTESIAN_POINT ( 'NONE',  ( 45.66470909604093720, 114.5311720768849995, -10.00000000000000000 ) ) ;
#50144 = AXIS2_PLACEMENT_3D ( 'NONE', #52789, #76134, #13329 ) ;
#50146 = ORIENTED_EDGE ( 'NONE', *, *, #46009, .T. ) ;
#50147 = CARTESIAN_POINT ( 'NONE',  ( 167.6847463121813462, 285.6965240061992972, 7.996140646124640483 ) ) ;
#50148 = CARTESIAN_POINT ( 'NONE',  ( 164.8251969117060298, 245.1613799118173063, -1.508678420156898348 ) ) ;
#50149 = CARTESIAN_POINT ( 'NONE',  ( 82.86586985908988368, 152.2544130683315871, 0.000000000000000000 ) ) ;
#50150 = B_SPLINE_CURVE_WITH_KNOTS ( 'NONE', 3,
 ( #26257, #9054, #40431, #10559, #40923, #39922, #41434, #17658, #32842, #71870, #2468, #33348, #72375, #18156, #90083, #98162, #42912, #97667, #28235, #66249, #20652, #59111, #51540, #35840, #98666, #97185, #4959, #27751, #57633, #96686, #67232, #82502, #12558, #27256, #88610, #58139, #13066, #43925, #67741, #74865, #12057, #19177, #89119, #50049, #66734, #43433, #81002, #73360 ),
 .UNSPECIFIED., .F., .F.,
 ( 4, 2, 2, 2, 2, 2, 2, 2, 2, 2, 2, 2, 2, 2, 2, 2, 2, 2, 2, 2, 2, 2, 2, 4 ),
 ( 0.001113145979540773644, 0.001586597418653406784, 0.002060048857766039708, 0.002296774577322319415, 0.002533500296878601291, 0.002651863156656742663, 0.002770226016434883601, 0.003006951735991266091, 0.003480403175104027601, 0.003953854614216789978, 0.004900757492442405806, 0.005847660370668021634, 0.006321111809780829982, 0.006794563248893638330, 0.006912926108671802253, 0.006972107538560923246, 0.007031288968450044238, 0.007149651828228287091, 0.007268014688006530812, 0.007504740407563156163, 0.007741466127119781514, 0.007978191846676406865, 0.008214917566233031349, 0.008688369005346287255 ),
 .UNSPECIFIED. ) ;
#50151 = CARTESIAN_POINT ( 'NONE',  ( 31.23567208480136514, 20.96004757982091604, -5.678558825948276656 ) ) ;
#50152 = CARTESIAN_POINT ( 'NONE',  ( 185.8221718112685039, 262.9784142112231393, 11.29663378258160655 ) ) ;
#50153 = CARTESIAN_POINT ( 'NONE',  ( 86.52156533961138507, 47.40180082335727718, -10.32616759113387062 ) ) ;
#50154 = CARTESIAN_POINT ( 'NONE',  ( 174.2371165158130566, 257.1234833113948071, 11.35068822046578774 ) ) ;
#50155 = EDGE_LOOP ( 'NONE', ( #13068, #25458, #35142, #76105 ) ) ;
#50156 = CARTESIAN_POINT ( 'NONE',  ( 13.89352694080530348, 28.99752408145591076, 5.678558825948276656 ) ) ;
#50157 = CARTESIAN_POINT ( 'NONE',  ( -26.59607535340072104, 23.41021043553327630, 10.00000000000000000 ) ) ;
#50158 = CARTESIAN_POINT ( 'NONE',  ( 174.2468074326821181, 254.8252884221085992, 8.251842399806214701 ) ) ;
#50159 = CARTESIAN_POINT ( 'NONE',  ( -27.42236680055714260, 166.5217562850347406, 1.224646799147364892E-15 ) ) ;
#50160 = ORIENTED_EDGE ( 'NONE', *, *, #67139, .F. ) ;
#50161 = CARTESIAN_POINT ( 'NONE',  ( 72.01497877597556396, 71.50364303677275757, -5.786257741033058011 ) ) ;
#50162 = CARTESIAN_POINT ( 'NONE',  ( 191.0900422946452011, 299.6693332556258724, 8.872191398975367349 ) ) ;
#50163 = CARTESIAN_POINT ( 'NONE',  ( 177.5411558806154062, 255.6075609413517213, -6.847706546168232045 ) ) ;
#50164 = CYLINDRICAL_SURFACE ( 'NONE', #38284, 14.99999999999968381 ) ;
#50165 = ORIENTED_EDGE ( 'NONE', *, *, #4979, .F. ) ;
#50166 = CIRCLE ( 'NONE', #42061, 50.00000000000000711 ) ;
#50167 = EDGE_LOOP ( 'NONE', ( #9550, #9475, #29554, #59988 ) ) ;
#50169 = CARTESIAN_POINT ( 'NONE',  ( -72.30469571560091424, 48.86078274006646183, 10.00000000000000000 ) ) ;
#50168 = CARTESIAN_POINT ( 'NONE',  ( 161.2133744761260061, 251.4172398781588811, -14.30368667312104058 ) ) ;
#50170 = CARTESIAN_POINT ( 'NONE',  ( 186.5128128464827455, 296.3652354721813822, -8.829210103799347564 ) ) ;
#50171 = ORIENTED_EDGE ( 'NONE', *, *, #64505, .F. ) ;
#50172 = CARTESIAN_POINT ( 'NONE',  ( 65.83577767310526951, 68.92730293486754078, -2.453578508652157097 ) ) ;
#50173 = DIRECTION ( 'NONE',  ( -0.9805290675673918876, -0.1963739994383708332, 0.000000000000000000 ) ) ;
#50174 = CARTESIAN_POINT ( 'NONE',  ( 72.59642922388725594, 57.37503576641776704, -16.32655392149956342 ) ) ;
#50175 = CARTESIAN_POINT ( 'NONE',  ( 77.94354854059760385, 61.39700473696555605, -16.15480247637162847 ) ) ;
#50176 = CARTESIAN_POINT ( 'NONE',  ( 205.1300674467857164, 275.3512963525735131, -12.60245643603069610 ) ) ;
#50177 = CARTESIAN_POINT ( 'NONE',  ( 117.0346129529493311, 244.5024278399160949, -9.188101187500093303 ) ) ;
#50178 = CARTESIAN_POINT ( 'NONE',  ( 182.4502886106904214, 259.6876753163259650, 10.69873880494191631 ) ) ;
#50179 = ORIENTED_EDGE ( 'NONE', *, *, #90752, .F. ) ;
#50180 = CARTESIAN_POINT ( 'NONE',  ( 164.4989226152910646, 245.7265035704120351, -6.575810094723514965 ) ) ;
#50181 = EDGE_LOOP ( 'NONE', ( #5300, #94428, #45319, #81732 ) ) ;
#50182 = CARTESIAN_POINT ( 'NONE',  ( 38.36533659613348846, 24.01110640527295104, 2.839279412974134775 ) ) ;
#50183 = FACE_BOUND ( 'NONE', #61654, .T. ) ;
#50184 = CARTESIAN_POINT ( 'NONE',  ( 194.5725374088679871, 291.6374747806817140, -16.23208319182986870 ) ) ;
#50185 = CARTESIAN_POINT ( 'NONE',  ( 70.10703493326258240, 211.2833772461660544, -9.188101187500095079 ) ) ;
#50186 = CARTESIAN_POINT ( 'NONE',  ( 15.08735849730845402, 189.5177522451419065, 5.000000000000046185 ) ) ;
#50187 =( BOUNDED_CURVE ( )  B_SPLINE_CURVE ( 2, ( #876, #76872, #71297, #70268, #24181, #38867, #8484, #54550, #69774 ),
 .UNSPECIFIED., .F., .T. ) 
 B_SPLINE_CURVE_WITH_KNOTS ( ( 3, 2, 2, 2, 3 ),
 ( 0.2540322580645161255, 0.2553763440860215006, 0.2580645161290322509, 0.2607526881720430012, 0.2620967741935483764 ),
 .UNSPECIFIED. ) 
 CURVE ( )  GEOMETRIC_REPRESENTATION_ITEM ( )  RATIONAL_B_SPLINE_CURVE ( ( 0.9330127018922194093, 0.9330127018922194093, 1.000000000000000000, 0.8660254037844387076, 1.000000000000000000, 0.8660254037844387076, 1.000000000000000000, 0.9330127018922194093, 0.9330127018922194093 ) ) 
 REPRESENTATION_ITEM ( '' )  );
#50188 = CARTESIAN_POINT ( 'NONE',  ( 151.0715479399129606, 268.9833987204304435, 14.24612252017116987 ) ) ;
#50189 = CARTESIAN_POINT ( 'NONE',  ( 150.8360166798673561, 269.3913508296000145, 13.81437070545826806 ) ) ;
#50190 = CARTESIAN_POINT ( 'NONE',  ( 175.0975211258509603, 278.2292065890057984, 15.47011627292242508 ) ) ;
#50191 = ORIENTED_EDGE ( 'NONE', *, *, #89062, .F. ) ;
#50192 = PLANE ( 'NONE',  #12465 ) ;
#50193 = CARTESIAN_POINT ( 'NONE',  ( 86.54292033101232562, 46.25028892199808439, 8.970843135639702481 ) ) ;
#50194 = CARTESIAN_POINT ( 'NONE',  ( 203.3684377202211522, 278.4025285431072803, -16.56116267537666076 ) ) ;
#50195 = ORIENTED_EDGE ( 'NONE', *, *, #37497, .T. ) ;
#50196 = CARTESIAN_POINT ( 'NONE',  ( 148.0654368686451221, 274.1901358290616031, 9.010908242870014462 ) ) ;
#50197 = CARTESIAN_POINT ( 'NONE',  ( 69.97979529158072864, 69.74216827977384980, -5.914717412081216708 ) ) ;
#50198 = CARTESIAN_POINT ( 'NONE',  ( 161.3773209892555371, 251.1332761876949746, -14.50043705923759241 ) ) ;
#50199 = EDGE_CURVE ( 'NONE', #33351, #6194, #85429, .T. ) ;
#50200 = CARTESIAN_POINT ( 'NONE',  ( 146.9700173529739970, 276.0874580858064746, -5.099093031535578469 ) ) ;
#50201 = CARTESIAN_POINT ( 'NONE',  ( 199.6130415427998344, 283.1155522273526230, -17.53316870511595127 ) ) ;
#50202 = CARTESIAN_POINT ( 'NONE',  ( 205.7639495959071212, 274.2533802642843170, 10.79039487422292432 ) ) ;
#50203 = CARTESIAN_POINT ( 'NONE',  ( 152.3377091156085896, 270.0594875778499500, -14.54836364073420008 ) ) ;
#50204 = CARTESIAN_POINT ( 'NONE',  ( 157.7255603307123408, 268.5163524934444013, 16.86592485641857309 ) ) ;
#50205 = CARTESIAN_POINT ( 'NONE',  ( 167.4844004446328256, 256.4883897734646894, 13.70360325908868049 ) ) ;
#50206 = CARTESIAN_POINT ( 'NONE',  ( 57.60966550219797000, 179.2419560658249225, 17.47570218321536117 ) ) ;
#50207 = CARTESIAN_POINT ( 'NONE',  ( 122.6094779419291712, 253.8464784336661353, 1.353441290958777327E-15 ) ) ;
#50208 = VERTEX_POINT ( 'NONE', #93519 ) ;
#50209 = CARTESIAN_POINT ( 'NONE',  ( 81.83453868260083652, 44.26299598697195847, -9.678769061459140843 ) ) ;
#50210 = CARTESIAN_POINT ( 'NONE',  ( 82.70413545112889153, 41.12970673414849188, 1.275000209075848101 ) ) ;
#50211 = FACE_OUTER_BOUND ( 'NONE', #11064, .T. ) ;
#50212 = CARTESIAN_POINT ( 'NONE',  ( 164.1259971043086239, 246.3724295028720519, 5.761669507629934905 ) ) ;
#50213 = CARTESIAN_POINT ( 'NONE',  ( 74.50257599732556457, 59.70488952813933281, 15.64583394787582726 ) ) ;
#50214 = CARTESIAN_POINT ( 'NONE',  ( -27.23710841895085011, 23.47708815495369450, 10.00000000000000000 ) ) ;
#50215 = ORIENTED_EDGE ( 'NONE', *, *, #56431, .F. ) ;
#50216 = CARTESIAN_POINT ( 'NONE',  ( 80.49253188860416230, 57.12688299469299125, -16.22935582423522405 ) ) ;
#50217 = CARTESIAN_POINT ( 'NONE',  ( 165.1786760834411609, 247.4249377785339448, -5.585047393798932447 ) ) ;
#50218 = CARTESIAN_POINT ( 'NONE',  ( 164.5379227956242687, 245.6589532765702870, -2.440899697315300987 ) ) ;
#50219 = DIRECTION ( 'NONE',  ( -0.7440200784635719877, -0.6681572590663519273, 0.000000000000000000 ) ) ;
#50220 = VECTOR ( 'NONE', #38793, 1000.000000000000000 ) ;
#50221 = CARTESIAN_POINT ( 'NONE',  ( 27.01324999880465327, 179.7365022471902307, 10.00000000000009948 ) ) ;
#50222 = CARTESIAN_POINT ( 'NONE',  ( 67.66865572057727718, 68.40145999173375913, 5.820033390399663276 ) ) ;
#50223 = CARTESIAN_POINT ( 'NONE',  ( 157.1269483542914998, 258.4951375425532092, -17.15328932028234377 ) ) ;
#50224 = CARTESIAN_POINT ( 'NONE',  ( 174.4776468927544499, 252.1408974215496528, 3.505067343168197347 ) ) ;
#50225 = CARTESIAN_POINT ( 'NONE',  ( 22.16837966976980567, 14.92755873383626053, 6.180339887498953466 ) ) ;
#50226 = CARTESIAN_POINT ( 'NONE',  ( 190.1751179328237242, 301.2540287353828035, 3.252640783176552475 ) ) ;
#50227 = CARTESIAN_POINT ( 'NONE',  ( 154.2298868780514454, 279.0943400367102072, -1.589968555053201449 ) ) ;
#50228 = CARTESIAN_POINT ( 'NONE',  ( 170.1001268420399697, 285.5941755235542701, -7.968252287399715250 ) ) ;
#50229 = CARTESIAN_POINT ( 'NONE',  ( 206.8073682671177664, 270.4461261121818438, -4.970999383176901709 ) ) ;
#50230 = VECTOR ( 'NONE', #45586, 1000.000000000000227 ) ;
#50231 = CARTESIAN_POINT ( 'NONE',  ( 193.1495885362050160, 289.2521248809247254, 16.30406654585521053 ) ) ;
#50232 = CARTESIAN_POINT ( 'NONE',  ( 136.7639277290221571, 249.7677522451418497, 10.00000000000009592 ) ) ;
#50233 = CARTESIAN_POINT ( 'NONE',  ( 16.01096549046674511, 31.01751292744055988, 6.180339887498949913 ) ) ;
#50234 = ORIENTED_EDGE ( 'NONE', *, *, #40599, .T. ) ;
#50235 = CARTESIAN_POINT ( 'NONE',  ( 196.0355168007595523, 291.1035201434990540, 17.55377893960077884 ) ) ;
#50236 = CARTESIAN_POINT ( 'NONE',  ( 147.7870527676176948, 274.6723112360602386, 9.257357958194809555 ) ) ;
#50237 = CARTESIAN_POINT ( 'NONE',  ( -6.860972828079417773, 166.8458772461660544, 9.188101187500095079 ) ) ;
#50238 = EDGE_CURVE ( 'NONE', #95379, #37787, #23560, .T. ) ;
#50239 = CARTESIAN_POINT ( 'NONE',  ( 31.29809797828990270, 195.0024278399160664, -9.188101187500093303 ) ) ;
#50240 = CARTESIAN_POINT ( 'NONE',  ( 85.86628601408199302, 44.95660682449336321, 8.361449031888060546 ) ) ;
#50241 = CARTESIAN_POINT ( 'NONE',  ( 21.39005255714673126, 24.30066082961421969, -10.00000000000000533 ) ) ;
#50242 = CARTESIAN_POINT ( 'NONE',  ( 88.21238909966383801, 43.70556102481675964, 0.1923655077720387852 ) ) ;
#50243 = LINE ( 'NONE', #89311, #96605 ) ;
#50244 = CARTESIAN_POINT ( 'NONE',  ( 192.6136217801248449, 292.3795896600195761, -14.34082932734286508 ) ) ;
#50245 = CARTESIAN_POINT ( 'NONE',  ( 190.1635032421960148, 301.2741459696644029, -5.047660290019184259 ) ) ;
#50246 = CARTESIAN_POINT ( 'NONE',  ( 73.94386985606865892, 54.90338819443267226, -16.13259590105355912 ) ) ;
#50248 = CARTESIAN_POINT ( 'NONE',  ( 66.61587002248261058, 209.2677522451418497, 10.00000000000009592 ) ) ;
#50247 = CARTESIAN_POINT ( 'NONE',  ( 167.6162704737794229, 256.6000348849465240, 13.71821036101052371 ) ) ;
#50249 = CARTESIAN_POINT ( 'NONE',  ( 76.65070268594573122, 58.80663122369263363, 16.45680034700567163 ) ) ;
#50250 = CARTESIAN_POINT ( 'NONE',  ( 32.29641253342593643, 23.81029122506296503, 8.090169943749479842 ) ) ;
#50251 = DIRECTION ( 'NONE',  ( -1.000000000000000000, 0.000000000000000000, 0.000000000000000000 ) ) ;
#50252 = EDGE_CURVE ( 'NONE', #42468, #84728, #23705, .T. ) ;
#50253 = CARTESIAN_POINT ( 'NONE',  ( 33.07542782529563397, 203.2365022471903444, 2.944929066748280225E-16 ) ) ;
#50254 = CARTESIAN_POINT ( 'NONE',  ( 181.5004962646415265, 292.1248343589982710, 8.982815215163469702 ) ) ;
#50255 = CARTESIAN_POINT ( 'NONE',  ( 203.0535368433499457, 278.9479528611958585, 16.46202213522710167 ) ) ;
#50256 = CARTESIAN_POINT ( 'NONE',  ( -6.076397627723526540, 176.4869531367911293, 4.594050593750046652 ) ) ;
#50257 = CARTESIAN_POINT ( 'NONE',  ( 35.55378427144160014, 29.03085787977765264, 9.188101187500006262 ) ) ;
#50258 = EDGE_CURVE ( 'NONE', #12902, #48310, #96969, .T. ) ;
#50259 = CARTESIAN_POINT ( 'NONE',  ( 192.2431834237441706, 297.6720342317289578, 11.07782187406058938 ) ) ;
#50260 = CARTESIAN_POINT ( 'NONE',  ( 37.50591675755416077, 22.44966523072497111, -2.296566073217252530E-15 ) ) ;
#50261 = CARTESIAN_POINT ( 'NONE',  ( 155.8365007042834520, 261.3224821757460177, -17.11083130380785633 ) ) ;
#50262 = CARTESIAN_POINT ( 'NONE',  ( 179.3274614371453595, 277.6279536742436562, 17.03900687375964296 ) ) ;
#50263 = CYLINDRICAL_SURFACE ( 'NONE', #77241, 17.82106496071139645 ) ;
#50264 = CARTESIAN_POINT ( 'NONE',  ( 65.14187045721612890, 219.9637435831425023, 2.679491924311251605 ) ) ;
#50265 = CARTESIAN_POINT ( 'NONE',  ( 177.6585084262452767, 260.6037935310539524, -13.90472577101287932 ) ) ;
#50266 = CARTESIAN_POINT ( 'NONE',  ( 13.56875384759882763, 10.76004757982087767, 5.678558825948272215 ) ) ;
#50267 = CARTESIAN_POINT ( 'NONE',  ( 71.83275678050462432, 72.56239119006677640, 1.040614184235684636 ) ) ;
#50268 = CARTESIAN_POINT ( 'NONE',  ( 11.52878981408637848, 24.84336893147754921, -7.433330006724137462 ) ) ;
#50269 = CARTESIAN_POINT ( 'NONE',  ( 68.53065452504849020, 198.8262482093457777, 3.021315404115420679E-15 ) ) ;
#50270 = CARTESIAN_POINT ( 'NONE',  ( 193.7114073116034945, 295.1289958610702797, 14.86160832869823345 ) ) ;
#50271 = ORIENTED_EDGE ( 'NONE', *, *, #87525, .T. ) ;
#50272 = CARTESIAN_POINT ( 'NONE',  ( 155.6531420801174761, 275.9231362174812148, 10.30624812126558076 ) ) ;
#50273 = CARTESIAN_POINT ( 'NONE',  ( 75.08378362262867256, 53.60473078829387106, -16.54206508529750508 ) ) ;
#50274 = CARTESIAN_POINT ( 'NONE',  ( 159.5895502557670795, 254.2297859303815244, -16.92708575547316485 ) ) ;
#50275 = ORIENTED_EDGE ( 'NONE', *, *, #21817, .F. ) ;
#50276 = CARTESIAN_POINT ( 'NONE',  ( 192.2943420783192323, 297.5834248427583475, 12.53393473147773562 ) ) ;
#50277 = CARTESIAN_POINT ( 'NONE',  ( 164.3524132573224392, 245.9802652221976587, -2.749586949851067441 ) ) ;
#50278 = B_SPLINE_CURVE_WITH_KNOTS ( 'NONE', 3,
 ( #28295, #50110, #43494, #36392 ),
 .UNSPECIFIED., .F., .F.,
 ( 4, 4 ),
 ( 0.003801382972845887033, 0.008042818574261435469 ),
 .UNSPECIFIED. ) ;
#50279 = CARTESIAN_POINT ( 'NONE',  ( 66.72318566906618287, 68.35417501291662745, 4.516870767104322226 ) ) ;
#50280 = CARTESIAN_POINT ( 'NONE',  ( 87.36072329576109041, 44.92403384853250259, 6.858028155142555704 ) ) ;
#50281 = EDGE_LOOP ( 'NONE', ( #51291, #69069, #17398, #85950 ) ) ;
#50282 = ORIENTED_EDGE ( 'NONE', *, *, #48604, .F. ) ;
#50284 = CARTESIAN_POINT ( 'NONE',  ( 164.1224127655298730, 246.3786377597482158, 7.356982420601481998 ) ) ;
#50283 = CARTESIAN_POINT ( 'NONE',  ( 159.7762908497461467, 278.5220354493135915, -9.751953824713970320 ) ) ;
#50285 = CARTESIAN_POINT ( 'NONE',  ( 153.3100492430090753, 265.1062007306585997, 16.32434963471121492 ) ) ;
#50286 = ORIENTED_EDGE ( 'NONE', *, *, #66944, .F. ) ;
#50287 = CARTESIAN_POINT ( 'NONE',  ( 77.57840026120739196, 56.51549017185177348, 16.17678933532221563 ) ) ;
#50288 = CARTESIAN_POINT ( 'NONE',  ( 178.0262838233909974, 263.6630881215525051, 15.29339064780925206 ) ) ;
#50289 = ORIENTED_EDGE ( 'NONE', *, *, #18310, .T. ) ;
#50290 = CARTESIAN_POINT ( 'NONE',  ( 78.08206365161463225, 61.83366292688850763, -15.70979438352861735 ) ) ;
#50291 = CARTESIAN_POINT ( 'NONE',  ( 82.46595807734689743, 49.18434068982010388, -13.48834215029216033 ) ) ;
#50292 = CARTESIAN_POINT ( 'NONE',  ( 34.86956345232661647, 202.4860189848785978, -2.679491924311252493 ) ) ;
#50293 = VERTEX_POINT ( 'NONE', #64961 ) ;
#50294 = CARTESIAN_POINT ( 'NONE',  ( 161.4726291907278721, 250.9681975403669867, 14.52346149734912117 ) ) ;
#50295 = CARTESIAN_POINT ( 'NONE',  ( 167.3161501383444261, 274.8626071502216064, -15.20120324154985880 ) ) ;
#50296 = LINE ( 'NONE', #80765, #59064 ) ;
#50297 = ORIENTED_EDGE ( 'NONE', *, *, #4205, .T. ) ;
#50298 = ADVANCED_FACE ( 'NONE', ( #22584 ), #53471, .F. ) ;
#50299 = ADVANCED_FACE ( 'NONE', ( #5150 ), #42629, .T. ) ;
#50300 = CARTESIAN_POINT ( 'NONE',  ( 177.3307538467140319, 279.0261758493545017, -15.97343219706607442 ) ) ;
#50301 = CARTESIAN_POINT ( 'NONE',  ( 163.2437751800324293, 247.9004826992694461, 9.806027032984305336 ) ) ;
#50302 = VERTEX_POINT ( 'NONE', #34547 ) ;
#50303 = CARTESIAN_POINT ( 'NONE',  ( 157.1587696251558555, 266.8444457941050700, -16.20406809633236023 ) ) ;
#50304 = EDGE_LOOP ( 'NONE', ( #27583, #70009, #62767, #71725 ) ) ;
#50305 = CARTESIAN_POINT ( 'NONE',  ( -31.49789205211705934, 23.81092751074078606, 10.00000000000000000 ) ) ;
#50306 = AXIS2_PLACEMENT_3D ( 'NONE', #31078, #8299, #44780 ) ;
#50307 = ORIENTED_EDGE ( 'NONE', *, *, #19310, .T. ) ;
#50308 = LINE ( 'NONE', #11834, #4006 ) ;
#50309 = CARTESIAN_POINT ( 'NONE',  ( 82.92115063973837152, 53.64018987990930043, 15.71948723892795385 ) ) ;
#50310 = CARTESIAN_POINT ( 'NONE',  ( 141.3286032983506004, 245.7365022471902307, 10.00000000000009948 ) ) ;
#50311 = CARTESIAN_POINT ( 'NONE',  ( 193.1255195334355506, 295.1544621841915159, 13.26913244492654265 ) ) ;
#50312 = CARTESIAN_POINT ( 'NONE',  ( 86.87294856589132053, 43.40665088353684808, 1.105523696438083459 ) ) ;
#50313 = EDGE_CURVE ( 'NONE', #77820, #33752, #50243, .T. ) ;
#50314 = CARTESIAN_POINT ( 'NONE',  ( 197.3765505787902441, 288.7807815052838123, -16.66600386213448814 ) ) ;
#50315 = EDGE_LOOP ( 'NONE', ( #64515, #3728, #94169, #70101 ) ) ;
#50316 = CARTESIAN_POINT ( 'NONE',  ( 15.70095469851434622, 53.54748473301773970, 59.99999999999999289 ) ) ;
#50317 = ADVANCED_FACE ( 'NONE', ( #35544 ), #5304, .F. ) ;
#50318 = CARTESIAN_POINT ( 'NONE',  ( 24.12344523961532161, 25.87878583063842086, -9.188101187500006262 ) ) ;
#50319 = LINE ( 'NONE', #11845, #46167 ) ;
#50320 = CARTESIAN_POINT ( 'NONE',  ( 164.3022921857394749, 246.0670774647090582, 1.862798784958315856 ) ) ;
#50322 = VERTEX_POINT ( 'NONE', #52229 ) ;
#50321 = CARTESIAN_POINT ( 'NONE',  ( 82.63281508726200286, 40.94328431233920895, -3.617117793111280122 ) ) ;
#50323 = VERTEX_POINT ( 'NONE', #76067 ) ;
#50324 = CARTESIAN_POINT ( 'NONE',  ( 187.0393956332045775, 276.8356235671391232, 16.76004927575691639 ) ) ;
#50325 = CARTESIAN_POINT ( 'NONE',  ( 171.4620979185174292, 259.3841603946243595, -13.88139083577690869 ) ) ;
#50326 = EDGE_CURVE ( 'NONE', #48318, #59756, #10538, .T. ) ;
#50327 = LINE ( 'NONE', #81278, #28535 ) ;
#50328 = LINE ( 'NONE', #10850, #60242 ) ;
#50329 = CARTESIAN_POINT ( 'NONE',  ( 160.6249589658661137, 252.4364054378906985, -15.80515328853796042 ) ) ;
#50330 = CARTESIAN_POINT ( 'NONE',  ( 81.29539683296886210, 43.25976067974499273, 9.624898955577574355 ) ) ;
#50331 = ORIENTED_EDGE ( 'NONE', *, *, #37082, .F. ) ;
#50332 = FACE_OUTER_BOUND ( 'NONE', #28997, .T. ) ;
#50333 = CARTESIAN_POINT ( 'NONE',  ( 5.404797899793122973, 27.42564005363386315, 10.00000000000000000 ) ) ;
#50334 = DIRECTION ( 'NONE',  ( 0.4999999999999998890, -0.8660254037844385966, 0.000000000000000000 ) ) ;
#50335 = B_SPLINE_CURVE_WITH_KNOTS ( 'NONE', 3,
 ( #16372, #8774, #78186, #55841, #33583, #71594, #71094, #80215, #86329, #62445, #39644, #47264, #31556, #79720, #10282, #33073, #16868, #18385, #40152, #2189, #93918, #86836, #48276, #64476, #62969, #24471, #55351, #1693, #63966, #78691, #17370, #41153, #79223, #9279, #10784, #9796, #93413, #32577, #70057, #63473, #94909, #94410, #24964, #25471, #674, #72090 ),
 .UNSPECIFIED., .F., .F.,
 ( 4, 2, 2, 2, 2, 2, 2, 2, 2, 2, 2, 2, 2, 2, 2, 2, 2, 2, 2, 2, 2, 2, 4 ),
 ( 0.0002401535358040922863, 0.001257124250616875431, 0.001765609608023326581, 0.002019852286726482767, 0.002146973626077981062, 0.002274094965429479791, 0.002401216304780978521, 0.002528337644132477250, 0.002782580322835466902, 0.003291065680241447074, 0.004308036395053377494, 0.005325007109865307481, 0.005833492467271272908, 0.006087735145974259958, 0.006341977824677245273, 0.006405538494353034754, 0.006469099164028824234, 0.006532659833704612846, 0.006596220503380401459, 0.006850463182083436214, 0.007358948539489502255, 0.007867433896895570031, 0.008375919254301636072 ),
 .UNSPECIFIED. ) ;
#50336 = CARTESIAN_POINT ( 'NONE',  ( 207.6826438088389750, 270.9301044032979462, 7.252082088659585146 ) ) ;
#50337 = CARTESIAN_POINT ( 'NONE',  ( 22.44857442947618154, 193.7677522451419350, -5.000000000000047962 ) ) ;
#50338 = CARTESIAN_POINT ( 'NONE',  ( 93.70588009062352342, 237.1589784336661637, -6.496448406907676862E-16 ) ) ;
#50339 = CARTESIAN_POINT ( 'NONE',  ( 82.79070683882470405, 40.63681047240066846, -1.342339673626402385 ) ) ;
#50340 = CARTESIAN_POINT ( 'NONE',  ( 162.7678667286918142, 249.1757505475115977, -10.38966524845342754 ) ) ;
#50341 = CARTESIAN_POINT ( 'NONE',  ( 84.78301923744977842, 50.41116426179083021, 13.48115605303108744 ) ) ;
#50342 = CARTESIAN_POINT ( 'NONE',  ( 207.6821401748263156, 270.9309767229963768, 1.759036204183980878 ) ) ;
#50343 = CARTESIAN_POINT ( 'NONE',  ( 26.12944271915780448, 176.7048013555409796, 4.594050593750051981 ) ) ;
#50344 = DIRECTION ( 'NONE',  ( 0.7891516029629116469, -0.6141984594095518668, 0.000000000000000000 ) ) ;
#50345 = VERTEX_POINT ( 'NONE', #47 ) ;
#50346 = ORIENTED_EDGE ( 'NONE', *, *, #15902, .T. ) ;
#50347 = CARTESIAN_POINT ( 'NONE',  ( 74.04232911944542650, 68.62205345152153768, 11.42009053252770912 ) ) ;
#50348 = CARTESIAN_POINT ( 'NONE',  ( 185.5908111669773177, 260.2313112761727325, -5.804257864100332398 ) ) ;
#50349 = CARTESIAN_POINT ( 'NONE',  ( 21.94339294393528306, 190.1427522451419350, 10.00000000000009415 ) ) ;
#50350 = CARTESIAN_POINT ( 'NONE',  ( 190.5653282632609091, 300.5781646174276602, -5.775635208185608604 ) ) ;
#50351 = FACE_OUTER_BOUND ( 'NONE', #45453, .T. ) ;
#50352 = CARTESIAN_POINT ( 'NONE',  ( 88.22000632671871756, 44.27423112938743088, 4.003506518527984781 ) ) ;
#50353 = CARTESIAN_POINT ( 'NONE',  ( 182.3152758659521169, 284.3638893697801677, 14.89189215024058299 ) ) ;
#50354 = CARTESIAN_POINT ( 'NONE',  ( 73.84430631328980610, 68.30184443197676103, -11.60545323109705507 ) ) ;
#50355 = CARTESIAN_POINT ( 'NONE',  ( 52.43496435911014686, 191.8923013555410080, 4.594050593750050204 ) ) ;
#50356 = CARTESIAN_POINT ( 'NONE',  ( 92.59663213601577070, 224.2677522451418497, 10.00000000000009592 ) ) ;
#50357 = ORIENTED_EDGE ( 'NONE', *, *, #35890, .F. ) ;
#50358 = CARTESIAN_POINT ( 'NONE',  ( 48.92549481379854370, 97.87922363803308201, -10.00000000000000000 ) ) ;
#50359 = CARTESIAN_POINT ( 'NONE',  ( 179.1448022382906515, 259.4449191438238813, -10.30622490606055308 ) ) ;
#50360 = EDGE_CURVE ( 'NONE', #22518, #89960, #21345, .T. ) ;
#50361 = CARTESIAN_POINT ( 'NONE',  ( 1.609577830863368586, 180.9244531367911577, -4.594050593750046652 ) ) ;
#50362 = B_SPLINE_CURVE_WITH_KNOTS ( 'NONE', 3,
 ( #7430, #69230, #100160, #2353, #87004, #9440, #1848, #95086, #48440, #25649, #86498, #87518, #48946, #88004, #72261, #71255, #96083, #9952, #34239, #71758, #18552, #32730, #32231, #63634, #94077, #49432, #70734, #41826, #56531, #65135, #11466, #57524, #88500, #1345, #24629, #55510, #47919, #94571, #5339, #50428, #12450, #89017, #42321, #96585, #19568, #35231, #36220, #89492, #98046, #67123 ),
 .UNSPECIFIED., .F., .F.,
 ( 4, 2, 2, 2, 2, 2, 2, 2, 2, 2, 2, 2, 2, 2, 2, 2, 2, 2, 2, 2, 2, 2, 2, 2, 4 ),
 ( 0.0003511452654897985752, 0.0008110166299435485121, 0.001040952312170387783, 0.001270887994397226946, 0.001385855835510643600, 0.001500823676624060687, 0.001615791517737477341, 0.001730759358850894429, 0.001960695041077721665, 0.002190630723304548468, 0.002650502087758290978, 0.003110373452212033922, 0.004030116181119518942, 0.004949858910027003962, 0.005409730274480709609, 0.005639665956707606669, 0.005754633797821010095, 0.005869601638934414389, 0.005927085559491183757, 0.005984569480047953992, 0.006099537321161371296, 0.006329473003388079271, 0.006789344367841503892, 0.007249215732294928514, 0.007709087096748353136 ),
 .UNSPECIFIED. ) ;
#50363 = CARTESIAN_POINT ( 'NONE',  ( 68.75905127766452551, 64.69927639754664028, -12.16833701327061945 ) ) ;
#50364 = CARTESIAN_POINT ( 'NONE',  ( 151.3681950933278983, 268.4695907787949523, -15.50699599486383917 ) ) ;
#50365 = CARTESIAN_POINT ( 'NONE',  ( 81.17232691891706509, 55.55242957854174080, 16.36487835605630536 ) ) ;
#50366 = CARTESIAN_POINT ( 'NONE',  ( 146.7943851877206214, 276.3916619194686746, -4.608908220452185844 ) ) ;
#50367 = EDGE_CURVE ( 'NONE', #53634, #52938, #61815, .T. ) ;
#50368 = PLANE ( 'NONE',  #31152 ) ;
#50369 = CARTESIAN_POINT ( 'NONE',  ( 26.37028381016231648, 40.32183835407519723, 177.5919119679930134 ) ) ;
#50370 = CARTESIAN_POINT ( 'NONE',  ( -32.80384426222999394, 95.87215644830973815, 44.08287417880057291 ) ) ;
#50371 = CARTESIAN_POINT ( 'NONE',  ( 164.8251969117060298, 245.1613799118173063, -1.508678420156898348 ) ) ;
#50372 = EDGE_LOOP ( 'NONE', ( #65754, #91895, #32742, #350, #43952 ) ) ;
#50373 = AXIS2_PLACEMENT_3D ( 'NONE', #21978, #92905, #44764 ) ;
#50374 = CARTESIAN_POINT ( 'NONE',  ( 208.3135187673106543, 269.8373969220020285, 2.829653198597726682 ) ) ;
#50375 = CARTESIAN_POINT ( 'NONE',  ( 0.9603191016227148324, 181.3615022471903444, 5.000000000000046185 ) ) ;
#50376 = DIRECTION ( 'NONE',  ( 0.3473291852294957405, -0.6015917957689906892, 0.7193398003386545225 ) ) ;
#50377 = CARTESIAN_POINT ( 'NONE',  ( 122.2307653756559773, 247.5024278399160949, -9.188101187500093303 ) ) ;
#50378 = CARTESIAN_POINT ( 'NONE',  ( 22.90017757337614768, 16.14754757982090183, -5.678558825948276656 ) ) ;
#50380 = EDGE_CURVE ( 'NONE', #90058, #71349, #70148, .T. ) ;
#50379 = CARTESIAN_POINT ( 'NONE',  ( 74.86935717915280009, 67.14205582119099347, 12.97785457704837953 ) ) ;
#50381 = LINE ( 'NONE', #26598, #11233 ) ;
#50383 = FACE_OUTER_BOUND ( 'NONE', #10561, .T. ) ;
#50382 = CARTESIAN_POINT ( 'NONE',  ( 157.8763546842245376, 257.1971277035954699, 17.68444922773363004 ) ) ;
#50384 = CARTESIAN_POINT ( 'NONE',  ( 13.94779419600527959, 26.79103043416548147, 8.090169943749478065 ) ) ;
#50385 = ORIENTED_EDGE ( 'NONE', *, *, #93104, .F. ) ;
#50386 = CARTESIAN_POINT ( 'NONE',  ( 191.2729698983822288, 299.3524933518466469, 8.871011392605806734 ) ) ;
#50387 = DIRECTION ( 'NONE',  ( 1.000000000000000000, 0.000000000000000000, 0.000000000000000000 ) ) ;
#50388 = CARTESIAN_POINT ( 'NONE',  ( 190.4179675745853899, 261.7305499122562651, -6.837651125279566422 ) ) ;
#50389 = CARTESIAN_POINT ( 'NONE',  ( 170.8539755607556856, 266.8602971898987448, -16.49407833488313102 ) ) ;
#50390 = CARTESIAN_POINT ( 'NONE',  ( 81.42010827217174551, 55.18017053111339010, -15.93332911233570215 ) ) ;
#50391 = ORIENTED_EDGE ( 'NONE', *, *, #23185, .F. ) ;
#50392 = CARTESIAN_POINT ( 'NONE',  ( 68.79154833403119085, 66.56514279001069667, 9.697512220263618588 ) ) ;
#50393 = CARTESIAN_POINT ( 'NONE',  ( 168.4118925024307316, 271.5375153668513803, -16.56645075760022223 ) ) ;
#50394 = EDGE_CURVE ( 'NONE', #70646, #16945, #41007, .T. ) ;
#50395 = EDGE_CURVE ( 'NONE', #41928, #39162, #99883, .T. ) ;
#50396 = CARTESIAN_POINT ( 'NONE',  ( 84.81378781617564755, 44.04893954711137383, 6.950746278775451259 ) ) ;
#50397 = CARTESIAN_POINT ( 'NONE',  ( 80.33815187331018137, 55.67465446643217319, 16.05710040854216203 ) ) ;
#50398 = CARTESIAN_POINT ( 'NONE',  ( 185.8564171466189805, 296.7006670448145655, 4.687756417891510985 ) ) ;
#50399 = CARTESIAN_POINT ( 'NONE',  ( 72.29604205201167133, 71.64671137691723857, -5.830803549263603891 ) ) ;
#50400 = CARTESIAN_POINT ( 'NONE',  ( 149.0244553356880886, 274.5290671187512999, 9.114935767028397251 ) ) ;
#50401 = CARTESIAN_POINT ( 'NONE',  ( -38.35373792487678202, 26.90998726756845727, 10.00000000000000000 ) ) ;
#50402 = CARTESIAN_POINT ( 'NONE',  ( 6.396987757676564357, 15.64441083166258295, -10.00000000000000533 ) ) ;
#50403 = CARTESIAN_POINT ( 'NONE',  ( 173.8216752892163868, 272.7590265814922077, -16.35953687348087726 ) ) ;
#50404 = ORIENTED_EDGE ( 'NONE', *, *, #59666, .F. ) ;
#50405 = DIRECTION ( 'NONE',  ( 0.4999999999999998890, -0.8660254037844385966, 0.000000000000000000 ) ) ;
#50406 = CARTESIAN_POINT ( 'NONE',  ( 148.1632261683078013, 274.0207597936089883, -7.853210555358286271 ) ) ;
#50407 = FACE_OUTER_BOUND ( 'NONE', #51957, .T. ) ;
#50408 = ORIENTED_EDGE ( 'NONE', *, *, #86807, .T. ) ;
#50409 = LINE ( 'NONE', #67102, #55543 ) ;
#50410 = CARTESIAN_POINT ( 'NONE',  ( -0.8836234265189104597, 25.35879081310345029, 10.00000000000000000 ) ) ;
#50411 = LINE ( 'NONE', #82861, #17177 ) ;
#50412 = ORIENTED_EDGE ( 'NONE', *, *, #75861, .T. ) ;
#50413 = CARTESIAN_POINT ( 'NONE',  ( 76.95378796010953693, 224.4244531367911293, -4.594050593750046652 ) ) ;
#50414 = CARTESIAN_POINT ( 'NONE',  ( 76.65771178043479495, 52.44190810767315725, -15.81497611108756729 ) ) ;
#50415 = DIRECTION ( 'NONE',  ( 0.4999999999999992784, -0.8660254037844390407, 0.000000000000000000 ) ) ;
#50416 = CARTESIAN_POINT ( 'NONE',  ( 185.4773086304266485, 259.3004018688347969, -6.871889497688444592 ) ) ;
#50417 = ORIENTED_EDGE ( 'NONE', *, *, #53344, .F. ) ;
#50418 = ADVANCED_FACE ( 'NONE', ( #18247 ), #52209, .F. ) ;
#50419 = EDGE_LOOP ( 'NONE', ( #42062, #3968, #87739, #45308 ) ) ;
#50420 = CARTESIAN_POINT ( 'NONE',  ( 207.2604828555043639, 270.4328560034130646, 1.704576742114322974 ) ) ;
#50421 = ORIENTED_EDGE ( 'NONE', *, *, #5026, .T. ) ;
#50422 = CARTESIAN_POINT ( 'NONE',  ( 177.5830009069409243, 288.2251281501418703, -12.31337555878815593 ) ) ;
#50423 = ORIENTED_EDGE ( 'NONE', *, *, #79298, .F. ) ;
#50424 = DIRECTION ( 'NONE',  ( -0.8660254037844387076, -0.4999999999999998890, -0.000000000000000000 ) ) ;
#50425 = CARTESIAN_POINT ( 'NONE',  ( 155.2193237801463113, 261.7992402267395846, -18.58295809893692407 ) ) ;
#50426 = ORIENTED_EDGE ( 'NONE', *, *, #25713, .T. ) ;
#50427 = EDGE_CURVE ( 'NONE', #80286, #91687, #26836, .T. ) ;
#50428 = CARTESIAN_POINT ( 'NONE',  ( 182.7415947523957414, 280.1175424322439653, -16.15561972179322581 ) ) ;
#50429 = CARTESIAN_POINT ( 'NONE',  ( 81.91079631343028211, 41.10426679011759887, 3.683705643908186111 ) ) ;
#50430 = DIRECTION ( 'NONE',  ( 0.000000000000000000, -0.7457702847286276082, -0.6662031840330557841 ) ) ;
#50431 = CARTESIAN_POINT ( 'NONE',  ( 160.0082391144745770, 275.8370785871085218, -12.54704109973508430 ) ) ;
#50432 = CARTESIAN_POINT ( 'NONE',  ( 152.6740002182599767, 266.2078699576288159, -17.16212636348624088 ) ) ;
#50433 = DIRECTION ( 'NONE',  ( 0.000000000000000000, 0.000000000000000000, 1.000000000000000000 ) ) ;
#50434 = CARTESIAN_POINT ( 'NONE',  ( 11.37297787527554327, 165.8262482093457777, 3.021315404115420679E-15 ) ) ;
#50435 = EDGE_CURVE ( 'NONE', #7044, #45081, #58150, .T. ) ;
#50436 = CARTESIAN_POINT ( 'NONE',  ( 139.3894143317827172, 239.0327760586659736, 1.948934522072303157E-15 ) ) ;
#50437 = LINE ( 'NONE', #41329, #98133 ) ;
#50438 = CARTESIAN_POINT ( 'NONE',  ( 6.089662503932698812, 18.91421378149916421, 9.188101187500008038 ) ) ;
#50439 = ORIENTED_EDGE ( 'NONE', *, *, #36678, .F. ) ;
#50440 = EDGE_CURVE ( 'NONE', #56639, #4089, #48472, .T. ) ;
#50442 = VERTEX_POINT ( 'NONE', #75954 ) ;
#50441 = DIRECTION ( 'NONE',  ( 1.000000000000000000, 0.000000000000000000, 0.000000000000000000 ) ) ;
#50443 = EDGE_CURVE ( 'NONE', #91009, #72912, #37406, .T. ) ;
#50444 = DIRECTION ( 'NONE',  ( -0.000000000000000000, -0.000000000000000000, 1.000000000000000000 ) ) ;
#50445 = CARTESIAN_POINT ( 'NONE',  ( -3.532187684056935062, 168.7677522451418781, 10.00000000000009592 ) ) ;
#50446 = EDGE_CURVE ( 'NONE', #68986, #95838, #88522, .T. ) ;
#50447 = CARTESIAN_POINT ( 'NONE',  ( 171.0538495004223876, 287.7798256178718361, -5.161094478304363520 ) ) ;
#50448 = CARTESIAN_POINT ( 'NONE',  ( 156.3189285634391297, 279.5595592535279934, 7.576391211794518910 ) ) ;
#50449 = CARTESIAN_POINT ( 'NONE',  ( 165.5268399678854507, 246.9190504269991777, -1.962147731062478861 ) ) ;
#50450 = CARTESIAN_POINT ( 'NONE',  ( 171.0551658227854830, 280.8129418237058985, 14.02084244714893302 ) ) ;
#50451 = CARTESIAN_POINT ( 'NONE',  ( 170.4855375986076638, 248.6613294790634541, -0.2716024841417116753 ) ) ;
#50452 = CARTESIAN_POINT ( 'NONE',  ( 194.0301671551565335, 292.9381004227619201, 15.31542839880081708 ) ) ;
#50453 = ORIENTED_EDGE ( 'NONE', *, *, #31342, .F. ) ;
#50454 = CARTESIAN_POINT ( 'NONE',  ( 196.1714484216475114, 286.8573191425118125, -17.65736119903840873 ) ) ;
#50455 = CARTESIAN_POINT ( 'NONE',  ( 77.82117886139609197, 61.13554303172738003, -15.83944663029401134 ) ) ;
#50456 = ORIENTED_EDGE ( 'NONE', *, *, #29825, .F. ) ;
#50457 = CARTESIAN_POINT ( 'NONE',  ( 161.3479856134717636, 276.1092341099754321, 12.81212134750285081 ) ) ;
#50458 = CARTESIAN_POINT ( 'NONE',  ( 205.1121091515972523, 269.0638940746846970, -3.021909147741778323 ) ) ;
#50459 = PLANE ( 'NONE',  #20736 ) ;
#50460 = CARTESIAN_POINT ( 'NONE',  ( 30.01653393904200584, 17.73415679381823296, -6.890680421881970419E-14 ) ) ;
#50461 = CARTESIAN_POINT ( 'NONE',  ( 164.6727963122121423, 274.3640629835949198, 16.11238128926960655 ) ) ;
#50463 = CARTESIAN_POINT ( 'NONE',  ( 87.90044328681766217, 44.19652605784722965, 2.801406232019506337 ) ) ;
#50462 = LINE ( 'NONE', #66171, #1520 ) ;
#50464 = CARTESIAN_POINT ( 'NONE',  ( 203.7017578282252828, 269.5031481065263961, 5.505061929047487368 ) ) ;
#50465 = ORIENTED_EDGE ( 'NONE', *, *, #44894, .T. ) ;
#50466 = CARTESIAN_POINT ( 'NONE',  ( 78.48493553110232313, 60.21799449290400474, -16.03803239114666113 ) ) ;
#50467 = PLANE ( 'NONE',  #41571 ) ;
#50468 = CARTESIAN_POINT ( 'NONE',  ( 170.3178023250738420, 289.0326318653803241, -4.561300590322002080 ) ) ;
#50469 = DIRECTION ( 'NONE',  ( 1.000000000000000000, 0.000000000000000000, 0.000000000000000000 ) ) ;
#50470 =( BOUNDED_CURVE ( )  B_SPLINE_CURVE ( 2, ( #93130, #23679, #63196, #94136, #85555, #24692, #47000, #17090, #47983 ),
 .UNSPECIFIED., .F., .T. ) 
 B_SPLINE_CURVE_WITH_KNOTS ( ( 3, 2, 2, 2, 3 ),
 ( 0.04435483870967742159, 0.04569892473118279674, 0.04838709677419354704, 0.05107526881720430428, 0.05241935483870967943 ),
 .UNSPECIFIED. ) 
 CURVE ( )  GEOMETRIC_REPRESENTATION_ITEM ( )  RATIONAL_B_SPLINE_CURVE ( ( 0.9330127018922194093, 0.9330127018922194093, 1.000000000000000000, 0.8660254037844387076, 1.000000000000000000, 0.8660254037844387076, 1.000000000000000000, 0.9330127018922194093, 0.9330127018922194093 ) ) 
 REPRESENTATION_ITEM ( '' )  );
#50471 = CARTESIAN_POINT ( 'NONE',  ( 81.01849461552974674, 43.39542731648039364, -9.975009594712970440 ) ) ;
#50472 = CARTESIAN_POINT ( 'NONE',  ( 47.29267820409023670, 198.1115022471902591, 10.00000000000009592 ) ) ;
#50473 = CARTESIAN_POINT ( 'NONE',  ( -3.153561889951042474, 178.1744531367911577, 4.594050593750047540 ) ) ;
#50474 = CARTESIAN_POINT ( 'NONE',  ( 112.9213393807382886, 229.8768266524160140, 9.188101187500098632 ) ) ;
#50475 = CARTESIAN_POINT ( 'NONE',  ( 203.4682009197399566, 278.2297336128146412, -15.36039508894693206 ) ) ;
#50476 = FACE_OUTER_BOUND ( 'NONE', #88643, .T. ) ;
#50477 = CARTESIAN_POINT ( 'NONE',  ( 183.2060477292669702, 294.1525339459620909, -7.844440212064340834 ) ) ;
#50478 = CARTESIAN_POINT ( 'NONE',  ( 190.4356836585210431, 300.3996184492839916, -0.5836641476860114919 ) ) ;
#50479 = VECTOR ( 'NONE', #50911, 1000.000000000000000 ) ;
#50480 = CARTESIAN_POINT ( 'NONE',  ( 197.5165420832383063, 285.5553545344866393, 17.81061140909387674 ) ) ;
#50481 = CARTESIAN_POINT ( 'NONE',  ( 160.3874973637684036, 282.4990615666047233, 5.130977648321134232 ) ) ;
#50482 = CARTESIAN_POINT ( 'NONE',  ( 194.4032909867620447, 293.9306181827685123, -16.05392006271526384 ) ) ;
#50483 = CARTESIAN_POINT ( 'NONE',  ( 84.90983652888880329, 50.15852115595398431, 13.71398460619150406 ) ) ;
#50484 = CARTESIAN_POINT ( 'NONE',  ( 86.26382137439000530, 210.6115022471902023, -5.000000000000041744 ) ) ;
#50485 = CARTESIAN_POINT ( 'NONE',  ( 165.9388254541857179, 253.6912615456542994, -13.21544657617518403 ) ) ;
#50486 = VECTOR ( 'NONE', #43126, 1000.000000000000114 ) ;
#50487 = CARTESIAN_POINT ( 'NONE',  ( 175.9503686591639280, 265.5728256660283932, -15.87756521623894379 ) ) ;
#50488 = CARTESIAN_POINT ( 'NONE',  ( 73.73334276372743545, 219.5024278399160664, 9.188101187500095079 ) ) ;
#50489 = CARTESIAN_POINT ( 'NONE',  ( -110.0000000000000000, 0.000000000000000000, 59.99999999999999289 ) ) ;
#50491 = EDGE_CURVE ( 'NONE', #87238, #65763, #9730, .T. ) ;
#50490 = CARTESIAN_POINT ( 'NONE',  ( 4.520885125481575173, 45.87218647215556899, 59.99999999999999289 ) ) ;
#50492 = CARTESIAN_POINT ( 'NONE',  ( -15.87523210145152674, 102.8908870699714697, 12.57042221494010903 ) ) ;
#50494 = CARTESIAN_POINT ( 'NONE',  ( 151.7175356514093778, 267.8645151830532996, 16.34156987408047357 ) ) ;
#50493 = CARTESIAN_POINT ( 'NONE',  ( 157.7365441389748923, 257.4392866714015895, 18.13124212464487073 ) ) ;
#50495 = CARTESIAN_POINT ( 'NONE',  ( 199.1526122334580862, 285.7045524820243259, -17.32174362185583050 ) ) ;
#50496 = CARTESIAN_POINT ( 'NONE',  ( 173.3473246007907846, 267.7778430732650463, -16.37773085552635166 ) ) ;
#50497 = CARTESIAN_POINT ( 'NONE',  ( 38.86330120330953974, 24.29860640527295246, -2.839279412974138328 ) ) ;
#50498 = CARTESIAN_POINT ( 'NONE',  ( 80.71202285803703091, 44.87545462257573803, 11.64689240967433292 ) ) ;
#50499 = CARTESIAN_POINT ( 'NONE',  ( 75.85623159827970596, 62.55299574685686537, 15.52670894256219469 ) ) ;
#50500 = ORIENTED_EDGE ( 'NONE', *, *, #12607, .F. ) ;
#50501 = CARTESIAN_POINT ( 'NONE',  ( 20.98410315089673261, 24.06628583063841376, -9.188101187500006262 ) ) ;
#50502 = B_SPLINE_CURVE_WITH_KNOTS ( 'NONE', 3,
 ( #20253, #83577, #22230, #91172, #21735, #52619 ),
 .UNSPECIFIED., .F., .F.,
 ( 4, 2, 4 ),
 ( 0.01896109736145757188, 0.02348162480702983140, 0.02800215225260209440 ),
 .UNSPECIFIED. ) ;
#50503 = CARTESIAN_POINT ( 'NONE',  ( 173.0805693784550101, 289.6645751659409029, -1.032230538571357936 ) ) ;
#50504 = CARTESIAN_POINT ( 'NONE',  ( -31.73672677518723972, 93.44825184473781121, 10.93130056797209981 ) ) ;
#50505 = CARTESIAN_POINT ( 'NONE',  ( 191.7410529245223358, 288.0106247083093081, -15.82820023231783857 ) ) ;
#50507 = VERTEX_POINT ( 'NONE', #76439 ) ;
#50506 = EDGE_CURVE ( 'NONE', #79874, #92910, #55610, .T. ) ;
#50508 = EDGE_CURVE ( 'NONE', #77062, #89714, #32664, .T. ) ;
#50509 = LINE ( 'NONE', #33850, #36 ) ;
#50510 = CARTESIAN_POINT ( 'NONE',  ( 154.6022411851589311, 267.2721739202577851, 16.02776763618498990 ) ) ;
#50511 = CARTESIAN_POINT ( 'NONE',  ( -36.30795748510355736, 64.30503951426791787, -10.00000000000000000 ) ) ;
#50512 = CARTESIAN_POINT ( 'NONE',  ( 144.6483673461909518, 240.9865022471901455, 1.119607411625061291E-15 ) ) ;
#50513 = CARTESIAN_POINT ( 'NONE',  ( 204.7237927799493775, 276.0549847173622879, -12.81020997223575364 ) ) ;
#50514 = CARTESIAN_POINT ( 'NONE',  ( 75.21686481362549159, 53.08771132160212858, 16.48832112884387868 ) ) ;
#50515 = VERTEX_POINT ( 'NONE', #91702 ) ;
#50516 = CARTESIAN_POINT ( 'NONE',  ( 169.0920981158736538, 248.6540344453142097, -1.899181296268086294 ) ) ;
#50517 = VERTEX_POINT ( 'NONE', #45552 ) ;
#50518 = CARTESIAN_POINT ( 'NONE',  ( 163.3543347837650686, 247.7089878483399730, 10.92686688779373405 ) ) ;
#50519 = CARTESIAN_POINT ( 'NONE',  ( 83.50485132091074547, 41.54316576433266306, 0.9957241127150030513 ) ) ;
#50520 = ORIENTED_EDGE ( 'NONE', *, *, #11096, .T. ) ;
#50521 = CARTESIAN_POINT ( 'NONE',  ( 173.8805019302338621, 250.6242863632701585, 0.4030408839048176262 ) ) ;
#50522 = ORIENTED_EDGE ( 'NONE', *, *, #90380, .T. ) ;
#50523 = CARTESIAN_POINT ( 'NONE',  ( 192.8119174027878273, 292.5372173574173758, 15.34371058135056209 ) ) ;
#50524 = CARTESIAN_POINT ( 'NONE',  ( 206.1123153341301304, 273.6499931060659492, 10.83704338634689002 ) ) ;
#50525 = CARTESIAN_POINT ( 'NONE',  ( 147.8871150585349881, 250.0643266524159287, -9.188101187500093303 ) ) ;
#50526 = B_SPLINE_CURVE_WITH_KNOTS ( 'NONE', 3,
 ( #40940, #81023, #19687, #71885, #2483, #50065, #33365, #18173, #18678, #95218, #56661, #3002, #80512, #49075 ),
 .UNSPECIFIED., .F., .F.,
 ( 4, 2, 2, 2, 2, 2, 4 ),
 ( 0.001362149104930265647, 0.001570548566876670557, 0.001778948028823075685, 0.001987347490769480595, 0.002195746952715885505, 0.002612545876608731322, 0.003029344800501577138 ),
 .UNSPECIFIED. ) ;
#50527 = CARTESIAN_POINT ( 'NONE',  ( 88.14071703455390150, 44.55363679567808788, -5.002659464432031911 ) ) ;
#50528 = CARTESIAN_POINT ( 'NONE',  ( 192.9518127100452034, 296.0217619941561793, -12.12386602825073645 ) ) ;
#50529 = CARTESIAN_POINT ( 'NONE',  ( 30.77620441319551503, 35.95586893147757479, 7.433330006724141015 ) ) ;
#50530 = CARTESIAN_POINT ( 'NONE',  ( 184.5123196318015459, 277.1383014161853566, -17.82024832176989904 ) ) ;
#50531 = CARTESIAN_POINT ( 'NONE',  ( 46.60452734134890562, 70.48356709729735314, -10.00000000000000000 ) ) ;
#50532 = CARTESIAN_POINT ( 'NONE',  ( 52.94219725692860834, 189.8262482093458061, 3.021315404115420679E-15 ) ) ;
#50533 = VERTEX_POINT ( 'NONE', #99777 ) ;
#50534 = VERTEX_POINT ( 'NONE', #7559 ) ;
#50535 = CARTESIAN_POINT ( 'NONE',  ( 81.17885442797722817, 42.40402381128041043, 7.623678581642264973 ) ) ;
#50536 = ADVANCED_FACE ( 'NONE', ( #37944 ), #92222, .T. ) ;
#50538 = CARTESIAN_POINT ( 'NONE',  ( -19.65312891409030271, 93.06504152958497400, 177.5919119679930134 ) ) ;
#50537 = CARTESIAN_POINT ( 'NONE',  ( 204.7235752877335244, 276.0553614249301972, 14.82397698933823271 ) ) ;
#50539 = CARTESIAN_POINT ( 'NONE',  ( 85.67419379123523981, 48.38599046538906379, -11.71860351056688820 ) ) ;
#50540 = CARTESIAN_POINT ( 'NONE',  ( 154.9683083969241011, 262.2340116239618055, 18.33261662430134109 ) ) ;
#50541 = DIRECTION ( 'NONE',  ( 0.7061384650677022812, 0.7080737730998298840, 0.000000000000000000 ) ) ;
#50542 = CARTESIAN_POINT ( 'NONE',  ( 187.1789365411204926, 291.3781964708418286, -14.15416893886036220 ) ) ;
#50543 = CARTESIAN_POINT ( 'NONE',  ( 207.3573038884736377, 271.4936096751011974, -4.269021768143928419 ) ) ;
#50544 = DIRECTION ( 'NONE',  ( 0.9291732088853837945, -0.3696446237802449852, 0.000000000000000000 ) ) ;
#50545 = LINE ( 'NONE', #12572, #35400 ) ;
#50546 = EDGE_CURVE ( 'NONE', #75741, #6085, #100284, .T. ) ;
#50547 = CARTESIAN_POINT ( 'NONE',  ( 98.36111373172988692, 227.5958772461660260, -9.188101187500095079 ) ) ;
#50548 = VERTEX_POINT ( 'NONE', #67364 ) ;
#50549 = CYLINDRICAL_SURFACE ( 'NONE', #59256, 70.00000000000002842 ) ;
#50550 = CARTESIAN_POINT ( 'NONE',  ( 163.0703755039977239, 276.5390454317725926, -13.97308584741530346 ) ) ;
#50551 = EDGE_LOOP ( 'NONE', ( #82964, #66507, #54880, #40296 ) ) ;
#50552 = VECTOR ( 'NONE', #54117, 1000.000000000000000 ) ;
#50553 = VERTEX_POINT ( 'NONE', #62243 ) ;
#50554 = CARTESIAN_POINT ( 'NONE',  ( 187.3985626036974281, 299.4490219941366149, -2.047446009836666025 ) ) ;
#50555 = EDGE_CURVE ( 'NONE', #8241, #20627, #47557, .T. ) ;
#50556 = VECTOR ( 'NONE', #87060, 1000.000000000000114 ) ;
#50558 = CARTESIAN_POINT ( 'NONE',  ( 177.0591519751789633, 293.1615183139489886, -2.811523650733721791 ) ) ;
#50557 = B_SPLINE_SURFACE_WITH_KNOTS ( 'NONE', 3, 1, ( 
 ( #92471, #74775 ),
 ( #67142, #98063 ),
 ( #59522, #21074 ),
 ( #51950, #82890 ),
 ( #92959, #93474 ),
 ( #94470, #8338 ),
 ( #38721, #85381 ),
 ( #77233, #9338 ),
 ( #39698, #32633 ),
 ( #23512, #69627 ),
 ( #63530, #55407 ),
 ( #70116, #94979 ),
 ( #1755, #727 ),
 ( #8829, #53911 ),
 ( #236, #70628 ),
 ( #63031, #31613 ),
 ( #64035, #62507 ),
 ( #48341, #71664 ),
 ( #86898, #9860 ),
 ( #47324, #31118 ),
 ( #24026, #62008 ),
 ( #25024, #86393 ),
 ( #54925, #54405 ),
 ( #84870, #85903 ),
 ( #55905, #2254 ),
 ( #93975, #15926 ),
 ( #79287, #46832 ),
 ( #78250, #16427 ),
 ( #77753, #71156 ),
 ( #7840, #39207 ),
 ( #40209, #24528 ),
 ( #1238, #32121 ),
 ( #16925, #47813 ),
 ( #17433, #78750 ) ),
 .UNSPECIFIED., .T., .F., .F.,
 ( 4, 2, 2, 2, 2, 2, 2, 2, 2, 2, 2, 2, 2, 2, 2, 2, 4 ),
 ( 2, 2 ),
 ( 0.000000000000000000, 0.06250000000000000000, 0.1250000000000000000, 0.1875000000000000000, 0.2500000000000000000, 0.3125000000000000000, 0.3750000000000000000, 0.4375000000000000000, 0.5000000000000000000, 0.5625000000000000000, 0.6250000000000000000, 0.6875000000000000000, 0.7500000000000000000, 0.8125000000000000000, 0.8750000000000000000, 0.9375000000000000000, 1.000000000000000000 ),
 ( 0.000000000000000000, 1.000000000000000000 ),
 .UNSPECIFIED. ) ;
#50559 = CARTESIAN_POINT ( 'NONE',  ( 164.2415456882844467, 249.8884775249601375, 10.08728766743346661 ) ) ;
#50560 = CARTESIAN_POINT ( 'NONE',  ( 206.8851632406098702, 272.3113812655195716, -9.957011741946159233 ) ) ;
#50561 = CARTESIAN_POINT ( 'NONE',  ( -56.34825754162683609, 48.22061105236409873, 59.99999999999999289 ) ) ;
#50562 = CARTESIAN_POINT ( 'NONE',  ( 88.83448719433606300, 234.3464784336661353, 1.353441290958777327E-15 ) ) ;
#50563 = ORIENTED_EDGE ( 'NONE', *, *, #66813, .F. ) ;
#50564 = B_SPLINE_CURVE_WITH_KNOTS ( 'NONE', 3,
 ( #90088, #68229, #51544, #52046, #13069, #82984 ),
 .UNSPECIFIED., .F., .F.,
 ( 4, 2, 4 ),
 ( 0.02200203206105470419, 0.02659844398923805545, 0.03119485591742140670 ),
 .UNSPECIFIED. ) ;
#50565 = CARTESIAN_POINT ( 'NONE',  ( 48.72058909919672942, 76.89514952714607432, -10.00000000000000000 ) ) ;
#50566 = CARTESIAN_POINT ( 'NONE',  ( 207.5959034698703078, 271.0803430774575418, -1.830000129038042544 ) ) ;
#50567 = ORIENTED_EDGE ( 'NONE', *, *, #13120, .T. ) ;
#50568 = VECTOR ( 'NONE', #14629, 1000.000000000000000 ) ;
#50569 = CARTESIAN_POINT ( 'NONE',  ( 192.6872782779862234, 265.0988251606153199, -7.785220727510485439 ) ) ;
#50570 = CARTESIAN_POINT ( 'NONE',  ( 153.8831531307005207, 265.2158041805028006, 16.69057008619190441 ) ) ;
#50571 = CARTESIAN_POINT ( 'NONE',  ( -44.74834796241764678, 29.05375577536863929, -10.00000000000000000 ) ) ;
#50573 = CARTESIAN_POINT ( 'NONE',  ( 199.9089016888823664, 283.9562045477092056, 16.92683867318715585 ) ) ;
#50572 = CARTESIAN_POINT ( 'NONE',  ( 139.3894143317827172, 239.0327760586659736, 1.948934522072303157E-15 ) ) ;
#50574 = CARTESIAN_POINT ( 'NONE',  ( -10.02737821244022776, 165.0177522451418781, -10.00000000000009592 ) ) ;
#50575 = CARTESIAN_POINT ( 'NONE',  ( 34.19524549848080852, 69.75853580221966865, 59.99999999999999289 ) ) ;
#50576 = ORIENTED_EDGE ( 'NONE', *, *, #18904, .T. ) ;
#50577 = CARTESIAN_POINT ( 'NONE',  ( 204.5773065883323056, 276.3087062438502812, 13.12907315817041187 ) ) ;
#50578 = CARTESIAN_POINT ( 'NONE',  ( 82.73648154191296555, 53.32161198284063630, 15.27338507632241793 ) ) ;
#50579 = CARTESIAN_POINT ( 'NONE',  ( 206.4640281786353171, 273.0408085897082060, -10.81921452789957883 ) ) ;
#50580 = CARTESIAN_POINT ( 'NONE',  ( 11.76667899187106059, 31.90941714274742225, -10.00000000000000000 ) ) ;
#50581 = CARTESIAN_POINT ( 'NONE',  ( 36.39519187313601378, 198.4865022471903160, 10.00000000000009415 ) ) ;
#50582 = DIRECTION ( 'NONE',  ( 0.5000000000000003331, -0.8660254037844383745, 0.000000000000000000 ) ) ;
#50583 = CARTESIAN_POINT ( 'NONE',  ( 199.0871366603265642, 281.9144776629251510, -16.60803299114443732 ) ) ;
#50584 = CARTESIAN_POINT ( 'NONE',  ( 131.0005090013125084, 234.8932355074535394, -2.679491924311248496 ) ) ;
#50585 = CARTESIAN_POINT ( 'NONE',  ( 79.74169968745719927, 49.12834186041503415, 14.22482900215453760 ) ) ;
#50586 = CARTESIAN_POINT ( 'NONE',  ( 206.7740269583881059, 271.5600005004544641, 6.228629494778278541 ) ) ;
#50587 = CARTESIAN_POINT ( 'NONE',  ( 190.2629546459234859, 273.4080951500121159, -16.67925241984795903 ) ) ;
#50588 = DIRECTION ( 'NONE',  ( -0.000000000000000000, 0.000000000000000000, -1.000000000000000000 ) ) ;
#50589 = CARTESIAN_POINT ( 'NONE',  ( 162.6257765080958677, 248.9708877980734485, -10.42859054881151160 ) ) ;
#50591 = EDGE_CURVE ( 'NONE', #46582, #15352, #10988, .T. ) ;
#50590 = B_SPLINE_CURVE_WITH_KNOTS ( 'NONE', 3,
 ( #77772, #33152, #15947, #9877 ),
 .UNSPECIFIED., .F., .F.,
 ( 4, 4 ),
 ( 0.02382166921119689001, 0.03306032650752911001 ),
 .UNSPECIFIED. ) ;
#50592 = CARTESIAN_POINT ( 'NONE',  ( 163.1628776802707534, 248.0406012790621446, -11.41865110901116331 ) ) ;
#50593 = CARTESIAN_POINT ( 'NONE',  ( 70.54855537558694323, 70.85739277034529948, -3.923908426818032424 ) ) ;
#50595 = CARTESIAN_POINT ( 'NONE',  ( 185.0497311390575703, 266.3498828813088153, 13.18479497404900869 ) ) ;
#50594 = B_SPLINE_CURVE_WITH_KNOTS ( 'NONE', 3,
 ( #11384, #3277, #42234, #73173 ),
 .UNSPECIFIED., .F., .F.,
 ( 4, 4 ),
 ( 0.000000000000000000, 0.003125900356142441959 ),
 .UNSPECIFIED. ) ;
#50596 = CARTESIAN_POINT ( 'NONE',  ( 15.24017643949430401, 10.92755873383624632, 6.180339887498953466 ) ) ;
#50597 = CARTESIAN_POINT ( 'NONE',  ( 41.80956963312145547, 25.10801979619932567, 3.090169943749476733 ) ) ;
#50598 = CARTESIAN_POINT ( 'NONE',  ( -26.08262083840154233, 139.2012482093457493, -37.49999999999996447 ) ) ;
#50599 = CARTESIAN_POINT ( 'NONE',  ( 174.9358745049650565, 292.2217799751211942, 2.235529367806339263 ) ) ;
#50600 = CARTESIAN_POINT ( 'NONE',  ( 157.6009339926387725, 270.9537869527873681, -14.75016313519251376 ) ) ;
#50601 = CARTESIAN_POINT ( 'NONE',  ( 80.78918961562681034, 43.20779693872438543, -9.098606657379765039 ) ) ;
#50602 = CARTESIAN_POINT ( 'NONE',  ( 20.74358691754956396, 182.7833772461660544, -9.188101187500095079 ) ) ;
#50603 = CARTESIAN_POINT ( 'NONE',  ( 67.36468726135395002, 67.68509535240536934, 7.969348504922436405 ) ) ;
#50604 = ORIENTED_EDGE ( 'NONE', *, *, #18119, .T. ) ;
#50605 = CARTESIAN_POINT ( 'NONE',  ( 87.08280028807568840, 46.42470512669584082, 8.779466583191080531 ) ) ;
#50606 = CARTESIAN_POINT ( 'NONE',  ( 39.83529790697233608, 25.12755873383629179, -6.180339887498949025 ) ) ;
#50607 = CARTESIAN_POINT ( 'NONE',  ( 37.65788526339063225, 201.7369531367911293, -4.594050593750048428 ) ) ;
#50608 = AXIS2_PLACEMENT_3D ( 'NONE', #19523, #33191, #26101 ) ;
#50609 = CARTESIAN_POINT ( 'NONE',  ( 87.37996854902368682, 45.84054858551529321, 8.374939902689632731 ) ) ;
#50610 = CARTESIAN_POINT ( 'NONE',  ( 146.8516045228164160, 276.2925551239072774, 3.995954059407343273 ) ) ;
#50611 = CARTESIAN_POINT ( 'NONE',  ( 32.48073783699224748, 37.49103043416551628, -8.090169943749479842 ) ) ;
#50612 = CARTESIAN_POINT ( 'NONE',  ( 201.6080342170015456, 269.2650188364875703, -6.427773377030693069 ) ) ;
#50613 = CARTESIAN_POINT ( 'NONE',  ( 191.0478321355427624, 299.7424433957868928, -9.006798842970001218 ) ) ;
#50614 = LINE ( 'NONE', #65814, #466 ) ;
#50615 = CARTESIAN_POINT ( 'NONE',  ( 67.32446469936046185, 67.76807788068994398, -6.698702025512672797 ) ) ;
#50616 = CARTESIAN_POINT ( 'NONE',  ( 86.02927282398376008, 227.1427522451419634, -10.00000000000009592 ) ) ;
#50617 = AXIS2_PLACEMENT_3D ( 'NONE', #3679, #58829, #75068 ) ;
#50618 = CARTESIAN_POINT ( 'NONE',  ( -27.52599651137551007, 146.7012482093458914, 2.297459087388069147E-14 ) ) ;
#50619 = EDGE_CURVE ( 'NONE', #1972, #11268, #1974, .T. ) ;
#50620 = EDGE_CURVE ( 'NONE', #79192, #84750, #35176, .T. ) ;
#50621 = LINE ( 'NONE', #70054, #61329 ) ;
#50622 = CARTESIAN_POINT ( 'NONE',  ( 87.60525524337998604, 45.45034058462092474, -6.736065127946986308 ) ) ;
#50623 = CARTESIAN_POINT ( 'NONE',  ( 92.68684311912460316, 210.9865022471901455, 1.119607411625061291E-15 ) ) ;
#50624 = CARTESIAN_POINT ( 'NONE',  ( 74.83655476910678317, 53.51806293180211327, 16.54630480343736210 ) ) ;
#50625 = CARTESIAN_POINT ( 'NONE',  ( 74.14312167556930433, 66.30466486950707861, 1.224646799147354045E-15 ) ) ;
#50626 = ORIENTED_EDGE ( 'NONE', *, *, #18191, .F. ) ;
#50627 = CARTESIAN_POINT ( 'NONE',  ( 37.65788526339063225, 201.7369531367911293, -4.594050593750048428 ) ) ;
#50628 = ORIENTED_EDGE ( 'NONE', *, *, #28954, .F. ) ;
#50629 = CARTESIAN_POINT ( 'NONE',  ( -18.11093984425370351, 79.64604002188578136, 14.00762583401780859 ) ) ;
#50630 = CARTESIAN_POINT ( 'NONE',  ( 198.4860348845112981, 286.8590983175747056, -18.20461732983060088 ) ) ;
#50631 = CARTESIAN_POINT ( 'NONE',  ( 67.07163056930700407, 67.06484247801786580, -8.621218654996820163 ) ) ;
#50632 = ORIENTED_EDGE ( 'NONE', *, *, #99796, .F. ) ;
#50634 = CARTESIAN_POINT ( 'NONE',  ( 171.2817005452050694, 286.5486442799788733, 7.499153033049632100 ) ) ;
#50633 = AXIS2_PLACEMENT_3D ( 'NONE', #88996, #57006, #18535 ) ;
#50635 = CARTESIAN_POINT ( 'NONE',  ( 164.9779129355220562, 244.8968679994381148, -1.771286574179712803 ) ) ;
#50636 = CARTESIAN_POINT ( 'NONE',  ( -21.75249381947929095, 146.7012482093458914, -37.49999999999995737 ) ) ;
#50637 = CARTESIAN_POINT ( 'NONE',  ( 34.79119414172389213, 25.80170272979928470, 7.433330006724137462 ) ) ;
#50638 = CARTESIAN_POINT ( 'NONE',  ( 189.7727577176825946, 264.4083146814396628, 11.16063339008121247 ) ) ;
#50639 = CARTESIAN_POINT ( 'NONE',  ( 149.6148422561466305, 277.4437614652936190, 3.137689077364430368 ) ) ;
#50640 = CARTESIAN_POINT ( 'NONE',  ( 171.4377511654674606, 255.6847064655358110, 11.24916129175043977 ) ) ;
#50641 = VERTEX_POINT ( 'NONE', #56145 ) ;
#50642 = CARTESIAN_POINT ( 'NONE',  ( 19.11131643181922968, 13.96004757982089473, -5.678558825948275768 ) ) ;
#50643 = CARTESIAN_POINT ( 'NONE',  ( 68.42755367300264879, 64.43063514657779933, 12.23043961556458470 ) ) ;
#50644 = CARTESIAN_POINT ( 'NONE',  ( -0.01211276271276609529, 139.0458036431182620, -21.50000000000001421 ) ) ;
#50645 = CARTESIAN_POINT ( 'NONE',  ( 156.6812872898450735, 261.2670451491295012, 0.000000000000000000 ) ) ;
#50646 = ORIENTED_EDGE ( 'NONE', *, *, #61006, .T. ) ;
#50647 = CARTESIAN_POINT ( 'NONE',  ( 182.4728335610948875, 284.0645720853299281, 16.33027959180494548 ) ) ;
#50648 = DIRECTION ( 'NONE',  ( 0.4999999999999998890, -0.8660254037844385966, 0.000000000000000000 ) ) ;
#50649 = DIRECTION ( 'NONE',  ( -0.8660254037844387076, -0.4999999999999998890, -0.000000000000000000 ) ) ;
#50650 = ORIENTED_EDGE ( 'NONE', *, *, #79346, .T. ) ;
#50651 = EDGE_LOOP ( 'NONE', ( #46396, #51506, #68977 ) ) ;
#50652 = EDGE_CURVE ( 'NONE', #84728, #56928, #78484, .T. ) ;
#50654 = DIRECTION ( 'NONE',  ( -0.8660254037844387076, -0.4999999999999998890, -0.000000000000000000 ) ) ;
#50653 = CARTESIAN_POINT ( 'NONE',  ( 161.7767236248226084, 250.4414905302161287, -13.15904643207033153 ) ) ;
#50655 = CARTESIAN_POINT ( 'NONE',  ( 196.3507576896697344, 290.5575069072837664, -17.68249398312240928 ) ) ;
#50656 = ORIENTED_EDGE ( 'NONE', *, *, #13474, .F. ) ;
#50657 = CARTESIAN_POINT ( 'NONE',  ( 65.90562114866830257, 69.02037705693993530, -2.125153001406280939 ) ) ;
#50658 = CARTESIAN_POINT ( 'NONE',  ( 198.0006249058153003, 287.6998530631771587, 18.31850453277666801 ) ) ;
#50659 = CARTESIAN_POINT ( 'NONE',  ( 45.57373283677819131, 114.7827874512442889, -10.00000000000000000 ) ) ;
#50660 = CARTESIAN_POINT ( 'NONE',  ( 78.38505820428797222, 61.21347221756810342, -15.89202726422457879 ) ) ;
#50661 = CARTESIAN_POINT ( 'NONE',  ( 198.0442595703406141, 286.6951278662819504, 16.97370723237650481 ) ) ;
#50662 = CARTESIAN_POINT ( 'NONE',  ( 125.1810982770029881, 233.8923013555409796, 4.594050593750050204 ) ) ;
#50663 = CARTESIAN_POINT ( 'NONE',  ( 164.2712161151136172, 246.1209027979328710, 7.276091357954241445 ) ) ;
#50664 = CARTESIAN_POINT ( 'NONE',  ( 185.7745234481418777, 262.1685992436391075, 11.32557499152616032 ) ) ;
#50665 = ORIENTED_EDGE ( 'NONE', *, *, #22839, .F. ) ;
#50666 = CARTESIAN_POINT ( 'NONE',  ( 207.6932907333322191, 270.9116633891313199, 2.120963121341169710 ) ) ;
#50667 = ORIENTED_EDGE ( 'NONE', *, *, #86010, .F. ) ;
#50668 = CARTESIAN_POINT ( 'NONE',  ( 38.77491099913230954, 28.10170272979929962, -7.433330006724141015 ) ) ;
#50669 = FACE_BOUND ( 'NONE', #9301, .T. ) ;
#50670 = CARTESIAN_POINT ( 'NONE',  ( 204.7736914288410048, 274.4078475787994194, -12.22241593628383960 ) ) ;
#50671 = CARTESIAN_POINT ( 'NONE',  ( 78.84873917453550973, 207.1423013555409796, -4.594050593750043987 ) ) ;
#50672 = CARTESIAN_POINT ( 'NONE',  ( -30.04356256989558815, 94.88921800892795488, 12.63376007436073323 ) ) ;
#50673 = CARTESIAN_POINT ( 'NONE',  ( 117.9459173961706995, 232.2365022471902307, 10.00000000000009948 ) ) ;
#50674 = CARTESIAN_POINT ( 'NONE',  ( 193.7999837595647250, 294.9755769528473479, 15.24609078262870199 ) ) ;
#50675 = CARTESIAN_POINT ( 'NONE',  ( 175.8504680664171360, 278.0623914581425993, 16.26995051269672743 ) ) ;
#50676 = EDGE_LOOP ( 'NONE', ( #42441, #47555, #94669, #25108 ) ) ;
#50677 = CARTESIAN_POINT ( 'NONE',  ( 77.38135075303371480, 62.12945940828362268, -15.52596300841300092 ) ) ;
#50678 = B_SPLINE_CURVE_WITH_KNOTS ( 'NONE', 3,
 ( #14009, #68192, #22601, #45873 ),
 .UNSPECIFIED., .F., .F.,
 ( 4, 4 ),
 ( 0.004396866609976072399, 0.01239144977271805503 ),
 .UNSPECIFIED. ) ;
#50679 = CARTESIAN_POINT ( 'NONE',  ( 74.81832046901196520, 67.48663194201290594, -12.71244991431774984 ) ) ;
#50680 = CARTESIAN_POINT ( 'NONE',  ( 203.5477091018662748, 278.0920214017542662, -16.09930363698006062 ) ) ;
#50681 = ORIENTED_EDGE ( 'NONE', *, *, #910, .T. ) ;
#50682 = CARTESIAN_POINT ( 'NONE',  ( 148.6952969693375337, 273.0991861330020924, 9.368475775849525178 ) ) ;
#50683 = DIRECTION ( 'NONE',  ( 0.4330127018922168558, -0.7499999999999987788, 0.5000000000000039968 ) ) ;
#50684 = CARTESIAN_POINT ( 'NONE',  ( 163.9376361691041382, 260.4867098386596354, -16.17183962581199808 ) ) ;
#50685 = CARTESIAN_POINT ( 'NONE',  ( 206.5733357898135978, 270.6748578492084789, 2.446890652106714636 ) ) ;
#50686 = CARTESIAN_POINT ( 'NONE',  ( 60.98670489788378291, 196.0177522451417929, 5.000000000000051514 ) ) ;
#50687 = EDGE_CURVE ( 'NONE', #97333, #49525, #39939, .T. ) ;
#50688 = CARTESIAN_POINT ( 'NONE',  ( 176.9854258871597779, 269.8460570511770129, 17.36332301788626609 ) ) ;
#50689 = VECTOR ( 'NONE', #300, 1000.000000000000000 ) ;
#50690 = CARTESIAN_POINT ( 'NONE',  ( 165.0087721269838710, 244.8434183119457543, 2.604344609212914108 ) ) ;
#50691 = SURFACE_SIDE_STYLE ('',( #19821 ) ) ;
#50692 = CARTESIAN_POINT ( 'NONE',  ( 163.8455942243524248, 246.8581015375447691, -7.178103170949780676 ) ) ;
#50693 = CARTESIAN_POINT ( 'NONE',  ( 132.2986577904150920, 241.0643266524159856, -9.188101187500093303 ) ) ;
#50694 = ORIENTED_EDGE ( 'NONE', *, *, #69031, .F. ) ;
#50695 = CARTESIAN_POINT ( 'NONE',  ( 82.42287977205688776, 44.22628728383867980, -9.237571607454468037 ) ) ;
#50696 = CARTESIAN_POINT ( 'NONE',  ( 83.27976113774722933, 41.54303965256077902, 2.024835421397801039 ) ) ;
#50697 = VECTOR ( 'NONE', #62206, 999.9999999999998863 ) ;
#50698 = CARTESIAN_POINT ( 'NONE',  ( 155.3716771045260714, 261.5353565282119348, -18.54934131471355840 ) ) ;
#50699 = CARTESIAN_POINT ( 'NONE',  ( 79.19548930461120051, 59.90515312544787463, -16.13566294680263624 ) ) ;
#50700 = CARTESIAN_POINT ( 'NONE',  ( 74.19664195402195617, 58.24996677738988637, 15.87843237399661334 ) ) ;
#50701 = CARTESIAN_POINT ( 'NONE',  ( 20.94669640352213236, 37.57748520232516398, -10.00000000000000000 ) ) ;
#50702 = ORIENTED_EDGE ( 'NONE', *, *, #425, .T. ) ;
#50703 = DIRECTION ( 'NONE',  ( -0.8098206029990988597, 0.5866775868892349921, 0.000000000000000000 ) ) ;
#50704 = VECTOR ( 'NONE', #47369, 1000.000000000000000 ) ;
#50705 = CARTESIAN_POINT ( 'NONE',  ( 72.62263890461544236, 71.39809534012815107, -5.857653296095948647 ) ) ;
#50706 = FACE_OUTER_BOUND ( 'NONE', #19760, .T. ) ;
#50707 = CARTESIAN_POINT ( 'NONE',  ( 38.60642373151230800, 181.5494855054051868, -2.679491924311248496 ) ) ;
#50708 = CARTESIAN_POINT ( 'NONE',  ( 160.8697417715285951, 254.0124291816641176, 15.72951850990217437 ) ) ;
#50709 = AXIS2_PLACEMENT_3D ( 'NONE', #8306, #92926, #7295 ) ;
#50710 = CARTESIAN_POINT ( 'NONE',  ( 51.80235952159636525, 85.00000000000000000, -59.99999999999999289 ) ) ;
#50711 = CARTESIAN_POINT ( 'NONE',  ( 69.84362963217853348, 70.73783495060057191, 2.524573071926013768 ) ) ;
#50712 = B_SPLINE_CURVE_WITH_KNOTS ( 'NONE', 3,
 ( #53206, #1009, #84159, #83654 ),
 .UNSPECIFIED., .F., .F.,
 ( 4, 4 ),
 ( 0.000000000000000000, 0.3032312338214309122 ),
 .UNSPECIFIED. ) ;
#50713 = CARTESIAN_POINT ( 'NONE',  ( 204.9184781223158609, 275.7177798128946620, -12.59106622113254126 ) ) ;
#50714 = CARTESIAN_POINT ( 'NONE',  ( 192.1278788183472841, 297.0771818909656190, 10.94873614883879576 ) ) ;
#50715 = CARTESIAN_POINT ( 'NONE',  ( 20.43632886220093425, 13.92755873383625698, 6.180339887498953466 ) ) ;
#50716 = CARTESIAN_POINT ( 'NONE',  ( 190.4249800432324662, 300.8212548652687133, 3.085047376053959400 ) ) ;
#50717 = CARTESIAN_POINT ( 'NONE',  ( 75.70913676221920241, 214.5177522451418497, -10.00000000000009592 ) ) ;
#50718 = CARTESIAN_POINT ( 'NONE',  ( 172.5844283141995845, 287.5847935883521131, -8.232867506822959314 ) ) ;
#50719 = CARTESIAN_POINT ( 'NONE',  ( 155.3250150347760723, 261.6161776038049425, -18.57420904020362684 ) ) ;
#50720 = CARTESIAN_POINT ( 'NONE',  ( 193.3367189744437837, 288.9287801845792956, 16.05736209422542871 ) ) ;
#50721 = CARTESIAN_POINT ( 'NONE',  ( 125.8664413980679342, 250.1427522451419350, 10.00000000000009237 ) ) ;
#50722 = CARTESIAN_POINT ( 'NONE',  ( 183.2938132151843149, 279.0290616485760893, 17.21975379680048235 ) ) ;
#50723 = ORIENTED_EDGE ( 'NONE', *, *, #80304, .F. ) ;
#50724 = CARTESIAN_POINT ( 'NONE',  ( 196.0727848089514964, 291.0389700598140621, 17.56388901715066808 ) ) ;
#50725 = CARTESIAN_POINT ( 'NONE',  ( 148.3190727836317535, 273.7508255376806119, 8.080277324579027365 ) ) ;
#50726 = CARTESIAN_POINT ( 'NONE',  ( 3.179769518870181777, 163.4548013555410080, -4.594050593750042211 ) ) ;
#50727 = EDGE_CURVE ( 'NONE', #89238, #35590, #41963, .T. ) ;
#50728 = CARTESIAN_POINT ( 'NONE',  ( 35.38456857845647363, 200.4244531367911293, -4.594050593750046652 ) ) ;
#50729 = CARTESIAN_POINT ( 'NONE',  ( 82.89821946049899282, 41.08885103174851849, 3.601454807390346513 ) ) ;
#50730 = CARTESIAN_POINT ( 'NONE',  ( 20.69167212271446488, 17.11029122506294087, -8.090169943749478065 ) ) ;
#50731 = CARTESIAN_POINT ( 'NONE',  ( 85.29362735876655677, 48.41412782346649379, 12.38048700662148072 ) ) ;
#50732 = CARTESIAN_POINT ( 'NONE',  ( 157.6668627405778409, 257.5599783937680058, -16.78811156090270629 ) ) ;
#50733 = CARTESIAN_POINT ( 'NONE',  ( 72.04989860578065475, 72.29315785138345518, -3.506402493552649435 ) ) ;
#50734 = CARTESIAN_POINT ( 'NONE',  ( 190.8907028847385448, 300.0145992415348815, -5.421341690443150618 ) ) ;
#50735 = CARTESIAN_POINT ( 'NONE',  ( 74.23290034432453410, 55.48174697381312370, -16.12021105329591819 ) ) ;
#50737 = CARTESIAN_POINT ( 'NONE',  ( 71.37900974329706116, 202.0177522451417929, 5.000000000000051514 ) ) ;
#50736 = CARTESIAN_POINT ( 'NONE',  ( 171.4130652328503004, 258.2459473316166623, 14.36335968337128755 ) ) ;
#50738 = CARTESIAN_POINT ( 'NONE',  ( 75.26062286730075357, 66.82642578153097190, 12.89509023346212402 ) ) ;
#50739 = CARTESIAN_POINT ( 'NONE',  ( 160.4962995477943650, 275.9333967852908813, 14.18032076246626794 ) ) ;
#50740 = CARTESIAN_POINT ( 'NONE',  ( 150.5824154016292198, 269.8306011283729617, 15.30661888403989046 ) ) ;
#50741 = ADVANCED_FACE ( 'NONE', ( #73379 ), #4977, .T. ) ;
#50742 = EDGE_CURVE ( 'NONE', #91371, #61436, #49612, .T. ) ;
#50743 = CARTESIAN_POINT ( 'NONE',  ( 44.69460199273692069, 196.6115022471902591, 10.00000000000009592 ) ) ;
#50744 = CARTESIAN_POINT ( 'NONE',  ( 181.8078859840880170, 291.6367625042899476, 9.277818018440548542 ) ) ;
#50745 = CARTESIAN_POINT ( 'NONE',  ( 172.9311764467664716, 268.4779053881692334, -17.72160738022306603 ) ) ;
#50746 = EDGE_CURVE ( 'NONE', #4283, #47151, #1102, .T. ) ;
#50747 = CARTESIAN_POINT ( 'NONE',  ( -5.021015940802497468, 180.1589784336661637, -6.496448406907675876E-16 ) ) ;
#50748 = CARTESIAN_POINT ( 'NONE',  ( 167.9225537833162889, 286.9219355629304005, 5.061554283893224593 ) ) ;
#50749 = ADVANCED_FACE ( 'NONE', ( #35358 ), #65752, .T. ) ;
#50750 = CARTESIAN_POINT ( 'NONE',  ( 79.04351678514861135, 60.08826646268103389, 16.12134523096112204 ) ) ;
#50751 = CARTESIAN_POINT ( 'NONE',  ( 34.12723495145388597, 35.10171378149922106, 9.188101187500008038 ) ) ;
#50752 = LINE ( 'NONE', #72601, #61139 ) ;
#50753 = CARTESIAN_POINT ( 'NONE',  ( 207.2383675728608239, 271.6996134166075763, 7.873592648726489784 ) ) ;
#50754 = CARTESIAN_POINT ( 'NONE',  ( -70.00000000000000000, 20.00000000000000000, 59.99999999999999289 ) ) ;
#50755 = DIRECTION ( 'NONE',  ( 0.4851478631379963491, -0.8403007481384849875, 0.2419218955996714493 ) ) ;
#50756 = DIRECTION ( 'NONE',  ( 0.9819794923402652698, -0.1889875038809575303, 0.000000000000000000 ) ) ;
#50757 = DIRECTION ( 'NONE',  ( 0.000000000000000000, 0.000000000000000000, 1.000000000000000000 ) ) ;
#50758 = CARTESIAN_POINT ( 'NONE',  ( 13.89352694080530171, 28.99752408145591076, 5.678558825948277544 ) ) ;
#50759 = CARTESIAN_POINT ( 'NONE',  ( 71.92106615665201730, 72.60175000959985425, 1.189886861346804769 ) ) ;
#50760 = CARTESIAN_POINT ( 'NONE',  ( 82.45129306854981621, 53.84777233740990710, 15.85475489262521975 ) ) ;
#50761 = PLANE ( 'NONE',  #40848 ) ;
#50762 = AXIS2_PLACEMENT_3D ( 'NONE', #84204, #14750, #86209 ) ;
#50763 = CARTESIAN_POINT ( 'NONE',  ( 153.0760735463355786, 278.0209436513679861, -4.743639997390301843 ) ) ;
#50764 = ORIENTED_EDGE ( 'NONE', *, *, #61642, .T. ) ;
#50765 = DIRECTION ( 'NONE',  ( 0.8660254037844383745, 0.5000000000000003331, -0.000000000000000000 ) ) ;
#50766 = CARTESIAN_POINT ( 'NONE',  ( 206.7893622945242385, 272.4773133715531230, -10.52881283832460291 ) ) ;
#50767 = ORIENTED_EDGE ( 'NONE', *, *, #88375, .T. ) ;
#50769 = CARTESIAN_POINT ( 'NONE',  ( 192.7507137768506880, 296.7929658737652971, 11.30364540927242345 ) ) ;
#50768 =( BOUNDED_CURVE ( )  B_SPLINE_CURVE ( 2, ( #38172, #47775, #69090, #78713, #100016, #61487, #92437, #69590, #35086 ),
 .UNSPECIFIED., .F., .T. ) 
 B_SPLINE_CURVE_WITH_KNOTS ( ( 3, 2, 2, 2, 3 ),
 ( 0.1491935483870967805, 0.1505376344086021556, 0.1532258064516129059, 0.1559139784946236562, 0.1572580645161290314 ),
 .UNSPECIFIED. ) 
 CURVE ( )  GEOMETRIC_REPRESENTATION_ITEM ( )  RATIONAL_B_SPLINE_CURVE ( ( 0.9330127018922194093, 0.9330127018922194093, 1.000000000000000000, 0.8660254037844387076, 1.000000000000000000, 0.8660254037844387076, 1.000000000000000000, 0.9330127018922194093, 0.9330127018922194093 ) ) 
 REPRESENTATION_ITEM ( '' )  );
#50770 = CARTESIAN_POINT ( 'NONE',  ( 66.54264984482914258, 68.81226801441182772, 2.258477026830895795 ) ) ;
#50771 = CARTESIAN_POINT ( 'NONE',  ( 66.42367604814864990, 68.18713262965796673, 4.499938400593175736 ) ) ;
#50772 = CARTESIAN_POINT ( 'NONE',  ( 87.34298713220451305, 45.48433765315401445, 7.112235686424480008 ) ) ;
#50773 = VECTOR ( 'NONE', #65855, 1000.000000000000000 ) ;
#50774 = VERTEX_POINT ( 'NONE', #12576 ) ;
#50775 = ORIENTED_EDGE ( 'NONE', *, *, #16743, .T. ) ;
#50777 = CARTESIAN_POINT ( 'NONE',  ( 204.3371846825755824, 276.7246095846310823, 14.72513001683937262 ) ) ;
#50776 = CARTESIAN_POINT ( 'NONE',  ( 159.3056354669941470, 256.7215407695565546, 17.03060606420897471 ) ) ;
#50778 = CARTESIAN_POINT ( 'NONE',  ( 153.3616370783189211, 265.0168479788495688, 17.48287904751960653 ) ) ;
#50779 = EDGE_LOOP ( 'NONE', ( #26028, #80374, #13441, #61453 ) ) ;
#50780 = CARTESIAN_POINT ( 'NONE',  ( 80.74781574657599492, 57.21644485803224711, 16.56566952311892749 ) ) ;
#50781 = CARTESIAN_POINT ( 'NONE',  ( 178.0913507944972309, 264.0370130977514123, 14.77546117709988671 ) ) ;
#50782 = EDGE_LOOP ( 'NONE', ( #94073, #99572, #43954, #34233 ) ) ;
#50783 = CARTESIAN_POINT ( 'NONE',  ( 87.67818183259522868, 45.22881258881258759, -6.241223674190681692 ) ) ;
#50784 = CARTESIAN_POINT ( 'NONE',  ( 80.03738279725816085, 49.90009009011918550, -14.50516081086794706 ) ) ;
#50785 = AXIS2_PLACEMENT_3D ( 'NONE', #49920, #42791, #66115 ) ;
#50786 = CARTESIAN_POINT ( 'NONE',  ( 81.03246857581767415, 43.63023369003471430, 9.437679533993755143 ) ) ;
#50787 = ORIENTED_EDGE ( 'NONE', *, *, #46761, .T. ) ;
#50788 = CARTESIAN_POINT ( 'NONE',  ( 202.9994410512713614, 268.1261253757152758, 2.508732235296817326 ) ) ;
#50789 = CARTESIAN_POINT ( 'NONE',  ( 166.2742916145368781, 273.7115028302620203, -15.76541653470950699 ) ) ;
#50790 = PRODUCT_RELATED_PRODUCT_CATEGORY ( 'part', '', ( #32929 ) ) ;
#50791 = CARTESIAN_POINT ( 'NONE',  ( 73.56986118162708976, 59.18547764286820723, 15.61157655548840495 ) ) ;
#50792 = B_SPLINE_SURFACE_WITH_KNOTS ( 'NONE', 3, 1, ( 
 ( #12838, #6706 ),
 ( #43698, #51293 ),
 ( #13803, #60877 ),
 ( #5216, #36096 ),
 ( #37584, #68494 ),
 ( #4728, #13326 ),
 ( #99418, #29021 ),
 ( #20427, #59892 ),
 ( #5703, #74641 ),
 ( #35611, #51818 ),
 ( #59380, #97924 ),
 ( #90860, #29995 ),
 ( #37098, #21412 ),
 ( #75128, #28499 ),
 ( #20937, #44189 ),
 ( #36594, #98430 ),
 ( #52297, #83235 ),
 ( #75614, #6203 ),
 ( #68002, #98926 ),
 ( #60381, #91337 ),
 ( #52786, #83743 ),
 ( #45192, #93332 ),
 ( #63398, #71020 ),
 ( #8700, #30499 ),
 ( #93845, #69985 ),
 ( #16294, #1620 ),
 ( #9202, #24399 ),
 ( #40074, #32506 ),
 ( #99913, #23885 ),
 ( #76604, #22400 ),
 ( #92831, #53295 ),
 ( #1106, #84248 ),
 ( #31483, #14796 ),
 ( #7190, #45678 ) ),
 .UNSPECIFIED., .T., .F., .F.,
 ( 4, 2, 2, 2, 2, 2, 2, 2, 2, 2, 2, 2, 2, 2, 2, 2, 4 ),
 ( 2, 2 ),
 ( 0.000000000000000000, 0.06250000000000000000, 0.1250000000000000000, 0.1875000000000000000, 0.2500000000000000000, 0.3125000000000000000, 0.3750000000000000000, 0.4375000000000000000, 0.5000000000000000000, 0.5625000000000000000, 0.6250000000000000000, 0.6875000000000000000, 0.7500000000000000000, 0.8125000000000000000, 0.8750000000000000000, 0.9375000000000000000, 1.000000000000000000 ),
 ( 0.000000000000000000, 1.000000000000000000 ),
 .UNSPECIFIED. ) ;
#50793 = ORIENTED_EDGE ( 'NONE', *, *, #93109, .T. ) ;
#50794 = CARTESIAN_POINT ( 'NONE',  ( 190.0274641710971082, 301.5097725526222803, 3.738976720635653450 ) ) ;
#50795 = CARTESIAN_POINT ( 'NONE',  ( 171.3756802470358593, 263.0934282751447313, -15.50830625591261658 ) ) ;
#50796 = ORIENTED_EDGE ( 'NONE', *, *, #84717, .T. ) ;
#50797 = CARTESIAN_POINT ( 'NONE',  ( 49.80235952159635815, 85.00000000000000000, -10.00000000000000000 ) ) ;
#50798 = ORIENTED_EDGE ( 'NONE', *, *, #92042, .T. ) ;
#50799 = CYLINDRICAL_SURFACE ( 'NONE', #28226, 70.00000000000002842 ) ;
#50800 = VERTEX_POINT ( 'NONE', #59128 ) ;
#50801 = CARTESIAN_POINT ( 'NONE',  ( 2.064617007569734319, 27.83817977871672511, -10.00000000000000000 ) ) ;
#50802 = CARTESIAN_POINT ( 'NONE',  ( 168.9116873843033488, 272.6398075186710344, 17.37279472990924134 ) ) ;
#50803 = PLANE ( 'NONE',  #60598 ) ;
#50804 = CARTESIAN_POINT ( 'NONE',  ( 188.2735287570237688, 299.1710073388255751, -5.251721556916531419 ) ) ;
#50805 = CARTESIAN_POINT ( 'NONE',  ( 6.117390533544194930, 29.33055864014943026, -10.00000000000000000 ) ) ;
#50806 = CYLINDRICAL_SURFACE ( 'NONE', #50144, 17.82106496071139645 ) ;
#50807 = CARTESIAN_POINT ( 'NONE',  ( 28.65277809448527080, 198.8967562850347122, -4.648177544792955347E-16 ) ) ;
#50808 = CARTESIAN_POINT ( 'NONE',  ( 158.5236181937289928, 256.0760344192481739, -17.53025359445634024 ) ) ;
#50809 = ORIENTED_EDGE ( 'NONE', *, *, #91483, .F. ) ;
#50810 = CARTESIAN_POINT ( 'NONE',  ( 71.85869513609316073, 58.67586711399008692, -15.48493562761569287 ) ) ;
#50811 = EDGE_CURVE ( 'NONE', #39107, #12301, #73772, .T. ) ;
#50812 = DIRECTION ( 'NONE',  ( 1.000000000000000000, 0.000000000000000000, -0.000000000000000000 ) ) ;
#50814 = CARTESIAN_POINT ( 'NONE',  ( 165.0297293518065658, 244.8071193337670195, 2.517333243890161665 ) ) ;
#50813 = CARTESIAN_POINT ( 'NONE',  ( 196.5114383562724072, 290.2791998289336561, -17.87308875047256862 ) ) ;
#50816 = ORIENTED_EDGE ( 'NONE', *, *, #90683, .F. ) ;
#50815 = CARTESIAN_POINT ( 'NONE',  ( 198.6012358295098750, 286.6595644277572887, 18.21911298807435386 ) ) ;
#50817 = ORIENTED_EDGE ( 'NONE', *, *, #80093, .F. ) ;
#50818 = CARTESIAN_POINT ( 'NONE',  ( 190.7696186671953740, 300.2243232583145414, 6.802752300423729359 ) ) ;
#50819 = CARTESIAN_POINT ( 'NONE',  ( 82.55707186143240506, 51.89045595487220908, -14.80451076870274107 ) ) ;
#50820 = LINE ( 'NONE', #81769, #49583 ) ;
#50821 = CARTESIAN_POINT ( 'NONE',  ( 180.2261984326610218, 279.1782745765357276, -17.42438828499370729 ) ) ;
#50822 = EDGE_CURVE ( 'NONE', #81636, #75751, #27818, .T. ) ;
#50823 = CARTESIAN_POINT ( 'NONE',  ( 198.9850252958828776, 285.9948215725895011, -17.02341478767141325 ) ) ;
#50824 = CARTESIAN_POINT ( 'NONE',  ( 148.6479252781755633, 273.1812363089349560, -10.09608632811856488 ) ) ;
#50825 = EDGE_LOOP ( 'NONE', ( #7347, #99170, #32030, #100001 ) ) ;
#50826 = CARTESIAN_POINT ( 'NONE',  ( 163.0424334805279045, 248.2492167524936804, -9.671494865076915914 ) ) ;
#50827 = CARTESIAN_POINT ( 'NONE',  ( 189.4381674897702794, 265.0040801212285828, 12.03645615491573828 ) ) ;
#50828 = CARTESIAN_POINT ( 'NONE',  ( 59.05618993882887224, 198.2365022471902023, -10.00000000000009237 ) ) ;
#50830 = EDGE_CURVE ( 'NONE', #56024, #57136, #37583, .T. ) ;
#50829 = CARTESIAN_POINT ( 'NONE',  ( 207.2824254892180704, 271.6233028670009162, 6.274396967990798046 ) ) ;
#50831 = CARTESIAN_POINT ( 'NONE',  ( 29.73762157799522399, 194.6427522451419065, 10.00000000000009237 ) ) ;
#50832 = CARTESIAN_POINT ( 'NONE',  ( 95.24857461505581568, 234.9869531367911293, 4.594050593750046652 ) ) ;
#50833 = CARTESIAN_POINT ( 'NONE',  ( 82.80082720015894893, 40.64166234397397659, -1.331724720465388812 ) ) ;
#50834 = CARTESIAN_POINT ( 'NONE',  ( 163.2329522299293956, 249.6859758605342279, -11.67970021474453723 ) ) ;
#50835 = CARTESIAN_POINT ( 'NONE',  ( 84.35279708572993229, 50.67471669617422236, 13.78338001634371857 ) ) ;
#50836 = CARTESIAN_POINT ( 'NONE',  ( 163.2109138634145609, 247.9574001692554077, 11.18215713980082171 ) ) ;
#50837 = CARTESIAN_POINT ( 'NONE',  ( 32.86828966629671811, 177.5327760586659736, 1.948934522072303157E-15 ) ) ;
#50838 = DIRECTION ( 'NONE',  ( -0.8660254037844387076, -0.4999999999999998890, -0.000000000000000000 ) ) ;
#50839 = VERTEX_POINT ( 'NONE', #69984 ) ;
#50840 = ORIENTED_EDGE ( 'NONE', *, *, #43745, .F. ) ;
#50841 = CARTESIAN_POINT ( 'NONE',  ( 20.46409116061435185, 58.39290319439324861, 59.99999999999999289 ) ) ;
#50842 = CARTESIAN_POINT ( 'NONE',  ( 74.27485901263420942, 68.48687493391096837, -11.14965480144356569 ) ) ;
#50843 = CARTESIAN_POINT ( 'NONE',  ( 74.34518270076702606, 65.51476795103405948, 13.81701700184060932 ) ) ;
#50844 = DIRECTION ( 'NONE',  ( -0.000000000000000000, 0.000000000000000000, 1.000000000000000000 ) ) ;
#50845 = CARTESIAN_POINT ( 'NONE',  ( 25.98835327777827686, 41.64452202306097206, -10.00000000000000000 ) ) ;
#50846 = VECTOR ( 'NONE', #22575, 1000.000000000000000 ) ;
#50847 = CARTESIAN_POINT ( 'NONE',  ( 207.4541616930702617, 271.3258470364304458, -6.834942797545373594 ) ) ;
#50848 = CARTESIAN_POINT ( 'NONE',  ( 182.5213470551811952, 284.2517036362584122, 14.95339142714455782 ) ) ;
#50849 = CARTESIAN_POINT ( 'NONE',  ( 107.7520767022434853, 223.0177522451418213, 5.000000000000051514 ) ) ;
#50850 = CARTESIAN_POINT ( 'NONE',  ( 54.35637144981560454, 196.0643266524159856, -9.188101187500093303 ) ) ;
#50851 = CARTESIAN_POINT ( 'NONE',  ( 99.01965388075039698, 214.6427522451417644, 1.119607411625061291E-15 ) ) ;
#50852 = VERTEX_POINT ( 'NONE', #69493 ) ;
#50853 = CARTESIAN_POINT ( 'NONE',  ( 198.7749709662292048, 267.8112567065418830, -8.151866048833305456 ) ) ;
#50854 = AXIS2_PLACEMENT_3D ( 'NONE', #63514, #64016, #79267 ) ;
#50855 = CARTESIAN_POINT ( 'NONE',  ( 3.578749241215597010, 161.3262482093458061, 3.021315404115420679E-15 ) ) ;
#50856 = PLANE ( 'NONE',  #49600 ) ;
#50857 = CARTESIAN_POINT ( 'NONE',  ( -3.153561889951042474, 178.1744531367911577, 4.594050593750047540 ) ) ;
#50858 = CARTESIAN_POINT ( 'NONE',  ( 184.1240780222136095, 289.0015729834078684, -14.54488561116068901 ) ) ;
#50859 = CARTESIAN_POINT ( 'NONE',  ( 79.48876273271771709, 46.38894273206648222, -12.71961528548989406 ) ) ;
#50860 = CARTESIAN_POINT ( 'NONE',  ( 147.3715240516018810, 275.3920280842035595, -3.728968767617475866 ) ) ;
#50861 = CARTESIAN_POINT ( 'NONE',  ( 73.31626447649914269, 69.83209129105155455, 9.123803007987715930 ) ) ;
#50862 = EDGE_CURVE ( 'NONE', #39984, #24856, #85765, .T. ) ;
#50863 = CARTESIAN_POINT ( 'NONE',  ( 56.57573509489573382, 191.2202760586659736, -5.415160957724236172E-17 ) ) ;
#50864 = CARTESIAN_POINT ( 'NONE',  ( 163.7183543885751078, 247.0784873978576854, -6.786164904910574336 ) ) ;
#50865 = CARTESIAN_POINT ( 'NONE',  ( 72.51945164430701141, 57.47770362461726279, 16.30230911779761982 ) ) ;
#50866 = CARTESIAN_POINT ( 'NONE',  ( -33.00185145827278177, 95.14108417060988643, 43.95777581227104491 ) ) ;
#50867 = CARTESIAN_POINT ( 'NONE',  ( 206.9026071836525205, 272.2811674698855313, 7.240992997279449561 ) ) ;
#50868 = ORIENTED_EDGE ( 'NONE', *, *, #33847, .F. ) ;
#50869 = CARTESIAN_POINT ( 'NONE',  ( 164.4915767550571957, 245.7392269735623529, -6.407198159945809657 ) ) ;
#50870 = CARTESIAN_POINT ( 'NONE',  ( 4.424420716760506522, 173.3615022471902591, -10.00000000000009592 ) ) ;
#50871 = DIRECTION ( 'NONE',  ( 0.8660254037844385966, 0.5000000000000002220, 7.511572993685832627E-16 ) ) ;
#50872 = CARTESIAN_POINT ( 'NONE',  ( 122.6094779419291712, 253.8464784336661353, 1.353441290958777327E-15 ) ) ;
#50873 = EDGE_CURVE ( 'NONE', #83096, #49399, #81174, .T. ) ;
#50874 = CARTESIAN_POINT ( 'NONE',  ( 31.21402144970675607, 20.94754757982090609, 5.678558825948272215 ) ) ;
#50875 = CARTESIAN_POINT ( 'NONE',  ( 206.8103133316597564, 272.4410251107632348, -7.853031083480094487 ) ) ;
#50876 = EDGE_CURVE ( 'NONE', #88538, #45464, #21299, .T. ) ;
#50877 = CARTESIAN_POINT ( 'NONE',  ( 183.1207986101861138, 294.8225010653632694, -8.165837621905515320 ) ) ;
#50879 = CARTESIAN_POINT ( 'NONE',  ( 189.3296586673964725, 289.9008618244355375, 14.45166222766822450 ) ) ;
#50878 = CARTESIAN_POINT ( 'NONE',  ( 181.2440676231241241, 294.5520841294345473, -6.623935519155441654 ) ) ;
#50880 = CARTESIAN_POINT ( 'NONE',  ( 68.44064878421174569, 64.54239741235952010, 12.14664289795469543 ) ) ;
#50881 = ORIENTED_EDGE ( 'NONE', *, *, #78956, .T. ) ;
#50882 = CARTESIAN_POINT ( 'NONE',  ( 151.1926529451685326, 268.7736386982768408, 14.30343427984827365 ) ) ;
#50883 = CARTESIAN_POINT ( 'NONE',  ( 208.0836152412896922, 270.2356015099098840, -1.823998521107428328 ) ) ;
#50884 = DIRECTION ( 'NONE',  ( 1.000000000000000000, 0.000000000000000000, -0.000000000000000000 ) ) ;
#50885 = CARTESIAN_POINT ( 'NONE',  ( 172.7539835797103933, 268.7884175745374478, -17.03505160535703311 ) ) ;
#50886 = CARTESIAN_POINT ( 'NONE',  ( 81.27316195909862984, 55.43468901134095006, -16.33783760952318431 ) ) ;
#50887 = VERTEX_POINT ( 'NONE', #19811 ) ;
#50888 = CARTESIAN_POINT ( 'NONE',  ( 68.35453417343931903, 65.67399229982113695, 10.37910612949749911 ) ) ;
#50889 = CARTESIAN_POINT ( 'NONE',  ( 48.81784752633560487, 86.82484054835779830, 10.00000000000000000 ) ) ;
#50890 = APPLICATION_CONTEXT ( 'automotive_design' ) ;
#50891 = CARTESIAN_POINT ( 'NONE',  ( 83.53995079529126144, 42.42627917222136347, 4.930145434067244814 ) ) ;
#50892 = CARTESIAN_POINT ( 'NONE',  ( 79.99648514317578929, 53.62058690794304283, 15.71113301258886530 ) ) ;
#50893 = CARTESIAN_POINT ( 'NONE',  ( 183.2522050184455509, 295.3237902215792019, 4.692948607239561198 ) ) ;
#50894 = FACE_OUTER_BOUND ( 'NONE', #8478, .T. ) ;
#50895 = CARTESIAN_POINT ( 'NONE',  ( 150.6398013895194197, 278.2883321928695182, -3.066054659821555001E-05 ) ) ;
#50896 = EDGE_LOOP ( 'NONE', ( #79311, #9768, #61364, #29250 ) ) ;
#50897 = CARTESIAN_POINT ( 'NONE',  ( 194.5266718979755751, 283.0022525440393224, 17.46869296283346884 ) ) ;
#50898 = CARTESIAN_POINT ( 'NONE',  ( 43.97106342183892735, 31.10170272979931028, -7.433330006724141015 ) ) ;
#50899 = ORIENTED_EDGE ( 'NONE', *, *, #56346, .T. ) ;
#50900 = DIRECTION ( 'NONE',  ( 0.4999999999999998890, -0.8660254037844385966, 0.000000000000000000 ) ) ;
#50901 = CARTESIAN_POINT ( 'NONE',  ( 148.1004780136491377, 274.1294427855589788, -7.811560775291159331 ) ) ;
#50902 = DIRECTION ( 'NONE',  ( -0.001635407438350360964, -0.9999986627203610867, 0.000000000000000000 ) ) ;
#50903 = VERTEX_POINT ( 'NONE', #50193 ) ;
#50904 = CARTESIAN_POINT ( 'NONE',  ( 79.11039871569171567, 60.06401293417182075, 16.12737026114500694 ) ) ;
#50905 = CARTESIAN_POINT ( 'NONE',  ( 185.9275958459120375, 291.3127718750328654, 12.18038867512309231 ) ) ;
#50906 = B_SPLINE_CURVE_WITH_KNOTS ( 'NONE', 3,
 ( #70388, #94725, #997, #9095, #77513, #62779, #7590, #15682, #30893, #93737, #497, #8104, #86651, #70902, #46072, #46575, #31384, #62268, #61781, #38978, #17182, #48084, #86157, #15172, #1509, #93224, #54670, #9614, #32392, #63288, #94231, #55664, #40476, #57676, #12096, #64294, #87167, #87669, #26793, #80538, #10600, #95747, #71908, #33914, #33392, #26300 ),
 .UNSPECIFIED., .F., .F.,
 ( 4, 1, 1, 1, 2, 2, 1, 1, 1, 2, 2, 1, 1, 2, 2, 1, 1, 2, 2, 1, 1, 2, 2, 1, 2, 2, 1, 2, 2, 4 ),
 ( 0.000000000000000000, 0.06249999999998895328, 0.09374999999998358258, 0.1093749999999792943, 0.1171874999999787809, 0.1249999999999782396, 0.1874999999999764910, 0.2187499999999757694, 0.2343749999999754086, 0.2421874999999754086, 0.2499999999999754086, 0.3124999999999897859, 0.3437499999999955036, 0.3593749999999983902, 0.3750000000000012212, 0.4375000000000066613, 0.4687500000000108802, 0.4843750000000129896, 0.5000000000000149880, 0.5625000000000202061, 0.5937500000000215383, 0.6093750000000206501, 0.6250000000000197620, 0.6875000000000135447, 0.7187500000000121014, 0.7500000000000105471, 0.8125000000000075495, 0.8437500000000063283, 0.8750000000000049960, 1.000000000000000000 ),
 .UNSPECIFIED. ) ;
#50907 = DIRECTION ( 'NONE',  ( 1.000000000000000000, 0.000000000000000000, 0.000000000000000000 ) ) ;
#50908 = VERTEX_POINT ( 'NONE', #50679 ) ;
#50909 = CARTESIAN_POINT ( 'NONE',  ( 85.18102929606172324, 229.1744531367911293, 4.594050593750047540 ) ) ;
#50910 = CARTESIAN_POINT ( 'NONE',  ( 203.1337100355901839, 278.8090888188308440, 15.01049473222304442 ) ) ;
#50911 = DIRECTION ( 'NONE',  ( -0.000000000000000000, 0.000000000000000000, 1.000000000000000000 ) ) ;
#50912 = CARTESIAN_POINT ( 'NONE',  ( 185.3936852094165602, 259.4458236461365459, -6.858812480693883273 ) ) ;
#50913 = EDGE_LOOP ( 'NONE', ( #21418, #25166, #88944, #2758 ) ) ;
#50914 = EDGE_LOOP ( 'NONE', ( #60354, #94586, #64762, #53151 ) ) ;
#50915 = CARTESIAN_POINT ( 'NONE',  ( 207.3589495855971450, 271.0586446502292119, 2.456771036675355457 ) ) ;
#50916 = EDGE_LOOP ( 'NONE', ( #84820, #36464, #40918, #58378 ) ) ;
#50917 = CARTESIAN_POINT ( 'NONE',  ( 192.6411016462967609, 294.0235828830534501, 14.35569275358684393 ) ) ;
#50918 = CIRCLE ( 'NONE', #63865, 70.00000000000001421 ) ;
#50919 = EDGE_LOOP ( 'NONE', ( #12540, #92602, #23756 ) ) ;
#50920 = CARTESIAN_POINT ( 'NONE',  ( 49.63464994930630070, 103.0251469596019120, 177.5919119679930134 ) ) ;
#50921 = CARTESIAN_POINT ( 'NONE',  ( 154.8545429534089237, 262.4310591522755089, -17.81746354318405778 ) ) ;
#50922 = VERTEX_POINT ( 'NONE', #81634 ) ;
#50923 = CARTESIAN_POINT ( 'NONE',  ( 207.5267809074749721, 271.2000668674752433, -7.171564386559168724 ) ) ;
#50924 = CARTESIAN_POINT ( 'NONE',  ( 82.12375653173634760, 41.12462394345740790, 3.261405856185052521 ) ) ;
#50925 = CARTESIAN_POINT ( 'NONE',  ( 147.1831281302520154, 275.7183393919203809, -6.957138126403704881 ) ) ;
#50926 = DIRECTION ( 'NONE',  ( 0.8951289669282637140, -0.4458072818673325943, 0.000000000000000000 ) ) ;
#50927 = CARTESIAN_POINT ( 'NONE',  ( 82.30224259357629535, 41.51585266698759824, -5.837696018585297963 ) ) ;
#50928 = AXIS2_PLACEMENT_3D ( 'NONE', #50149, #42531, #73464 ) ;
#50929 = CARTESIAN_POINT ( 'NONE',  ( 29.37675396051999144, 17.36477965099641452, 1.583844403245364907 ) ) ;
#50930 = CARTESIAN_POINT ( 'NONE',  ( 144.9642793207625004, 248.3768266524159856, -9.188101187500091527 ) ) ;
#50931 = CARTESIAN_POINT ( 'NONE',  ( 167.4161476617964865, 266.6887600003616967, -16.78267018717890124 ) ) ;
#50932 = ORIENTED_EDGE ( 'NONE', *, *, #56009, .F. ) ;
#50933 = CARTESIAN_POINT ( 'NONE',  ( 76.43229601622785196, 58.36452290443871505, 16.05521737458219533 ) ) ;
#50934 = CARTESIAN_POINT ( 'NONE',  ( 7.739928672529463149, 22.65586893147754211, -7.433330006724137462 ) ) ;
#50935 = ORIENTED_EDGE ( 'NONE', *, *, #51085, .T. ) ;
#50936 = EDGE_CURVE ( 'NONE', #86369, #29349, #4594, .T. ) ;
#50937 = CARTESIAN_POINT ( 'NONE',  ( 165.8206990081297931, 283.8978799598649516, 9.576760697357309837 ) ) ;
#50939 = VERTEX_POINT ( 'NONE', #14193 ) ;
#50938 = CARTESIAN_POINT ( 'NONE',  ( 202.3159758243612316, 271.2934567965075416, 9.391350104624100581 ) ) ;
#50940 = CARTESIAN_POINT ( 'NONE',  ( 78.36279588851795097, 47.41043415324340771, -13.73196331463247688 ) ) ;
#50941 = EDGE_CURVE ( 'NONE', #44888, #56418, #94926, .T. ) ;
#50942 = CARTESIAN_POINT ( 'NONE',  ( 70.96429761875693032, 61.15374941679502996, 14.99935025239129871 ) ) ;
#50943 = CARTESIAN_POINT ( 'NONE',  ( 153.5156304082400425, 276.9426167816297948, 7.161423272292579689 ) ) ;
#50944 = CARTESIAN_POINT ( 'NONE',  ( 70.37934122712871954, 61.23818324669216651, 14.28954007458889386 ) ) ;
#50945 = CARTESIAN_POINT ( 'NONE',  ( 157.8973161155885805, 257.8193490992549073, 16.76962879910869120 ) ) ;
#50946 = CYLINDRICAL_SURFACE ( 'NONE', #88843, 2.471954595299370006 ) ;
#50947 = CARTESIAN_POINT ( 'NONE',  ( 88.12308754723774484, 43.81089488678613009, -2.128676964009123651 ) ) ;
#50948 = ORIENTED_EDGE ( 'NONE', *, *, #39884, .F. ) ;
#50949 = CARTESIAN_POINT ( 'NONE',  ( 38.36706665919591330, 84.31990413814679641, 59.99999999999999289 ) ) ;
#50950 = CARTESIAN_POINT ( 'NONE',  ( 66.19182003012738846, 68.79183717905171136, 0.1039918714880866402 ) ) ;
#50951 = VERTEX_POINT ( 'NONE', #486 ) ;
#50952 = EDGE_CURVE ( 'NONE', #25006, #1813, #24136, .T. ) ;
#50953 = CARTESIAN_POINT ( 'NONE',  ( 201.5238370281167022, 268.0995926086904433, -2.854707868619844824 ) ) ;
#50954 = CARTESIAN_POINT ( 'NONE',  ( 192.1478677531999608, 280.9830581577164708, -17.81712158036913252 ) ) ;
#50955 = CARTESIAN_POINT ( 'NONE',  ( 190.7516742497373059, 300.2554039010641418, 4.342609251298632067 ) ) ;
#50956 = CARTESIAN_POINT ( 'NONE',  ( 26.15794687706369004, 39.79426100978996317, -10.00000000000000000 ) ) ;
#50958 = CARTESIAN_POINT ( 'NONE',  ( 88.48864216585432985, 44.00423028902886102, 2.007554169862322713 ) ) ;
#50957 = CARTESIAN_POINT ( 'NONE',  ( 161.4272922886058836, 281.4068005242934305, -7.043569301989234255 ) ) ;
#50959 = AXIS2_PLACEMENT_3D ( 'NONE', #23706, #7019, #37904 ) ;
#50960 = CARTESIAN_POINT ( 'NONE',  ( -19.65312891409030271, 93.06504152958497400, -10.00000000000000888 ) ) ;
#50961 = ORIENTED_EDGE ( 'NONE', *, *, #72017, .T. ) ;
#50962 = CARTESIAN_POINT ( 'NONE',  ( 71.69040520065344424, 62.44079089823191708, -14.09287754070083487 ) ) ;
#50963 = CARTESIAN_POINT ( 'NONE',  ( 122.6368883333364010, 241.6115022471902591, 10.00000000000009592 ) ) ;
#50964 = B_SPLINE_CURVE_WITH_KNOTS ( 'NONE', 3,
 ( #23852, #40042, #17258, #48163 ),
 .UNSPECIFIED., .F., .F.,
 ( 4, 4 ),
 ( 0.008192639775029337407, 0.01433920746624550366 ),
 .UNSPECIFIED. ) ;
#50965 = CARTESIAN_POINT ( 'NONE',  ( 85.51062282364698319, 48.96702101389664108, -12.23238128493629517 ) ) ;
#50966 = EDGE_CURVE ( 'NONE', #24509, #80425, #13694, .T. ) ;
